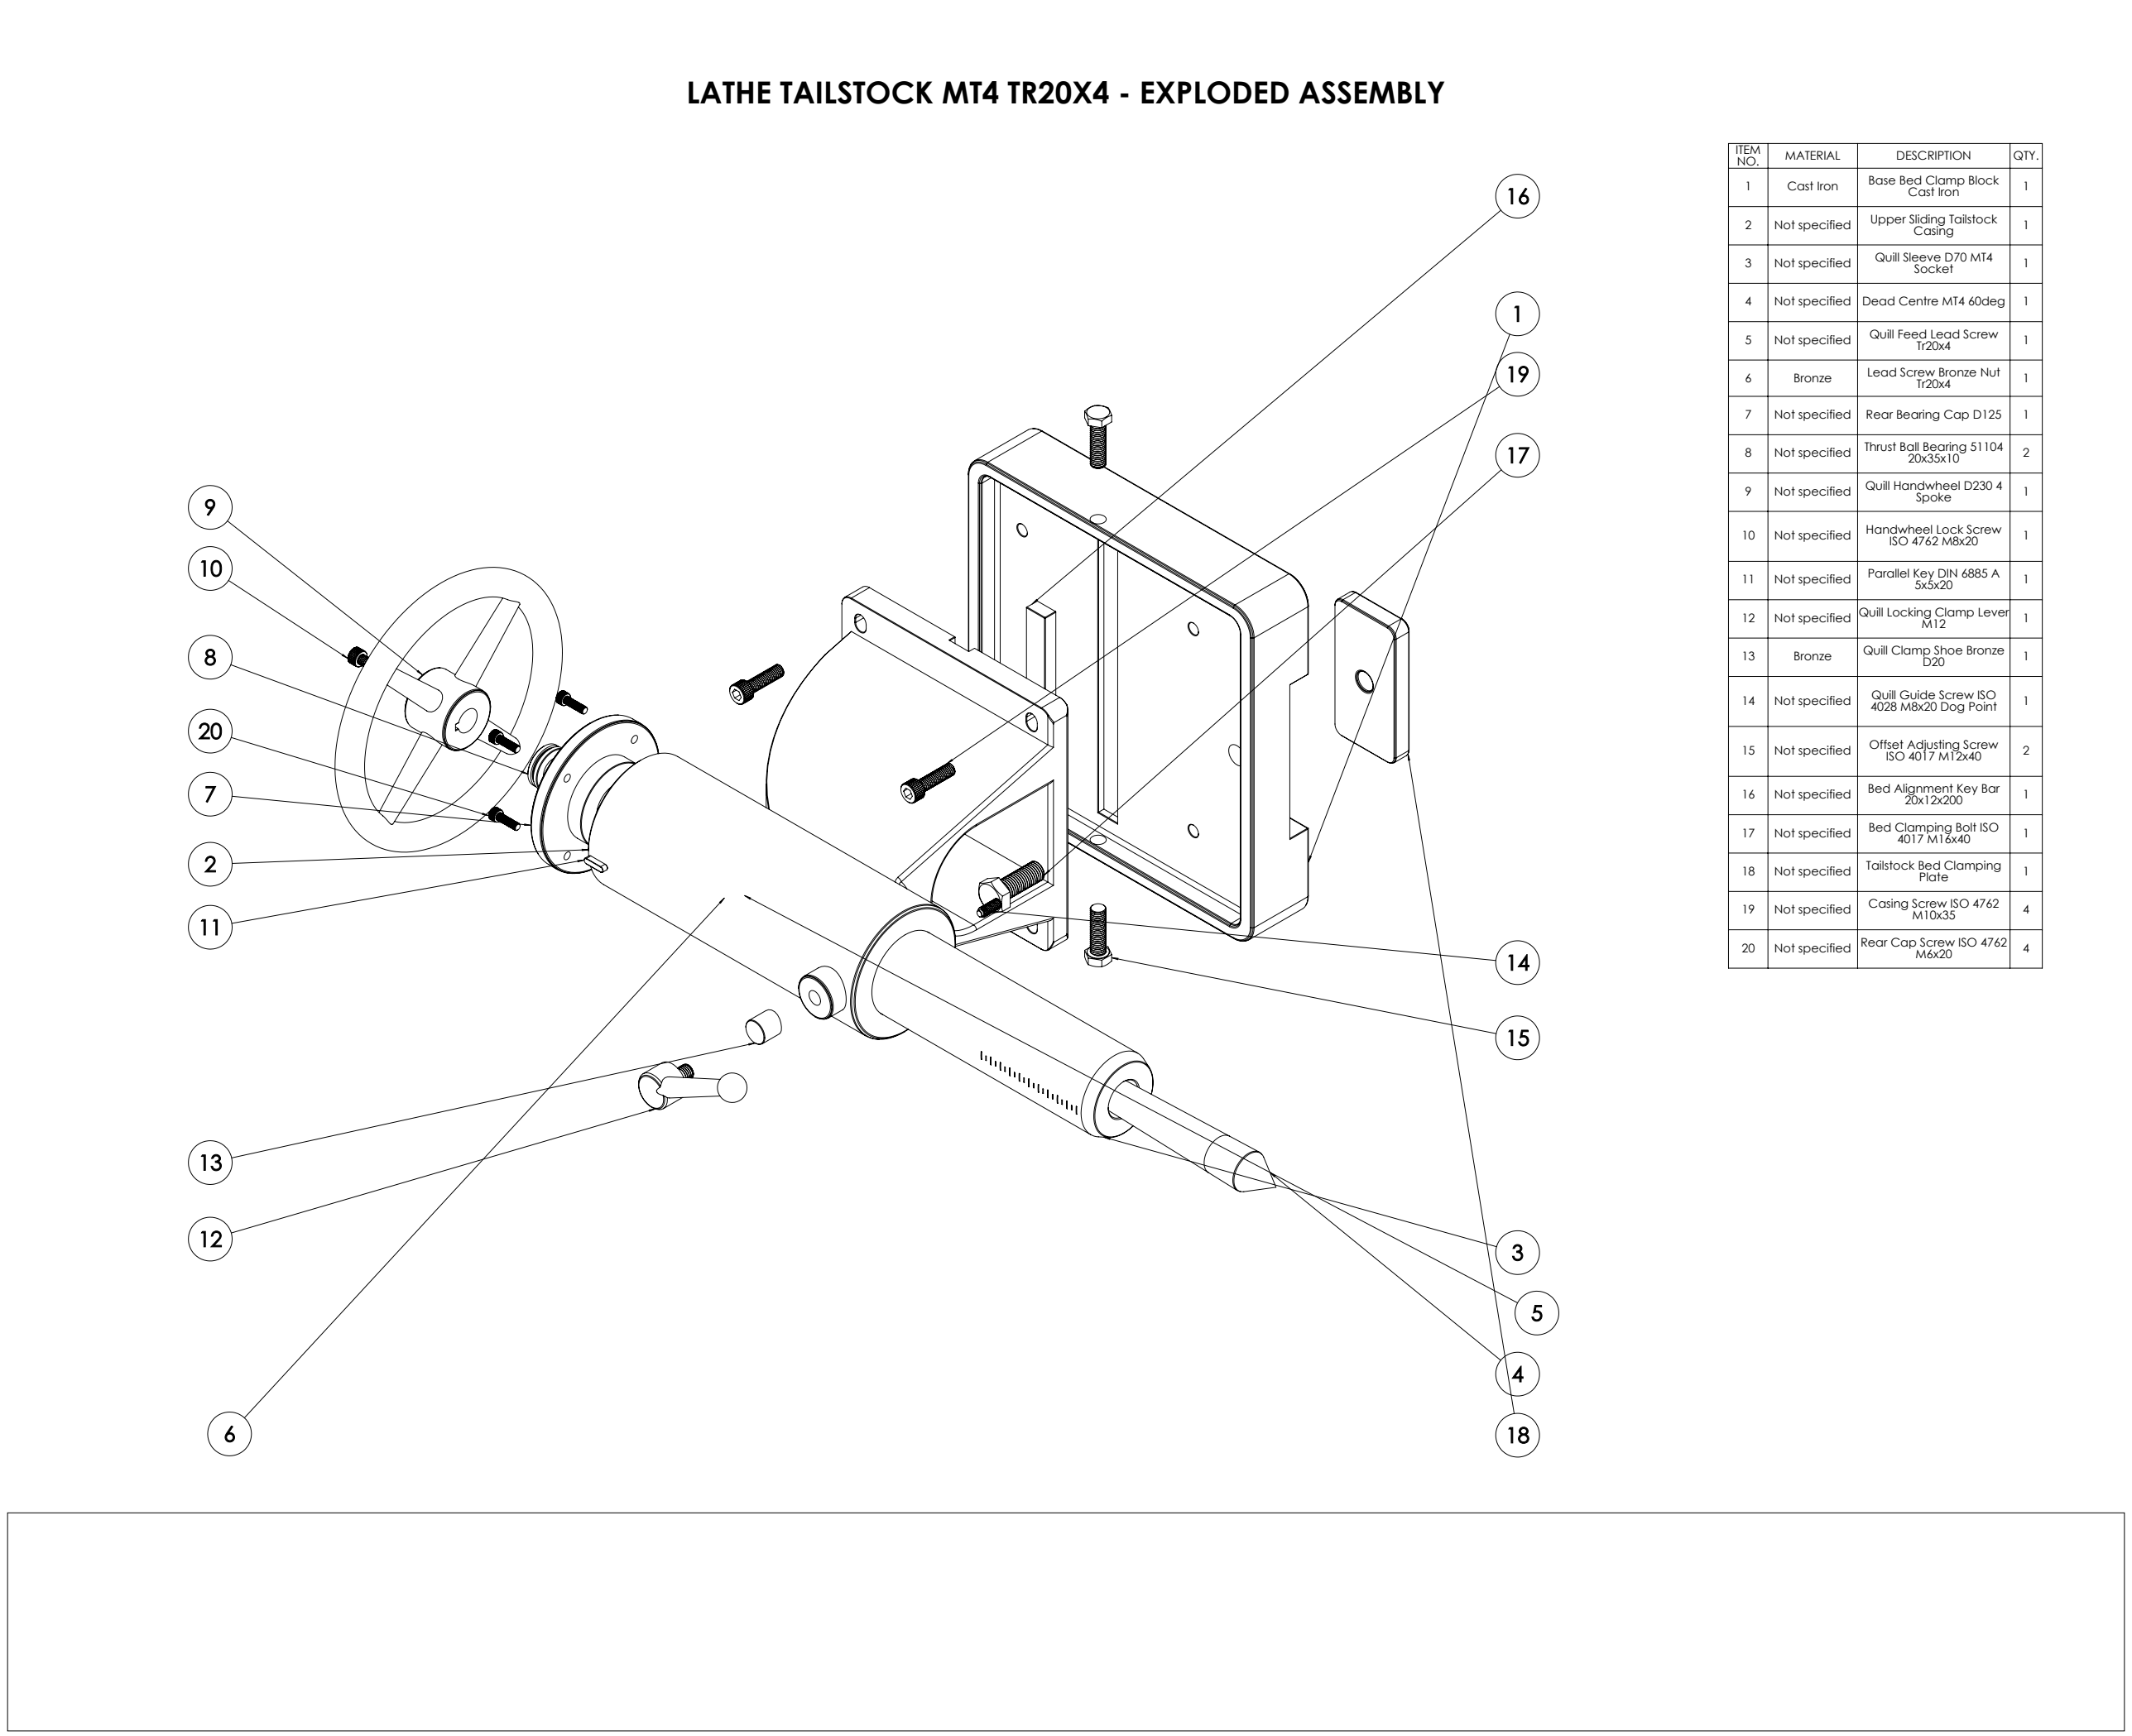
ISO-10303-21;
HEADER;
/* Generated by software containing ST-Developer
 * from STEP Tools, Inc. (www.steptools.com) 
 */

FILE_DESCRIPTION(
/* description */ (''),
/* implementation_level */ '2;1');

FILE_NAME(
/* name */ 'MAS-311',
/* time_stamp */ '2026-10-26T03:50:32-07:00',
/* author */ (''),
/* organization */ (''),
/* preprocessor_version */ 'ST-DEVELOPER v20.2',
/* originating_system */ 'Autodesk Translation Framework v15.15.0.0',
/* authorisation */ '');

FILE_SCHEMA (('AUTOMOTIVE_DESIGN { 1 0 10303 214 3 1 1 }'));
ENDSEC;

DATA;
#10=MECHANICAL_DESIGN_GEOMETRIC_PRESENTATION_REPRESENTATION('',(#1039,#1040,
#1041,#1042,#1043,#1044,#1045,#1046,#1047,#1048,#1049,#1050,#1051,#1052,
#1053,#1054,#1055,#1056,#1057,#1058),#76660);
#11=ITEM_DEFINED_TRANSFORMATION($,$,#26906,#29317);
#12=ITEM_DEFINED_TRANSFORMATION($,$,#27141,#29318);
#13=ITEM_DEFINED_TRANSFORMATION($,$,#27395,#29319);
#14=ITEM_DEFINED_TRANSFORMATION($,$,#27575,#29320);
#15=ITEM_DEFINED_TRANSFORMATION($,$,#27589,#29321);
#16=ITEM_DEFINED_TRANSFORMATION($,$,#27721,#29322);
#17=ITEM_DEFINED_TRANSFORMATION($,$,#27753,#29323);
#18=ITEM_DEFINED_TRANSFORMATION($,$,#28525,#29324);
#19=ITEM_DEFINED_TRANSFORMATION($,$,#27825,#29325);
#20=ITEM_DEFINED_TRANSFORMATION($,$,#27875,#29326);
#21=ITEM_DEFINED_TRANSFORMATION($,$,#28206,#29327);
#22=ITEM_DEFINED_TRANSFORMATION($,$,#28229,#29328);
#23=ITEM_DEFINED_TRANSFORMATION($,$,#28282,#29329);
#24=ITEM_DEFINED_TRANSFORMATION($,$,#28289,#29330);
#25=ITEM_DEFINED_TRANSFORMATION($,$,#28560,#29331);
#26=ITEM_DEFINED_TRANSFORMATION($,$,#28344,#29332);
#27=ITEM_DEFINED_TRANSFORMATION($,$,#28363,#29333);
#28=ITEM_DEFINED_TRANSFORMATION($,$,#28431,#29334);
#29=ITEM_DEFINED_TRANSFORMATION($,$,#28632,#29335);
#30=ITEM_DEFINED_TRANSFORMATION($,$,#28978,#29336);
#31=ITEM_DEFINED_TRANSFORMATION($,$,#28525,#29337);
#32=ITEM_DEFINED_TRANSFORMATION($,$,#28560,#29338);
#33=ITEM_DEFINED_TRANSFORMATION($,$,#28632,#29339);
#34=ITEM_DEFINED_TRANSFORMATION($,$,#28632,#29340);
#35=ITEM_DEFINED_TRANSFORMATION($,$,#28632,#29341);
#36=ITEM_DEFINED_TRANSFORMATION($,$,#28978,#29342);
#37=ITEM_DEFINED_TRANSFORMATION($,$,#28978,#29343);
#38=ITEM_DEFINED_TRANSFORMATION($,$,#28978,#29344);
#39=(
REPRESENTATION_RELATIONSHIP($,$,#76736,#76735)
REPRESENTATION_RELATIONSHIP_WITH_TRANSFORMATION(#11)
SHAPE_REPRESENTATION_RELATIONSHIP()
);
#40=(
REPRESENTATION_RELATIONSHIP($,$,#76737,#76735)
REPRESENTATION_RELATIONSHIP_WITH_TRANSFORMATION(#12)
SHAPE_REPRESENTATION_RELATIONSHIP()
);
#41=(
REPRESENTATION_RELATIONSHIP($,$,#76738,#76735)
REPRESENTATION_RELATIONSHIP_WITH_TRANSFORMATION(#13)
SHAPE_REPRESENTATION_RELATIONSHIP()
);
#42=(
REPRESENTATION_RELATIONSHIP($,$,#76739,#76735)
REPRESENTATION_RELATIONSHIP_WITH_TRANSFORMATION(#14)
SHAPE_REPRESENTATION_RELATIONSHIP()
);
#43=(
REPRESENTATION_RELATIONSHIP($,$,#76740,#76735)
REPRESENTATION_RELATIONSHIP_WITH_TRANSFORMATION(#15)
SHAPE_REPRESENTATION_RELATIONSHIP()
);
#44=(
REPRESENTATION_RELATIONSHIP($,$,#76741,#76735)
REPRESENTATION_RELATIONSHIP_WITH_TRANSFORMATION(#16)
SHAPE_REPRESENTATION_RELATIONSHIP()
);
#45=(
REPRESENTATION_RELATIONSHIP($,$,#76742,#76735)
REPRESENTATION_RELATIONSHIP_WITH_TRANSFORMATION(#17)
SHAPE_REPRESENTATION_RELATIONSHIP()
);
#46=(
REPRESENTATION_RELATIONSHIP($,$,#76752,#76735)
REPRESENTATION_RELATIONSHIP_WITH_TRANSFORMATION(#18)
SHAPE_REPRESENTATION_RELATIONSHIP()
);
#47=(
REPRESENTATION_RELATIONSHIP($,$,#76743,#76735)
REPRESENTATION_RELATIONSHIP_WITH_TRANSFORMATION(#19)
SHAPE_REPRESENTATION_RELATIONSHIP()
);
#48=(
REPRESENTATION_RELATIONSHIP($,$,#76744,#76735)
REPRESENTATION_RELATIONSHIP_WITH_TRANSFORMATION(#20)
SHAPE_REPRESENTATION_RELATIONSHIP()
);
#49=(
REPRESENTATION_RELATIONSHIP($,$,#76745,#76735)
REPRESENTATION_RELATIONSHIP_WITH_TRANSFORMATION(#21)
SHAPE_REPRESENTATION_RELATIONSHIP()
);
#50=(
REPRESENTATION_RELATIONSHIP($,$,#76746,#76735)
REPRESENTATION_RELATIONSHIP_WITH_TRANSFORMATION(#22)
SHAPE_REPRESENTATION_RELATIONSHIP()
);
#51=(
REPRESENTATION_RELATIONSHIP($,$,#76747,#76735)
REPRESENTATION_RELATIONSHIP_WITH_TRANSFORMATION(#23)
SHAPE_REPRESENTATION_RELATIONSHIP()
);
#52=(
REPRESENTATION_RELATIONSHIP($,$,#76748,#76735)
REPRESENTATION_RELATIONSHIP_WITH_TRANSFORMATION(#24)
SHAPE_REPRESENTATION_RELATIONSHIP()
);
#53=(
REPRESENTATION_RELATIONSHIP($,$,#76753,#76735)
REPRESENTATION_RELATIONSHIP_WITH_TRANSFORMATION(#25)
SHAPE_REPRESENTATION_RELATIONSHIP()
);
#54=(
REPRESENTATION_RELATIONSHIP($,$,#76749,#76735)
REPRESENTATION_RELATIONSHIP_WITH_TRANSFORMATION(#26)
SHAPE_REPRESENTATION_RELATIONSHIP()
);
#55=(
REPRESENTATION_RELATIONSHIP($,$,#76750,#76735)
REPRESENTATION_RELATIONSHIP_WITH_TRANSFORMATION(#27)
SHAPE_REPRESENTATION_RELATIONSHIP()
);
#56=(
REPRESENTATION_RELATIONSHIP($,$,#76751,#76735)
REPRESENTATION_RELATIONSHIP_WITH_TRANSFORMATION(#28)
SHAPE_REPRESENTATION_RELATIONSHIP()
);
#57=(
REPRESENTATION_RELATIONSHIP($,$,#76754,#76735)
REPRESENTATION_RELATIONSHIP_WITH_TRANSFORMATION(#29)
SHAPE_REPRESENTATION_RELATIONSHIP()
);
#58=(
REPRESENTATION_RELATIONSHIP($,$,#76755,#76735)
REPRESENTATION_RELATIONSHIP_WITH_TRANSFORMATION(#30)
SHAPE_REPRESENTATION_RELATIONSHIP()
);
#59=(
REPRESENTATION_RELATIONSHIP($,$,#76752,#76735)
REPRESENTATION_RELATIONSHIP_WITH_TRANSFORMATION(#31)
SHAPE_REPRESENTATION_RELATIONSHIP()
);
#60=(
REPRESENTATION_RELATIONSHIP($,$,#76753,#76735)
REPRESENTATION_RELATIONSHIP_WITH_TRANSFORMATION(#32)
SHAPE_REPRESENTATION_RELATIONSHIP()
);
#61=(
REPRESENTATION_RELATIONSHIP($,$,#76754,#76735)
REPRESENTATION_RELATIONSHIP_WITH_TRANSFORMATION(#33)
SHAPE_REPRESENTATION_RELATIONSHIP()
);
#62=(
REPRESENTATION_RELATIONSHIP($,$,#76754,#76735)
REPRESENTATION_RELATIONSHIP_WITH_TRANSFORMATION(#34)
SHAPE_REPRESENTATION_RELATIONSHIP()
);
#63=(
REPRESENTATION_RELATIONSHIP($,$,#76754,#76735)
REPRESENTATION_RELATIONSHIP_WITH_TRANSFORMATION(#35)
SHAPE_REPRESENTATION_RELATIONSHIP()
);
#64=(
REPRESENTATION_RELATIONSHIP($,$,#76755,#76735)
REPRESENTATION_RELATIONSHIP_WITH_TRANSFORMATION(#36)
SHAPE_REPRESENTATION_RELATIONSHIP()
);
#65=(
REPRESENTATION_RELATIONSHIP($,$,#76755,#76735)
REPRESENTATION_RELATIONSHIP_WITH_TRANSFORMATION(#37)
SHAPE_REPRESENTATION_RELATIONSHIP()
);
#66=(
REPRESENTATION_RELATIONSHIP($,$,#76755,#76735)
REPRESENTATION_RELATIONSHIP_WITH_TRANSFORMATION(#38)
SHAPE_REPRESENTATION_RELATIONSHIP()
);
#67=CONTEXT_DEPENDENT_SHAPE_REPRESENTATION(#39,#76707);
#68=CONTEXT_DEPENDENT_SHAPE_REPRESENTATION(#40,#76708);
#69=CONTEXT_DEPENDENT_SHAPE_REPRESENTATION(#41,#76709);
#70=CONTEXT_DEPENDENT_SHAPE_REPRESENTATION(#42,#76710);
#71=CONTEXT_DEPENDENT_SHAPE_REPRESENTATION(#43,#76711);
#72=CONTEXT_DEPENDENT_SHAPE_REPRESENTATION(#44,#76712);
#73=CONTEXT_DEPENDENT_SHAPE_REPRESENTATION(#45,#76713);
#74=CONTEXT_DEPENDENT_SHAPE_REPRESENTATION(#46,#76714);
#75=CONTEXT_DEPENDENT_SHAPE_REPRESENTATION(#47,#76715);
#76=CONTEXT_DEPENDENT_SHAPE_REPRESENTATION(#48,#76716);
#77=CONTEXT_DEPENDENT_SHAPE_REPRESENTATION(#49,#76717);
#78=CONTEXT_DEPENDENT_SHAPE_REPRESENTATION(#50,#76718);
#79=CONTEXT_DEPENDENT_SHAPE_REPRESENTATION(#51,#76719);
#80=CONTEXT_DEPENDENT_SHAPE_REPRESENTATION(#52,#76720);
#81=CONTEXT_DEPENDENT_SHAPE_REPRESENTATION(#53,#76721);
#82=CONTEXT_DEPENDENT_SHAPE_REPRESENTATION(#54,#76722);
#83=CONTEXT_DEPENDENT_SHAPE_REPRESENTATION(#55,#76723);
#84=CONTEXT_DEPENDENT_SHAPE_REPRESENTATION(#56,#76724);
#85=CONTEXT_DEPENDENT_SHAPE_REPRESENTATION(#57,#76725);
#86=CONTEXT_DEPENDENT_SHAPE_REPRESENTATION(#58,#76726);
#87=CONTEXT_DEPENDENT_SHAPE_REPRESENTATION(#59,#76727);
#88=CONTEXT_DEPENDENT_SHAPE_REPRESENTATION(#60,#76728);
#89=CONTEXT_DEPENDENT_SHAPE_REPRESENTATION(#61,#76729);
#90=CONTEXT_DEPENDENT_SHAPE_REPRESENTATION(#62,#76730);
#91=CONTEXT_DEPENDENT_SHAPE_REPRESENTATION(#63,#76731);
#92=CONTEXT_DEPENDENT_SHAPE_REPRESENTATION(#64,#76732);
#93=CONTEXT_DEPENDENT_SHAPE_REPRESENTATION(#65,#76733);
#94=CONTEXT_DEPENDENT_SHAPE_REPRESENTATION(#66,#76734);
#95=NEXT_ASSEMBLY_USAGE_OCCURRENCE(
'01_Base_Bed_Clamp_Block_Cast_Iron:1',
'01_Base_Bed_Clamp_Block_Cast_Iron:1',
'01_Base_Bed_Clamp_Block_Cast_Iron:1',#76757,#76758,
'01_Base_Bed_Clamp_Block_Cast_Iron:1');
#96=NEXT_ASSEMBLY_USAGE_OCCURRENCE(
'02_Upper_Sliding_Tailstock_Casing:1',
'02_Upper_Sliding_Tailstock_Casing:1',
'02_Upper_Sliding_Tailstock_Casing:1',#76757,#76759,
'02_Upper_Sliding_Tailstock_Casing:1');
#97=NEXT_ASSEMBLY_USAGE_OCCURRENCE('03_Quill_Sleeve_D70_MT4_Socket:1',
'03_Quill_Sleeve_D70_MT4_Socket:1','03_Quill_Sleeve_D70_MT4_Socket:1',#76757,
#76760,'03_Quill_Sleeve_D70_MT4_Socket:1');
#98=NEXT_ASSEMBLY_USAGE_OCCURRENCE('04_Dead_Centre_MT4_60deg:1',
'04_Dead_Centre_MT4_60deg:1','04_Dead_Centre_MT4_60deg:1',#76757,#76761,
'04_Dead_Centre_MT4_60deg:1');
#99=NEXT_ASSEMBLY_USAGE_OCCURRENCE('05_Quill_Feed_Lead_Screw_Tr20x4:1',
'05_Quill_Feed_Lead_Screw_Tr20x4:1','05_Quill_Feed_Lead_Screw_Tr20x4:1',
#76757,#76762,'05_Quill_Feed_Lead_Screw_Tr20x4:1');
#100=NEXT_ASSEMBLY_USAGE_OCCURRENCE('06_Lead_Screw_Bronze_Nut_Tr20x4:1',
'06_Lead_Screw_Bronze_Nut_Tr20x4:1','06_Lead_Screw_Bronze_Nut_Tr20x4:1',
#76757,#76763,'06_Lead_Screw_Bronze_Nut_Tr20x4:1');
#101=NEXT_ASSEMBLY_USAGE_OCCURRENCE('07_Rear_Bearing_Cap_D125:1',
'07_Rear_Bearing_Cap_D125:1','07_Rear_Bearing_Cap_D125:1',#76757,#76764,
'07_Rear_Bearing_Cap_D125:1');
#102=NEXT_ASSEMBLY_USAGE_OCCURRENCE(
'08_Thrust_Ball_Bearing_51104_20x35x10:1',
'08_Thrust_Ball_Bearing_51104_20x35x10:1',
'08_Thrust_Ball_Bearing_51104_20x35x10:1',#76757,#76774,
'08_Thrust_Ball_Bearing_51104_20x35x10:1');
#103=NEXT_ASSEMBLY_USAGE_OCCURRENCE('09_Quill_Handwheel_D230_4_Spoke:1',
'09_Quill_Handwheel_D230_4_Spoke:1','09_Quill_Handwheel_D230_4_Spoke:1',
#76757,#76765,'09_Quill_Handwheel_D230_4_Spoke:1');
#104=NEXT_ASSEMBLY_USAGE_OCCURRENCE(
'10_Handwheel_Lock_Screw_ISO_4762_M8x20:1',
'10_Handwheel_Lock_Screw_ISO_4762_M8x20:1',
'10_Handwheel_Lock_Screw_ISO_4762_M8x20:1',#76757,#76766,
'10_Handwheel_Lock_Screw_ISO_4762_M8x20:1');
#105=NEXT_ASSEMBLY_USAGE_OCCURRENCE(
'11_Parallel_Key_DIN_6885_A_5x5x20:1',
'11_Parallel_Key_DIN_6885_A_5x5x20:1',
'11_Parallel_Key_DIN_6885_A_5x5x20:1',#76757,#76767,
'11_Parallel_Key_DIN_6885_A_5x5x20:1');
#106=NEXT_ASSEMBLY_USAGE_OCCURRENCE(
'12_Quill_Locking_Clamp_Lever_M12:1',
'12_Quill_Locking_Clamp_Lever_M12:1',
'12_Quill_Locking_Clamp_Lever_M12:1',#76757,#76768,
'12_Quill_Locking_Clamp_Lever_M12:1');
#107=NEXT_ASSEMBLY_USAGE_OCCURRENCE('13_Quill_Clamp_Shoe_Bronze_D20:1',
'13_Quill_Clamp_Shoe_Bronze_D20:1','13_Quill_Clamp_Shoe_Bronze_D20:1',#76757,
#76769,'13_Quill_Clamp_Shoe_Bronze_D20:1');
#108=NEXT_ASSEMBLY_USAGE_OCCURRENCE(
'14_Quill_Guide_Screw_ISO_4028_M8x20_Dog_Point:1',
'14_Quill_Guide_Screw_ISO_4028_M8x20_Dog_Point:1',
'14_Quill_Guide_Screw_ISO_4028_M8x20_Dog_Point:1',#76757,#76770,
'14_Quill_Guide_Screw_ISO_4028_M8x20_Dog_Point:1');
#109=NEXT_ASSEMBLY_USAGE_OCCURRENCE(
'15_Offset_Adjusting_Screw_ISO_4017_M12x40:1',
'15_Offset_Adjusting_Screw_ISO_4017_M12x40:1',
'15_Offset_Adjusting_Screw_ISO_4017_M12x40:1',#76757,#76775,
'15_Offset_Adjusting_Screw_ISO_4017_M12x40:1');
#110=NEXT_ASSEMBLY_USAGE_OCCURRENCE(
'16_Bed_Alignment_Key_Bar_20x12x200:1',
'16_Bed_Alignment_Key_Bar_20x12x200:1',
'16_Bed_Alignment_Key_Bar_20x12x200:1',#76757,#76771,
'16_Bed_Alignment_Key_Bar_20x12x200:1');
#111=NEXT_ASSEMBLY_USAGE_OCCURRENCE(
'17_Bed_Clamping_Bolt_ISO_4017_M16x40:1',
'17_Bed_Clamping_Bolt_ISO_4017_M16x40:1',
'17_Bed_Clamping_Bolt_ISO_4017_M16x40:1',#76757,#76772,
'17_Bed_Clamping_Bolt_ISO_4017_M16x40:1');
#112=NEXT_ASSEMBLY_USAGE_OCCURRENCE('18_Tailstock_Bed_Clamping_Plate:1',
'18_Tailstock_Bed_Clamping_Plate:1','18_Tailstock_Bed_Clamping_Plate:1',
#76757,#76773,'18_Tailstock_Bed_Clamping_Plate:1');
#113=NEXT_ASSEMBLY_USAGE_OCCURRENCE('19_Casing_Screw_ISO_4762_M10x35:1',
'19_Casing_Screw_ISO_4762_M10x35:1','19_Casing_Screw_ISO_4762_M10x35:1',
#76757,#76776,'19_Casing_Screw_ISO_4762_M10x35:1');
#114=NEXT_ASSEMBLY_USAGE_OCCURRENCE(
'20_Rear_Cap_Screw_ISO_4762_M6x20:1',
'20_Rear_Cap_Screw_ISO_4762_M6x20:1',
'20_Rear_Cap_Screw_ISO_4762_M6x20:1',#76757,#76777,
'20_Rear_Cap_Screw_ISO_4762_M6x20:1');
#115=NEXT_ASSEMBLY_USAGE_OCCURRENCE(
'08_Thrust_Ball_Bearing_51104_20x35x10:2',
'08_Thrust_Ball_Bearing_51104_20x35x10:2',
'08_Thrust_Ball_Bearing_51104_20x35x10:2',#76757,#76774,
'08_Thrust_Ball_Bearing_51104_20x35x10:2');
#116=NEXT_ASSEMBLY_USAGE_OCCURRENCE(
'15_Offset_Adjusting_Screw_ISO_4017_M12x40:2',
'15_Offset_Adjusting_Screw_ISO_4017_M12x40:2',
'15_Offset_Adjusting_Screw_ISO_4017_M12x40:2',#76757,#76775,
'15_Offset_Adjusting_Screw_ISO_4017_M12x40:2');
#117=NEXT_ASSEMBLY_USAGE_OCCURRENCE('19_Casing_Screw_ISO_4762_M10x35:2',
'19_Casing_Screw_ISO_4762_M10x35:2','19_Casing_Screw_ISO_4762_M10x35:2',
#76757,#76776,'19_Casing_Screw_ISO_4762_M10x35:2');
#118=NEXT_ASSEMBLY_USAGE_OCCURRENCE('19_Casing_Screw_ISO_4762_M10x35:3',
'19_Casing_Screw_ISO_4762_M10x35:3','19_Casing_Screw_ISO_4762_M10x35:3',
#76757,#76776,'19_Casing_Screw_ISO_4762_M10x35:3');
#119=NEXT_ASSEMBLY_USAGE_OCCURRENCE('19_Casing_Screw_ISO_4762_M10x35:4',
'19_Casing_Screw_ISO_4762_M10x35:4','19_Casing_Screw_ISO_4762_M10x35:4',
#76757,#76776,'19_Casing_Screw_ISO_4762_M10x35:4');
#120=NEXT_ASSEMBLY_USAGE_OCCURRENCE(
'20_Rear_Cap_Screw_ISO_4762_M6x20:2',
'20_Rear_Cap_Screw_ISO_4762_M6x20:2',
'20_Rear_Cap_Screw_ISO_4762_M6x20:2',#76757,#76777,
'20_Rear_Cap_Screw_ISO_4762_M6x20:2');
#121=NEXT_ASSEMBLY_USAGE_OCCURRENCE(
'20_Rear_Cap_Screw_ISO_4762_M6x20:3',
'20_Rear_Cap_Screw_ISO_4762_M6x20:3',
'20_Rear_Cap_Screw_ISO_4762_M6x20:3',#76757,#76777,
'20_Rear_Cap_Screw_ISO_4762_M6x20:3');
#122=NEXT_ASSEMBLY_USAGE_OCCURRENCE(
'20_Rear_Cap_Screw_ISO_4762_M6x20:4',
'20_Rear_Cap_Screw_ISO_4762_M6x20:4',
'20_Rear_Cap_Screw_ISO_4762_M6x20:4',#76757,#76777,
'20_Rear_Cap_Screw_ISO_4762_M6x20:4');
#123=(
BOUNDED_CURVE()
B_SPLINE_CURVE(2,(#63169,#63170,#63171),.UNSPECIFIED.,.F.,.F.)
B_SPLINE_CURVE_WITH_KNOTS((3,3),(0.0830692064483411,1.5163968327409),
 .UNSPECIFIED.)
CURVE()
GEOMETRIC_REPRESENTATION_ITEM()
RATIONAL_B_SPLINE_CURVE((1.01933756729741,1.17702963774851,1.01933756729741))
REPRESENTATION_ITEM('')
);
#124=(
BOUNDED_CURVE()
B_SPLINE_CURVE(2,(#63173,#63174,#63175),.UNSPECIFIED.,.F.,.F.)
B_SPLINE_CURVE_WITH_KNOTS((3,3),(0.0830692064483407,1.5163968327409),
 .UNSPECIFIED.)
CURVE()
GEOMETRIC_REPRESENTATION_ITEM()
RATIONAL_B_SPLINE_CURVE((1.01933756729741,1.17702963774851,1.01933756729741))
REPRESENTATION_ITEM('')
);
#125=(
BOUNDED_CURVE()
B_SPLINE_CURVE(2,(#63177,#63178,#63179),.UNSPECIFIED.,.F.,.F.)
B_SPLINE_CURVE_WITH_KNOTS((3,3),(0.0830692064483414,1.5163968327409),
 .UNSPECIFIED.)
CURVE()
GEOMETRIC_REPRESENTATION_ITEM()
RATIONAL_B_SPLINE_CURVE((1.01933756729741,1.17702963774851,1.01933756729741))
REPRESENTATION_ITEM('')
);
#126=(
BOUNDED_CURVE()
B_SPLINE_CURVE(2,(#63181,#63182,#63183),.UNSPECIFIED.,.F.,.F.)
B_SPLINE_CURVE_WITH_KNOTS((3,3),(0.0830692064483412,1.5163968327409),
 .UNSPECIFIED.)
CURVE()
GEOMETRIC_REPRESENTATION_ITEM()
RATIONAL_B_SPLINE_CURVE((1.01933756729741,1.17702963774851,1.01933756729741))
REPRESENTATION_ITEM('')
);
#127=(
BOUNDED_CURVE()
B_SPLINE_CURVE(2,(#63185,#63186,#63187),.UNSPECIFIED.,.F.,.F.)
B_SPLINE_CURVE_WITH_KNOTS((3,3),(0.799733019594622,1.5163968327409),
 .UNSPECIFIED.)
CURVE()
GEOMETRIC_REPRESENTATION_ITEM()
RATIONAL_B_SPLINE_CURVE((1.09818360252296,1.09818360252296,1.01933756729741))
REPRESENTATION_ITEM('')
);
#128=(
BOUNDED_CURVE()
B_SPLINE_CURVE(2,(#63192,#63193,#63194),.UNSPECIFIED.,.F.,.F.)
B_SPLINE_CURVE_WITH_KNOTS((3,3),(0.083069206448341,0.799733019594622),
 .UNSPECIFIED.)
CURVE()
GEOMETRIC_REPRESENTATION_ITEM()
RATIONAL_B_SPLINE_CURVE((1.01933756729741,1.09818360252296,1.09818360252296))
REPRESENTATION_ITEM('')
);
#129=(
BOUNDED_CURVE()
B_SPLINE_CURVE(2,(#63195,#63196,#63197),.UNSPECIFIED.,.F.,.F.)
B_SPLINE_CURVE_WITH_KNOTS((3,3),(0.0830692064483408,1.5163968327409),
 .UNSPECIFIED.)
CURVE()
GEOMETRIC_REPRESENTATION_ITEM()
RATIONAL_B_SPLINE_CURVE((1.01933756729741,1.17702963774851,1.01933756729741))
REPRESENTATION_ITEM('')
);
#130=(
BOUNDED_CURVE()
B_SPLINE_CURVE(2,(#68996,#68997,#68998),.UNSPECIFIED.,.F.,.F.)
B_SPLINE_CURVE_WITH_KNOTS((3,3),(0.0817872044632405,1.1645820942826),
 .UNSPECIFIED.)
CURVE()
GEOMETRIC_REPRESENTATION_ITEM()
RATIONAL_B_SPLINE_CURVE((1.02578342306321,1.1844726708716,1.02578342306321))
REPRESENTATION_ITEM('')
);
#131=(
BOUNDED_CURVE()
B_SPLINE_CURVE(2,(#69000,#69001,#69002),.UNSPECIFIED.,.F.,.F.)
B_SPLINE_CURVE_WITH_KNOTS((3,3),(0.0817872044632409,1.1645820942826),
 .UNSPECIFIED.)
CURVE()
GEOMETRIC_REPRESENTATION_ITEM()
RATIONAL_B_SPLINE_CURVE((1.02578342306321,1.1844726708716,1.02578342306321))
REPRESENTATION_ITEM('')
);
#132=(
BOUNDED_CURVE()
B_SPLINE_CURVE(2,(#69004,#69005,#69006),.UNSPECIFIED.,.F.,.F.)
B_SPLINE_CURVE_WITH_KNOTS((3,3),(0.0817872044632405,1.1645820942826),
 .UNSPECIFIED.)
CURVE()
GEOMETRIC_REPRESENTATION_ITEM()
RATIONAL_B_SPLINE_CURVE((1.02578342306321,1.1844726708716,1.02578342306321))
REPRESENTATION_ITEM('')
);
#133=(
BOUNDED_CURVE()
B_SPLINE_CURVE(2,(#69008,#69009,#69010),.UNSPECIFIED.,.F.,.F.)
B_SPLINE_CURVE_WITH_KNOTS((3,3),(0.0817872044632409,1.1645820942826),
 .UNSPECIFIED.)
CURVE()
GEOMETRIC_REPRESENTATION_ITEM()
RATIONAL_B_SPLINE_CURVE((1.02578342306321,1.1844726708716,1.02578342306321))
REPRESENTATION_ITEM('')
);
#134=(
BOUNDED_CURVE()
B_SPLINE_CURVE(2,(#69012,#69013,#69014),.UNSPECIFIED.,.F.,.F.)
B_SPLINE_CURVE_WITH_KNOTS((3,3),(0.623184649372919,1.1645820942826),
 .UNSPECIFIED.)
CURVE()
GEOMETRIC_REPRESENTATION_ITEM()
RATIONAL_B_SPLINE_CURVE((1.1051280469674,1.1051280469674,1.02578342306321))
REPRESENTATION_ITEM('')
);
#135=(
BOUNDED_CURVE()
B_SPLINE_CURVE(2,(#69019,#69020,#69021),.UNSPECIFIED.,.F.,.F.)
B_SPLINE_CURVE_WITH_KNOTS((3,3),(0.081787204463241,0.623184649372919),
 .UNSPECIFIED.)
CURVE()
GEOMETRIC_REPRESENTATION_ITEM()
RATIONAL_B_SPLINE_CURVE((1.02578342306321,1.1051280469674,1.1051280469674))
REPRESENTATION_ITEM('')
);
#136=(
BOUNDED_CURVE()
B_SPLINE_CURVE(2,(#69022,#69023,#69024),.UNSPECIFIED.,.F.,.F.)
B_SPLINE_CURVE_WITH_KNOTS((3,3),(0.0817872044632407,1.1645820942826),
 .UNSPECIFIED.)
CURVE()
GEOMETRIC_REPRESENTATION_ITEM()
RATIONAL_B_SPLINE_CURVE((1.02578342306321,1.1844726708716,1.02578342306321))
REPRESENTATION_ITEM('')
);
#137=SPHERICAL_SURFACE('',#28269,1.1);
#138=B_SPLINE_SURFACE_WITH_KNOTS('',3,3,((#37277,#37278,#37279,#37280,#37281,
#37282,#37283,#37284,#37285,#37286,#37287,#37288,#37289,#37290,#37291,#37292,
#37293,#37294,#37295,#37296,#37297,#37298,#37299,#37300,#37301,#37302,#37303,
#37304,#37305,#37306,#37307,#37308,#37309,#37310,#37311,#37312,#37313,#37314,
#37315,#37316,#37317,#37318,#37319,#37320,#37321,#37322,#37323,#37324),
(#37325,#37326,#37327,#37328,#37329,#37330,#37331,#37332,#37333,#37334,
#37335,#37336,#37337,#37338,#37339,#37340,#37341,#37342,#37343,#37344,#37345,
#37346,#37347,#37348,#37349,#37350,#37351,#37352,#37353,#37354,#37355,#37356,
#37357,#37358,#37359,#37360,#37361,#37362,#37363,#37364,#37365,#37366,#37367,
#37368,#37369,#37370,#37371,#37372),(#37373,#37374,#37375,#37376,#37377,
#37378,#37379,#37380,#37381,#37382,#37383,#37384,#37385,#37386,#37387,#37388,
#37389,#37390,#37391,#37392,#37393,#37394,#37395,#37396,#37397,#37398,#37399,
#37400,#37401,#37402,#37403,#37404,#37405,#37406,#37407,#37408,#37409,#37410,
#37411,#37412,#37413,#37414,#37415,#37416,#37417,#37418,#37419,#37420),
(#37421,#37422,#37423,#37424,#37425,#37426,#37427,#37428,#37429,#37430,
#37431,#37432,#37433,#37434,#37435,#37436,#37437,#37438,#37439,#37440,#37441,
#37442,#37443,#37444,#37445,#37446,#37447,#37448,#37449,#37450,#37451,#37452,
#37453,#37454,#37455,#37456,#37457,#37458,#37459,#37460,#37461,#37462,#37463,
#37464,#37465,#37466,#37467,#37468)),.UNSPECIFIED.,.F.,.T.,.F.,(4,4),(4,
1,1,1,1,1,1,1,1,1,1,1,1,1,1,1,1,1,1,1,1,1,1,1,1,1,1,1,1,1,1,1,1,1,1,1,1,
1,1,1,1,1,1,1,1,4),(0.,1.),(0.,0.301700924572155,0.452551386858232,0.60340184914431,
0.62225815693007,0.641114464715829,0.678827080287349,0.716539695858868,
0.754252311430387,0.829677542573426,0.867390158144946,0.905102773716465,
1.20680369828862,1.23194544200297,1.25708718571731,1.307370673146,1.40793764800339,
1.81020554743293,1.83534729114728,1.86048903486162,1.91077252229031,2.0113394971477,
2.21247344686247,2.26275693429116,2.41360739657724,2.56445785886332,2.71530832114939,
2.86615878343547,2.94158401457851,2.96044032236427,2.97929663015003,2.99815293793579,
3.00758109182867,3.01229516877511,3.01700924572155,3.3187101702937,3.35642278586522,
3.39413540143674,3.46956063257978,3.54498586372282,3.58269847929434,3.6015547870801,
3.62041109486586,3.77126155715194,3.92211201943801,4.22381294401017),
 .UNSPECIFIED.);
#139=B_SPLINE_SURFACE_WITH_KNOTS('',3,3,((#37678,#37679,#37680,#37681,#37682,
#37683,#37684,#37685),(#37686,#37687,#37688,#37689,#37690,#37691,#37692,
#37693),(#37694,#37695,#37696,#37697,#37698,#37699,#37700,#37701),(#37702,
#37703,#37704,#37705,#37706,#37707,#37708,#37709)),.UNSPECIFIED.,.F.,.F.,
 .F.,(4,4),(4,1,1,1,1,4),(0.,1.),(0.,0.142857142857143,0.428571428571429,
0.571428571428571,0.857142857142857,1.),.UNSPECIFIED.);
#140=B_SPLINE_SURFACE_WITH_KNOTS('',3,3,((#37811,#37812,#37813,#37814,#37815,
#37816,#37817,#37818),(#37819,#37820,#37821,#37822,#37823,#37824,#37825,
#37826),(#37827,#37828,#37829,#37830,#37831,#37832,#37833,#37834),(#37835,
#37836,#37837,#37838,#37839,#37840,#37841,#37842)),.UNSPECIFIED.,.F.,.F.,
 .F.,(4,4),(4,1,1,1,1,4),(0.,1.),(0.,0.142857142857143,0.428571428571429,
0.571428571428571,0.857142857142857,1.),.UNSPECIFIED.);
#141=B_SPLINE_SURFACE_WITH_KNOTS('',3,3,((#37944,#37945,#37946,#37947,#37948),
(#37949,#37950,#37951,#37952,#37953),(#37954,#37955,#37956,#37957,#37958),
(#37959,#37960,#37961,#37962,#37963)),.UNSPECIFIED.,.F.,.F.,.F.,(4,4),(4,
1,4),(0.,1.),(1.87779361595245,2.32640602317479,2.66286532859155),
 .UNSPECIFIED.);
#142=B_SPLINE_SURFACE_WITH_KNOTS('',3,3,((#38058,#38059,#38060,#38061),
(#38062,#38063,#38064,#38065),(#38066,#38067,#38068,#38069),(#38070,#38071,
#38072,#38073)),.UNSPECIFIED.,.F.,.F.,.F.,(4,4),(4,4),(0.,1.),(-1.87779361595245,
-1.82480525135948),.UNSPECIFIED.);
#143=B_SPLINE_SURFACE_WITH_KNOTS('',3,3,((#38078,#38079,#38080,#38081,#38082),
(#38083,#38084,#38085,#38086,#38087),(#38088,#38089,#38090,#38091,#38092),
(#38093,#38094,#38095,#38096,#38097)),.UNSPECIFIED.,.F.,.F.,.F.,(4,4),(4,
1,4),(0.,1.),(0.000100035134689748,0.3365592783323,0.78517160259578),
 .UNSPECIFIED.);
#144=B_SPLINE_SURFACE_WITH_KNOTS('',3,3,((#38110,#38111,#38112,#38113),
(#38114,#38115,#38116,#38117),(#38118,#38119,#38120,#38121),(#38122,#38123,
#38124,#38125)),.UNSPECIFIED.,.F.,.F.,.F.,(4,4),(4,4),(0.,1.),(-0.838159967188763,
-0.78517160259578),.UNSPECIFIED.);
#145=B_SPLINE_SURFACE_WITH_KNOTS('',3,3,((#38503,#38504,#38505,#38506,#38507,
#38508,#38509,#38510),(#38511,#38512,#38513,#38514,#38515,#38516,#38517,
#38518),(#38519,#38520,#38521,#38522,#38523,#38524,#38525,#38526),(#38527,
#38528,#38529,#38530,#38531,#38532,#38533,#38534)),.UNSPECIFIED.,.F.,.F.,
 .F.,(4,4),(4,1,1,1,1,4),(0.,1.),(0.,0.142857142857143,0.428571428571429,
0.571428571428571,0.857142857142857,1.),.UNSPECIFIED.);
#146=B_SPLINE_SURFACE_WITH_KNOTS('',3,3,((#38592,#38593,#38594,#38595,#38596,
#38597,#38598,#38599),(#38600,#38601,#38602,#38603,#38604,#38605,#38606,
#38607),(#38608,#38609,#38610,#38611,#38612,#38613,#38614,#38615),(#38616,
#38617,#38618,#38619,#38620,#38621,#38622,#38623)),.UNSPECIFIED.,.F.,.F.,
 .F.,(4,4),(4,1,1,1,1,4),(0.,1.),(0.,0.142857142857143,0.428571428571429,
0.571428571428571,0.857142857142857,1.),.UNSPECIFIED.);
#147=B_SPLINE_SURFACE_WITH_KNOTS('',3,3,((#38722,#38723,#38724,#38725,#38726,
#38727,#38728),(#38729,#38730,#38731,#38732,#38733,#38734,#38735),(#38736,
#38737,#38738,#38739,#38740,#38741,#38742),(#38743,#38744,#38745,#38746,
#38747,#38748,#38749)),.UNSPECIFIED.,.F.,.F.,.F.,(4,4),(4,1,1,1,4),(0.,
1.),(9.97415695384386E-5,0.217192720402113,0.325739209818401,0.542832188650975,
0.75992516748355),.UNSPECIFIED.);
#148=B_SPLINE_SURFACE_WITH_KNOTS('',3,3,((#38791,#38792,#38793,#38794),
(#38795,#38796,#38797,#38798),(#38799,#38800,#38801,#38802),(#38803,#38804,
#38805,#38806)),.UNSPECIFIED.,.F.,.F.,.F.,(4,4),(4,4),(0.,1.),(0.759925167483548,
0.811761172549836),.UNSPECIFIED.);
#149=B_SPLINE_SURFACE_WITH_KNOTS('',3,3,((#38811,#38812,#38813,#38814,#38815,
#38816,#38817,#38818,#38819,#38820),(#38821,#38822,#38823,#38824,#38825,
#38826,#38827,#38828,#38829,#38830),(#38831,#38832,#38833,#38834,#38835,
#38836,#38837,#38838,#38839,#38840),(#38841,#38842,#38843,#38844,#38845,
#38846,#38847,#38848,#38849,#38850)),.UNSPECIFIED.,.F.,.F.,.F.,(4,4),(4,
2,1,1,2,4),(0.,1.),(1.90304005106469,2.0340806772701,2.19643291178007,2.27760902903505,
2.43996126354502,2.66286552223545),.UNSPECIFIED.);
#150=B_SPLINE_SURFACE_WITH_KNOTS('',3,3,((#38862,#38863,#38864,#38865),
(#38866,#38867,#38868,#38869),(#38870,#38871,#38872,#38873),(#38874,#38875,
#38876,#38877)),.UNSPECIFIED.,.F.,.F.,.F.,(4,4),(4,4),(0.,1.),(1.85120404599841,
1.90304005106469),.UNSPECIFIED.);
#151=B_SPLINE_SURFACE_WITH_KNOTS('',3,3,((#38903,#38904,#38905,#38906,#38907,
#38908,#38909,#38910,#38911,#38912,#38913,#38914,#38915,#38916,#38917,#38918,
#38919,#38920,#38921,#38922),(#38923,#38924,#38925,#38926,#38927,#38928,
#38929,#38930,#38931,#38932,#38933,#38934,#38935,#38936,#38937,#38938,#38939,
#38940,#38941,#38942),(#38943,#38944,#38945,#38946,#38947,#38948,#38949,
#38950,#38951,#38952,#38953,#38954,#38955,#38956,#38957,#38958,#38959,#38960,
#38961,#38962),(#38963,#38964,#38965,#38966,#38967,#38968,#38969,#38970,
#38971,#38972,#38973,#38974,#38975,#38976,#38977,#38978,#38979,#38980,#38981,
#38982)),.UNSPECIFIED.,.F.,.F.,.F.,(4,4),(4,1,1,1,1,1,1,1,1,1,1,1,1,1,1,
1,1,4),(0.,1.),(6.93617595249389,7.96866100733354,9.0011460621732,10.0336311170129,
10.5498736444327,11.0661161718525,12.0986012266922,13.1310862815318,13.8194096514249,
14.507733021318,15.1960563912111,16.5727031309973,17.2610265008905,17.7772690283103,
18.2935115557301,19.3259966105698,20.3584816654094,21.3909667202491),
 .UNSPECIFIED.);
#152=B_SPLINE_SURFACE_WITH_KNOTS('',3,3,((#39029,#39030,#39031,#39032),
(#39033,#39034,#39035,#39036),(#39037,#39038,#39039,#39040),(#39041,#39042,
#39043,#39044)),.UNSPECIFIED.,.F.,.F.,.F.,(4,4),(4,4),(0.,1.),(6.91671820418794,
6.93617595249389),.UNSPECIFIED.);
#153=B_SPLINE_SURFACE_WITH_KNOTS('',3,3,((#39053,#39054,#39055,#39056),
(#39057,#39058,#39059,#39060),(#39061,#39062,#39063,#39064),(#39065,#39066,
#39067,#39068)),.UNSPECIFIED.,.F.,.F.,.F.,(4,4),(4,4),(0.,1.),(21.3909667202491,
21.410424468555),.UNSPECIFIED.);
#154=B_SPLINE_SURFACE_WITH_KNOTS('',3,3,((#39101,#39102,#39103,#39104,#39105,
#39106,#39107),(#39108,#39109,#39110,#39111,#39112,#39113,#39114),(#39115,
#39116,#39117,#39118,#39119,#39120,#39121),(#39122,#39123,#39124,#39125,
#39126,#39127,#39128)),.UNSPECIFIED.,.F.,.F.,.F.,(4,4),(4,1,1,1,4),(0.,
1.),(0.645522939086389,0.821861702311259,0.998200465536129,1.23331881650262,
1.46843716746911),.UNSPECIFIED.);
#155=B_SPLINE_SURFACE_WITH_KNOTS('',3,3,((#39165,#39166,#39167,#39168,#39169,
#39170,#39171),(#39172,#39173,#39174,#39175,#39176,#39177,#39178),(#39179,
#39180,#39181,#39182,#39183,#39184,#39185),(#39186,#39187,#39188,#39189,
#39190,#39191,#39192)),.UNSPECIFIED.,.F.,.F.,.F.,(4,4),(4,1,1,1,4),(0.,
1.),(-1.46843716746912,-1.29209840424425,-1.11575964101938,-0.880641290052883,
-0.645522939086389),.UNSPECIFIED.);
#156=B_SPLINE_SURFACE_WITH_KNOTS('',3,3,((#39211,#39212,#39213,#39214,#39215,
#39216),(#39217,#39218,#39219,#39220,#39221,#39222),(#39223,#39224,#39225,
#39226,#39227,#39228),(#39229,#39230,#39231,#39232,#39233,#39234),(#39235,
#39236,#39237,#39238,#39239,#39240)),.UNSPECIFIED.,.F.,.F.,.F.,(4,1,4),
(4,1,1,4),(0.,0.571428571428571,1.),(3.93038111840777,4.35323723299001,
4.63514130937817,4.91704538576632),.UNSPECIFIED.);
#157=B_SPLINE_SURFACE_WITH_KNOTS('',3,3,((#39269,#39270,#39271,#39272,#39273,
#39274),(#39275,#39276,#39277,#39278,#39279,#39280),(#39281,#39282,#39283,
#39284,#39285,#39286),(#39287,#39288,#39289,#39290,#39291,#39292),(#39293,
#39294,#39295,#39296,#39297,#39298)),.UNSPECIFIED.,.F.,.F.,.F.,(4,1,4),
(4,1,1,4),(0.,0.571428571428571,1.),(0.317698823900363,0.599602900914624,
0.740554939421754,1.30436309345028),.UNSPECIFIED.);
#158=B_SPLINE_SURFACE_WITH_KNOTS('',3,3,((#45164,#45165,#45166,#45167,#45168,
#45169,#45170,#45171,#45172,#45173,#45174,#45175,#45176,#45177,#45178,#45179,
#45180,#45181,#45182,#45183,#45184,#45185,#45186,#45187,#45188,#45189,#45190,
#45191,#45192,#45193,#45194,#45195,#45196,#45197,#45198,#45199,#45200,#45201,
#45202,#45203,#45204,#45205,#45206,#45207,#45208,#45209,#45210,#45211,#45212,
#45213,#45214,#45215,#45216,#45217,#45218,#45219,#45220,#45221,#45222,#45223,
#45224,#45225,#45226,#45227,#45228,#45229,#45230,#45231,#45232,#45233,#45234,
#45235,#45236,#45237,#45238,#45239,#45240,#45241,#45242,#45243,#45244,#45245,
#45246,#45247,#45248,#45249,#45250,#45251,#45252,#45253,#45254,#45255,#45256,
#45257,#45258,#45259,#45260,#45261,#45262,#45263,#45264,#45265,#45266,#45267,
#45268,#45269,#45270,#45271,#45272,#45273,#45274,#45275,#45276,#45277,#45278,
#45279,#45280,#45281,#45282,#45283,#45284,#45285,#45286,#45287,#45288,#45289,
#45290,#45291,#45292,#45293,#45294,#45295,#45296,#45297,#45298,#45299,#45300,
#45301,#45302,#45303,#45304,#45305,#45306,#45307,#45308,#45309,#45310,#45311,
#45312,#45313,#45314,#45315,#45316,#45317,#45318,#45319,#45320,#45321,#45322,
#45323,#45324,#45325,#45326,#45327,#45328,#45329,#45330,#45331,#45332,#45333,
#45334,#45335,#45336,#45337,#45338,#45339,#45340,#45341,#45342,#45343,#45344,
#45345,#45346,#45347,#45348,#45349,#45350,#45351,#45352,#45353,#45354,#45355,
#45356,#45357,#45358,#45359,#45360,#45361,#45362,#45363,#45364,#45365,#45366,
#45367,#45368,#45369,#45370,#45371,#45372,#45373,#45374,#45375,#45376,#45377,
#45378,#45379,#45380,#45381,#45382,#45383,#45384,#45385,#45386,#45387,#45388,
#45389,#45390,#45391,#45392,#45393,#45394,#45395,#45396,#45397,#45398,#45399,
#45400,#45401,#45402,#45403,#45404,#45405,#45406,#45407,#45408,#45409,#45410,
#45411,#45412,#45413,#45414,#45415,#45416,#45417,#45418,#45419,#45420,#45421,
#45422,#45423,#45424,#45425,#45426,#45427,#45428,#45429,#45430,#45431,#45432,
#45433,#45434,#45435,#45436,#45437,#45438,#45439,#45440,#45441,#45442,#45443,
#45444,#45445,#45446,#45447,#45448,#45449,#45450,#45451,#45452,#45453,#45454,
#45455,#45456,#45457,#45458,#45459,#45460,#45461,#45462,#45463,#45464,#45465,
#45466,#45467,#45468,#45469,#45470,#45471,#45472,#45473,#45474,#45475,#45476,
#45477,#45478,#45479,#45480,#45481,#45482,#45483,#45484,#45485,#45486,#45487,
#45488,#45489,#45490,#45491,#45492,#45493,#45494,#45495,#45496,#45497,#45498,
#45499,#45500,#45501,#45502,#45503,#45504,#45505,#45506,#45507,#45508,#45509,
#45510,#45511,#45512,#45513,#45514,#45515,#45516,#45517,#45518,#45519,#45520,
#45521,#45522,#45523,#45524,#45525,#45526,#45527,#45528,#45529,#45530,#45531,
#45532,#45533,#45534,#45535,#45536,#45537,#45538,#45539,#45540,#45541,#45542,
#45543,#45544,#45545,#45546,#45547,#45548,#45549,#45550,#45551,#45552,#45553,
#45554,#45555,#45556,#45557,#45558,#45559,#45560,#45561,#45562,#45563,#45564,
#45565,#45566,#45567,#45568,#45569,#45570,#45571,#45572,#45573,#45574,#45575,
#45576,#45577,#45578,#45579,#45580,#45581,#45582,#45583,#45584,#45585,#45586,
#45587,#45588,#45589,#45590,#45591,#45592,#45593,#45594,#45595,#45596,#45597,
#45598,#45599,#45600,#45601,#45602,#45603,#45604,#45605,#45606,#45607,#45608,
#45609,#45610,#45611,#45612,#45613,#45614,#45615,#45616,#45617,#45618,#45619,
#45620,#45621,#45622,#45623,#45624,#45625,#45626,#45627,#45628,#45629,#45630,
#45631,#45632,#45633,#45634,#45635,#45636,#45637,#45638,#45639,#45640,#45641,
#45642,#45643,#45644,#45645,#45646,#45647,#45648,#45649,#45650,#45651,#45652,
#45653,#45654,#45655,#45656,#45657,#45658,#45659,#45660),(#45661,#45662,
#45663,#45664,#45665,#45666,#45667,#45668,#45669,#45670,#45671,#45672,#45673,
#45674,#45675,#45676,#45677,#45678,#45679,#45680,#45681,#45682,#45683,#45684,
#45685,#45686,#45687,#45688,#45689,#45690,#45691,#45692,#45693,#45694,#45695,
#45696,#45697,#45698,#45699,#45700,#45701,#45702,#45703,#45704,#45705,#45706,
#45707,#45708,#45709,#45710,#45711,#45712,#45713,#45714,#45715,#45716,#45717,
#45718,#45719,#45720,#45721,#45722,#45723,#45724,#45725,#45726,#45727,#45728,
#45729,#45730,#45731,#45732,#45733,#45734,#45735,#45736,#45737,#45738,#45739,
#45740,#45741,#45742,#45743,#45744,#45745,#45746,#45747,#45748,#45749,#45750,
#45751,#45752,#45753,#45754,#45755,#45756,#45757,#45758,#45759,#45760,#45761,
#45762,#45763,#45764,#45765,#45766,#45767,#45768,#45769,#45770,#45771,#45772,
#45773,#45774,#45775,#45776,#45777,#45778,#45779,#45780,#45781,#45782,#45783,
#45784,#45785,#45786,#45787,#45788,#45789,#45790,#45791,#45792,#45793,#45794,
#45795,#45796,#45797,#45798,#45799,#45800,#45801,#45802,#45803,#45804,#45805,
#45806,#45807,#45808,#45809,#45810,#45811,#45812,#45813,#45814,#45815,#45816,
#45817,#45818,#45819,#45820,#45821,#45822,#45823,#45824,#45825,#45826,#45827,
#45828,#45829,#45830,#45831,#45832,#45833,#45834,#45835,#45836,#45837,#45838,
#45839,#45840,#45841,#45842,#45843,#45844,#45845,#45846,#45847,#45848,#45849,
#45850,#45851,#45852,#45853,#45854,#45855,#45856,#45857,#45858,#45859,#45860,
#45861,#45862,#45863,#45864,#45865,#45866,#45867,#45868,#45869,#45870,#45871,
#45872,#45873,#45874,#45875,#45876,#45877,#45878,#45879,#45880,#45881,#45882,
#45883,#45884,#45885,#45886,#45887,#45888,#45889,#45890,#45891,#45892,#45893,
#45894,#45895,#45896,#45897,#45898,#45899,#45900,#45901,#45902,#45903,#45904,
#45905,#45906,#45907,#45908,#45909,#45910,#45911,#45912,#45913,#45914,#45915,
#45916,#45917,#45918,#45919,#45920,#45921,#45922,#45923,#45924,#45925,#45926,
#45927,#45928,#45929,#45930,#45931,#45932,#45933,#45934,#45935,#45936,#45937,
#45938,#45939,#45940,#45941,#45942,#45943,#45944,#45945,#45946,#45947,#45948,
#45949,#45950,#45951,#45952,#45953,#45954,#45955,#45956,#45957,#45958,#45959,
#45960,#45961,#45962,#45963,#45964,#45965,#45966,#45967,#45968,#45969,#45970,
#45971,#45972,#45973,#45974,#45975,#45976,#45977,#45978,#45979,#45980,#45981,
#45982,#45983,#45984,#45985,#45986,#45987,#45988,#45989,#45990,#45991,#45992,
#45993,#45994,#45995,#45996,#45997,#45998,#45999,#46000,#46001,#46002,#46003,
#46004,#46005,#46006,#46007,#46008,#46009,#46010,#46011,#46012,#46013,#46014,
#46015,#46016,#46017,#46018,#46019,#46020,#46021,#46022,#46023,#46024,#46025,
#46026,#46027,#46028,#46029,#46030,#46031,#46032,#46033,#46034,#46035,#46036,
#46037,#46038,#46039,#46040,#46041,#46042,#46043,#46044,#46045,#46046,#46047,
#46048,#46049,#46050,#46051,#46052,#46053,#46054,#46055,#46056,#46057,#46058,
#46059,#46060,#46061,#46062,#46063,#46064,#46065,#46066,#46067,#46068,#46069,
#46070,#46071,#46072,#46073,#46074,#46075,#46076,#46077,#46078,#46079,#46080,
#46081,#46082,#46083,#46084,#46085,#46086,#46087,#46088,#46089,#46090,#46091,
#46092,#46093,#46094,#46095,#46096,#46097,#46098,#46099,#46100,#46101,#46102,
#46103,#46104,#46105,#46106,#46107,#46108,#46109,#46110,#46111,#46112,#46113,
#46114,#46115,#46116,#46117,#46118,#46119,#46120,#46121,#46122,#46123,#46124,
#46125,#46126,#46127,#46128,#46129,#46130,#46131,#46132,#46133,#46134,#46135,
#46136,#46137,#46138,#46139,#46140,#46141,#46142,#46143,#46144,#46145,#46146,
#46147,#46148,#46149,#46150,#46151,#46152,#46153,#46154,#46155,#46156,#46157),
(#46158,#46159,#46160,#46161,#46162,#46163,#46164,#46165,#46166,#46167,
#46168,#46169,#46170,#46171,#46172,#46173,#46174,#46175,#46176,#46177,#46178,
#46179,#46180,#46181,#46182,#46183,#46184,#46185,#46186,#46187,#46188,#46189,
#46190,#46191,#46192,#46193,#46194,#46195,#46196,#46197,#46198,#46199,#46200,
#46201,#46202,#46203,#46204,#46205,#46206,#46207,#46208,#46209,#46210,#46211,
#46212,#46213,#46214,#46215,#46216,#46217,#46218,#46219,#46220,#46221,#46222,
#46223,#46224,#46225,#46226,#46227,#46228,#46229,#46230,#46231,#46232,#46233,
#46234,#46235,#46236,#46237,#46238,#46239,#46240,#46241,#46242,#46243,#46244,
#46245,#46246,#46247,#46248,#46249,#46250,#46251,#46252,#46253,#46254,#46255,
#46256,#46257,#46258,#46259,#46260,#46261,#46262,#46263,#46264,#46265,#46266,
#46267,#46268,#46269,#46270,#46271,#46272,#46273,#46274,#46275,#46276,#46277,
#46278,#46279,#46280,#46281,#46282,#46283,#46284,#46285,#46286,#46287,#46288,
#46289,#46290,#46291,#46292,#46293,#46294,#46295,#46296,#46297,#46298,#46299,
#46300,#46301,#46302,#46303,#46304,#46305,#46306,#46307,#46308,#46309,#46310,
#46311,#46312,#46313,#46314,#46315,#46316,#46317,#46318,#46319,#46320,#46321,
#46322,#46323,#46324,#46325,#46326,#46327,#46328,#46329,#46330,#46331,#46332,
#46333,#46334,#46335,#46336,#46337,#46338,#46339,#46340,#46341,#46342,#46343,
#46344,#46345,#46346,#46347,#46348,#46349,#46350,#46351,#46352,#46353,#46354,
#46355,#46356,#46357,#46358,#46359,#46360,#46361,#46362,#46363,#46364,#46365,
#46366,#46367,#46368,#46369,#46370,#46371,#46372,#46373,#46374,#46375,#46376,
#46377,#46378,#46379,#46380,#46381,#46382,#46383,#46384,#46385,#46386,#46387,
#46388,#46389,#46390,#46391,#46392,#46393,#46394,#46395,#46396,#46397,#46398,
#46399,#46400,#46401,#46402,#46403,#46404,#46405,#46406,#46407,#46408,#46409,
#46410,#46411,#46412,#46413,#46414,#46415,#46416,#46417,#46418,#46419,#46420,
#46421,#46422,#46423,#46424,#46425,#46426,#46427,#46428,#46429,#46430,#46431,
#46432,#46433,#46434,#46435,#46436,#46437,#46438,#46439,#46440,#46441,#46442,
#46443,#46444,#46445,#46446,#46447,#46448,#46449,#46450,#46451,#46452,#46453,
#46454,#46455,#46456,#46457,#46458,#46459,#46460,#46461,#46462,#46463,#46464,
#46465,#46466,#46467,#46468,#46469,#46470,#46471,#46472,#46473,#46474,#46475,
#46476,#46477,#46478,#46479,#46480,#46481,#46482,#46483,#46484,#46485,#46486,
#46487,#46488,#46489,#46490,#46491,#46492,#46493,#46494,#46495,#46496,#46497,
#46498,#46499,#46500,#46501,#46502,#46503,#46504,#46505,#46506,#46507,#46508,
#46509,#46510,#46511,#46512,#46513,#46514,#46515,#46516,#46517,#46518,#46519,
#46520,#46521,#46522,#46523,#46524,#46525,#46526,#46527,#46528,#46529,#46530,
#46531,#46532,#46533,#46534,#46535,#46536,#46537,#46538,#46539,#46540,#46541,
#46542,#46543,#46544,#46545,#46546,#46547,#46548,#46549,#46550,#46551,#46552,
#46553,#46554,#46555,#46556,#46557,#46558,#46559,#46560,#46561,#46562,#46563,
#46564,#46565,#46566,#46567,#46568,#46569,#46570,#46571,#46572,#46573,#46574,
#46575,#46576,#46577,#46578,#46579,#46580,#46581,#46582,#46583,#46584,#46585,
#46586,#46587,#46588,#46589,#46590,#46591,#46592,#46593,#46594,#46595,#46596,
#46597,#46598,#46599,#46600,#46601,#46602,#46603,#46604,#46605,#46606,#46607,
#46608,#46609,#46610,#46611,#46612,#46613,#46614,#46615,#46616,#46617,#46618,
#46619,#46620,#46621,#46622,#46623,#46624,#46625,#46626,#46627,#46628,#46629,
#46630,#46631,#46632,#46633,#46634,#46635,#46636,#46637,#46638,#46639,#46640,
#46641,#46642,#46643,#46644,#46645,#46646,#46647,#46648,#46649,#46650,#46651,
#46652,#46653,#46654),(#46655,#46656,#46657,#46658,#46659,#46660,#46661,
#46662,#46663,#46664,#46665,#46666,#46667,#46668,#46669,#46670,#46671,#46672,
#46673,#46674,#46675,#46676,#46677,#46678,#46679,#46680,#46681,#46682,#46683,
#46684,#46685,#46686,#46687,#46688,#46689,#46690,#46691,#46692,#46693,#46694,
#46695,#46696,#46697,#46698,#46699,#46700,#46701,#46702,#46703,#46704,#46705,
#46706,#46707,#46708,#46709,#46710,#46711,#46712,#46713,#46714,#46715,#46716,
#46717,#46718,#46719,#46720,#46721,#46722,#46723,#46724,#46725,#46726,#46727,
#46728,#46729,#46730,#46731,#46732,#46733,#46734,#46735,#46736,#46737,#46738,
#46739,#46740,#46741,#46742,#46743,#46744,#46745,#46746,#46747,#46748,#46749,
#46750,#46751,#46752,#46753,#46754,#46755,#46756,#46757,#46758,#46759,#46760,
#46761,#46762,#46763,#46764,#46765,#46766,#46767,#46768,#46769,#46770,#46771,
#46772,#46773,#46774,#46775,#46776,#46777,#46778,#46779,#46780,#46781,#46782,
#46783,#46784,#46785,#46786,#46787,#46788,#46789,#46790,#46791,#46792,#46793,
#46794,#46795,#46796,#46797,#46798,#46799,#46800,#46801,#46802,#46803,#46804,
#46805,#46806,#46807,#46808,#46809,#46810,#46811,#46812,#46813,#46814,#46815,
#46816,#46817,#46818,#46819,#46820,#46821,#46822,#46823,#46824,#46825,#46826,
#46827,#46828,#46829,#46830,#46831,#46832,#46833,#46834,#46835,#46836,#46837,
#46838,#46839,#46840,#46841,#46842,#46843,#46844,#46845,#46846,#46847,#46848,
#46849,#46850,#46851,#46852,#46853,#46854,#46855,#46856,#46857,#46858,#46859,
#46860,#46861,#46862,#46863,#46864,#46865,#46866,#46867,#46868,#46869,#46870,
#46871,#46872,#46873,#46874,#46875,#46876,#46877,#46878,#46879,#46880,#46881,
#46882,#46883,#46884,#46885,#46886,#46887,#46888,#46889,#46890,#46891,#46892,
#46893,#46894,#46895,#46896,#46897,#46898,#46899,#46900,#46901,#46902,#46903,
#46904,#46905,#46906,#46907,#46908,#46909,#46910,#46911,#46912,#46913,#46914,
#46915,#46916,#46917,#46918,#46919,#46920,#46921,#46922,#46923,#46924,#46925,
#46926,#46927,#46928,#46929,#46930,#46931,#46932,#46933,#46934,#46935,#46936,
#46937,#46938,#46939,#46940,#46941,#46942,#46943,#46944,#46945,#46946,#46947,
#46948,#46949,#46950,#46951,#46952,#46953,#46954,#46955,#46956,#46957,#46958,
#46959,#46960,#46961,#46962,#46963,#46964,#46965,#46966,#46967,#46968,#46969,
#46970,#46971,#46972,#46973,#46974,#46975,#46976,#46977,#46978,#46979,#46980,
#46981,#46982,#46983,#46984,#46985,#46986,#46987,#46988,#46989,#46990,#46991,
#46992,#46993,#46994,#46995,#46996,#46997,#46998,#46999,#47000,#47001,#47002,
#47003,#47004,#47005,#47006,#47007,#47008,#47009,#47010,#47011,#47012,#47013,
#47014,#47015,#47016,#47017,#47018,#47019,#47020,#47021,#47022,#47023,#47024,
#47025,#47026,#47027,#47028,#47029,#47030,#47031,#47032,#47033,#47034,#47035,
#47036,#47037,#47038,#47039,#47040,#47041,#47042,#47043,#47044,#47045,#47046,
#47047,#47048,#47049,#47050,#47051,#47052,#47053,#47054,#47055,#47056,#47057,
#47058,#47059,#47060,#47061,#47062,#47063,#47064,#47065,#47066,#47067,#47068,
#47069,#47070,#47071,#47072,#47073,#47074,#47075,#47076,#47077,#47078,#47079,
#47080,#47081,#47082,#47083,#47084,#47085,#47086,#47087,#47088,#47089,#47090,
#47091,#47092,#47093,#47094,#47095,#47096,#47097,#47098,#47099,#47100,#47101,
#47102,#47103,#47104,#47105,#47106,#47107,#47108,#47109,#47110,#47111,#47112,
#47113,#47114,#47115,#47116,#47117,#47118,#47119,#47120,#47121,#47122,#47123,
#47124,#47125,#47126,#47127,#47128,#47129,#47130,#47131,#47132,#47133,#47134,
#47135,#47136,#47137,#47138,#47139,#47140,#47141,#47142,#47143,#47144,#47145,
#47146,#47147,#47148,#47149,#47150,#47151)),.UNSPECIFIED.,.F.,.F.,.F.,(4,
4),(4,1,1,1,1,1,1,1,1,1,1,1,1,1,1,1,1,1,1,1,1,1,1,1,1,1,1,1,1,1,1,1,1,1,
1,1,1,1,1,1,1,1,1,1,1,1,1,1,1,1,1,1,1,1,1,1,1,1,1,1,1,1,1,1,1,1,1,1,1,1,
1,1,1,1,1,1,1,1,1,1,1,1,1,1,1,1,1,1,1,1,1,1,1,1,1,1,1,1,1,1,1,1,1,1,1,1,
1,1,1,1,1,1,1,1,1,1,1,1,1,1,1,1,1,1,1,1,1,1,1,1,1,1,1,1,1,1,1,1,1,1,1,1,
1,1,1,1,1,1,1,1,1,1,1,1,1,1,1,1,1,1,1,1,1,1,1,1,1,1,1,1,1,1,1,1,1,1,1,1,
1,1,1,1,1,1,1,1,1,1,1,1,1,1,1,1,1,1,1,1,1,1,1,1,1,1,1,1,1,1,1,1,1,1,1,1,
1,1,1,1,1,1,1,1,1,1,1,1,1,1,1,1,1,1,1,1,1,1,1,1,1,1,1,1,1,1,1,1,1,1,1,1,
1,1,1,1,1,1,1,1,1,1,1,1,1,1,1,1,1,1,1,1,1,1,1,1,1,1,1,1,1,1,1,1,1,1,1,1,
1,1,1,1,1,1,1,1,1,1,1,1,1,1,1,1,1,1,1,1,1,1,1,1,1,1,1,1,1,1,1,1,1,1,1,1,
1,1,1,1,1,1,1,1,1,1,1,1,1,1,1,1,1,1,1,1,1,1,1,1,1,1,1,1,1,1,1,1,1,1,1,1,
1,1,1,1,1,1,1,1,1,1,1,1,1,1,1,1,1,1,1,1,1,1,1,1,1,1,1,1,1,1,1,1,1,1,1,1,
1,1,1,1,1,1,1,1,1,1,1,1,1,1,1,1,1,1,1,1,1,1,1,1,1,1,1,1,1,1,1,1,1,1,1,1,
1,1,1,1,1,1,1,1,1,1,1,1,1,1,1,1,1,1,1,1,1,1,1,1,1,1,1,1,1,1,1,1,1,1,1,1,
1,1,1,1,1,1,1,1,1,1,1,1,1,1,1,1,1,1,1,1,1,1,1,1,1,1,1,1,4),(-1.54457385216123E-14,
0.236198260560645),(12.043305083964,12.5421366924057,13.0409683008475,13.5397999092893,
14.0386315177311,14.5374631261729,15.0362947346147,15.5351263430564,16.0339579514982,
17.0316211683818,17.5304527768236,18.0292843852654,18.5281159937072,19.0269476021489,
19.5257792105907,20.0246108190325,20.5234424274743,21.0222740359161,21.5211056443579,
22.0199372527997,22.5187688612414,23.0176004696832,24.0152636865668,24.5140952950086,
25.0129269034504,25.5117585118921,26.0105901203339,26.5094217287757,27.0082533372175,
27.5070849456593,28.0059165541011,28.5047481625429,29.0035797709846,29.5024113794264,
30.0012429878682,30.9989062047518,31.4977378131936,31.9965694216353,32.4954010300771,
32.9942326385189,33.4930642469607,33.9918958554025,34.4907274638443,34.9895590722861,
35.4883906807278,35.9872222891696,36.4860538976114,36.9848855060532,37.9825487229368,
38.4813803313785,38.9802119398203,39.4790435482621,39.9778751567039,40.4767067651457,
40.9755383735875,41.4743699820293,41.973201590471,42.4720331989128,42.9708648073546,
43.4696964157964,43.9685280242382,44.9661912411217,45.4650228495635,45.9638544580053,
46.4626860664471,46.9615176748889,47.4603492833307,47.9591808917725,48.4580125002142,
48.956844108656,49.4556757170978,49.9545073255396,50.4533389339814,50.9521705424232,
51.9498337593067,52.4486653677485,52.9474969761903,53.4463285846321,53.9451601930739,
54.4439918015157,54.9428234099574,55.4416550183992,55.940486626841,56.4393182352828,
56.9381498437246,57.4369814521664,57.9358130606082,58.9334762774917,59.4323078859335,
59.9311394943753,60.4299711028171,60.9288027112589,61.4276343197006,61.9264659281424,
62.4252975365842,62.924129145026,63.4229607534678,63.9217923619096,64.4206239703514,
64.9194555787931,65.9171187956767,66.4159504041185,66.9147820125603,67.4136136210021,
67.9124452294438,68.4112768378856,68.9101084463274,69.4089400547692,69.907771663211,
70.4066032716528,70.9054348800946,71.4042664885363,71.9030980969781,72.9007613138617,
73.3995929223035,73.8984245307453,74.397256139187,74.8960877476288,75.3949193560706,
75.8937509645124,76.3925825729542,76.891414181396,77.3902457898378,77.8890773982795,
78.3879090067213,78.8867406151631,79.8844038320467,80.3832354404885,80.8820670489303,
81.380898657372,81.8797302658138,82.3785618742556,82.8773934826974,83.3762250911392,
83.875056699581,84.3738883080227,84.8727199164645,85.3715515249063,85.8703831333481,
86.8680463502317,87.3668779586735,87.8657095671152,88.364541175557,88.8633727839988,
89.3622043924406,89.8610360008824,90.3598676093242,90.8586992177659,91.3575308262077,
91.8563624346495,92.3551940430913,92.8540256515331,93.8516888684167,94.3505204768584,
94.8493520853002,95.348183693742,95.8470153021838,96.3458469106256,96.8446785190674,
97.3435101275091,97.8423417359509,98.3411733443927,98.8400049528345,99.3388365612763,
99.8376681697181,100.835331386602,101.334162995043,101.832994603485,102.331826211927,
102.830657820369,103.329489428811,103.828321037252,104.327152645694,104.825984254136,
105.324815862578,105.823647471019,106.322479079461,106.821310687903,107.818973904787,
108.317805513228,108.81663712167,109.315468730112,109.814300338554,110.313131946996,
110.811963555437,111.310795163879,111.809626772321,112.308458380763,112.807289989204,
113.306121597646,113.804953206088,114.802616422972,115.301448031413,115.800279639855,
116.299111248297,116.797942856739,117.296774465181,117.795606073622,118.294437682064,
118.793269290506,119.292100898948,119.790932507389,120.289764115831,120.788595724273,
121.786258941157,122.285090549598,122.78392215804,123.282753766482,123.781585374924,
124.280416983366,124.779248591807,125.278080200249,125.776911808691,126.275743417133,
126.774575025574,127.273406634016,127.772238242458,128.769901459342,129.268733067783,
129.767564676225,130.266396284667,130.765227893109,131.26405950155,131.762891109992,
132.261722718434,132.760554326876,133.259385935318,133.758217543759,134.257049152201,
134.755880760643,135.753543977527,136.252375585968,136.75120719441,137.250038802852,
137.748870411294,138.247702019735,138.746533628177,139.245365236619,139.744196845061,
140.243028453503,140.741860061944,141.240691670386,141.739523278828,142.737186495712,
143.236018104153,143.734849712595,144.233681321037,144.732512929479,145.231344537921,
145.730176146362,146.229007754804,146.727839363246,147.725502580129,148.224334188571,
148.723165797013,149.221997405455,149.720829013897,150.219660622338,150.71849223078,
151.217323839222,151.716155447664,152.214987056105,152.713818664547,153.212650272989,
153.711481881431,154.709145098314,155.207976706756,155.706808315198,156.20563992364,
156.704471532082,157.203303140523,157.702134748965,158.200966357407,158.699797965849,
159.19862957429,159.697461182732,160.196292791174,160.695124399616,161.692787616499,
162.191619224941,162.690450833383,163.189282441825,163.688114050267,164.186945658708,
164.68577726715,165.184608875592,165.683440484034,166.182272092475,166.681103700917,
167.179935309359,167.678766917801,168.676430134684,169.175261743126,169.674093351568,
170.17292496001,170.671756568452,171.170588176893,171.669419785335,172.168251393777,
172.667083002219,173.16591461066,173.664746219102,174.163577827544,174.662409435986,
175.660072652869,176.158904261311,176.657735869753,177.156567478195,177.655399086636,
178.154230695078,178.65306230352,179.151893911962,179.650725520404,180.149557128845,
180.648388737287,181.147220345729,181.646051954171,182.643715171054,183.142546779496,
183.641378387938,184.14020999638,184.639041604821,185.137873213263,185.636704821705,
186.135536430147,186.634368038589,187.13319964703,187.632031255472,188.130862863914,
188.629694472356,189.627357689239,190.126189297681,190.625020906123,191.123852514565,
191.622684123006,192.121515731448,192.62034733989,193.119178948332,193.618010556774,
194.116842165215,194.615673773657,195.114505382099,195.613336990541,196.611000207424,
197.109831815866,197.608663424308,198.10749503275,198.606326641191,199.105158249633,
199.603989858075,200.102821466517,200.601653074959,201.1004846834,201.599316291842,
202.098147900284,202.596979508726,203.594642725609,204.093474334051,204.592305942493,
205.091137550935,205.589969159376,206.088800767818,206.58763237626,207.086463984702,
207.585295593144,208.084127201585,208.582958810027,209.081790418469,209.580622026911,
210.578285243794,211.077116852236,211.575948460678,212.07478006912,212.573611677561,
213.072443286003,213.571274894445,214.070106502887,214.568938111329,215.06776971977,
215.566601328212,216.065432936654,216.564264545096,217.561927761979,218.060759370421,
218.559590978863,219.058422587305,219.557254195746,220.056085804188,220.55491741263,
221.053749021072,221.552580629514,222.051412237955,222.550243846397,223.049075454839,
223.547907063281,224.545570280164,225.044401888606,225.543233497048,226.04206510549,
226.540896713931,227.039728322373,227.538559930815,228.037391539257,228.536223147699,
229.03505475614,229.533886364582,230.032717973024,230.531549581466,231.529212798349,
232.028044406791,232.526876015233,233.025707623675,233.524539232116,234.023370840558,
234.522202449,235.021034057442,235.519865665884,236.018697274325,236.517528882767,
237.016360491209,237.515192099651,238.512855316534,239.011686924976,239.510518533418,
240.00935014186,240.508181750301,241.007013358743,241.505844967185,242.004676575627,
242.503508184069,243.00233979251,243.501171400952,244.000003009394,244.498834617836,
245.496497834719,245.995329443161,246.494161051603,246.992992660045,247.491824268486,
247.990655876928,248.48948748537,248.988319093812,249.487150702254,249.985982310695,
250.484813919137,250.983645527579,251.482477136021,252.480140352904,252.978971961346,
253.477803569788,253.97663517823,254.475466786671,254.974298395113,255.473130003555,
255.971961611997,256.470793220438,256.96962482888,257.468456437322,257.967288045764,
258.466119654206,259.463782871089,259.962614479531,260.461446087973,260.960277696415,
261.459109304856,261.957940913298,262.45677252174,262.955604130182,263.454435738623,
263.953267347065,264.452098955507,264.950930563949,265.449762172391,266.447425389274,
266.946256997716,267.445088606158,267.9439202146,268.442751823041,268.941583431483,
269.440415039925,269.939246648367,270.438078256808,270.93690986525,271.435741473692,
271.934573082134,272.433404690576,273.431067907459,273.929899515901,274.428731124343,
274.927562732785,275.426394341226,275.925225949668,276.42405755811,276.922889166552,
277.421720774993),.UNSPECIFIED.);
#159=B_SPLINE_SURFACE_WITH_KNOTS('',3,3,((#47328,#47329,#47330,#47331,#47332,
#47333,#47334,#47335,#47336,#47337,#47338,#47339,#47340,#47341,#47342,#47343,
#47344,#47345,#47346,#47347,#47348,#47349,#47350,#47351,#47352,#47353,#47354,
#47355,#47356,#47357,#47358,#47359,#47360,#47361,#47362,#47363,#47364,#47365,
#47366,#47367,#47368,#47369,#47370,#47371,#47372,#47373,#47374,#47375,#47376,
#47377,#47378,#47379,#47380,#47381,#47382,#47383,#47384,#47385,#47386,#47387,
#47388,#47389,#47390,#47391,#47392,#47393,#47394,#47395,#47396,#47397,#47398,
#47399,#47400,#47401,#47402,#47403,#47404,#47405,#47406,#47407,#47408,#47409,
#47410,#47411,#47412,#47413,#47414,#47415,#47416,#47417,#47418,#47419,#47420,
#47421,#47422,#47423,#47424,#47425,#47426,#47427,#47428,#47429,#47430,#47431,
#47432,#47433,#47434,#47435,#47436,#47437,#47438,#47439,#47440,#47441,#47442,
#47443,#47444,#47445,#47446,#47447,#47448,#47449,#47450,#47451,#47452,#47453,
#47454,#47455,#47456,#47457,#47458,#47459,#47460,#47461,#47462,#47463,#47464,
#47465,#47466,#47467,#47468,#47469,#47470,#47471,#47472,#47473,#47474,#47475,
#47476,#47477,#47478,#47479,#47480,#47481,#47482,#47483,#47484,#47485,#47486,
#47487,#47488,#47489,#47490,#47491,#47492,#47493,#47494,#47495,#47496,#47497,
#47498,#47499,#47500,#47501,#47502,#47503,#47504,#47505,#47506,#47507,#47508,
#47509,#47510,#47511,#47512,#47513,#47514,#47515,#47516,#47517,#47518,#47519,
#47520,#47521,#47522,#47523,#47524,#47525,#47526,#47527,#47528,#47529,#47530,
#47531,#47532,#47533,#47534,#47535,#47536,#47537,#47538,#47539,#47540,#47541,
#47542,#47543,#47544,#47545,#47546,#47547,#47548,#47549,#47550,#47551,#47552,
#47553,#47554,#47555,#47556,#47557,#47558,#47559,#47560,#47561,#47562,#47563,
#47564,#47565,#47566,#47567,#47568,#47569,#47570,#47571,#47572,#47573,#47574,
#47575,#47576,#47577,#47578,#47579,#47580,#47581,#47582,#47583,#47584,#47585,
#47586,#47587,#47588,#47589,#47590,#47591,#47592,#47593,#47594,#47595,#47596,
#47597,#47598,#47599,#47600,#47601,#47602,#47603,#47604,#47605,#47606,#47607,
#47608,#47609,#47610,#47611,#47612,#47613,#47614,#47615,#47616,#47617,#47618,
#47619,#47620,#47621,#47622,#47623,#47624,#47625,#47626,#47627,#47628,#47629,
#47630,#47631,#47632,#47633,#47634,#47635,#47636,#47637,#47638,#47639,#47640,
#47641,#47642,#47643,#47644,#47645,#47646,#47647,#47648,#47649,#47650,#47651,
#47652,#47653,#47654,#47655,#47656,#47657,#47658,#47659,#47660,#47661,#47662,
#47663,#47664,#47665,#47666,#47667,#47668,#47669,#47670,#47671,#47672,#47673,
#47674,#47675,#47676,#47677,#47678,#47679,#47680,#47681,#47682,#47683,#47684,
#47685,#47686,#47687,#47688,#47689,#47690,#47691,#47692,#47693,#47694,#47695,
#47696,#47697,#47698,#47699,#47700,#47701,#47702,#47703,#47704,#47705,#47706,
#47707,#47708,#47709,#47710,#47711,#47712,#47713,#47714,#47715,#47716,#47717,
#47718,#47719,#47720,#47721,#47722,#47723,#47724,#47725,#47726,#47727,#47728,
#47729,#47730,#47731,#47732,#47733,#47734,#47735,#47736,#47737,#47738,#47739,
#47740,#47741,#47742,#47743,#47744,#47745,#47746,#47747,#47748,#47749,#47750,
#47751,#47752,#47753,#47754,#47755,#47756,#47757,#47758,#47759,#47760,#47761,
#47762,#47763,#47764,#47765,#47766,#47767,#47768,#47769,#47770,#47771,#47772,
#47773,#47774,#47775,#47776,#47777,#47778,#47779,#47780,#47781,#47782,#47783,
#47784,#47785,#47786,#47787,#47788,#47789,#47790,#47791,#47792,#47793,#47794,
#47795,#47796,#47797,#47798,#47799,#47800,#47801,#47802,#47803,#47804,#47805,
#47806,#47807,#47808,#47809,#47810,#47811,#47812,#47813,#47814,#47815,#47816,
#47817,#47818,#47819,#47820,#47821,#47822,#47823,#47824,#47825,#47826,#47827,
#47828,#47829,#47830,#47831,#47832,#47833,#47834,#47835,#47836,#47837,#47838,
#47839,#47840,#47841,#47842,#47843,#47844,#47845,#47846,#47847,#47848,#47849,
#47850,#47851,#47852,#47853,#47854,#47855,#47856,#47857,#47858),(#47859,
#47860,#47861,#47862,#47863,#47864,#47865,#47866,#47867,#47868,#47869,#47870,
#47871,#47872,#47873,#47874,#47875,#47876,#47877,#47878,#47879,#47880,#47881,
#47882,#47883,#47884,#47885,#47886,#47887,#47888,#47889,#47890,#47891,#47892,
#47893,#47894,#47895,#47896,#47897,#47898,#47899,#47900,#47901,#47902,#47903,
#47904,#47905,#47906,#47907,#47908,#47909,#47910,#47911,#47912,#47913,#47914,
#47915,#47916,#47917,#47918,#47919,#47920,#47921,#47922,#47923,#47924,#47925,
#47926,#47927,#47928,#47929,#47930,#47931,#47932,#47933,#47934,#47935,#47936,
#47937,#47938,#47939,#47940,#47941,#47942,#47943,#47944,#47945,#47946,#47947,
#47948,#47949,#47950,#47951,#47952,#47953,#47954,#47955,#47956,#47957,#47958,
#47959,#47960,#47961,#47962,#47963,#47964,#47965,#47966,#47967,#47968,#47969,
#47970,#47971,#47972,#47973,#47974,#47975,#47976,#47977,#47978,#47979,#47980,
#47981,#47982,#47983,#47984,#47985,#47986,#47987,#47988,#47989,#47990,#47991,
#47992,#47993,#47994,#47995,#47996,#47997,#47998,#47999,#48000,#48001,#48002,
#48003,#48004,#48005,#48006,#48007,#48008,#48009,#48010,#48011,#48012,#48013,
#48014,#48015,#48016,#48017,#48018,#48019,#48020,#48021,#48022,#48023,#48024,
#48025,#48026,#48027,#48028,#48029,#48030,#48031,#48032,#48033,#48034,#48035,
#48036,#48037,#48038,#48039,#48040,#48041,#48042,#48043,#48044,#48045,#48046,
#48047,#48048,#48049,#48050,#48051,#48052,#48053,#48054,#48055,#48056,#48057,
#48058,#48059,#48060,#48061,#48062,#48063,#48064,#48065,#48066,#48067,#48068,
#48069,#48070,#48071,#48072,#48073,#48074,#48075,#48076,#48077,#48078,#48079,
#48080,#48081,#48082,#48083,#48084,#48085,#48086,#48087,#48088,#48089,#48090,
#48091,#48092,#48093,#48094,#48095,#48096,#48097,#48098,#48099,#48100,#48101,
#48102,#48103,#48104,#48105,#48106,#48107,#48108,#48109,#48110,#48111,#48112,
#48113,#48114,#48115,#48116,#48117,#48118,#48119,#48120,#48121,#48122,#48123,
#48124,#48125,#48126,#48127,#48128,#48129,#48130,#48131,#48132,#48133,#48134,
#48135,#48136,#48137,#48138,#48139,#48140,#48141,#48142,#48143,#48144,#48145,
#48146,#48147,#48148,#48149,#48150,#48151,#48152,#48153,#48154,#48155,#48156,
#48157,#48158,#48159,#48160,#48161,#48162,#48163,#48164,#48165,#48166,#48167,
#48168,#48169,#48170,#48171,#48172,#48173,#48174,#48175,#48176,#48177,#48178,
#48179,#48180,#48181,#48182,#48183,#48184,#48185,#48186,#48187,#48188,#48189,
#48190,#48191,#48192,#48193,#48194,#48195,#48196,#48197,#48198,#48199,#48200,
#48201,#48202,#48203,#48204,#48205,#48206,#48207,#48208,#48209,#48210,#48211,
#48212,#48213,#48214,#48215,#48216,#48217,#48218,#48219,#48220,#48221,#48222,
#48223,#48224,#48225,#48226,#48227,#48228,#48229,#48230,#48231,#48232,#48233,
#48234,#48235,#48236,#48237,#48238,#48239,#48240,#48241,#48242,#48243,#48244,
#48245,#48246,#48247,#48248,#48249,#48250,#48251,#48252,#48253,#48254,#48255,
#48256,#48257,#48258,#48259,#48260,#48261,#48262,#48263,#48264,#48265,#48266,
#48267,#48268,#48269,#48270,#48271,#48272,#48273,#48274,#48275,#48276,#48277,
#48278,#48279,#48280,#48281,#48282,#48283,#48284,#48285,#48286,#48287,#48288,
#48289,#48290,#48291,#48292,#48293,#48294,#48295,#48296,#48297,#48298,#48299,
#48300,#48301,#48302,#48303,#48304,#48305,#48306,#48307,#48308,#48309,#48310,
#48311,#48312,#48313,#48314,#48315,#48316,#48317,#48318,#48319,#48320,#48321,
#48322,#48323,#48324,#48325,#48326,#48327,#48328,#48329,#48330,#48331,#48332,
#48333,#48334,#48335,#48336,#48337,#48338,#48339,#48340,#48341,#48342,#48343,
#48344,#48345,#48346,#48347,#48348,#48349,#48350,#48351,#48352,#48353,#48354,
#48355,#48356,#48357,#48358,#48359,#48360,#48361,#48362,#48363,#48364,#48365,
#48366,#48367,#48368,#48369,#48370,#48371,#48372,#48373,#48374,#48375,#48376,
#48377,#48378,#48379,#48380,#48381,#48382,#48383,#48384,#48385,#48386,#48387,
#48388,#48389),(#48390,#48391,#48392,#48393,#48394,#48395,#48396,#48397,
#48398,#48399,#48400,#48401,#48402,#48403,#48404,#48405,#48406,#48407,#48408,
#48409,#48410,#48411,#48412,#48413,#48414,#48415,#48416,#48417,#48418,#48419,
#48420,#48421,#48422,#48423,#48424,#48425,#48426,#48427,#48428,#48429,#48430,
#48431,#48432,#48433,#48434,#48435,#48436,#48437,#48438,#48439,#48440,#48441,
#48442,#48443,#48444,#48445,#48446,#48447,#48448,#48449,#48450,#48451,#48452,
#48453,#48454,#48455,#48456,#48457,#48458,#48459,#48460,#48461,#48462,#48463,
#48464,#48465,#48466,#48467,#48468,#48469,#48470,#48471,#48472,#48473,#48474,
#48475,#48476,#48477,#48478,#48479,#48480,#48481,#48482,#48483,#48484,#48485,
#48486,#48487,#48488,#48489,#48490,#48491,#48492,#48493,#48494,#48495,#48496,
#48497,#48498,#48499,#48500,#48501,#48502,#48503,#48504,#48505,#48506,#48507,
#48508,#48509,#48510,#48511,#48512,#48513,#48514,#48515,#48516,#48517,#48518,
#48519,#48520,#48521,#48522,#48523,#48524,#48525,#48526,#48527,#48528,#48529,
#48530,#48531,#48532,#48533,#48534,#48535,#48536,#48537,#48538,#48539,#48540,
#48541,#48542,#48543,#48544,#48545,#48546,#48547,#48548,#48549,#48550,#48551,
#48552,#48553,#48554,#48555,#48556,#48557,#48558,#48559,#48560,#48561,#48562,
#48563,#48564,#48565,#48566,#48567,#48568,#48569,#48570,#48571,#48572,#48573,
#48574,#48575,#48576,#48577,#48578,#48579,#48580,#48581,#48582,#48583,#48584,
#48585,#48586,#48587,#48588,#48589,#48590,#48591,#48592,#48593,#48594,#48595,
#48596,#48597,#48598,#48599,#48600,#48601,#48602,#48603,#48604,#48605,#48606,
#48607,#48608,#48609,#48610,#48611,#48612,#48613,#48614,#48615,#48616,#48617,
#48618,#48619,#48620,#48621,#48622,#48623,#48624,#48625,#48626,#48627,#48628,
#48629,#48630,#48631,#48632,#48633,#48634,#48635,#48636,#48637,#48638,#48639,
#48640,#48641,#48642,#48643,#48644,#48645,#48646,#48647,#48648,#48649,#48650,
#48651,#48652,#48653,#48654,#48655,#48656,#48657,#48658,#48659,#48660,#48661,
#48662,#48663,#48664,#48665,#48666,#48667,#48668,#48669,#48670,#48671,#48672,
#48673,#48674,#48675,#48676,#48677,#48678,#48679,#48680,#48681,#48682,#48683,
#48684,#48685,#48686,#48687,#48688,#48689,#48690,#48691,#48692,#48693,#48694,
#48695,#48696,#48697,#48698,#48699,#48700,#48701,#48702,#48703,#48704,#48705,
#48706,#48707,#48708,#48709,#48710,#48711,#48712,#48713,#48714,#48715,#48716,
#48717,#48718,#48719,#48720,#48721,#48722,#48723,#48724,#48725,#48726,#48727,
#48728,#48729,#48730,#48731,#48732,#48733,#48734,#48735,#48736,#48737,#48738,
#48739,#48740,#48741,#48742,#48743,#48744,#48745,#48746,#48747,#48748,#48749,
#48750,#48751,#48752,#48753,#48754,#48755,#48756,#48757,#48758,#48759,#48760,
#48761,#48762,#48763,#48764,#48765,#48766,#48767,#48768,#48769,#48770,#48771,
#48772,#48773,#48774,#48775,#48776,#48777,#48778,#48779,#48780,#48781,#48782,
#48783,#48784,#48785,#48786,#48787,#48788,#48789,#48790,#48791,#48792,#48793,
#48794,#48795,#48796,#48797,#48798,#48799,#48800,#48801,#48802,#48803,#48804,
#48805,#48806,#48807,#48808,#48809,#48810,#48811,#48812,#48813,#48814,#48815,
#48816,#48817,#48818,#48819,#48820,#48821,#48822,#48823,#48824,#48825,#48826,
#48827,#48828,#48829,#48830,#48831,#48832,#48833,#48834,#48835,#48836,#48837,
#48838,#48839,#48840,#48841,#48842,#48843,#48844,#48845,#48846,#48847,#48848,
#48849,#48850,#48851,#48852,#48853,#48854,#48855,#48856,#48857,#48858,#48859,
#48860,#48861,#48862,#48863,#48864,#48865,#48866,#48867,#48868,#48869,#48870,
#48871,#48872,#48873,#48874,#48875,#48876,#48877,#48878,#48879,#48880,#48881,
#48882,#48883,#48884,#48885,#48886,#48887,#48888,#48889,#48890,#48891,#48892,
#48893,#48894,#48895,#48896,#48897,#48898,#48899,#48900,#48901,#48902,#48903,
#48904,#48905,#48906,#48907,#48908,#48909,#48910,#48911,#48912,#48913,#48914,
#48915,#48916,#48917,#48918,#48919,#48920),(#48921,#48922,#48923,#48924,
#48925,#48926,#48927,#48928,#48929,#48930,#48931,#48932,#48933,#48934,#48935,
#48936,#48937,#48938,#48939,#48940,#48941,#48942,#48943,#48944,#48945,#48946,
#48947,#48948,#48949,#48950,#48951,#48952,#48953,#48954,#48955,#48956,#48957,
#48958,#48959,#48960,#48961,#48962,#48963,#48964,#48965,#48966,#48967,#48968,
#48969,#48970,#48971,#48972,#48973,#48974,#48975,#48976,#48977,#48978,#48979,
#48980,#48981,#48982,#48983,#48984,#48985,#48986,#48987,#48988,#48989,#48990,
#48991,#48992,#48993,#48994,#48995,#48996,#48997,#48998,#48999,#49000,#49001,
#49002,#49003,#49004,#49005,#49006,#49007,#49008,#49009,#49010,#49011,#49012,
#49013,#49014,#49015,#49016,#49017,#49018,#49019,#49020,#49021,#49022,#49023,
#49024,#49025,#49026,#49027,#49028,#49029,#49030,#49031,#49032,#49033,#49034,
#49035,#49036,#49037,#49038,#49039,#49040,#49041,#49042,#49043,#49044,#49045,
#49046,#49047,#49048,#49049,#49050,#49051,#49052,#49053,#49054,#49055,#49056,
#49057,#49058,#49059,#49060,#49061,#49062,#49063,#49064,#49065,#49066,#49067,
#49068,#49069,#49070,#49071,#49072,#49073,#49074,#49075,#49076,#49077,#49078,
#49079,#49080,#49081,#49082,#49083,#49084,#49085,#49086,#49087,#49088,#49089,
#49090,#49091,#49092,#49093,#49094,#49095,#49096,#49097,#49098,#49099,#49100,
#49101,#49102,#49103,#49104,#49105,#49106,#49107,#49108,#49109,#49110,#49111,
#49112,#49113,#49114,#49115,#49116,#49117,#49118,#49119,#49120,#49121,#49122,
#49123,#49124,#49125,#49126,#49127,#49128,#49129,#49130,#49131,#49132,#49133,
#49134,#49135,#49136,#49137,#49138,#49139,#49140,#49141,#49142,#49143,#49144,
#49145,#49146,#49147,#49148,#49149,#49150,#49151,#49152,#49153,#49154,#49155,
#49156,#49157,#49158,#49159,#49160,#49161,#49162,#49163,#49164,#49165,#49166,
#49167,#49168,#49169,#49170,#49171,#49172,#49173,#49174,#49175,#49176,#49177,
#49178,#49179,#49180,#49181,#49182,#49183,#49184,#49185,#49186,#49187,#49188,
#49189,#49190,#49191,#49192,#49193,#49194,#49195,#49196,#49197,#49198,#49199,
#49200,#49201,#49202,#49203,#49204,#49205,#49206,#49207,#49208,#49209,#49210,
#49211,#49212,#49213,#49214,#49215,#49216,#49217,#49218,#49219,#49220,#49221,
#49222,#49223,#49224,#49225,#49226,#49227,#49228,#49229,#49230,#49231,#49232,
#49233,#49234,#49235,#49236,#49237,#49238,#49239,#49240,#49241,#49242,#49243,
#49244,#49245,#49246,#49247,#49248,#49249,#49250,#49251,#49252,#49253,#49254,
#49255,#49256,#49257,#49258,#49259,#49260,#49261,#49262,#49263,#49264,#49265,
#49266,#49267,#49268,#49269,#49270,#49271,#49272,#49273,#49274,#49275,#49276,
#49277,#49278,#49279,#49280,#49281,#49282,#49283,#49284,#49285,#49286,#49287,
#49288,#49289,#49290,#49291,#49292,#49293,#49294,#49295,#49296,#49297,#49298,
#49299,#49300,#49301,#49302,#49303,#49304,#49305,#49306,#49307,#49308,#49309,
#49310,#49311,#49312,#49313,#49314,#49315,#49316,#49317,#49318,#49319,#49320,
#49321,#49322,#49323,#49324,#49325,#49326,#49327,#49328,#49329,#49330,#49331,
#49332,#49333,#49334,#49335,#49336,#49337,#49338,#49339,#49340,#49341,#49342,
#49343,#49344,#49345,#49346,#49347,#49348,#49349,#49350,#49351,#49352,#49353,
#49354,#49355,#49356,#49357,#49358,#49359,#49360,#49361,#49362,#49363,#49364,
#49365,#49366,#49367,#49368,#49369,#49370,#49371,#49372,#49373,#49374,#49375,
#49376,#49377,#49378,#49379,#49380,#49381,#49382,#49383,#49384,#49385,#49386,
#49387,#49388,#49389,#49390,#49391,#49392,#49393,#49394,#49395,#49396,#49397,
#49398,#49399,#49400,#49401,#49402,#49403,#49404,#49405,#49406,#49407,#49408,
#49409,#49410,#49411,#49412,#49413,#49414,#49415,#49416,#49417,#49418,#49419,
#49420,#49421,#49422,#49423,#49424,#49425,#49426,#49427,#49428,#49429,#49430,
#49431,#49432,#49433,#49434,#49435,#49436,#49437,#49438,#49439,#49440,#49441,
#49442,#49443,#49444,#49445,#49446,#49447,#49448,#49449,#49450,#49451)),
 .UNSPECIFIED.,.F.,.F.,.F.,(4,4),(4,1,1,1,1,1,1,1,1,1,1,1,1,1,1,1,1,1,1,
1,1,1,1,1,1,1,1,1,1,1,1,1,1,1,1,1,1,1,1,1,1,1,1,1,1,1,1,1,1,1,1,1,1,1,1,
1,1,1,1,1,1,1,1,1,1,1,1,1,1,1,1,1,1,1,1,1,1,1,1,1,1,1,1,1,1,1,1,1,1,1,1,
1,1,1,1,1,1,1,1,1,1,1,1,1,1,1,1,1,1,1,1,1,1,1,1,1,1,1,1,1,1,1,1,1,1,1,1,
1,1,1,1,1,1,1,1,1,1,1,1,1,1,1,1,1,1,1,1,1,1,1,1,1,1,1,1,1,1,1,1,1,1,1,1,
1,1,1,1,1,1,1,1,1,1,1,1,1,1,1,1,1,1,1,1,1,1,1,1,1,1,1,1,1,1,1,1,1,1,1,1,
1,1,1,1,1,1,1,1,1,1,1,1,1,1,1,1,1,1,1,1,1,1,1,1,1,1,1,1,1,1,1,1,1,1,1,1,
1,1,1,1,1,1,1,1,1,1,1,1,1,1,1,1,1,1,1,1,1,1,1,1,1,1,1,1,1,1,1,1,1,1,1,1,
1,1,1,1,1,1,1,1,1,1,1,1,1,1,1,1,1,1,1,1,1,1,1,1,1,1,1,1,1,1,1,1,1,1,1,1,
1,1,1,1,1,1,1,1,1,1,1,1,1,1,1,1,1,1,1,1,1,1,1,1,1,1,1,1,1,1,1,1,1,1,1,1,
1,1,1,1,1,1,1,1,1,1,1,1,1,1,1,1,1,1,1,1,1,1,1,1,1,1,1,1,1,1,1,1,1,1,1,1,
1,1,1,1,1,1,1,1,1,1,1,1,1,1,1,1,1,1,1,1,1,1,1,1,1,1,1,1,1,1,1,1,1,1,1,1,
1,1,1,1,1,1,1,1,1,1,1,1,1,1,1,1,1,1,1,1,1,1,1,1,1,1,1,1,1,1,1,1,1,1,1,1,
1,1,1,1,1,1,1,1,1,1,1,1,1,1,1,1,1,1,1,1,1,1,1,1,1,1,1,1,1,1,1,1,1,1,1,1,
1,1,1,1,1,1,1,1,1,1,1,1,1,1,1,1,1,1,1,1,1,1,1,1,1,1,1,1,1,1,1,1,1,1,1,1,
1,1,1,1,1,4),(-1.81545167298606E-13,0.23619887080812),(8.98757472625061,
9.48752163453545,9.98746854282029,10.4874154511051,10.98736235939,11.4873092676748,
11.9872561759597,12.4872030842445,12.9871499925294,13.4870969008142,13.987043809099,
14.4869907173839,14.9869376256687,15.4868845339536,15.9868314422384,16.4867783505233,
16.9867252588081,17.4866721670929,17.9866190753778,18.4865659836626,18.9865128919475,
19.4864598002323,19.9864067085172,20.486353616802,20.9863005250869,21.4862474333717,
21.9861943416565,22.4861412499414,22.9860881582262,23.4860350665111,23.9859819747959,
24.4859288830808,24.9858757913656,25.4858226996504,25.9857696079353,26.4857165162201,
26.985663424505,27.4856103327898,27.9855572410747,28.4855041493595,28.9854510576443,
29.4853979659292,29.985344874214,30.4852917824989,30.9852386907837,31.4851855990686,
31.9851325073534,32.4850794156383,32.9850263239231,33.4849732322079,33.9849201404928,
34.4848670487776,34.9848139570625,35.4847608653473,35.9847077736322,36.484654681917,
36.9846015902018,37.4845484984867,37.9844954067715,38.4844423150564,38.9843892233412,
39.4843361316261,39.9842830399109,40.4842299481957,40.9841768564806,41.4841237647654,
41.9840706730503,42.4840175813351,42.98396448962,43.4839113979048,43.9838583061896,
44.4838052144745,44.9837521227593,45.4836990310442,45.983645939329,46.4835928476139,
46.9835397558987,47.4834866641836,47.9834335724684,48.4833804807532,48.9833273890381,
49.4832742973229,49.9832212056078,50.4831681138926,50.9831150221775,51.4830619304623,
51.9830088387471,52.482955747032,52.9829026553168,53.4828495636017,53.9827964718865,
54.4827433801714,54.9826902884562,55.4826371967411,55.9825841050259,56.4825310133107,
56.9824779215956,57.4824248298804,57.9823717381653,58.4823186464501,58.982265554735,
59.4822124630198,59.9821593713046,60.4821062795895,60.9820531878743,61.4820000961592,
61.981947004444,62.4818939127289,62.9818408210137,63.4817877292985,63.9817346375834,
64.4816815458682,64.9816284541531,65.4815753624379,65.9815222707228,66.4814691790076,
66.9814160872924,67.4813629955773,67.9813099038621,68.481256812147,68.9812037204318,
69.4811506287167,69.9810975370015,70.4810444452864,70.9809913535712,71.480938261856,
71.9808851701409,72.4808320784257,72.9807789867106,73.4807258949954,73.9806728032802,
74.4806197115651,74.98056661985,75.4805135281348,75.9804604364196,76.4804073447045,
76.9803542529893,77.4803011612742,77.980248069559,78.4801949778438,78.9801418861287,
79.4800887944135,79.9800357026984,80.4799826109832,80.9799295192681,81.4798764275529,
81.9798233358378,82.4797702441226,82.9797171524074,83.4796640606923,83.9796109689771,
84.479557877262,84.9795047855468,85.4794516938317,85.9793986021165,86.4793455104013,
86.9792924186862,87.479239326971,87.9791862352559,88.4791331435407,88.9790800518255,
89.4790269601104,89.9789738683953,90.4789207766801,90.9788676849649,91.4788145932498,
91.9787615015346,92.4787084098195,92.9786553181043,93.4786022263891,93.978549134674,
94.4784960429588,94.9784429512437,95.4783898595285,95.9783367678134,96.4782836760982,
96.9782305843831,97.4781774926679,97.9781244009527,98.4780713092376,98.9780182175224,
99.4779651258073,99.9779120340921,100.477858942377,100.977805850662,101.477752758947,
101.977699667231,102.477646575516,102.977593483801,103.477540392086,103.977487300371,
104.477434208656,104.977381116941,105.477328025225,105.97727493351,106.477221841795,
106.97716875008,107.477115658365,107.97706256665,108.477009474934,108.976956383219,
109.476903291504,109.976850199789,110.476797108074,110.976744016359,111.476690924644,
111.976637832928,112.476584741213,112.976531649498,113.476478557783,113.976425466068,
114.476372374353,114.976319282637,115.476266190922,115.976213099207,116.476160007492,
116.976106915777,117.476053824062,117.976000732346,118.475947640631,118.975894548916,
119.475841457201,119.975788365486,120.475735273771,120.975682182056,121.47562909034,
121.975575998625,122.47552290691,122.975469815195,123.47541672348,123.975363631765,
124.475310540049,124.975257448334,125.475204356619,125.975151264904,126.475098173189,
126.975045081474,127.474991989759,127.974938898043,128.474885806328,128.974832714613,
129.474779622898,129.974726531183,130.474673439468,130.974620347752,131.474567256037,
131.974514164322,132.474461072607,132.974407980892,133.474354889177,133.974301797461,
134.474248705746,134.974195614031,135.474142522316,135.974089430601,136.474036338886,
136.973983247171,137.473930155455,137.97387706374,138.473823972025,138.97377088031,
139.97366469688,140.973558513449,141.473505421734,141.973452330019,142.473399238304,
142.973346146589,143.473293054873,143.973239963158,144.473186871443,144.973133779728,
145.473080688013,145.973027596298,146.472974504583,146.972921412867,147.472868321152,
147.972815229437,148.472762137722,148.972709046007,149.472655954292,149.972602862576,
150.472549770861,150.972496679146,151.472443587431,151.972390495716,152.472337404001,
152.972284312286,153.47223122057,153.972178128855,154.47212503714,154.972071945425,
155.47201885371,155.971965761995,156.471912670279,156.971859578564,157.471806486849,
157.971753395134,158.471700303419,158.971647211704,159.471594119988,159.971541028273,
160.471487936558,160.971434844843,161.471381753128,161.971328661413,162.471275569698,
162.971222477982,163.471169386267,163.971116294552,164.471063202837,164.971010111122,
165.470957019407,165.970903927691,166.470850835976,166.970797744261,167.470744652546,
167.970691560831,168.470638469116,168.970585377401,169.470532285685,169.97047919397,
170.470426102255,170.97037301054,171.470319918825,171.97026682711,172.470213735394,
172.970160643679,173.470107551964,173.970054460249,174.470001368534,174.969948276819,
175.469895185103,175.969842093388,176.469789001673,176.969735909958,177.469682818243,
177.969629726528,178.469576634813,178.969523543097,179.469470451382,179.969417359667,
180.469364267952,180.969311176237,181.469258084522,181.969204992806,182.469151901091,
182.969098809376,183.469045717661,183.968992625946,184.468939534231,184.968886442515,
185.4688333508,185.968780259085,186.46872716737,186.968674075655,187.46862098394,
187.968567892225,188.468514800509,188.968461708794,189.468408617079,189.968355525364,
190.468302433649,190.968249341934,191.468196250218,191.968143158503,192.468090066788,
192.968036975073,193.467983883358,193.967930791643,194.467877699928,194.967824608212,
195.467771516497,195.967718424782,196.467665333067,196.967612241352,197.467559149637,
197.967506057921,198.467452966206,198.967399874491,199.467346782776,199.967293691061,
200.467240599346,200.967187507631,201.467134415915,201.9670813242,202.467028232485,
202.96697514077,203.466922049055,203.96686895734,204.466815865624,204.966762773909,
205.466709682194,205.966656590479,206.466603498764,206.966550407049,207.466497315333,
207.966444223618,208.466391131903,208.966338040188,209.466284948473,209.966231856758,
210.466178765043,210.966125673327,211.466072581612,211.966019489897,212.465966398182,
212.965913306467,213.465860214752,213.965807123036,214.465754031321,214.965700939606,
215.465647847891,215.965594756176,216.465541664461,216.965488572745,217.46543548103,
217.965382389315,218.4653292976,218.965276205885,219.46522311417,219.965170022455,
220.465116930739,220.965063839024,221.465010747309,221.964957655594,222.464904563879,
222.964851472164,223.464798380448,223.964745288733,224.464692197018,224.964639105303,
225.464586013588,225.964532921873,226.464479830158,226.964426738442,227.464373646727,
227.964320555012,228.464267463297,228.964214371582,229.464161279867,229.964108188151,
230.464055096436,230.964002004721,231.463948913006,231.963895821291,232.463842729576,
232.96378963786,233.463736546145,233.96368345443,234.463630362715,234.963577271,
235.463524179285,235.96347108757,236.463417995854,236.963364904139,237.463311812424,
237.963258720709,238.463205628994,238.963152537279,239.463099445563,239.963046353848,
240.462993262133,240.962940170418,241.462887078703,241.962833986988,242.462780895273,
242.962727803557,243.462674711842,243.962621620127,244.462568528412,244.962515436697,
245.462462344982,245.962409253266,246.462356161551,246.962303069836,247.462249978121,
247.962196886406,248.462143794691,248.962090702975,249.46203761126,249.961984519545,
250.46193142783,250.961878336115,251.4618252444,251.961772152685,252.461719060969,
252.961665969254,253.461612877539,253.961559785824,254.461506694109,254.961453602394,
255.461400510678,255.961347418963,256.461294327248,256.961241235533,257.461188143818,
257.961135052103,258.461081960387,258.961028868672,259.460975776957,259.960922685242,
260.460869593527,260.960816501812,261.460763410097,261.960710318381,262.460657226666,
262.960604134951,263.460551043236,263.960497951521,264.460444859806,264.96039176809,
265.460338676375,265.96028558466,266.460232492945,266.96017940123,267.460126309515,
267.9600732178,268.460020126084,268.959967034369,269.459913942654,269.959860850939,
270.459807759224,270.959754667509,271.459701575793,271.959648484078,272.459595392363,
272.959542300648,273.459489208933,273.959436117218),.UNSPECIFIED.);
#160=B_SPLINE_SURFACE_WITH_KNOTS('',3,3,((#51582,#51583,#51584,#51585,#51586,
#51587,#51588,#51589,#51590,#51591,#51592,#51593,#51594,#51595,#51596,#51597,
#51598,#51599,#51600,#51601,#51602,#51603,#51604,#51605,#51606,#51607,#51608,
#51609,#51610,#51611,#51612,#51613,#51614,#51615,#51616,#51617,#51618,#51619,
#51620,#51621,#51622,#51623,#51624,#51625,#51626,#51627,#51628,#51629,#51630,
#51631,#51632,#51633,#51634,#51635,#51636,#51637,#51638,#51639,#51640,#51641,
#51642,#51643,#51644,#51645,#51646,#51647,#51648,#51649,#51650,#51651,#51652,
#51653,#51654,#51655,#51656,#51657,#51658,#51659,#51660,#51661,#51662,#51663,
#51664,#51665,#51666,#51667,#51668,#51669,#51670,#51671,#51672,#51673,#51674,
#51675,#51676,#51677,#51678,#51679,#51680,#51681,#51682,#51683,#51684),
(#51685,#51686,#51687,#51688,#51689,#51690,#51691,#51692,#51693,#51694,
#51695,#51696,#51697,#51698,#51699,#51700,#51701,#51702,#51703,#51704,#51705,
#51706,#51707,#51708,#51709,#51710,#51711,#51712,#51713,#51714,#51715,#51716,
#51717,#51718,#51719,#51720,#51721,#51722,#51723,#51724,#51725,#51726,#51727,
#51728,#51729,#51730,#51731,#51732,#51733,#51734,#51735,#51736,#51737,#51738,
#51739,#51740,#51741,#51742,#51743,#51744,#51745,#51746,#51747,#51748,#51749,
#51750,#51751,#51752,#51753,#51754,#51755,#51756,#51757,#51758,#51759,#51760,
#51761,#51762,#51763,#51764,#51765,#51766,#51767,#51768,#51769,#51770,#51771,
#51772,#51773,#51774,#51775,#51776,#51777,#51778,#51779,#51780,#51781,#51782,
#51783,#51784,#51785,#51786,#51787),(#51788,#51789,#51790,#51791,#51792,
#51793,#51794,#51795,#51796,#51797,#51798,#51799,#51800,#51801,#51802,#51803,
#51804,#51805,#51806,#51807,#51808,#51809,#51810,#51811,#51812,#51813,#51814,
#51815,#51816,#51817,#51818,#51819,#51820,#51821,#51822,#51823,#51824,#51825,
#51826,#51827,#51828,#51829,#51830,#51831,#51832,#51833,#51834,#51835,#51836,
#51837,#51838,#51839,#51840,#51841,#51842,#51843,#51844,#51845,#51846,#51847,
#51848,#51849,#51850,#51851,#51852,#51853,#51854,#51855,#51856,#51857,#51858,
#51859,#51860,#51861,#51862,#51863,#51864,#51865,#51866,#51867,#51868,#51869,
#51870,#51871,#51872,#51873,#51874,#51875,#51876,#51877,#51878,#51879,#51880,
#51881,#51882,#51883,#51884,#51885,#51886,#51887,#51888,#51889,#51890),
(#51891,#51892,#51893,#51894,#51895,#51896,#51897,#51898,#51899,#51900,
#51901,#51902,#51903,#51904,#51905,#51906,#51907,#51908,#51909,#51910,#51911,
#51912,#51913,#51914,#51915,#51916,#51917,#51918,#51919,#51920,#51921,#51922,
#51923,#51924,#51925,#51926,#51927,#51928,#51929,#51930,#51931,#51932,#51933,
#51934,#51935,#51936,#51937,#51938,#51939,#51940,#51941,#51942,#51943,#51944,
#51945,#51946,#51947,#51948,#51949,#51950,#51951,#51952,#51953,#51954,#51955,
#51956,#51957,#51958,#51959,#51960,#51961,#51962,#51963,#51964,#51965,#51966,
#51967,#51968,#51969,#51970,#51971,#51972,#51973,#51974,#51975,#51976,#51977,
#51978,#51979,#51980,#51981,#51982,#51983,#51984,#51985,#51986,#51987,#51988,
#51989,#51990,#51991,#51992,#51993)),.UNSPECIFIED.,.F.,.F.,.F.,(4,4),(4,
1,1,1,1,1,1,1,1,1,1,1,1,1,1,1,1,1,1,1,1,1,1,1,1,1,1,1,1,1,1,1,1,1,1,1,1,
1,1,1,1,1,1,1,1,1,1,1,1,1,1,1,1,1,1,1,1,1,1,1,1,1,1,1,1,1,1,1,1,1,1,1,1,
1,1,1,1,1,1,1,1,1,1,1,1,1,1,1,1,1,1,1,1,1,1,1,1,1,1,1,4),(0.,0.0820126057383863),
(8.31473274985795,9.30632309046341,10.2979134310689,11.2895037716743,12.2810941122798,
13.2726844528853,14.2642747934907,15.2558651340962,16.2474554747016,17.2390458153071,
18.2306361559126,19.222226496518,20.2138168371235,21.205407177729,22.1969975183344,
23.1885878589399,24.1801781995453,25.1717685401508,26.1633588807563,27.1549492213617,
28.1465395619672,29.1381299025727,30.1297202431781,31.1213105837836,32.112900924389,
33.1044912649945,34.0960816056,35.0876719462054,36.0792622868109,37.0708526274164,
38.0624429680218,39.0540333086273,40.0456236492327,41.0372139898382,42.0288043304437,
43.0203946710491,44.0119850116546,45.0035753522601,45.9951656928655,46.986756033471,
47.9783463740764,48.9699367146819,49.9615270552874,50.9531173958928,51.9447077364983,
52.9362980771037,53.9278884177092,54.9194787583147,55.9110690989201,56.9026594395256,
57.8942497801311,58.8858401207365,59.877430461342,60.8690208019474,61.8606111425529,
62.8522014831584,63.8437918237638,64.8353821643693,65.8269725049748,66.8185628455802,
67.8101531861857,68.8017435267912,69.7933338673966,70.7849242080021,71.7765145486075,
72.768104889213,73.7596952298185,74.7512855704239,75.7428759110294,76.7344662516349,
77.7260565922403,78.7176469328458,79.7092372734512,80.7008276140567,81.6924179546622,
82.6840082952676,83.6755986358731,84.6671889764786,85.658779317084,86.6503696576895,
87.6419599982949,88.6335503389004,89.6251406795059,90.6167310201113,91.6083213607168,
92.5999117013223,93.5915020419277,94.5830923825332,95.5746827231386,96.5662730637441,
97.5578634043496,98.549453744955,99.5410440855605,100.532634426166,101.524224766771,
102.515815107377,103.507405447982,104.498995788588,105.490586129193,106.482176469799,
107.473766810404),.UNSPECIFIED.);
#161=B_SPLINE_SURFACE_WITH_KNOTS('',3,3,((#52148,#52149,#52150,#52151,#52152,
#52153,#52154,#52155,#52156,#52157,#52158,#52159,#52160,#52161,#52162,#52163,
#52164,#52165,#52166,#52167,#52168,#52169,#52170,#52171,#52172,#52173,#52174,
#52175,#52176,#52177,#52178,#52179,#52180,#52181,#52182,#52183,#52184,#52185,
#52186,#52187,#52188,#52189,#52190,#52191,#52192,#52193,#52194,#52195,#52196,
#52197,#52198,#52199,#52200,#52201,#52202,#52203,#52204,#52205,#52206,#52207,
#52208,#52209,#52210,#52211,#52212,#52213,#52214,#52215,#52216,#52217,#52218,
#52219,#52220,#52221,#52222,#52223,#52224,#52225,#52226,#52227,#52228,#52229,
#52230,#52231,#52232,#52233,#52234,#52235,#52236,#52237,#52238,#52239,#52240,
#52241,#52242,#52243,#52244,#52245,#52246,#52247,#52248,#52249,#52250),
(#52251,#52252,#52253,#52254,#52255,#52256,#52257,#52258,#52259,#52260,
#52261,#52262,#52263,#52264,#52265,#52266,#52267,#52268,#52269,#52270,#52271,
#52272,#52273,#52274,#52275,#52276,#52277,#52278,#52279,#52280,#52281,#52282,
#52283,#52284,#52285,#52286,#52287,#52288,#52289,#52290,#52291,#52292,#52293,
#52294,#52295,#52296,#52297,#52298,#52299,#52300,#52301,#52302,#52303,#52304,
#52305,#52306,#52307,#52308,#52309,#52310,#52311,#52312,#52313,#52314,#52315,
#52316,#52317,#52318,#52319,#52320,#52321,#52322,#52323,#52324,#52325,#52326,
#52327,#52328,#52329,#52330,#52331,#52332,#52333,#52334,#52335,#52336,#52337,
#52338,#52339,#52340,#52341,#52342,#52343,#52344,#52345,#52346,#52347,#52348,
#52349,#52350,#52351,#52352,#52353),(#52354,#52355,#52356,#52357,#52358,
#52359,#52360,#52361,#52362,#52363,#52364,#52365,#52366,#52367,#52368,#52369,
#52370,#52371,#52372,#52373,#52374,#52375,#52376,#52377,#52378,#52379,#52380,
#52381,#52382,#52383,#52384,#52385,#52386,#52387,#52388,#52389,#52390,#52391,
#52392,#52393,#52394,#52395,#52396,#52397,#52398,#52399,#52400,#52401,#52402,
#52403,#52404,#52405,#52406,#52407,#52408,#52409,#52410,#52411,#52412,#52413,
#52414,#52415,#52416,#52417,#52418,#52419,#52420,#52421,#52422,#52423,#52424,
#52425,#52426,#52427,#52428,#52429,#52430,#52431,#52432,#52433,#52434,#52435,
#52436,#52437,#52438,#52439,#52440,#52441,#52442,#52443,#52444,#52445,#52446,
#52447,#52448,#52449,#52450,#52451,#52452,#52453,#52454,#52455,#52456),
(#52457,#52458,#52459,#52460,#52461,#52462,#52463,#52464,#52465,#52466,
#52467,#52468,#52469,#52470,#52471,#52472,#52473,#52474,#52475,#52476,#52477,
#52478,#52479,#52480,#52481,#52482,#52483,#52484,#52485,#52486,#52487,#52488,
#52489,#52490,#52491,#52492,#52493,#52494,#52495,#52496,#52497,#52498,#52499,
#52500,#52501,#52502,#52503,#52504,#52505,#52506,#52507,#52508,#52509,#52510,
#52511,#52512,#52513,#52514,#52515,#52516,#52517,#52518,#52519,#52520,#52521,
#52522,#52523,#52524,#52525,#52526,#52527,#52528,#52529,#52530,#52531,#52532,
#52533,#52534,#52535,#52536,#52537,#52538,#52539,#52540,#52541,#52542,#52543,
#52544,#52545,#52546,#52547,#52548,#52549,#52550,#52551,#52552,#52553,#52554,
#52555,#52556,#52557,#52558,#52559)),.UNSPECIFIED.,.F.,.F.,.F.,(4,4),(4,
1,1,1,1,1,1,1,1,1,1,1,1,1,1,1,1,1,1,1,1,1,1,1,1,1,1,1,1,1,1,1,1,1,1,1,1,
1,1,1,1,1,1,1,1,1,1,1,1,1,1,1,1,1,1,1,1,1,1,1,1,1,1,1,1,1,1,1,1,1,1,1,1,
1,1,1,1,1,1,1,1,1,1,1,1,1,1,1,1,1,1,1,1,1,1,1,1,1,1,1,4),(0.,0.0820126057383863),
(11.6152142277546,12.6068045683601,13.5983949089656,14.589985249571,15.5815755901765,
16.573165930782,17.5647562713874,18.5563466119929,19.5479369525983,20.5395272932038,
21.5311176338093,22.5227079744147,23.5142983150202,24.5058886556257,25.4974789962311,
26.4890693368366,27.480659677442,28.4722500180475,29.463840358653,30.4554306992584,
31.4470210398639,32.4386113804694,33.4302017210748,34.4217920616803,35.4133824022857,
36.4049727428912,37.3965630834967,38.3881534241021,39.3797437647076,40.3713341053131,
41.3629244459185,42.354514786524,43.3461051271294,44.3376954677349,45.3292858083404,
46.3208761489458,47.3124664895513,48.3040568301568,49.2956471707622,50.2872375113677,
51.2788278519731,52.2704181925786,53.2620085331841,54.2535988737895,55.245189214395,
56.2367795550005,57.2283698956059,58.2199602362114,59.2115505768168,60.2031409174223,
61.1947312580278,62.1863215986332,63.1779119392387,64.1695022798442,65.1610926204496,
66.1526829610551,67.1442733016605,68.135863642266,69.1274539828715,70.1190443234769,
71.1106346640824,72.1022250046879,73.0938153452933,74.0854056858988,75.0769960265042,
76.0685863671097,77.0601767077152,78.0517670483206,79.0433573889261,80.0349477295316,
81.026538070137,82.0181284107425,83.0097187513479,84.0013090919534,84.9928994325589,
85.9844897731643,86.9760801137698,87.9676704543753,88.9592607949807,89.9508511355862,
90.9424414761916,91.9340318167971,92.9256221574026,93.917212498008,94.9088028386135,
95.900393179219,96.8919835198244,97.8835738604299,98.8751642010353,99.8667545416408,
100.858344882246,101.849935222852,102.841525563457,103.833115904063,104.824706244668,
105.816296585274,106.807886925879,107.799477266485,108.79106760709,109.782657947695,
110.774248288301),.UNSPECIFIED.);
#162=B_SPLINE_SURFACE_WITH_KNOTS('',3,3,((#54617,#54618,#54619,#54620,#54621,
#54622,#54623,#54624,#54625,#54626,#54627,#54628,#54629,#54630,#54631,#54632,
#54633,#54634,#54635,#54636,#54637,#54638,#54639,#54640,#54641,#54642,#54643,
#54644,#54645,#54646,#54647,#54648,#54649,#54650,#54651,#54652,#54653,#54654,
#54655,#54656,#54657,#54658,#54659,#54660,#54661,#54662,#54663,#54664,#54665,
#54666,#54667,#54668,#54669,#54670,#54671,#54672,#54673,#54674,#54675,#54676,
#54677,#54678,#54679,#54680,#54681,#54682,#54683,#54684,#54685,#54686,#54687,
#54688,#54689,#54690,#54691,#54692,#54693,#54694,#54695,#54696,#54697,#54698,
#54699,#54700,#54701,#54702,#54703,#54704,#54705,#54706,#54707,#54708,#54709,
#54710,#54711,#54712,#54713,#54714,#54715,#54716,#54717,#54718,#54719,#54720,
#54721,#54722,#54723,#54724,#54725,#54726,#54727,#54728,#54729,#54730,#54731,
#54732,#54733,#54734,#54735,#54736,#54737,#54738,#54739,#54740,#54741,#54742,
#54743),(#54744,#54745,#54746,#54747,#54748,#54749,#54750,#54751,#54752,
#54753,#54754,#54755,#54756,#54757,#54758,#54759,#54760,#54761,#54762,#54763,
#54764,#54765,#54766,#54767,#54768,#54769,#54770,#54771,#54772,#54773,#54774,
#54775,#54776,#54777,#54778,#54779,#54780,#54781,#54782,#54783,#54784,#54785,
#54786,#54787,#54788,#54789,#54790,#54791,#54792,#54793,#54794,#54795,#54796,
#54797,#54798,#54799,#54800,#54801,#54802,#54803,#54804,#54805,#54806,#54807,
#54808,#54809,#54810,#54811,#54812,#54813,#54814,#54815,#54816,#54817,#54818,
#54819,#54820,#54821,#54822,#54823,#54824,#54825,#54826,#54827,#54828,#54829,
#54830,#54831,#54832,#54833,#54834,#54835,#54836,#54837,#54838,#54839,#54840,
#54841,#54842,#54843,#54844,#54845,#54846,#54847,#54848,#54849,#54850,#54851,
#54852,#54853,#54854,#54855,#54856,#54857,#54858,#54859,#54860,#54861,#54862,
#54863,#54864,#54865,#54866,#54867,#54868,#54869,#54870),(#54871,#54872,
#54873,#54874,#54875,#54876,#54877,#54878,#54879,#54880,#54881,#54882,#54883,
#54884,#54885,#54886,#54887,#54888,#54889,#54890,#54891,#54892,#54893,#54894,
#54895,#54896,#54897,#54898,#54899,#54900,#54901,#54902,#54903,#54904,#54905,
#54906,#54907,#54908,#54909,#54910,#54911,#54912,#54913,#54914,#54915,#54916,
#54917,#54918,#54919,#54920,#54921,#54922,#54923,#54924,#54925,#54926,#54927,
#54928,#54929,#54930,#54931,#54932,#54933,#54934,#54935,#54936,#54937,#54938,
#54939,#54940,#54941,#54942,#54943,#54944,#54945,#54946,#54947,#54948,#54949,
#54950,#54951,#54952,#54953,#54954,#54955,#54956,#54957,#54958,#54959,#54960,
#54961,#54962,#54963,#54964,#54965,#54966,#54967,#54968,#54969,#54970,#54971,
#54972,#54973,#54974,#54975,#54976,#54977,#54978,#54979,#54980,#54981,#54982,
#54983,#54984,#54985,#54986,#54987,#54988,#54989,#54990,#54991,#54992,#54993,
#54994,#54995,#54996,#54997),(#54998,#54999,#55000,#55001,#55002,#55003,
#55004,#55005,#55006,#55007,#55008,#55009,#55010,#55011,#55012,#55013,#55014,
#55015,#55016,#55017,#55018,#55019,#55020,#55021,#55022,#55023,#55024,#55025,
#55026,#55027,#55028,#55029,#55030,#55031,#55032,#55033,#55034,#55035,#55036,
#55037,#55038,#55039,#55040,#55041,#55042,#55043,#55044,#55045,#55046,#55047,
#55048,#55049,#55050,#55051,#55052,#55053,#55054,#55055,#55056,#55057,#55058,
#55059,#55060,#55061,#55062,#55063,#55064,#55065,#55066,#55067,#55068,#55069,
#55070,#55071,#55072,#55073,#55074,#55075,#55076,#55077,#55078,#55079,#55080,
#55081,#55082,#55083,#55084,#55085,#55086,#55087,#55088,#55089,#55090,#55091,
#55092,#55093,#55094,#55095,#55096,#55097,#55098,#55099,#55100,#55101,#55102,
#55103,#55104,#55105,#55106,#55107,#55108,#55109,#55110,#55111,#55112,#55113,
#55114,#55115,#55116,#55117,#55118,#55119,#55120,#55121,#55122,#55123,#55124)),
 .UNSPECIFIED.,.F.,.F.,.F.,(4,4),(4,1,1,1,1,1,1,1,1,1,1,1,1,1,1,1,1,1,1,
1,1,1,1,1,1,1,1,1,1,1,1,1,1,1,1,1,1,1,1,1,1,1,1,1,1,1,1,1,1,1,1,1,1,1,1,
1,1,1,1,1,1,1,1,1,1,1,1,1,1,1,1,1,1,1,1,1,1,1,1,1,1,1,1,1,1,1,1,1,1,1,1,
1,1,1,1,1,1,1,1,1,1,1,1,1,1,1,1,1,1,1,1,1,1,1,1,1,1,1,1,1,1,1,1,1,4),(0.,
0.115296848757171),(8.30592286723169,8.80277904269557,9.29963521815945,
9.79649139362333,10.2933475690872,10.7902037445511,11.287059920015,11.7839160954788,
12.2807722709427,12.7776284464066,13.2744846218705,13.7713407973344,14.2681969727983,
14.7650531482621,15.261909323726,15.7587654991899,16.2556216746538,16.7524778501176,
17.2493340255815,17.7461902010454,18.2430463765093,18.7399025519732,19.236758727437,
19.7336149029009,20.2304710783648,20.7273272538287,21.2241834292926,21.7210396047565,
22.2178957802203,22.7147519556842,23.2116081311481,23.708464306612,24.2053204820759,
24.7021766575397,25.1990328330036,25.6958890084675,26.1927451839314,26.6896013593953,
27.1864575348591,27.683313710323,28.1801698857869,28.6770260612508,29.1738822367147,
29.6707384121785,30.1675945876424,30.6644507631063,31.1613069385702,31.6581631140341,
32.1550192894979,32.6518754649618,33.1487316404257,33.6455878158896,34.1424439913535,
34.6393001668173,35.1361563422812,35.6330125177451,36.129868693209,36.6267248686729,
37.1235810441367,37.6204372196006,38.1172933950645,38.6141495705284,39.1110057459923,
39.6078619214561,40.10471809692,40.6015742723839,41.0984304478478,41.5952866233117,
42.0921427987755,42.5889989742394,43.0858551497033,43.5827113251672,44.0795675006311,
44.5764236760949,45.0732798515588,45.5701360270227,46.0669922024866,46.5638483779504,
47.0607045534143,47.5575607288782,48.0544169043421,48.551273079806,49.0481292552699,
49.5449854307337,50.0418416061976,50.5386977816615,51.0355539571254,51.5324101325893,
52.0292663080531,52.526122483517,53.0229786589809,53.5198348344448,54.0166910099087,
54.5135471853725,55.0104033608364,55.5072595363003,56.0041157117642,56.5009718872281,
56.9978280626919,57.4946842381558,57.9915404136197,58.4883965890836,58.9852527645475,
59.4821089400113,59.9789651154752,60.4758212909391,60.972677466403,61.4695336418669,
61.9663898173307,62.4632459927946,62.9601021682585,63.4569583437224,63.9538145191863,
64.4506706946501,64.947526870114,65.4443830455779,65.9412392210418,66.4380953965057,
66.9349515719695,67.4318077474334,67.9286639228973,68.4255200983612,68.9223762738251,
69.4192324492889,69.9160886247528),.UNSPECIFIED.);
#163=B_SPLINE_SURFACE_WITH_KNOTS('',3,3,((#55386,#55387,#55388,#55389,#55390,
#55391,#55392,#55393,#55394,#55395,#55396,#55397,#55398,#55399,#55400,#55401,
#55402,#55403,#55404,#55405,#55406,#55407,#55408,#55409,#55410,#55411,#55412,
#55413,#55414,#55415,#55416,#55417,#55418,#55419,#55420,#55421,#55422,#55423,
#55424,#55425,#55426,#55427,#55428,#55429,#55430,#55431,#55432,#55433,#55434,
#55435,#55436,#55437,#55438,#55439,#55440,#55441,#55442,#55443,#55444,#55445,
#55446,#55447,#55448,#55449,#55450,#55451,#55452,#55453,#55454,#55455,#55456,
#55457,#55458,#55459,#55460,#55461,#55462,#55463,#55464,#55465,#55466,#55467,
#55468,#55469,#55470,#55471,#55472,#55473,#55474,#55475,#55476,#55477,#55478,
#55479,#55480,#55481,#55482,#55483,#55484,#55485,#55486,#55487,#55488,#55489,
#55490,#55491,#55492,#55493,#55494,#55495,#55496,#55497,#55498,#55499,#55500,
#55501,#55502,#55503,#55504,#55505,#55506,#55507,#55508,#55509,#55510,#55511,
#55512),(#55513,#55514,#55515,#55516,#55517,#55518,#55519,#55520,#55521,
#55522,#55523,#55524,#55525,#55526,#55527,#55528,#55529,#55530,#55531,#55532,
#55533,#55534,#55535,#55536,#55537,#55538,#55539,#55540,#55541,#55542,#55543,
#55544,#55545,#55546,#55547,#55548,#55549,#55550,#55551,#55552,#55553,#55554,
#55555,#55556,#55557,#55558,#55559,#55560,#55561,#55562,#55563,#55564,#55565,
#55566,#55567,#55568,#55569,#55570,#55571,#55572,#55573,#55574,#55575,#55576,
#55577,#55578,#55579,#55580,#55581,#55582,#55583,#55584,#55585,#55586,#55587,
#55588,#55589,#55590,#55591,#55592,#55593,#55594,#55595,#55596,#55597,#55598,
#55599,#55600,#55601,#55602,#55603,#55604,#55605,#55606,#55607,#55608,#55609,
#55610,#55611,#55612,#55613,#55614,#55615,#55616,#55617,#55618,#55619,#55620,
#55621,#55622,#55623,#55624,#55625,#55626,#55627,#55628,#55629,#55630,#55631,
#55632,#55633,#55634,#55635,#55636,#55637,#55638,#55639),(#55640,#55641,
#55642,#55643,#55644,#55645,#55646,#55647,#55648,#55649,#55650,#55651,#55652,
#55653,#55654,#55655,#55656,#55657,#55658,#55659,#55660,#55661,#55662,#55663,
#55664,#55665,#55666,#55667,#55668,#55669,#55670,#55671,#55672,#55673,#55674,
#55675,#55676,#55677,#55678,#55679,#55680,#55681,#55682,#55683,#55684,#55685,
#55686,#55687,#55688,#55689,#55690,#55691,#55692,#55693,#55694,#55695,#55696,
#55697,#55698,#55699,#55700,#55701,#55702,#55703,#55704,#55705,#55706,#55707,
#55708,#55709,#55710,#55711,#55712,#55713,#55714,#55715,#55716,#55717,#55718,
#55719,#55720,#55721,#55722,#55723,#55724,#55725,#55726,#55727,#55728,#55729,
#55730,#55731,#55732,#55733,#55734,#55735,#55736,#55737,#55738,#55739,#55740,
#55741,#55742,#55743,#55744,#55745,#55746,#55747,#55748,#55749,#55750,#55751,
#55752,#55753,#55754,#55755,#55756,#55757,#55758,#55759,#55760,#55761,#55762,
#55763,#55764,#55765,#55766),(#55767,#55768,#55769,#55770,#55771,#55772,
#55773,#55774,#55775,#55776,#55777,#55778,#55779,#55780,#55781,#55782,#55783,
#55784,#55785,#55786,#55787,#55788,#55789,#55790,#55791,#55792,#55793,#55794,
#55795,#55796,#55797,#55798,#55799,#55800,#55801,#55802,#55803,#55804,#55805,
#55806,#55807,#55808,#55809,#55810,#55811,#55812,#55813,#55814,#55815,#55816,
#55817,#55818,#55819,#55820,#55821,#55822,#55823,#55824,#55825,#55826,#55827,
#55828,#55829,#55830,#55831,#55832,#55833,#55834,#55835,#55836,#55837,#55838,
#55839,#55840,#55841,#55842,#55843,#55844,#55845,#55846,#55847,#55848,#55849,
#55850,#55851,#55852,#55853,#55854,#55855,#55856,#55857,#55858,#55859,#55860,
#55861,#55862,#55863,#55864,#55865,#55866,#55867,#55868,#55869,#55870,#55871,
#55872,#55873,#55874,#55875,#55876,#55877,#55878,#55879,#55880,#55881,#55882,
#55883,#55884,#55885,#55886,#55887,#55888,#55889,#55890,#55891,#55892,#55893)),
 .UNSPECIFIED.,.F.,.F.,.F.,(4,4),(4,1,1,1,1,1,1,1,1,1,1,1,1,1,1,1,1,1,1,
1,1,1,1,1,1,1,1,1,1,1,1,1,1,1,1,1,1,1,1,1,1,1,1,1,1,1,1,1,1,1,1,1,1,1,1,
1,1,1,1,1,1,1,1,1,1,1,1,1,1,1,1,1,1,1,1,1,1,1,1,1,1,1,1,1,1,1,1,1,1,1,1,
1,1,1,1,1,1,1,1,1,1,1,1,1,1,1,1,1,1,1,1,1,1,1,1,1,1,1,1,1,1,1,1,1,4),(0.,
0.115296848757171),(11.6154215191106,12.1122776945745,12.6091338700384,
13.1059900455022,13.6028462209661,14.09970239643,14.5965585718939,15.0934147473578,
15.5902709228216,16.0871270982855,16.5839832737494,17.0808394492133,17.5776956246772,
18.074551800141,18.5714079756049,19.0682641510688,19.5651203265327,20.0619765019966,
20.5588326774604,21.0556888529243,21.5525450283882,22.0494012038521,22.546257379316,
23.0431135547798,23.5399697302437,24.0368259057076,24.5336820811715,25.0305382566354,
25.5273944320992,26.0242506075631,26.521106783027,27.0179629584909,27.5148191339548,
28.0116753094186,28.5085314848825,29.0053876603464,29.5022438358103,29.9991000112742,
30.495956186738,30.9928123622019,31.4896685376658,31.9865247131297,32.4833808885936,
32.9802370640574,33.4770932395213,33.9739494149852,34.4708055904491,34.967661765913,
35.4645179413769,35.9613741168407,36.4582302923046,36.9550864677685,37.4519426432324,
37.9487988186963,38.4456549941601,38.942511169624,39.4393673450879,39.9362235205518,
40.4330796960157,40.9299358714795,41.4267920469434,41.9236482224073,42.4205043978712,
42.9173605733351,43.4142167487989,43.9110729242628,44.4079290997267,44.9047852751906,
45.4016414506545,45.8984976261183,46.3953538015822,46.8922099770461,47.38906615251,
47.8859223279739,48.3827785034377,48.8796346789016,49.3764908543655,49.8733470298294,
50.3702032052933,50.8670593807571,51.363915556221,51.8607717316849,52.3576279071488,
52.8544840826127,53.3513402580765,53.8481964335404,54.3450526090043,54.8419087844682,
55.3387649599321,55.8356211353959,56.3324773108598,56.8293334863237,57.3261896617876,
57.8230458372515,58.3199020127153,58.8167581881792,59.3136143636431,59.810470539107,
60.3073267145709,60.8041828900348,61.3010390654986,61.7978952409625,62.2947514164264,
62.7916075918903,63.2884637673542,63.785319942818,64.2821761182819,64.7790322937458,
65.2758884692097,65.7727446446736,66.2696008201374,66.7664569956013,67.2633131710652,
67.7601693465291,68.257025521993,68.7538816974568,69.2507378729207,69.7475940483846,
70.2444502238485,70.7413063993124,71.2381625747762,71.7350187502401,72.231874925704,
72.7287311011679,73.2255872766318),.UNSPECIFIED.);
#164=B_SPLINE_SURFACE_WITH_KNOTS('',3,3,((#57090,#57091,#57092,#57093,#57094,
#57095,#57096,#57097,#57098,#57099,#57100,#57101,#57102,#57103,#57104,#57105,
#57106,#57107,#57108,#57109,#57110,#57111,#57112,#57113,#57114,#57115,#57116,
#57117,#57118,#57119,#57120,#57121,#57122,#57123,#57124,#57125,#57126,#57127,
#57128,#57129,#57130,#57131,#57132,#57133,#57134,#57135,#57136,#57137,#57138,
#57139,#57140,#57141,#57142,#57143,#57144,#57145,#57146,#57147,#57148,#57149,
#57150,#57151,#57152,#57153,#57154,#57155,#57156,#57157,#57158,#57159,#57160,
#57161,#57162,#57163,#57164,#57165,#57166,#57167,#57168,#57169,#57170,#57171,
#57172,#57173,#57174,#57175,#57176,#57177,#57178,#57179,#57180,#57181,#57182),
(#57183,#57184,#57185,#57186,#57187,#57188,#57189,#57190,#57191,#57192,
#57193,#57194,#57195,#57196,#57197,#57198,#57199,#57200,#57201,#57202,#57203,
#57204,#57205,#57206,#57207,#57208,#57209,#57210,#57211,#57212,#57213,#57214,
#57215,#57216,#57217,#57218,#57219,#57220,#57221,#57222,#57223,#57224,#57225,
#57226,#57227,#57228,#57229,#57230,#57231,#57232,#57233,#57234,#57235,#57236,
#57237,#57238,#57239,#57240,#57241,#57242,#57243,#57244,#57245,#57246,#57247,
#57248,#57249,#57250,#57251,#57252,#57253,#57254,#57255,#57256,#57257,#57258,
#57259,#57260,#57261,#57262,#57263,#57264,#57265,#57266,#57267,#57268,#57269,
#57270,#57271,#57272,#57273,#57274,#57275),(#57276,#57277,#57278,#57279,
#57280,#57281,#57282,#57283,#57284,#57285,#57286,#57287,#57288,#57289,#57290,
#57291,#57292,#57293,#57294,#57295,#57296,#57297,#57298,#57299,#57300,#57301,
#57302,#57303,#57304,#57305,#57306,#57307,#57308,#57309,#57310,#57311,#57312,
#57313,#57314,#57315,#57316,#57317,#57318,#57319,#57320,#57321,#57322,#57323,
#57324,#57325,#57326,#57327,#57328,#57329,#57330,#57331,#57332,#57333,#57334,
#57335,#57336,#57337,#57338,#57339,#57340,#57341,#57342,#57343,#57344,#57345,
#57346,#57347,#57348,#57349,#57350,#57351,#57352,#57353,#57354,#57355,#57356,
#57357,#57358,#57359,#57360,#57361,#57362,#57363,#57364,#57365,#57366,#57367,
#57368),(#57369,#57370,#57371,#57372,#57373,#57374,#57375,#57376,#57377,
#57378,#57379,#57380,#57381,#57382,#57383,#57384,#57385,#57386,#57387,#57388,
#57389,#57390,#57391,#57392,#57393,#57394,#57395,#57396,#57397,#57398,#57399,
#57400,#57401,#57402,#57403,#57404,#57405,#57406,#57407,#57408,#57409,#57410,
#57411,#57412,#57413,#57414,#57415,#57416,#57417,#57418,#57419,#57420,#57421,
#57422,#57423,#57424,#57425,#57426,#57427,#57428,#57429,#57430,#57431,#57432,
#57433,#57434,#57435,#57436,#57437,#57438,#57439,#57440,#57441,#57442,#57443,
#57444,#57445,#57446,#57447,#57448,#57449,#57450,#57451,#57452,#57453,#57454,
#57455,#57456,#57457,#57458,#57459,#57460,#57461)),.UNSPECIFIED.,.F.,.F.,
 .F.,(4,4),(4,1,1,1,1,1,1,1,1,1,1,1,1,1,1,1,1,1,1,1,1,1,1,1,1,1,1,1,1,1,
1,1,1,1,1,1,1,1,1,1,1,1,1,1,1,1,1,1,1,1,1,1,1,1,1,1,1,1,1,1,1,1,1,1,1,1,
1,1,1,1,1,1,1,1,1,1,1,1,1,1,1,1,1,1,1,1,1,1,1,1,4),(0.,0.0820126057383863),
(8.31473274985796,9.31317630325708,10.3116198566562,11.3100634100553,12.3085069634544,
13.3069505168535,14.3053940702527,15.3038376236518,16.3022811770509,17.30072473045,
18.2991682838491,19.2976118372482,20.2960553906474,21.2944989440465,22.2929424974456,
23.2913860508447,24.2898296042438,25.2882731576429,26.2867167110421,27.2851602644412,
28.2836038178403,29.2820473712394,30.2804909246385,31.2789344780376,32.2773780314368,
33.2758215848359,34.274265138235,35.2727086916341,36.2711522450332,37.2695957984323,
38.2680393518314,39.2664829052306,40.2649264586297,41.2633700120288,42.2618135654279,
43.260257118827,44.2587006722261,45.2571442256253,46.2555877790244,47.2540313324235,
48.2524748858226,49.2509184392217,50.2493619926208,51.2478055460199,52.2462490994191,
53.2446926528182,54.2431362062173,55.2415797596164,56.2400233130155,57.2384668664147,
58.2369104198138,59.2353539732129,60.233797526612,61.2322410800111,62.2306846334102,
63.2291281868093,64.2275717402085,65.2260152936076,66.2244588470067,67.2229024004058,
68.2213459538049,69.219789507204,70.2182330606032,71.2166766140023,72.2151201674014,
73.2135637208005,74.2120072741996,75.2104508275987,76.2088943809979,77.207337934397,
78.2057814877961,79.2042250411952,80.2026685945943,81.2011121479934,82.1995557013926,
83.1979992547917,84.1964428081908,85.1948863615899,86.193329914989,87.1917734683881,
88.1902170217872,89.1886605751864,90.1871041285855,91.1855476819846,92.1839912353837,
93.1824347887828,94.1808783421819,95.1793218955811,96.1777654489802,97.1762090023793,
98.1746525557784),.UNSPECIFIED.);
#165=B_SPLINE_SURFACE_WITH_KNOTS('',3,3,((#57702,#57703,#57704,#57705,#57706,
#57707,#57708,#57709,#57710,#57711,#57712,#57713,#57714,#57715,#57716,#57717,
#57718,#57719,#57720,#57721,#57722,#57723,#57724,#57725,#57726,#57727,#57728,
#57729,#57730,#57731,#57732,#57733,#57734,#57735,#57736,#57737,#57738,#57739,
#57740,#57741,#57742,#57743,#57744,#57745,#57746,#57747,#57748,#57749,#57750,
#57751,#57752,#57753,#57754,#57755,#57756,#57757,#57758,#57759,#57760,#57761,
#57762,#57763,#57764,#57765,#57766,#57767,#57768,#57769,#57770,#57771,#57772,
#57773,#57774,#57775,#57776,#57777,#57778,#57779,#57780,#57781,#57782,#57783,
#57784,#57785,#57786,#57787,#57788,#57789,#57790,#57791,#57792,#57793,#57794),
(#57795,#57796,#57797,#57798,#57799,#57800,#57801,#57802,#57803,#57804,
#57805,#57806,#57807,#57808,#57809,#57810,#57811,#57812,#57813,#57814,#57815,
#57816,#57817,#57818,#57819,#57820,#57821,#57822,#57823,#57824,#57825,#57826,
#57827,#57828,#57829,#57830,#57831,#57832,#57833,#57834,#57835,#57836,#57837,
#57838,#57839,#57840,#57841,#57842,#57843,#57844,#57845,#57846,#57847,#57848,
#57849,#57850,#57851,#57852,#57853,#57854,#57855,#57856,#57857,#57858,#57859,
#57860,#57861,#57862,#57863,#57864,#57865,#57866,#57867,#57868,#57869,#57870,
#57871,#57872,#57873,#57874,#57875,#57876,#57877,#57878,#57879,#57880,#57881,
#57882,#57883,#57884,#57885,#57886,#57887),(#57888,#57889,#57890,#57891,
#57892,#57893,#57894,#57895,#57896,#57897,#57898,#57899,#57900,#57901,#57902,
#57903,#57904,#57905,#57906,#57907,#57908,#57909,#57910,#57911,#57912,#57913,
#57914,#57915,#57916,#57917,#57918,#57919,#57920,#57921,#57922,#57923,#57924,
#57925,#57926,#57927,#57928,#57929,#57930,#57931,#57932,#57933,#57934,#57935,
#57936,#57937,#57938,#57939,#57940,#57941,#57942,#57943,#57944,#57945,#57946,
#57947,#57948,#57949,#57950,#57951,#57952,#57953,#57954,#57955,#57956,#57957,
#57958,#57959,#57960,#57961,#57962,#57963,#57964,#57965,#57966,#57967,#57968,
#57969,#57970,#57971,#57972,#57973,#57974,#57975,#57976,#57977,#57978,#57979,
#57980),(#57981,#57982,#57983,#57984,#57985,#57986,#57987,#57988,#57989,
#57990,#57991,#57992,#57993,#57994,#57995,#57996,#57997,#57998,#57999,#58000,
#58001,#58002,#58003,#58004,#58005,#58006,#58007,#58008,#58009,#58010,#58011,
#58012,#58013,#58014,#58015,#58016,#58017,#58018,#58019,#58020,#58021,#58022,
#58023,#58024,#58025,#58026,#58027,#58028,#58029,#58030,#58031,#58032,#58033,
#58034,#58035,#58036,#58037,#58038,#58039,#58040,#58041,#58042,#58043,#58044,
#58045,#58046,#58047,#58048,#58049,#58050,#58051,#58052,#58053,#58054,#58055,
#58056,#58057,#58058,#58059,#58060,#58061,#58062,#58063,#58064,#58065,#58066,
#58067,#58068,#58069,#58070,#58071,#58072,#58073)),.UNSPECIFIED.,.F.,.F.,
 .F.,(4,4),(4,1,1,1,1,1,1,1,1,1,1,1,1,1,1,1,1,1,1,1,1,1,1,1,1,1,1,1,1,1,
1,1,1,1,1,1,1,1,1,1,1,1,1,1,1,1,1,1,1,1,1,1,1,1,1,1,1,1,1,1,1,1,1,1,1,1,
1,1,1,1,1,1,1,1,1,1,1,1,1,1,1,1,1,1,1,1,1,1,1,1,4),(0.,0.0820126057383863),
(11.6152142277547,12.6136577811538,13.6121013345529,14.610544887952,15.6089884413511,
16.6074319947502,17.6058755481493,18.6043191015485,19.6027626549476,20.6012062083467,
21.5996497617458,22.5980933151449,23.596536868544,24.5949804219432,25.5934239753423,
26.5918675287414,27.5903110821405,28.5887546355396,29.5871981889387,30.5856417423379,
31.584085295737,32.5825288491361,33.5809724025352,34.5794159559343,35.5778595093334,
36.5763030627326,37.5747466161317,38.5731901695308,39.5716337229299,40.570077276329,
41.5685208297281,42.5669643831273,43.5654079365264,44.5638514899255,45.5622950433246,
46.5607385967237,47.5591821501228,48.557625703522,49.5560692569211,50.5545128103202,
51.5529563637193,52.5513999171184,53.5498434705175,54.5482870239167,55.5467305773158,
56.5451741307149,57.543617684114,58.5420612375131,59.5405047909122,60.5389483443114,
61.5373918977105,62.5358354511096,63.5342790045087,64.5327225579078,65.5311661113069,
66.529609664706,67.5280532181052,68.5264967715043,69.5249403249034,70.5233838783025,
71.5218274317016,72.5202709851007,73.5187145384999,74.517158091899,75.5156016452981,
76.5140451986972,77.5124887520963,78.5109323054954,79.5093758588945,80.5078194122937,
81.5062629656928,82.5047065190919,83.503150072491,84.5015936258901,85.5000371792893,
86.4984807326884,87.4969242860875,88.4953678394866,89.4938113928857,90.4922549462848,
91.4906984996839,92.4891420530831,93.4875856064822,94.4860291598813,95.4844727132804,
96.4829162666795,97.4813598200786,98.4798033734778,99.4782469268769,100.476690480276,
101.475134033675),.UNSPECIFIED.);
#166=B_SPLINE_SURFACE_WITH_KNOTS('',3,3,((#60732,#60733,#60734,#60735,#60736,
#60737,#60738,#60739,#60740,#60741,#60742,#60743,#60744,#60745,#60746,#60747,
#60748,#60749,#60750,#60751,#60752,#60753,#60754,#60755,#60756,#60757,#60758,
#60759,#60760,#60761,#60762,#60763,#60764,#60765,#60766,#60767,#60768,#60769,
#60770,#60771,#60772,#60773,#60774,#60775,#60776,#60777,#60778,#60779,#60780,
#60781,#60782,#60783,#60784,#60785,#60786,#60787,#60788,#60789,#60790,#60791,
#60792,#60793,#60794,#60795,#60796,#60797,#60798,#60799,#60800,#60801,#60802,
#60803,#60804,#60805,#60806,#60807,#60808,#60809,#60810,#60811,#60812,#60813,
#60814,#60815,#60816,#60817,#60818,#60819,#60820,#60821,#60822,#60823,#60824,
#60825,#60826,#60827,#60828,#60829,#60830,#60831,#60832,#60833,#60834,#60835,
#60836,#60837,#60838,#60839,#60840,#60841,#60842,#60843,#60844,#60845,#60846,
#60847,#60848,#60849,#60850,#60851,#60852,#60853,#60854,#60855,#60856,#60857,
#60858,#60859,#60860,#60861,#60862,#60863,#60864,#60865,#60866,#60867,#60868,
#60869,#60870,#60871,#60872,#60873,#60874,#60875,#60876,#60877,#60878,#60879,
#60880,#60881,#60882,#60883,#60884,#60885,#60886,#60887,#60888,#60889,#60890,
#60891,#60892,#60893,#60894,#60895,#60896,#60897,#60898,#60899,#60900,#60901,
#60902,#60903,#60904,#60905,#60906,#60907,#60908,#60909,#60910,#60911,#60912,
#60913,#60914,#60915,#60916,#60917,#60918,#60919,#60920,#60921,#60922,#60923,
#60924,#60925,#60926,#60927,#60928,#60929,#60930,#60931,#60932,#60933,#60934,
#60935,#60936,#60937,#60938,#60939,#60940,#60941,#60942,#60943,#60944,#60945,
#60946,#60947,#60948,#60949,#60950,#60951,#60952,#60953,#60954,#60955,#60956,
#60957,#60958,#60959,#60960,#60961,#60962,#60963,#60964,#60965,#60966,#60967,
#60968,#60969,#60970,#60971,#60972,#60973,#60974,#60975,#60976,#60977,#60978,
#60979,#60980,#60981,#60982,#60983,#60984,#60985,#60986,#60987,#60988),
(#60989,#60990,#60991,#60992,#60993,#60994,#60995,#60996,#60997,#60998,
#60999,#61000,#61001,#61002,#61003,#61004,#61005,#61006,#61007,#61008,#61009,
#61010,#61011,#61012,#61013,#61014,#61015,#61016,#61017,#61018,#61019,#61020,
#61021,#61022,#61023,#61024,#61025,#61026,#61027,#61028,#61029,#61030,#61031,
#61032,#61033,#61034,#61035,#61036,#61037,#61038,#61039,#61040,#61041,#61042,
#61043,#61044,#61045,#61046,#61047,#61048,#61049,#61050,#61051,#61052,#61053,
#61054,#61055,#61056,#61057,#61058,#61059,#61060,#61061,#61062,#61063,#61064,
#61065,#61066,#61067,#61068,#61069,#61070,#61071,#61072,#61073,#61074,#61075,
#61076,#61077,#61078,#61079,#61080,#61081,#61082,#61083,#61084,#61085,#61086,
#61087,#61088,#61089,#61090,#61091,#61092,#61093,#61094,#61095,#61096,#61097,
#61098,#61099,#61100,#61101,#61102,#61103,#61104,#61105,#61106,#61107,#61108,
#61109,#61110,#61111,#61112,#61113,#61114,#61115,#61116,#61117,#61118,#61119,
#61120,#61121,#61122,#61123,#61124,#61125,#61126,#61127,#61128,#61129,#61130,
#61131,#61132,#61133,#61134,#61135,#61136,#61137,#61138,#61139,#61140,#61141,
#61142,#61143,#61144,#61145,#61146,#61147,#61148,#61149,#61150,#61151,#61152,
#61153,#61154,#61155,#61156,#61157,#61158,#61159,#61160,#61161,#61162,#61163,
#61164,#61165,#61166,#61167,#61168,#61169,#61170,#61171,#61172,#61173,#61174,
#61175,#61176,#61177,#61178,#61179,#61180,#61181,#61182,#61183,#61184,#61185,
#61186,#61187,#61188,#61189,#61190,#61191,#61192,#61193,#61194,#61195,#61196,
#61197,#61198,#61199,#61200,#61201,#61202,#61203,#61204,#61205,#61206,#61207,
#61208,#61209,#61210,#61211,#61212,#61213,#61214,#61215,#61216,#61217,#61218,
#61219,#61220,#61221,#61222,#61223,#61224,#61225,#61226,#61227,#61228,#61229,
#61230,#61231,#61232,#61233,#61234,#61235,#61236,#61237,#61238,#61239,#61240,
#61241,#61242,#61243,#61244,#61245),(#61246,#61247,#61248,#61249,#61250,
#61251,#61252,#61253,#61254,#61255,#61256,#61257,#61258,#61259,#61260,#61261,
#61262,#61263,#61264,#61265,#61266,#61267,#61268,#61269,#61270,#61271,#61272,
#61273,#61274,#61275,#61276,#61277,#61278,#61279,#61280,#61281,#61282,#61283,
#61284,#61285,#61286,#61287,#61288,#61289,#61290,#61291,#61292,#61293,#61294,
#61295,#61296,#61297,#61298,#61299,#61300,#61301,#61302,#61303,#61304,#61305,
#61306,#61307,#61308,#61309,#61310,#61311,#61312,#61313,#61314,#61315,#61316,
#61317,#61318,#61319,#61320,#61321,#61322,#61323,#61324,#61325,#61326,#61327,
#61328,#61329,#61330,#61331,#61332,#61333,#61334,#61335,#61336,#61337,#61338,
#61339,#61340,#61341,#61342,#61343,#61344,#61345,#61346,#61347,#61348,#61349,
#61350,#61351,#61352,#61353,#61354,#61355,#61356,#61357,#61358,#61359,#61360,
#61361,#61362,#61363,#61364,#61365,#61366,#61367,#61368,#61369,#61370,#61371,
#61372,#61373,#61374,#61375,#61376,#61377,#61378,#61379,#61380,#61381,#61382,
#61383,#61384,#61385,#61386,#61387,#61388,#61389,#61390,#61391,#61392,#61393,
#61394,#61395,#61396,#61397,#61398,#61399,#61400,#61401,#61402,#61403,#61404,
#61405,#61406,#61407,#61408,#61409,#61410,#61411,#61412,#61413,#61414,#61415,
#61416,#61417,#61418,#61419,#61420,#61421,#61422,#61423,#61424,#61425,#61426,
#61427,#61428,#61429,#61430,#61431,#61432,#61433,#61434,#61435,#61436,#61437,
#61438,#61439,#61440,#61441,#61442,#61443,#61444,#61445,#61446,#61447,#61448,
#61449,#61450,#61451,#61452,#61453,#61454,#61455,#61456,#61457,#61458,#61459,
#61460,#61461,#61462,#61463,#61464,#61465,#61466,#61467,#61468,#61469,#61470,
#61471,#61472,#61473,#61474,#61475,#61476,#61477,#61478,#61479,#61480,#61481,
#61482,#61483,#61484,#61485,#61486,#61487,#61488,#61489,#61490,#61491,#61492,
#61493,#61494,#61495,#61496,#61497,#61498,#61499,#61500,#61501,#61502),
(#61503,#61504,#61505,#61506,#61507,#61508,#61509,#61510,#61511,#61512,
#61513,#61514,#61515,#61516,#61517,#61518,#61519,#61520,#61521,#61522,#61523,
#61524,#61525,#61526,#61527,#61528,#61529,#61530,#61531,#61532,#61533,#61534,
#61535,#61536,#61537,#61538,#61539,#61540,#61541,#61542,#61543,#61544,#61545,
#61546,#61547,#61548,#61549,#61550,#61551,#61552,#61553,#61554,#61555,#61556,
#61557,#61558,#61559,#61560,#61561,#61562,#61563,#61564,#61565,#61566,#61567,
#61568,#61569,#61570,#61571,#61572,#61573,#61574,#61575,#61576,#61577,#61578,
#61579,#61580,#61581,#61582,#61583,#61584,#61585,#61586,#61587,#61588,#61589,
#61590,#61591,#61592,#61593,#61594,#61595,#61596,#61597,#61598,#61599,#61600,
#61601,#61602,#61603,#61604,#61605,#61606,#61607,#61608,#61609,#61610,#61611,
#61612,#61613,#61614,#61615,#61616,#61617,#61618,#61619,#61620,#61621,#61622,
#61623,#61624,#61625,#61626,#61627,#61628,#61629,#61630,#61631,#61632,#61633,
#61634,#61635,#61636,#61637,#61638,#61639,#61640,#61641,#61642,#61643,#61644,
#61645,#61646,#61647,#61648,#61649,#61650,#61651,#61652,#61653,#61654,#61655,
#61656,#61657,#61658,#61659,#61660,#61661,#61662,#61663,#61664,#61665,#61666,
#61667,#61668,#61669,#61670,#61671,#61672,#61673,#61674,#61675,#61676,#61677,
#61678,#61679,#61680,#61681,#61682,#61683,#61684,#61685,#61686,#61687,#61688,
#61689,#61690,#61691,#61692,#61693,#61694,#61695,#61696,#61697,#61698,#61699,
#61700,#61701,#61702,#61703,#61704,#61705,#61706,#61707,#61708,#61709,#61710,
#61711,#61712,#61713,#61714,#61715,#61716,#61717,#61718,#61719,#61720,#61721,
#61722,#61723,#61724,#61725,#61726,#61727,#61728,#61729,#61730,#61731,#61732,
#61733,#61734,#61735,#61736,#61737,#61738,#61739,#61740,#61741,#61742,#61743,
#61744,#61745,#61746,#61747,#61748,#61749,#61750,#61751,#61752,#61753,#61754,
#61755,#61756,#61757,#61758,#61759)),.UNSPECIFIED.,.F.,.F.,.F.,(4,4),(4,
1,1,1,1,1,1,1,1,1,1,1,1,1,1,1,1,1,1,1,1,1,1,1,1,1,1,1,1,1,1,1,1,1,1,1,1,
1,1,1,1,1,1,1,1,1,1,1,1,1,1,1,1,1,1,1,1,1,1,1,1,1,1,1,1,1,1,1,1,1,1,1,1,
1,1,1,1,1,1,1,1,1,1,1,1,1,1,1,1,1,1,1,1,1,1,1,1,1,1,1,1,1,1,1,1,1,1,1,1,
1,1,1,1,1,1,1,1,1,1,1,1,1,1,1,1,1,1,1,1,1,1,1,1,1,1,1,1,1,1,1,1,1,1,1,1,
1,1,1,1,1,1,1,1,1,1,1,1,1,1,1,1,1,1,1,1,1,1,1,1,1,1,1,1,1,1,1,1,1,1,1,1,
1,1,1,1,1,1,1,1,1,1,1,1,1,1,1,1,1,1,1,1,1,1,1,1,1,1,1,1,1,1,1,1,1,1,1,1,
1,1,1,1,1,1,1,1,1,1,1,1,1,1,1,1,1,1,1,1,1,1,1,1,1,1,1,1,1,1,1,1,1,1,1,1,
1,4),(0.,0.132097741590587),(8.30112925462614,8.79771720254068,9.29430515045521,
9.79089309836974,10.2874810462843,10.7840689941988,11.2806569421133,11.7772448900279,
12.2738328379424,12.7704207858569,13.2670087337715,13.763596681686,14.2601846296005,
14.7567725775151,15.2533605254296,15.7499484733441,16.2465364212587,16.7431243691732,
17.2397123170877,17.7363002650023,18.2328882129168,18.7294761608313,19.2260641087459,
19.7226520566604,20.2192400045749,20.7158279524895,21.212415900404,21.7090038483185,
22.2055917962331,22.7021797441476,23.1987676920621,23.6953556399767,24.1919435878912,
24.6885315358057,25.1851194837203,25.6817074316348,26.1782953795493,26.6748833274639,
27.1714712753784,27.6680592232929,28.1646471712075,28.661235119122,29.1578230670365,
29.6544110149511,30.1509989628656,30.6475869107801,31.1441748586947,31.6407628066092,
32.1373507545237,32.6339387024382,33.1305266503528,33.6271145982673,34.1237025461818,
34.6202904940964,35.1168784420109,35.6134663899254,36.11005433784,36.6066422857545,
37.103230233669,37.5998181815836,38.0964061294981,38.5929940774126,39.0895820253272,
39.5861699732417,40.0827579211562,40.5793458690708,41.0759338169853,41.5725217648998,
42.0691097128144,42.5656976607289,43.0622856086434,43.558873556558,44.0554615044725,
44.552049452387,45.0486374003016,45.5452253482161,46.0418132961306,46.5384012440452,
47.0349891919597,47.5315771398742,48.0281650877888,48.5247530357033,49.0213409836178,
49.5179289315324,50.0145168794469,50.5111048273614,51.007692775276,51.5042807231905,
52.000868671105,52.4974566190196,52.9940445669341,53.4906325148486,53.9872204627632,
54.4838084106777,54.9803963585922,55.4769843065068,55.9735722544213,56.4701602023358,
56.9667481502504,57.4633360981649,57.9599240460794,58.456511993994,58.9530999419085,
59.449687889823,59.9462758377375,60.4428637856521,60.9394517335666,61.4360396814811,
61.9326276293957,62.4292155773102,62.9258035252248,63.4223914731393,63.9189794210538,
64.4155673689683,64.9121553168829,65.4087432647974,65.9053312127119,66.4019191606265,
66.898507108541,67.3950950564555,67.8916830043701,68.3882709522846,68.8848589001991,
69.3814468481137,69.8780347960282,70.3746227439427,70.8712106918573,71.3677986397718,
71.8643865876863,72.3609745356009,72.8575624835154,73.3541504314299,73.8507383793445,
74.347326327259,74.8439142751735,75.3405022230881,75.8370901710026,76.3336781189171,
76.8302660668317,77.3268540147462,77.8234419626607,78.3200299105753,78.8166178584898,
79.3132058064043,79.8097937543189,80.3063817022334,80.8029696501479,81.2995575980625,
81.796145545977,82.2927334938915,82.7893214418061,83.2859093897206,83.7824973376351,
84.2790852855497,84.7756732334642,85.2722611813787,85.7688491292933,86.2654370772078,
86.7620250251223,87.2586129730369,87.7552009209514,88.2517888688659,88.7483768167804,
89.244964764695,89.7415527126095,90.2381406605241,90.7347286084386,91.2313165563531,
91.7279045042677,92.2244924521822,92.7210804000967,93.2176683480112,93.7142562959258,
94.2108442438403,94.7074321917548,95.2040201396694,95.7006080875839,96.1971960354985,
96.693783983413,97.1903719313275,97.686959879242,98.1835478271566,98.6801357750711,
99.1767237229856,99.6733116709002,100.169899618815,100.666487566729,101.163075514644,
101.659663462558,102.156251410473,102.652839358387,103.149427306302,103.646015254216,
104.142603202131,104.639191150046,105.13577909796,105.632367045875,106.128954993789,
106.625542941704,107.122130889618,107.618718837533,108.115306785447,108.611894733362,
109.108482681276,109.605070629191,110.101658577105,110.59824652502,111.094834472934,
111.591422420849,112.088010368763,112.584598316678,113.081186264593,113.577774212507,
114.074362160422,114.570950108336,115.067538056251,115.564126004165,116.06071395208,
116.557301899994,117.053889847909,117.550477795823,118.047065743738,118.543653691652,
119.040241639567,119.536829587481,120.033417535396,120.530005483311,121.026593431225,
121.52318137914,122.019769327054,122.516357274969,123.012945222883,123.509533170798,
124.006121118712,124.502709066627,124.999297014541,125.495884962456,125.99247291037,
126.489060858285,126.985648806199,127.482236754114,127.978824702029,128.475412649943,
128.972000597858,129.468588545772,129.965176493687,130.461764441601,130.958352389516,
131.45494033743,131.951528285345,132.448116233259,132.944704181174,133.441292129088,
133.937880077003,134.434468024917),.UNSPECIFIED.);
#167=B_SPLINE_SURFACE_WITH_KNOTS('',3,3,((#62045,#62046,#62047,#62048,#62049,
#62050,#62051,#62052,#62053,#62054,#62055,#62056,#62057,#62058,#62059,#62060,
#62061,#62062,#62063,#62064,#62065,#62066,#62067,#62068,#62069,#62070,#62071,
#62072,#62073,#62074,#62075,#62076,#62077,#62078,#62079,#62080,#62081,#62082,
#62083,#62084,#62085,#62086,#62087,#62088,#62089,#62090,#62091,#62092,#62093,
#62094,#62095,#62096,#62097,#62098,#62099,#62100,#62101,#62102,#62103,#62104,
#62105,#62106,#62107,#62108,#62109,#62110,#62111,#62112,#62113,#62114,#62115,
#62116,#62117,#62118,#62119,#62120,#62121,#62122,#62123,#62124,#62125,#62126,
#62127,#62128,#62129,#62130,#62131,#62132,#62133,#62134,#62135,#62136,#62137,
#62138,#62139,#62140,#62141,#62142,#62143,#62144,#62145,#62146,#62147,#62148,
#62149,#62150,#62151,#62152,#62153,#62154,#62155,#62156,#62157,#62158,#62159,
#62160,#62161,#62162,#62163,#62164,#62165,#62166,#62167,#62168,#62169,#62170,
#62171,#62172,#62173,#62174,#62175,#62176,#62177,#62178,#62179,#62180,#62181,
#62182,#62183,#62184,#62185,#62186,#62187,#62188,#62189,#62190,#62191,#62192,
#62193,#62194,#62195,#62196,#62197,#62198,#62199,#62200,#62201,#62202,#62203,
#62204,#62205,#62206,#62207,#62208,#62209,#62210,#62211,#62212,#62213,#62214,
#62215,#62216,#62217,#62218,#62219,#62220,#62221,#62222,#62223,#62224,#62225,
#62226,#62227,#62228,#62229,#62230,#62231,#62232,#62233,#62234,#62235,#62236,
#62237,#62238,#62239,#62240,#62241,#62242,#62243,#62244,#62245,#62246,#62247,
#62248,#62249,#62250,#62251,#62252,#62253,#62254,#62255,#62256,#62257,#62258,
#62259,#62260,#62261,#62262,#62263,#62264,#62265,#62266,#62267,#62268,#62269,
#62270,#62271,#62272,#62273,#62274,#62275,#62276,#62277,#62278,#62279,#62280,
#62281,#62282,#62283,#62284,#62285,#62286,#62287,#62288,#62289,#62290,#62291,
#62292,#62293,#62294,#62295,#62296,#62297,#62298,#62299,#62300,#62301),
(#62302,#62303,#62304,#62305,#62306,#62307,#62308,#62309,#62310,#62311,
#62312,#62313,#62314,#62315,#62316,#62317,#62318,#62319,#62320,#62321,#62322,
#62323,#62324,#62325,#62326,#62327,#62328,#62329,#62330,#62331,#62332,#62333,
#62334,#62335,#62336,#62337,#62338,#62339,#62340,#62341,#62342,#62343,#62344,
#62345,#62346,#62347,#62348,#62349,#62350,#62351,#62352,#62353,#62354,#62355,
#62356,#62357,#62358,#62359,#62360,#62361,#62362,#62363,#62364,#62365,#62366,
#62367,#62368,#62369,#62370,#62371,#62372,#62373,#62374,#62375,#62376,#62377,
#62378,#62379,#62380,#62381,#62382,#62383,#62384,#62385,#62386,#62387,#62388,
#62389,#62390,#62391,#62392,#62393,#62394,#62395,#62396,#62397,#62398,#62399,
#62400,#62401,#62402,#62403,#62404,#62405,#62406,#62407,#62408,#62409,#62410,
#62411,#62412,#62413,#62414,#62415,#62416,#62417,#62418,#62419,#62420,#62421,
#62422,#62423,#62424,#62425,#62426,#62427,#62428,#62429,#62430,#62431,#62432,
#62433,#62434,#62435,#62436,#62437,#62438,#62439,#62440,#62441,#62442,#62443,
#62444,#62445,#62446,#62447,#62448,#62449,#62450,#62451,#62452,#62453,#62454,
#62455,#62456,#62457,#62458,#62459,#62460,#62461,#62462,#62463,#62464,#62465,
#62466,#62467,#62468,#62469,#62470,#62471,#62472,#62473,#62474,#62475,#62476,
#62477,#62478,#62479,#62480,#62481,#62482,#62483,#62484,#62485,#62486,#62487,
#62488,#62489,#62490,#62491,#62492,#62493,#62494,#62495,#62496,#62497,#62498,
#62499,#62500,#62501,#62502,#62503,#62504,#62505,#62506,#62507,#62508,#62509,
#62510,#62511,#62512,#62513,#62514,#62515,#62516,#62517,#62518,#62519,#62520,
#62521,#62522,#62523,#62524,#62525,#62526,#62527,#62528,#62529,#62530,#62531,
#62532,#62533,#62534,#62535,#62536,#62537,#62538,#62539,#62540,#62541,#62542,
#62543,#62544,#62545,#62546,#62547,#62548,#62549,#62550,#62551,#62552,#62553,
#62554,#62555,#62556,#62557,#62558),(#62559,#62560,#62561,#62562,#62563,
#62564,#62565,#62566,#62567,#62568,#62569,#62570,#62571,#62572,#62573,#62574,
#62575,#62576,#62577,#62578,#62579,#62580,#62581,#62582,#62583,#62584,#62585,
#62586,#62587,#62588,#62589,#62590,#62591,#62592,#62593,#62594,#62595,#62596,
#62597,#62598,#62599,#62600,#62601,#62602,#62603,#62604,#62605,#62606,#62607,
#62608,#62609,#62610,#62611,#62612,#62613,#62614,#62615,#62616,#62617,#62618,
#62619,#62620,#62621,#62622,#62623,#62624,#62625,#62626,#62627,#62628,#62629,
#62630,#62631,#62632,#62633,#62634,#62635,#62636,#62637,#62638,#62639,#62640,
#62641,#62642,#62643,#62644,#62645,#62646,#62647,#62648,#62649,#62650,#62651,
#62652,#62653,#62654,#62655,#62656,#62657,#62658,#62659,#62660,#62661,#62662,
#62663,#62664,#62665,#62666,#62667,#62668,#62669,#62670,#62671,#62672,#62673,
#62674,#62675,#62676,#62677,#62678,#62679,#62680,#62681,#62682,#62683,#62684,
#62685,#62686,#62687,#62688,#62689,#62690,#62691,#62692,#62693,#62694,#62695,
#62696,#62697,#62698,#62699,#62700,#62701,#62702,#62703,#62704,#62705,#62706,
#62707,#62708,#62709,#62710,#62711,#62712,#62713,#62714,#62715,#62716,#62717,
#62718,#62719,#62720,#62721,#62722,#62723,#62724,#62725,#62726,#62727,#62728,
#62729,#62730,#62731,#62732,#62733,#62734,#62735,#62736,#62737,#62738,#62739,
#62740,#62741,#62742,#62743,#62744,#62745,#62746,#62747,#62748,#62749,#62750,
#62751,#62752,#62753,#62754,#62755,#62756,#62757,#62758,#62759,#62760,#62761,
#62762,#62763,#62764,#62765,#62766,#62767,#62768,#62769,#62770,#62771,#62772,
#62773,#62774,#62775,#62776,#62777,#62778,#62779,#62780,#62781,#62782,#62783,
#62784,#62785,#62786,#62787,#62788,#62789,#62790,#62791,#62792,#62793,#62794,
#62795,#62796,#62797,#62798,#62799,#62800,#62801,#62802,#62803,#62804,#62805,
#62806,#62807,#62808,#62809,#62810,#62811,#62812,#62813,#62814,#62815),
(#62816,#62817,#62818,#62819,#62820,#62821,#62822,#62823,#62824,#62825,
#62826,#62827,#62828,#62829,#62830,#62831,#62832,#62833,#62834,#62835,#62836,
#62837,#62838,#62839,#62840,#62841,#62842,#62843,#62844,#62845,#62846,#62847,
#62848,#62849,#62850,#62851,#62852,#62853,#62854,#62855,#62856,#62857,#62858,
#62859,#62860,#62861,#62862,#62863,#62864,#62865,#62866,#62867,#62868,#62869,
#62870,#62871,#62872,#62873,#62874,#62875,#62876,#62877,#62878,#62879,#62880,
#62881,#62882,#62883,#62884,#62885,#62886,#62887,#62888,#62889,#62890,#62891,
#62892,#62893,#62894,#62895,#62896,#62897,#62898,#62899,#62900,#62901,#62902,
#62903,#62904,#62905,#62906,#62907,#62908,#62909,#62910,#62911,#62912,#62913,
#62914,#62915,#62916,#62917,#62918,#62919,#62920,#62921,#62922,#62923,#62924,
#62925,#62926,#62927,#62928,#62929,#62930,#62931,#62932,#62933,#62934,#62935,
#62936,#62937,#62938,#62939,#62940,#62941,#62942,#62943,#62944,#62945,#62946,
#62947,#62948,#62949,#62950,#62951,#62952,#62953,#62954,#62955,#62956,#62957,
#62958,#62959,#62960,#62961,#62962,#62963,#62964,#62965,#62966,#62967,#62968,
#62969,#62970,#62971,#62972,#62973,#62974,#62975,#62976,#62977,#62978,#62979,
#62980,#62981,#62982,#62983,#62984,#62985,#62986,#62987,#62988,#62989,#62990,
#62991,#62992,#62993,#62994,#62995,#62996,#62997,#62998,#62999,#63000,#63001,
#63002,#63003,#63004,#63005,#63006,#63007,#63008,#63009,#63010,#63011,#63012,
#63013,#63014,#63015,#63016,#63017,#63018,#63019,#63020,#63021,#63022,#63023,
#63024,#63025,#63026,#63027,#63028,#63029,#63030,#63031,#63032,#63033,#63034,
#63035,#63036,#63037,#63038,#63039,#63040,#63041,#63042,#63043,#63044,#63045,
#63046,#63047,#63048,#63049,#63050,#63051,#63052,#63053,#63054,#63055,#63056,
#63057,#63058,#63059,#63060,#63061,#63062,#63063,#63064,#63065,#63066,#63067,
#63068,#63069,#63070,#63071,#63072)),.UNSPECIFIED.,.F.,.F.,.F.,(4,4),(4,
1,1,1,1,1,1,1,1,1,1,1,1,1,1,1,1,1,1,1,1,1,1,1,1,1,1,1,1,1,1,1,1,1,1,1,1,
1,1,1,1,1,1,1,1,1,1,1,1,1,1,1,1,1,1,1,1,1,1,1,1,1,1,1,1,1,1,1,1,1,1,1,1,
1,1,1,1,1,1,1,1,1,1,1,1,1,1,1,1,1,1,1,1,1,1,1,1,1,1,1,1,1,1,1,1,1,1,1,1,
1,1,1,1,1,1,1,1,1,1,1,1,1,1,1,1,1,1,1,1,1,1,1,1,1,1,1,1,1,1,1,1,1,1,1,1,
1,1,1,1,1,1,1,1,1,1,1,1,1,1,1,1,1,1,1,1,1,1,1,1,1,1,1,1,1,1,1,1,1,1,1,1,
1,1,1,1,1,1,1,1,1,1,1,1,1,1,1,1,1,1,1,1,1,1,1,1,1,1,1,1,1,1,1,1,1,1,1,1,
1,1,1,1,1,1,1,1,1,1,1,1,1,1,1,1,1,1,1,1,1,1,1,1,1,1,1,1,1,1,1,1,1,1,1,1,
1,4),(0.,0.132097741590587),(11.6150328478182,12.1116207957327,12.6082087436472,
13.1047966915618,13.6013846394763,14.0979725873908,14.5945605353054,15.0911484832199,
15.5877364311344,16.084324379049,16.5809123269635,17.077500274878,17.5740882227926,
18.0706761707071,18.5672641186216,19.0638520665362,19.5604400144507,20.0570279623652,
20.5536159102798,21.0502038581943,21.5467918061088,22.0433797540234,22.5399677019379,
23.0365556498524,23.533143597767,24.0297315456815,24.526319493596,25.0229074415106,
25.5194953894251,26.0160833373396,26.5126712852542,27.0092592331687,27.5058471810832,
28.0024351289978,28.4990230769123,28.9956110248268,29.4921989727414,29.9887869206559,
30.4853748685704,30.981962816485,31.4785507643995,31.975138712314,32.4717266602286,
32.9683146081431,33.4649025560576,33.9614905039722,34.4580784518867,34.9546663998012,
35.4512543477158,35.9478422956303,36.4444302435448,36.9410181914593,37.4376061393739,
37.9341940872884,38.430782035203,38.9273699831175,39.423957931032,39.9205458789466,
40.4171338268611,40.9137217747756,41.4103097226902,41.9068976706047,42.4034856185192,
42.9000735664337,43.3966615143483,43.8932494622628,44.3898374101773,44.8864253580919,
45.3830133060064,45.8796012539209,46.3761892018355,46.87277714975,47.3693650976645,
47.8659530455791,48.3625409934936,48.8591289414081,49.3557168893227,49.8523048372372,
50.3488927851517,50.8454807330663,51.3420686809808,51.8386566288953,52.3352445768099,
52.8318325247244,53.3284204726389,53.8250084205535,54.321596368468,54.8181843163825,
55.3147722642971,55.8113602122116,56.3079481601261,56.8045361080407,57.3011240559552,
57.7977120038697,58.2942999517843,58.7908878996988,59.2874758476133,59.7840637955279,
60.2806517434424,60.7772396913569,61.2738276392715,61.770415587186,62.2670035351005,
62.7635914830151,63.2601794309296,63.7567673788441,64.2533553267587,64.7499432746732,
65.2465312225877,65.7431191705023,66.2397071184168,66.7362950663313,67.2328830142459,
67.7294709621604,68.2260589100749,68.7226468579895,69.219234805904,69.7158227538185,
70.2124107017331,70.7089986496476,71.2055865975621,71.7021745454767,72.1987624933912,
72.6953504413057,73.1919383892203,73.6885263371348,74.1851142850493,74.6817022329639,
75.1782901808784,75.6748781287929,76.1714660767074,76.668054024622,77.1646419725365,
77.661229920451,78.1578178683656,78.6544058162801,79.1509937641947,79.6475817121092,
80.1441696600237,80.6407576079382,81.1373455558528,81.6339335037673,82.1305214516818,
82.6271093995964,83.1236973475109,83.6202852954254,84.11687324334,84.6134611912545,
85.110049139169,85.6066370870836,86.1032250349981,86.5998129829126,87.0964009308272,
87.5929888787417,88.0895768266562,88.5861647745708,89.0827527224853,89.5793406703998,
90.0759286183144,90.5725165662289,91.0691045141434,91.565692462058,92.0622804099725,
92.558868357887,93.0554563058016,93.5520442537161,94.0486322016306,94.5452201495452,
95.0418080974597,95.5383960453742,96.0349839932888,96.5315719412033,97.0281598891178,
97.5247478370324,98.0213357849469,98.5179237328614,99.014511680776,99.5110996286905,
100.007687576605,100.50427552452,101.000863472434,101.497451420349,101.994039368263,
102.490627316178,102.987215264092,103.483803212007,103.980391159921,104.476979107836,
104.97356705575,105.470155003665,105.966742951579,106.463330899494,106.959918847408,
107.456506795323,107.953094743238,108.449682691152,108.946270639067,109.442858586981,
109.939446534896,110.43603448281,110.932622430725,111.429210378639,111.925798326554,
112.422386274468,112.918974222383,113.415562170297,113.912150118212,114.408738066126,
114.905326014041,115.401913961956,115.89850190987,116.395089857785,116.891677805699,
117.388265753614,117.884853701528,118.381441649443,118.878029597357,119.374617545272,
119.871205493186,120.367793441101,120.864381389015,121.36096933693,121.857557284844,
122.354145232759,122.850733180674,123.347321128588,123.843909076503,124.340497024417,
124.837084972332,125.333672920246,125.830260868161,126.326848816075,126.82343676399,
127.320024711904,127.816612659819,128.313200607733,128.809788555648,129.306376503562,
129.802964451477,130.299552399392,130.796140347306,131.292728295221,131.789316243135,
132.28590419105,132.782492138964,133.279080086879,133.775668034793,134.272255982708,
134.768843930622,135.265431878537,135.762019826451,136.258607774366,136.75519572228,
137.251783670195,137.74837161811),.UNSPECIFIED.);
#168=B_SPLINE_SURFACE_WITH_KNOTS('',3,3,((#66314,#66315,#66316,#66317,#66318,
#66319,#66320,#66321,#66322,#66323,#66324,#66325,#66326,#66327,#66328,#66329,
#66330,#66331,#66332,#66333,#66334,#66335,#66336,#66337,#66338,#66339,#66340,
#66341,#66342,#66343,#66344,#66345,#66346,#66347,#66348,#66349,#66350,#66351,
#66352,#66353,#66354,#66355,#66356,#66357,#66358,#66359,#66360,#66361,#66362,
#66363,#66364,#66365,#66366,#66367,#66368,#66369,#66370,#66371,#66372,#66373,
#66374,#66375,#66376,#66377,#66378,#66379,#66380,#66381,#66382,#66383,#66384,
#66385,#66386,#66387,#66388,#66389,#66390,#66391,#66392,#66393,#66394,#66395,
#66396,#66397,#66398,#66399,#66400,#66401,#66402,#66403,#66404,#66405,#66406,
#66407,#66408,#66409,#66410,#66411,#66412,#66413,#66414,#66415,#66416,#66417,
#66418,#66419,#66420,#66421,#66422,#66423,#66424,#66425,#66426,#66427,#66428,
#66429,#66430,#66431,#66432,#66433,#66434,#66435,#66436,#66437,#66438,#66439,
#66440,#66441,#66442,#66443,#66444,#66445,#66446,#66447,#66448,#66449,#66450,
#66451,#66452,#66453,#66454,#66455,#66456,#66457,#66458,#66459,#66460,#66461,
#66462,#66463,#66464,#66465,#66466,#66467,#66468,#66469,#66470,#66471,#66472,
#66473,#66474,#66475,#66476,#66477,#66478,#66479,#66480,#66481,#66482,#66483,
#66484,#66485,#66486,#66487,#66488,#66489,#66490,#66491,#66492,#66493,#66494,
#66495,#66496,#66497,#66498,#66499,#66500,#66501,#66502,#66503,#66504,#66505,
#66506,#66507,#66508,#66509,#66510,#66511,#66512,#66513,#66514,#66515,#66516,
#66517,#66518,#66519,#66520,#66521,#66522,#66523,#66524,#66525,#66526,#66527,
#66528,#66529,#66530,#66531,#66532,#66533,#66534,#66535,#66536,#66537,#66538,
#66539,#66540,#66541,#66542,#66543,#66544,#66545,#66546,#66547,#66548,#66549,
#66550,#66551,#66552,#66553,#66554,#66555,#66556,#66557,#66558,#66559,#66560,
#66561,#66562,#66563,#66564,#66565,#66566,#66567,#66568,#66569,#66570,#66571,
#66572,#66573,#66574,#66575,#66576,#66577,#66578,#66579,#66580,#66581,#66582,
#66583,#66584,#66585,#66586,#66587,#66588,#66589,#66590,#66591,#66592,#66593,
#66594,#66595,#66596,#66597,#66598,#66599,#66600,#66601,#66602,#66603,#66604),
(#66605,#66606,#66607,#66608,#66609,#66610,#66611,#66612,#66613,#66614,
#66615,#66616,#66617,#66618,#66619,#66620,#66621,#66622,#66623,#66624,#66625,
#66626,#66627,#66628,#66629,#66630,#66631,#66632,#66633,#66634,#66635,#66636,
#66637,#66638,#66639,#66640,#66641,#66642,#66643,#66644,#66645,#66646,#66647,
#66648,#66649,#66650,#66651,#66652,#66653,#66654,#66655,#66656,#66657,#66658,
#66659,#66660,#66661,#66662,#66663,#66664,#66665,#66666,#66667,#66668,#66669,
#66670,#66671,#66672,#66673,#66674,#66675,#66676,#66677,#66678,#66679,#66680,
#66681,#66682,#66683,#66684,#66685,#66686,#66687,#66688,#66689,#66690,#66691,
#66692,#66693,#66694,#66695,#66696,#66697,#66698,#66699,#66700,#66701,#66702,
#66703,#66704,#66705,#66706,#66707,#66708,#66709,#66710,#66711,#66712,#66713,
#66714,#66715,#66716,#66717,#66718,#66719,#66720,#66721,#66722,#66723,#66724,
#66725,#66726,#66727,#66728,#66729,#66730,#66731,#66732,#66733,#66734,#66735,
#66736,#66737,#66738,#66739,#66740,#66741,#66742,#66743,#66744,#66745,#66746,
#66747,#66748,#66749,#66750,#66751,#66752,#66753,#66754,#66755,#66756,#66757,
#66758,#66759,#66760,#66761,#66762,#66763,#66764,#66765,#66766,#66767,#66768,
#66769,#66770,#66771,#66772,#66773,#66774,#66775,#66776,#66777,#66778,#66779,
#66780,#66781,#66782,#66783,#66784,#66785,#66786,#66787,#66788,#66789,#66790,
#66791,#66792,#66793,#66794,#66795,#66796,#66797,#66798,#66799,#66800,#66801,
#66802,#66803,#66804,#66805,#66806,#66807,#66808,#66809,#66810,#66811,#66812,
#66813,#66814,#66815,#66816,#66817,#66818,#66819,#66820,#66821,#66822,#66823,
#66824,#66825,#66826,#66827,#66828,#66829,#66830,#66831,#66832,#66833,#66834,
#66835,#66836,#66837,#66838,#66839,#66840,#66841,#66842,#66843,#66844,#66845,
#66846,#66847,#66848,#66849,#66850,#66851,#66852,#66853,#66854,#66855,#66856,
#66857,#66858,#66859,#66860,#66861,#66862,#66863,#66864,#66865,#66866,#66867,
#66868,#66869,#66870,#66871,#66872,#66873,#66874,#66875,#66876,#66877,#66878,
#66879,#66880,#66881,#66882,#66883,#66884,#66885,#66886,#66887,#66888,#66889,
#66890,#66891,#66892,#66893,#66894,#66895),(#66896,#66897,#66898,#66899,
#66900,#66901,#66902,#66903,#66904,#66905,#66906,#66907,#66908,#66909,#66910,
#66911,#66912,#66913,#66914,#66915,#66916,#66917,#66918,#66919,#66920,#66921,
#66922,#66923,#66924,#66925,#66926,#66927,#66928,#66929,#66930,#66931,#66932,
#66933,#66934,#66935,#66936,#66937,#66938,#66939,#66940,#66941,#66942,#66943,
#66944,#66945,#66946,#66947,#66948,#66949,#66950,#66951,#66952,#66953,#66954,
#66955,#66956,#66957,#66958,#66959,#66960,#66961,#66962,#66963,#66964,#66965,
#66966,#66967,#66968,#66969,#66970,#66971,#66972,#66973,#66974,#66975,#66976,
#66977,#66978,#66979,#66980,#66981,#66982,#66983,#66984,#66985,#66986,#66987,
#66988,#66989,#66990,#66991,#66992,#66993,#66994,#66995,#66996,#66997,#66998,
#66999,#67000,#67001,#67002,#67003,#67004,#67005,#67006,#67007,#67008,#67009,
#67010,#67011,#67012,#67013,#67014,#67015,#67016,#67017,#67018,#67019,#67020,
#67021,#67022,#67023,#67024,#67025,#67026,#67027,#67028,#67029,#67030,#67031,
#67032,#67033,#67034,#67035,#67036,#67037,#67038,#67039,#67040,#67041,#67042,
#67043,#67044,#67045,#67046,#67047,#67048,#67049,#67050,#67051,#67052,#67053,
#67054,#67055,#67056,#67057,#67058,#67059,#67060,#67061,#67062,#67063,#67064,
#67065,#67066,#67067,#67068,#67069,#67070,#67071,#67072,#67073,#67074,#67075,
#67076,#67077,#67078,#67079,#67080,#67081,#67082,#67083,#67084,#67085,#67086,
#67087,#67088,#67089,#67090,#67091,#67092,#67093,#67094,#67095,#67096,#67097,
#67098,#67099,#67100,#67101,#67102,#67103,#67104,#67105,#67106,#67107,#67108,
#67109,#67110,#67111,#67112,#67113,#67114,#67115,#67116,#67117,#67118,#67119,
#67120,#67121,#67122,#67123,#67124,#67125,#67126,#67127,#67128,#67129,#67130,
#67131,#67132,#67133,#67134,#67135,#67136,#67137,#67138,#67139,#67140,#67141,
#67142,#67143,#67144,#67145,#67146,#67147,#67148,#67149,#67150,#67151,#67152,
#67153,#67154,#67155,#67156,#67157,#67158,#67159,#67160,#67161,#67162,#67163,
#67164,#67165,#67166,#67167,#67168,#67169,#67170,#67171,#67172,#67173,#67174,
#67175,#67176,#67177,#67178,#67179,#67180,#67181,#67182,#67183,#67184,#67185,
#67186),(#67187,#67188,#67189,#67190,#67191,#67192,#67193,#67194,#67195,
#67196,#67197,#67198,#67199,#67200,#67201,#67202,#67203,#67204,#67205,#67206,
#67207,#67208,#67209,#67210,#67211,#67212,#67213,#67214,#67215,#67216,#67217,
#67218,#67219,#67220,#67221,#67222,#67223,#67224,#67225,#67226,#67227,#67228,
#67229,#67230,#67231,#67232,#67233,#67234,#67235,#67236,#67237,#67238,#67239,
#67240,#67241,#67242,#67243,#67244,#67245,#67246,#67247,#67248,#67249,#67250,
#67251,#67252,#67253,#67254,#67255,#67256,#67257,#67258,#67259,#67260,#67261,
#67262,#67263,#67264,#67265,#67266,#67267,#67268,#67269,#67270,#67271,#67272,
#67273,#67274,#67275,#67276,#67277,#67278,#67279,#67280,#67281,#67282,#67283,
#67284,#67285,#67286,#67287,#67288,#67289,#67290,#67291,#67292,#67293,#67294,
#67295,#67296,#67297,#67298,#67299,#67300,#67301,#67302,#67303,#67304,#67305,
#67306,#67307,#67308,#67309,#67310,#67311,#67312,#67313,#67314,#67315,#67316,
#67317,#67318,#67319,#67320,#67321,#67322,#67323,#67324,#67325,#67326,#67327,
#67328,#67329,#67330,#67331,#67332,#67333,#67334,#67335,#67336,#67337,#67338,
#67339,#67340,#67341,#67342,#67343,#67344,#67345,#67346,#67347,#67348,#67349,
#67350,#67351,#67352,#67353,#67354,#67355,#67356,#67357,#67358,#67359,#67360,
#67361,#67362,#67363,#67364,#67365,#67366,#67367,#67368,#67369,#67370,#67371,
#67372,#67373,#67374,#67375,#67376,#67377,#67378,#67379,#67380,#67381,#67382,
#67383,#67384,#67385,#67386,#67387,#67388,#67389,#67390,#67391,#67392,#67393,
#67394,#67395,#67396,#67397,#67398,#67399,#67400,#67401,#67402,#67403,#67404,
#67405,#67406,#67407,#67408,#67409,#67410,#67411,#67412,#67413,#67414,#67415,
#67416,#67417,#67418,#67419,#67420,#67421,#67422,#67423,#67424,#67425,#67426,
#67427,#67428,#67429,#67430,#67431,#67432,#67433,#67434,#67435,#67436,#67437,
#67438,#67439,#67440,#67441,#67442,#67443,#67444,#67445,#67446,#67447,#67448,
#67449,#67450,#67451,#67452,#67453,#67454,#67455,#67456,#67457,#67458,#67459,
#67460,#67461,#67462,#67463,#67464,#67465,#67466,#67467,#67468,#67469,#67470,
#67471,#67472,#67473,#67474,#67475,#67476,#67477)),.UNSPECIFIED.,.F.,.F.,
 .F.,(4,4),(4,1,1,1,1,1,1,1,1,1,1,1,1,1,1,1,1,1,1,1,1,1,1,1,1,1,1,1,1,1,
1,1,1,1,1,1,1,1,1,1,1,1,1,1,1,1,1,1,1,1,1,1,1,1,1,1,1,1,1,1,1,1,1,1,1,1,
1,1,1,1,1,1,1,1,1,1,1,1,1,1,1,1,1,1,1,1,1,1,1,1,1,1,1,1,1,1,1,1,1,1,1,1,
1,1,1,1,1,1,1,1,1,1,1,1,1,1,1,1,1,1,1,1,1,1,1,1,1,1,1,1,1,1,1,1,1,1,1,1,
1,1,1,1,1,1,1,1,1,1,1,1,1,1,1,1,1,1,1,1,1,1,1,1,1,1,1,1,1,1,1,1,1,1,1,1,
1,1,1,1,1,1,1,1,1,1,1,1,1,1,1,1,1,1,1,1,1,1,1,1,1,1,1,1,1,1,1,1,1,1,1,1,
1,1,1,1,1,1,1,1,1,1,1,1,1,1,1,1,1,1,1,1,1,1,1,1,1,1,1,1,1,1,1,1,1,1,1,1,
1,1,1,1,1,1,1,1,1,1,1,1,1,1,1,1,1,1,1,1,1,1,1,1,1,1,1,1,1,1,1,1,1,1,1,1,
1,1,1,1,1,1,4),(0.,0.115296848757168),(8.30592286723176,8.80533305296603,
9.30474323870031,9.80415342443458,10.3035636101689,10.8029737959031,11.3023839816374,
11.8017941673717,12.301204353106,12.8006145388402,13.3000247245745,13.7994349103088,
14.298845096043,14.7982552817773,15.2976654675116,15.7970756532459,16.2964858389801,
16.7958960247144,17.2953062104487,17.794716396183,18.2941265819172,18.7935367676515,
19.2929469533858,19.7923571391201,20.2917673248543,20.7911775105886,21.2905876963229,
21.7899978820572,22.2894080677914,22.7888182535257,23.28822843926,23.7876386249943,
24.2870488107285,24.7864589964628,25.2858691821971,25.7852793679313,26.2846895536656,
26.7840997393999,27.2835099251342,27.7829201108684,28.2823302966027,28.781740482337,
29.2811506680713,29.7805608538055,30.2799710395398,30.7793812252741,31.2787914110084,
31.7782015967426,32.2776117824769,32.7770219682112,33.2764321539455,33.7758423396797,
34.275252525414,34.7746627111483,35.2740728968826,35.7734830826168,36.2728932683511,
36.7723034540854,37.2717136398197,37.7711238255539,38.2705340112882,38.7699441970225,
39.2693543827567,39.768764568491,40.2681747542253,40.7675849399596,41.2669951256938,
41.7664053114281,42.2658154971624,42.7652256828967,43.2646358686309,43.7640460543652,
44.2634562400995,44.7628664258338,45.262276611568,45.7616867973023,46.2610969830366,
46.7605071687709,47.2599173545051,47.7593275402394,48.2587377259737,48.758147911708,
49.2575580974422,49.7569682831765,50.2563784689108,50.755788654645,51.2551988403793,
51.7546090261136,52.2540192118479,52.7534293975821,53.2528395833164,53.7522497690507,
54.251659954785,54.7510701405192,55.2504803262535,55.7498905119878,56.2493006977221,
56.7487108834563,57.2481210691906,57.7475312549249,58.2469414406592,58.7463516263934,
59.2457618121277,59.745171997862,60.2445821835963,60.7439923693305,61.2434025550648,
61.7428127407991,62.2422229265333,62.7416331122676,63.2410432980019,63.7404534837362,
64.2398636694704,64.7392738552047,65.238684040939,65.7380942266733,66.2375044124075,
66.7369145981418,67.2363247838761,67.7357349696103,68.2351451553446,68.7345553410789,
69.2339655268132,69.7333757125475,70.2327858982817,70.732196084016,71.2316062697503,
71.7310164554845,72.2304266412188,72.7298368269531,73.2292470126874,73.7286571984216,
74.2280673841559,74.7274775698902,75.2268877556245,75.7262979413587,76.225708127093,
76.7251183128273,77.2245284985616,77.7239386842958,78.2233488700301,78.7227590557644,
79.2221692414986,79.7215794272329,80.2209896129672,80.7203997987015,81.2198099844358,
81.71922017017,82.2186303559043,82.7180405416386,83.2174507273728,83.7168609131071,
84.2162710988414,84.7156812845757,85.2150914703099,85.7145016560442,86.2139118417785,
86.7133220275128,87.212732213247,87.7121423989813,88.2115525847156,88.7109627704499,
89.2103729561841,89.7097831419184,90.2091933276527,90.7086035133869,91.2080136991212,
91.7074238848555,92.2068340705898,92.7062442563241,93.2056544420583,93.7050646277926,
94.2044748135269,94.7038849992611,95.2032951849954,95.7027053707297,96.202115556464,
96.7015257421982,97.2009359279325,97.7003461136668,98.1997562994011,98.6991664851353,
99.1985766708696,99.6979868566039,100.197397042338,100.696807228072,101.196217413807,
101.695627599541,102.195037785275,102.69444797101,103.193858156744,103.693268342478,
104.192678528212,104.692088713947,105.191498899681,105.690909085415,106.190319271149,
106.689729456884,107.189139642618,107.688549828352,108.187960014087,108.687370199821,
109.186780385555,109.686190571289,110.185600757024,110.685010942758,111.184421128492,
111.683831314226,112.183241499961,112.682651685695,113.182061871429,113.681472057164,
114.180882242898,114.680292428632,115.179702614366,115.679112800101,116.178522985835,
116.677933171569,117.177343357303,117.676753543038,118.176163728772,118.675573914506,
119.174984100241,119.674394285975,120.173804471709,120.673214657443,121.172624843178,
121.672035028912,122.171445214646,122.67085540038,123.170265586115,123.669675771849,
124.169085957583,124.668496143318,125.167906329052,125.667316514786,126.16672670052,
126.666136886255,127.165547071989,127.664957257723,128.164367443458,128.663777629192,
129.163187814926,129.66259800066,130.162008186395,130.661418372129,131.160828557863,
131.660238743597,132.159648929332,132.659059115066,133.1584693008,133.657879486535,
134.157289672269,134.656699858003,135.156110043737,135.655520229472,136.154930415206,
136.65434060094,137.153750786674,137.653160972409,138.152571158143,138.651981343877,
139.151391529612,139.650801715346,140.15021190108,140.649622086814,141.149032272549,
141.648442458283,142.147852644017,142.647262829751,143.146673015486,143.64608320122,
144.145493386954,144.644903572689,145.144313758423,145.643723944157,146.143134129891,
146.642544315626,147.14195450136,147.641364687094,148.140774872828,148.640185058563,
149.139595244297,149.639005430031,150.138415615766,150.6378258015,151.137235987234,
151.636646172968,152.136056358703),.UNSPECIFIED.);
#169=B_SPLINE_SURFACE_WITH_KNOTS('',3,3,((#67742,#67743,#67744,#67745,#67746,
#67747,#67748,#67749,#67750,#67751,#67752,#67753,#67754,#67755,#67756,#67757,
#67758,#67759,#67760,#67761,#67762,#67763,#67764,#67765,#67766,#67767,#67768,
#67769,#67770,#67771,#67772,#67773,#67774,#67775,#67776,#67777,#67778,#67779,
#67780,#67781,#67782,#67783,#67784,#67785,#67786,#67787,#67788,#67789,#67790,
#67791,#67792,#67793,#67794,#67795,#67796,#67797,#67798,#67799,#67800,#67801,
#67802,#67803,#67804,#67805,#67806,#67807,#67808,#67809,#67810,#67811,#67812,
#67813,#67814,#67815,#67816,#67817,#67818,#67819,#67820,#67821,#67822,#67823,
#67824,#67825,#67826,#67827,#67828,#67829,#67830,#67831,#67832,#67833,#67834,
#67835,#67836,#67837,#67838,#67839,#67840,#67841,#67842,#67843,#67844,#67845,
#67846,#67847,#67848,#67849,#67850,#67851,#67852,#67853,#67854,#67855,#67856,
#67857,#67858,#67859,#67860,#67861,#67862,#67863,#67864,#67865,#67866,#67867,
#67868,#67869,#67870,#67871,#67872,#67873,#67874,#67875,#67876,#67877,#67878,
#67879,#67880,#67881,#67882,#67883,#67884,#67885,#67886,#67887,#67888,#67889,
#67890,#67891,#67892,#67893,#67894,#67895,#67896,#67897,#67898,#67899,#67900,
#67901,#67902,#67903,#67904,#67905,#67906,#67907,#67908,#67909,#67910,#67911,
#67912,#67913,#67914,#67915,#67916,#67917,#67918,#67919,#67920,#67921,#67922,
#67923,#67924,#67925,#67926,#67927,#67928,#67929,#67930,#67931,#67932,#67933,
#67934,#67935,#67936,#67937,#67938,#67939,#67940,#67941,#67942,#67943,#67944,
#67945,#67946,#67947,#67948,#67949,#67950,#67951,#67952,#67953,#67954,#67955,
#67956,#67957,#67958,#67959,#67960,#67961,#67962,#67963,#67964,#67965,#67966,
#67967,#67968,#67969,#67970,#67971,#67972,#67973,#67974,#67975,#67976,#67977,
#67978,#67979,#67980,#67981,#67982,#67983,#67984,#67985,#67986,#67987,#67988,
#67989,#67990,#67991,#67992,#67993,#67994,#67995,#67996,#67997,#67998,#67999,
#68000,#68001,#68002,#68003,#68004,#68005,#68006,#68007,#68008,#68009,#68010,
#68011,#68012,#68013,#68014,#68015,#68016,#68017,#68018,#68019,#68020,#68021,
#68022,#68023,#68024,#68025,#68026,#68027,#68028,#68029,#68030,#68031,#68032),
(#68033,#68034,#68035,#68036,#68037,#68038,#68039,#68040,#68041,#68042,
#68043,#68044,#68045,#68046,#68047,#68048,#68049,#68050,#68051,#68052,#68053,
#68054,#68055,#68056,#68057,#68058,#68059,#68060,#68061,#68062,#68063,#68064,
#68065,#68066,#68067,#68068,#68069,#68070,#68071,#68072,#68073,#68074,#68075,
#68076,#68077,#68078,#68079,#68080,#68081,#68082,#68083,#68084,#68085,#68086,
#68087,#68088,#68089,#68090,#68091,#68092,#68093,#68094,#68095,#68096,#68097,
#68098,#68099,#68100,#68101,#68102,#68103,#68104,#68105,#68106,#68107,#68108,
#68109,#68110,#68111,#68112,#68113,#68114,#68115,#68116,#68117,#68118,#68119,
#68120,#68121,#68122,#68123,#68124,#68125,#68126,#68127,#68128,#68129,#68130,
#68131,#68132,#68133,#68134,#68135,#68136,#68137,#68138,#68139,#68140,#68141,
#68142,#68143,#68144,#68145,#68146,#68147,#68148,#68149,#68150,#68151,#68152,
#68153,#68154,#68155,#68156,#68157,#68158,#68159,#68160,#68161,#68162,#68163,
#68164,#68165,#68166,#68167,#68168,#68169,#68170,#68171,#68172,#68173,#68174,
#68175,#68176,#68177,#68178,#68179,#68180,#68181,#68182,#68183,#68184,#68185,
#68186,#68187,#68188,#68189,#68190,#68191,#68192,#68193,#68194,#68195,#68196,
#68197,#68198,#68199,#68200,#68201,#68202,#68203,#68204,#68205,#68206,#68207,
#68208,#68209,#68210,#68211,#68212,#68213,#68214,#68215,#68216,#68217,#68218,
#68219,#68220,#68221,#68222,#68223,#68224,#68225,#68226,#68227,#68228,#68229,
#68230,#68231,#68232,#68233,#68234,#68235,#68236,#68237,#68238,#68239,#68240,
#68241,#68242,#68243,#68244,#68245,#68246,#68247,#68248,#68249,#68250,#68251,
#68252,#68253,#68254,#68255,#68256,#68257,#68258,#68259,#68260,#68261,#68262,
#68263,#68264,#68265,#68266,#68267,#68268,#68269,#68270,#68271,#68272,#68273,
#68274,#68275,#68276,#68277,#68278,#68279,#68280,#68281,#68282,#68283,#68284,
#68285,#68286,#68287,#68288,#68289,#68290,#68291,#68292,#68293,#68294,#68295,
#68296,#68297,#68298,#68299,#68300,#68301,#68302,#68303,#68304,#68305,#68306,
#68307,#68308,#68309,#68310,#68311,#68312,#68313,#68314,#68315,#68316,#68317,
#68318,#68319,#68320,#68321,#68322,#68323),(#68324,#68325,#68326,#68327,
#68328,#68329,#68330,#68331,#68332,#68333,#68334,#68335,#68336,#68337,#68338,
#68339,#68340,#68341,#68342,#68343,#68344,#68345,#68346,#68347,#68348,#68349,
#68350,#68351,#68352,#68353,#68354,#68355,#68356,#68357,#68358,#68359,#68360,
#68361,#68362,#68363,#68364,#68365,#68366,#68367,#68368,#68369,#68370,#68371,
#68372,#68373,#68374,#68375,#68376,#68377,#68378,#68379,#68380,#68381,#68382,
#68383,#68384,#68385,#68386,#68387,#68388,#68389,#68390,#68391,#68392,#68393,
#68394,#68395,#68396,#68397,#68398,#68399,#68400,#68401,#68402,#68403,#68404,
#68405,#68406,#68407,#68408,#68409,#68410,#68411,#68412,#68413,#68414,#68415,
#68416,#68417,#68418,#68419,#68420,#68421,#68422,#68423,#68424,#68425,#68426,
#68427,#68428,#68429,#68430,#68431,#68432,#68433,#68434,#68435,#68436,#68437,
#68438,#68439,#68440,#68441,#68442,#68443,#68444,#68445,#68446,#68447,#68448,
#68449,#68450,#68451,#68452,#68453,#68454,#68455,#68456,#68457,#68458,#68459,
#68460,#68461,#68462,#68463,#68464,#68465,#68466,#68467,#68468,#68469,#68470,
#68471,#68472,#68473,#68474,#68475,#68476,#68477,#68478,#68479,#68480,#68481,
#68482,#68483,#68484,#68485,#68486,#68487,#68488,#68489,#68490,#68491,#68492,
#68493,#68494,#68495,#68496,#68497,#68498,#68499,#68500,#68501,#68502,#68503,
#68504,#68505,#68506,#68507,#68508,#68509,#68510,#68511,#68512,#68513,#68514,
#68515,#68516,#68517,#68518,#68519,#68520,#68521,#68522,#68523,#68524,#68525,
#68526,#68527,#68528,#68529,#68530,#68531,#68532,#68533,#68534,#68535,#68536,
#68537,#68538,#68539,#68540,#68541,#68542,#68543,#68544,#68545,#68546,#68547,
#68548,#68549,#68550,#68551,#68552,#68553,#68554,#68555,#68556,#68557,#68558,
#68559,#68560,#68561,#68562,#68563,#68564,#68565,#68566,#68567,#68568,#68569,
#68570,#68571,#68572,#68573,#68574,#68575,#68576,#68577,#68578,#68579,#68580,
#68581,#68582,#68583,#68584,#68585,#68586,#68587,#68588,#68589,#68590,#68591,
#68592,#68593,#68594,#68595,#68596,#68597,#68598,#68599,#68600,#68601,#68602,
#68603,#68604,#68605,#68606,#68607,#68608,#68609,#68610,#68611,#68612,#68613,
#68614),(#68615,#68616,#68617,#68618,#68619,#68620,#68621,#68622,#68623,
#68624,#68625,#68626,#68627,#68628,#68629,#68630,#68631,#68632,#68633,#68634,
#68635,#68636,#68637,#68638,#68639,#68640,#68641,#68642,#68643,#68644,#68645,
#68646,#68647,#68648,#68649,#68650,#68651,#68652,#68653,#68654,#68655,#68656,
#68657,#68658,#68659,#68660,#68661,#68662,#68663,#68664,#68665,#68666,#68667,
#68668,#68669,#68670,#68671,#68672,#68673,#68674,#68675,#68676,#68677,#68678,
#68679,#68680,#68681,#68682,#68683,#68684,#68685,#68686,#68687,#68688,#68689,
#68690,#68691,#68692,#68693,#68694,#68695,#68696,#68697,#68698,#68699,#68700,
#68701,#68702,#68703,#68704,#68705,#68706,#68707,#68708,#68709,#68710,#68711,
#68712,#68713,#68714,#68715,#68716,#68717,#68718,#68719,#68720,#68721,#68722,
#68723,#68724,#68725,#68726,#68727,#68728,#68729,#68730,#68731,#68732,#68733,
#68734,#68735,#68736,#68737,#68738,#68739,#68740,#68741,#68742,#68743,#68744,
#68745,#68746,#68747,#68748,#68749,#68750,#68751,#68752,#68753,#68754,#68755,
#68756,#68757,#68758,#68759,#68760,#68761,#68762,#68763,#68764,#68765,#68766,
#68767,#68768,#68769,#68770,#68771,#68772,#68773,#68774,#68775,#68776,#68777,
#68778,#68779,#68780,#68781,#68782,#68783,#68784,#68785,#68786,#68787,#68788,
#68789,#68790,#68791,#68792,#68793,#68794,#68795,#68796,#68797,#68798,#68799,
#68800,#68801,#68802,#68803,#68804,#68805,#68806,#68807,#68808,#68809,#68810,
#68811,#68812,#68813,#68814,#68815,#68816,#68817,#68818,#68819,#68820,#68821,
#68822,#68823,#68824,#68825,#68826,#68827,#68828,#68829,#68830,#68831,#68832,
#68833,#68834,#68835,#68836,#68837,#68838,#68839,#68840,#68841,#68842,#68843,
#68844,#68845,#68846,#68847,#68848,#68849,#68850,#68851,#68852,#68853,#68854,
#68855,#68856,#68857,#68858,#68859,#68860,#68861,#68862,#68863,#68864,#68865,
#68866,#68867,#68868,#68869,#68870,#68871,#68872,#68873,#68874,#68875,#68876,
#68877,#68878,#68879,#68880,#68881,#68882,#68883,#68884,#68885,#68886,#68887,
#68888,#68889,#68890,#68891,#68892,#68893,#68894,#68895,#68896,#68897,#68898,
#68899,#68900,#68901,#68902,#68903,#68904,#68905)),.UNSPECIFIED.,.F.,.F.,
 .F.,(4,4),(4,1,1,1,1,1,1,1,1,1,1,1,1,1,1,1,1,1,1,1,1,1,1,1,1,1,1,1,1,1,
1,1,1,1,1,1,1,1,1,1,1,1,1,1,1,1,1,1,1,1,1,1,1,1,1,1,1,1,1,1,1,1,1,1,1,1,
1,1,1,1,1,1,1,1,1,1,1,1,1,1,1,1,1,1,1,1,1,1,1,1,1,1,1,1,1,1,1,1,1,1,1,1,
1,1,1,1,1,1,1,1,1,1,1,1,1,1,1,1,1,1,1,1,1,1,1,1,1,1,1,1,1,1,1,1,1,1,1,1,
1,1,1,1,1,1,1,1,1,1,1,1,1,1,1,1,1,1,1,1,1,1,1,1,1,1,1,1,1,1,1,1,1,1,1,1,
1,1,1,1,1,1,1,1,1,1,1,1,1,1,1,1,1,1,1,1,1,1,1,1,1,1,1,1,1,1,1,1,1,1,1,1,
1,1,1,1,1,1,1,1,1,1,1,1,1,1,1,1,1,1,1,1,1,1,1,1,1,1,1,1,1,1,1,1,1,1,1,1,
1,1,1,1,1,1,1,1,1,1,1,1,1,1,1,1,1,1,1,1,1,1,1,1,1,1,1,1,1,1,1,1,1,1,1,1,
1,1,1,1,1,1,4),(0.,0.115296848757168),(11.6154215191107,12.1148317048449,
12.6142418905792,13.1136520763135,13.6130622620478,14.112472447782,14.6118826335163,
15.1112928192506,15.6107030049849,16.1101131907191,16.6095233764534,17.1089335621877,
17.608343747922,18.1077539336562,18.6071641193905,19.1065743051248,19.6059844908591,
20.1053946765933,20.6048048623276,21.1042150480619,21.6036252337962,22.1030354195304,
22.6024456052647,23.101855790999,23.6012659767333,24.1006761624675,24.6000863482018,
25.0994965339361,25.5989067196703,26.0983169054046,26.5977270911389,27.0971372768732,
27.5965474626074,28.0959576483417,28.595367834076,29.0947780198103,29.5941882055445,
30.0935983912788,30.5930085770131,31.0924187627474,31.5918289484816,32.0912391342159,
32.5906493199502,33.0900595056845,33.5894696914187,34.088879877153,34.5882900628873,
35.0877002486216,35.5871104343558,36.0865206200901,36.5859308058244,37.0853409915587,
37.5847511772929,38.0841613630272,38.5835715487615,39.0829817344957,39.58239192023,
40.0818021059643,40.5812122916986,41.0806224774328,41.5800326631671,42.0794428489014,
42.5788530346357,43.0782632203699,43.5776734061042,44.0770835918385,44.5764937775728,
45.075903963307,45.5753141490413,46.0747243347756,46.5741345205099,47.0735447062441,
47.5729548919784,48.0723650777127,48.571775263447,49.0711854491812,49.5705956349155,
50.0700058206498,50.5694160063841,51.0688261921183,51.5682363778526,52.0676465635869,
52.5670567493211,53.0664669350554,53.5658771207897,54.065287306524,54.5646974922582,
55.0641076779925,55.5635178637268,56.0629280494611,56.5623382351953,57.0617484209296,
57.5611586066639,58.0605687923982,58.5599789781324,59.0593891638667,59.558799349601,
60.0582095353353,60.5576197210695,61.0570299068038,61.5564400925381,62.0558502782724,
62.5552604640066,63.0546706497409,63.5540808354752,64.0534910212095,64.5529012069437,
65.052311392678,65.5517215784123,66.0511317641465,66.5505419498808,67.0499521356151,
67.5493623213494,68.0487725070836,68.5481826928179,69.0475928785522,69.5470030642865,
70.0464132500207,70.545823435755,71.0452336214893,71.5446438072236,72.0440539929578,
72.5434641786921,73.0428743644264,73.5422845501607,74.0416947358949,74.5411049216292,
75.0405151073635,75.5399252930978,76.039335478832,76.5387456645663,77.0381558503006,
77.5375660360349,78.0369762217691,78.5363864075034,79.0357965932377,79.5352067789719,
80.0346169647062,80.5340271504405,81.0334373361748,81.532847521909,82.0322577076433,
82.5316678933776,83.0310780791119,83.5304882648461,84.0298984505804,84.5293086363147,
85.028718822049,85.5281290077832,86.0275391935175,86.5269493792518,87.0263595649861,
87.5257697507203,88.0251799364546,88.5245901221889,89.0240003079231,89.5234104936574,
90.0228206793917,90.522230865126,91.0216410508603,91.5210512365945,92.0204614223288,
92.5198716080631,93.0192817937973,93.5186919795316,94.0181021652659,94.5175123510002,
95.0169225367344,95.5163327224687,96.015742908203,96.5151530939373,97.0145632796715,
97.5139734654058,98.0133836511401,98.5127938368744,99.0122040226086,99.5116142083429,
100.011024394077,100.510434579811,101.009844765546,101.50925495128,102.008665137014,
102.508075322749,103.007485508483,103.506895694217,104.006305879951,104.505716065686,
105.00512625142,105.504536437154,106.003946622888,106.503356808623,107.002766994357,
107.502177180091,108.001587365826,108.50099755156,109.000407737294,109.499817923028,
109.999228108763,110.498638294497,110.998048480231,111.497458665965,111.9968688517,
112.496279037434,112.995689223168,113.495099408903,113.994509594637,114.493919780371,
114.993329966105,115.49274015184,115.992150337574,116.491560523308,116.990970709043,
117.490380894777,117.989791080511,118.489201266245,118.98861145198,119.488021637714,
119.987431823448,120.486842009182,120.986252194917,121.485662380651,121.985072566385,
122.48448275212,122.983892937854,123.483303123588,123.982713309322,124.482123495057,
124.981533680791,125.480943866525,125.980354052259,126.479764237994,126.979174423728,
127.478584609462,127.977994795197,128.477404980931,128.976815166665,129.476225352399,
129.975635538134,130.475045723868,130.974455909602,131.473866095336,131.973276281071,
132.472686466805,132.972096652539,133.471506838274,133.970917024008,134.470327209742,
134.969737395476,135.469147581211,135.968557766945,136.467967952679,136.967378138413,
137.466788324148,137.966198509882,138.465608695616,138.965018881351,139.464429067085,
139.963839252819,140.463249438553,140.962659624288,141.462069810022,141.961479995756,
142.46089018149,142.960300367225,143.459710552959,143.959120738693,144.458530924428,
144.957941110162,145.457351295896,145.95676148163,146.456171667365,146.955581853099,
147.454992038833,147.954402224568,148.453812410302,148.953222596036,149.45263278177,
149.952042967505,150.451453153239,150.950863338973,151.450273524707,151.949683710442,
152.449093896176,152.94850408191,153.447914267645,153.947324453379,154.446734639113,
154.946144824847,155.445555010582),.UNSPECIFIED.);
#170=B_SPLINE_SURFACE_WITH_KNOTS('',3,3,((#70882,#70883,#70884,#70885,#70886,
#70887,#70888,#70889,#70890,#70891,#70892,#70893,#70894,#70895,#70896,#70897,
#70898,#70899,#70900,#70901,#70902,#70903,#70904,#70905,#70906,#70907,#70908,
#70909,#70910,#70911,#70912,#70913,#70914,#70915,#70916,#70917,#70918,#70919,
#70920,#70921,#70922,#70923,#70924,#70925,#70926,#70927,#70928,#70929,#70930,
#70931,#70932,#70933,#70934,#70935,#70936,#70937,#70938,#70939,#70940,#70941,
#70942,#70943,#70944,#70945,#70946,#70947,#70948,#70949,#70950,#70951,#70952,
#70953,#70954,#70955,#70956,#70957,#70958,#70959,#70960,#70961,#70962,#70963,
#70964,#70965,#70966,#70967,#70968,#70969,#70970,#70971,#70972,#70973,#70974,
#70975,#70976,#70977,#70978,#70979,#70980,#70981,#70982,#70983,#70984,#70985,
#70986,#70987,#70988,#70989,#70990,#70991,#70992,#70993,#70994,#70995,#70996,
#70997,#70998,#70999,#71000,#71001,#71002,#71003,#71004,#71005,#71006,#71007,
#71008,#71009,#71010,#71011,#71012,#71013,#71014,#71015,#71016,#71017,#71018,
#71019,#71020,#71021,#71022,#71023,#71024,#71025,#71026,#71027,#71028,#71029,
#71030,#71031,#71032),(#71033,#71034,#71035,#71036,#71037,#71038,#71039,
#71040,#71041,#71042,#71043,#71044,#71045,#71046,#71047,#71048,#71049,#71050,
#71051,#71052,#71053,#71054,#71055,#71056,#71057,#71058,#71059,#71060,#71061,
#71062,#71063,#71064,#71065,#71066,#71067,#71068,#71069,#71070,#71071,#71072,
#71073,#71074,#71075,#71076,#71077,#71078,#71079,#71080,#71081,#71082,#71083,
#71084,#71085,#71086,#71087,#71088,#71089,#71090,#71091,#71092,#71093,#71094,
#71095,#71096,#71097,#71098,#71099,#71100,#71101,#71102,#71103,#71104,#71105,
#71106,#71107,#71108,#71109,#71110,#71111,#71112,#71113,#71114,#71115,#71116,
#71117,#71118,#71119,#71120,#71121,#71122,#71123,#71124,#71125,#71126,#71127,
#71128,#71129,#71130,#71131,#71132,#71133,#71134,#71135,#71136,#71137,#71138,
#71139,#71140,#71141,#71142,#71143,#71144,#71145,#71146,#71147,#71148,#71149,
#71150,#71151,#71152,#71153,#71154,#71155,#71156,#71157,#71158,#71159,#71160,
#71161,#71162,#71163,#71164,#71165,#71166,#71167,#71168,#71169,#71170,#71171,
#71172,#71173,#71174,#71175,#71176,#71177,#71178,#71179,#71180,#71181,#71182,
#71183),(#71184,#71185,#71186,#71187,#71188,#71189,#71190,#71191,#71192,
#71193,#71194,#71195,#71196,#71197,#71198,#71199,#71200,#71201,#71202,#71203,
#71204,#71205,#71206,#71207,#71208,#71209,#71210,#71211,#71212,#71213,#71214,
#71215,#71216,#71217,#71218,#71219,#71220,#71221,#71222,#71223,#71224,#71225,
#71226,#71227,#71228,#71229,#71230,#71231,#71232,#71233,#71234,#71235,#71236,
#71237,#71238,#71239,#71240,#71241,#71242,#71243,#71244,#71245,#71246,#71247,
#71248,#71249,#71250,#71251,#71252,#71253,#71254,#71255,#71256,#71257,#71258,
#71259,#71260,#71261,#71262,#71263,#71264,#71265,#71266,#71267,#71268,#71269,
#71270,#71271,#71272,#71273,#71274,#71275,#71276,#71277,#71278,#71279,#71280,
#71281,#71282,#71283,#71284,#71285,#71286,#71287,#71288,#71289,#71290,#71291,
#71292,#71293,#71294,#71295,#71296,#71297,#71298,#71299,#71300,#71301,#71302,
#71303,#71304,#71305,#71306,#71307,#71308,#71309,#71310,#71311,#71312,#71313,
#71314,#71315,#71316,#71317,#71318,#71319,#71320,#71321,#71322,#71323,#71324,
#71325,#71326,#71327,#71328,#71329,#71330,#71331,#71332,#71333,#71334),
(#71335,#71336,#71337,#71338,#71339,#71340,#71341,#71342,#71343,#71344,
#71345,#71346,#71347,#71348,#71349,#71350,#71351,#71352,#71353,#71354,#71355,
#71356,#71357,#71358,#71359,#71360,#71361,#71362,#71363,#71364,#71365,#71366,
#71367,#71368,#71369,#71370,#71371,#71372,#71373,#71374,#71375,#71376,#71377,
#71378,#71379,#71380,#71381,#71382,#71383,#71384,#71385,#71386,#71387,#71388,
#71389,#71390,#71391,#71392,#71393,#71394,#71395,#71396,#71397,#71398,#71399,
#71400,#71401,#71402,#71403,#71404,#71405,#71406,#71407,#71408,#71409,#71410,
#71411,#71412,#71413,#71414,#71415,#71416,#71417,#71418,#71419,#71420,#71421,
#71422,#71423,#71424,#71425,#71426,#71427,#71428,#71429,#71430,#71431,#71432,
#71433,#71434,#71435,#71436,#71437,#71438,#71439,#71440,#71441,#71442,#71443,
#71444,#71445,#71446,#71447,#71448,#71449,#71450,#71451,#71452,#71453,#71454,
#71455,#71456,#71457,#71458,#71459,#71460,#71461,#71462,#71463,#71464,#71465,
#71466,#71467,#71468,#71469,#71470,#71471,#71472,#71473,#71474,#71475,#71476,
#71477,#71478,#71479,#71480,#71481,#71482,#71483,#71484,#71485)),
 .UNSPECIFIED.,.F.,.F.,.F.,(4,4),(4,1,1,1,1,1,1,1,1,1,1,1,1,1,1,1,1,1,1,
1,1,1,1,1,1,1,1,1,1,1,1,1,1,1,1,1,1,1,1,1,1,1,1,1,1,1,1,1,1,1,1,1,1,1,1,
1,1,1,1,1,1,1,1,1,1,1,1,1,1,1,1,1,1,1,1,1,1,1,1,1,1,1,1,1,1,1,1,1,1,1,1,
1,1,1,1,1,1,1,1,1,1,1,1,1,1,1,1,1,1,1,1,1,1,1,1,1,1,1,1,1,1,1,1,1,1,1,1,
1,1,1,1,1,1,1,1,1,1,1,1,1,1,1,1,1,1,1,1,1,4),(0.,0.0986691610045069),(8.3098959515534,
8.80937110859088,9.30884626562835,10.3077965797033,11.3067468937783,12.3056972078532,
13.3046475219282,14.3035978360031,15.3025481500781,16.3014984641531,17.300448778228,
18.299399092303,19.2983494063779,20.2972997204529,21.2962500345278,22.2952003486028,
23.2941506626778,24.2931009767527,25.2920512908277,26.2910016049026,27.2899519189776,
28.2889022330525,29.2878525471275,30.2868028612024,31.2857531752774,32.2847034893524,
33.2836538034273,34.2826041175023,35.2815544315772,36.2805047456522,37.2794550597271,
38.2784053738021,39.2773556878771,40.276306001952,41.275256316027,42.2742066301019,
43.2731569441769,44.2721072582518,45.2710575723268,46.2700078864018,47.2689582004767,
48.2679085145517,49.2668588286266,50.2658091427016,51.2647594567765,52.2637097708515,
53.2626600849265,54.2616103990014,55.2605607130764,56.2595110271513,57.2584613412263,
58.2574116553012,59.2563619693762,60.2553122834511,61.2542625975261,62.2532129116011,
63.252163225676,64.251113539751,65.2500638538259,66.2490141679009,67.2479644819759,
68.2469147960508,69.2458651101258,70.2448154242007,71.2437657382757,72.2427160523506,
73.2416663664256,74.2406166805006,75.2395669945755,76.2385173086505,77.2374676227254,
78.2364179368004,79.2353682508753,80.2343185649503,81.2332688790252,82.2322191931002,
83.2311695071752,84.2301198212501,85.2290701353251,86.2280204494,87.226970763475,
88.2259210775499,89.2248713916249,90.2238217056999,91.2227720197748,92.2217223338498,
93.2206726479247,94.2196229619997,95.2185732760747,96.2175235901496,97.2164739042246,
98.2154242182995,99.2143745323745,100.213324846449,101.212275160524,102.211225474599,
103.210175788674,104.209126102749,105.208076416824,106.207026730899,107.205977044974,
108.204927359049,109.203877673124,110.202827987199,111.201778301274,112.200728615349,
113.199678929424,114.198629243499,115.197579557574,116.196529871649,117.195480185724,
118.194430499799,119.193380813874,120.192331127949,121.191281442024,122.190231756098,
123.189182070173,124.188132384248,125.187082698323,126.186033012398,127.184983326473,
128.183933640548,129.182883954623,130.181834268698,131.180784582773,132.179734896848,
133.178685210923,134.177635524998,135.176585839073,136.175536153148,137.174486467223,
138.173436781298,139.172387095373,140.171337409448,141.170287723523,142.169238037598,
143.168188351673,144.167138665748,145.166088979822,146.165039293897,147.163989607972,
148.162939922047,149.161890236122,150.160840550197,151.159790864272,152.158741178347,
153.157691492422,153.65716664946,154.156641806497),.UNSPECIFIED.);
#171=B_SPLINE_SURFACE_WITH_KNOTS('',3,3,((#71662,#71663,#71664,#71665,#71666,
#71667,#71668,#71669,#71670,#71671,#71672,#71673,#71674,#71675,#71676,#71677,
#71678,#71679,#71680,#71681,#71682,#71683,#71684,#71685,#71686,#71687,#71688,
#71689,#71690,#71691,#71692,#71693,#71694,#71695,#71696,#71697,#71698,#71699,
#71700,#71701,#71702,#71703,#71704,#71705,#71706,#71707,#71708,#71709,#71710,
#71711,#71712,#71713,#71714,#71715,#71716,#71717,#71718,#71719,#71720,#71721,
#71722,#71723,#71724,#71725,#71726,#71727,#71728,#71729,#71730,#71731,#71732,
#71733,#71734,#71735,#71736,#71737,#71738,#71739,#71740,#71741,#71742,#71743,
#71744,#71745,#71746,#71747,#71748,#71749,#71750,#71751,#71752,#71753,#71754,
#71755,#71756,#71757,#71758,#71759,#71760,#71761,#71762,#71763,#71764,#71765,
#71766,#71767,#71768,#71769,#71770,#71771,#71772,#71773,#71774,#71775,#71776,
#71777,#71778,#71779,#71780,#71781,#71782,#71783,#71784,#71785,#71786,#71787,
#71788,#71789,#71790,#71791,#71792,#71793,#71794,#71795,#71796,#71797,#71798,
#71799,#71800,#71801,#71802,#71803,#71804,#71805,#71806,#71807,#71808,#71809,
#71810,#71811,#71812),(#71813,#71814,#71815,#71816,#71817,#71818,#71819,
#71820,#71821,#71822,#71823,#71824,#71825,#71826,#71827,#71828,#71829,#71830,
#71831,#71832,#71833,#71834,#71835,#71836,#71837,#71838,#71839,#71840,#71841,
#71842,#71843,#71844,#71845,#71846,#71847,#71848,#71849,#71850,#71851,#71852,
#71853,#71854,#71855,#71856,#71857,#71858,#71859,#71860,#71861,#71862,#71863,
#71864,#71865,#71866,#71867,#71868,#71869,#71870,#71871,#71872,#71873,#71874,
#71875,#71876,#71877,#71878,#71879,#71880,#71881,#71882,#71883,#71884,#71885,
#71886,#71887,#71888,#71889,#71890,#71891,#71892,#71893,#71894,#71895,#71896,
#71897,#71898,#71899,#71900,#71901,#71902,#71903,#71904,#71905,#71906,#71907,
#71908,#71909,#71910,#71911,#71912,#71913,#71914,#71915,#71916,#71917,#71918,
#71919,#71920,#71921,#71922,#71923,#71924,#71925,#71926,#71927,#71928,#71929,
#71930,#71931,#71932,#71933,#71934,#71935,#71936,#71937,#71938,#71939,#71940,
#71941,#71942,#71943,#71944,#71945,#71946,#71947,#71948,#71949,#71950,#71951,
#71952,#71953,#71954,#71955,#71956,#71957,#71958,#71959,#71960,#71961,#71962,
#71963),(#71964,#71965,#71966,#71967,#71968,#71969,#71970,#71971,#71972,
#71973,#71974,#71975,#71976,#71977,#71978,#71979,#71980,#71981,#71982,#71983,
#71984,#71985,#71986,#71987,#71988,#71989,#71990,#71991,#71992,#71993,#71994,
#71995,#71996,#71997,#71998,#71999,#72000,#72001,#72002,#72003,#72004,#72005,
#72006,#72007,#72008,#72009,#72010,#72011,#72012,#72013,#72014,#72015,#72016,
#72017,#72018,#72019,#72020,#72021,#72022,#72023,#72024,#72025,#72026,#72027,
#72028,#72029,#72030,#72031,#72032,#72033,#72034,#72035,#72036,#72037,#72038,
#72039,#72040,#72041,#72042,#72043,#72044,#72045,#72046,#72047,#72048,#72049,
#72050,#72051,#72052,#72053,#72054,#72055,#72056,#72057,#72058,#72059,#72060,
#72061,#72062,#72063,#72064,#72065,#72066,#72067,#72068,#72069,#72070,#72071,
#72072,#72073,#72074,#72075,#72076,#72077,#72078,#72079,#72080,#72081,#72082,
#72083,#72084,#72085,#72086,#72087,#72088,#72089,#72090,#72091,#72092,#72093,
#72094,#72095,#72096,#72097,#72098,#72099,#72100,#72101,#72102,#72103,#72104,
#72105,#72106,#72107,#72108,#72109,#72110,#72111,#72112,#72113,#72114),
(#72115,#72116,#72117,#72118,#72119,#72120,#72121,#72122,#72123,#72124,
#72125,#72126,#72127,#72128,#72129,#72130,#72131,#72132,#72133,#72134,#72135,
#72136,#72137,#72138,#72139,#72140,#72141,#72142,#72143,#72144,#72145,#72146,
#72147,#72148,#72149,#72150,#72151,#72152,#72153,#72154,#72155,#72156,#72157,
#72158,#72159,#72160,#72161,#72162,#72163,#72164,#72165,#72166,#72167,#72168,
#72169,#72170,#72171,#72172,#72173,#72174,#72175,#72176,#72177,#72178,#72179,
#72180,#72181,#72182,#72183,#72184,#72185,#72186,#72187,#72188,#72189,#72190,
#72191,#72192,#72193,#72194,#72195,#72196,#72197,#72198,#72199,#72200,#72201,
#72202,#72203,#72204,#72205,#72206,#72207,#72208,#72209,#72210,#72211,#72212,
#72213,#72214,#72215,#72216,#72217,#72218,#72219,#72220,#72221,#72222,#72223,
#72224,#72225,#72226,#72227,#72228,#72229,#72230,#72231,#72232,#72233,#72234,
#72235,#72236,#72237,#72238,#72239,#72240,#72241,#72242,#72243,#72244,#72245,
#72246,#72247,#72248,#72249,#72250,#72251,#72252,#72253,#72254,#72255,#72256,
#72257,#72258,#72259,#72260,#72261,#72262,#72263,#72264,#72265)),
 .UNSPECIFIED.,.F.,.F.,.F.,(4,4),(4,1,1,1,1,1,1,1,1,1,1,1,1,1,1,1,1,1,1,
1,1,1,1,1,1,1,1,1,1,1,1,1,1,1,1,1,1,1,1,1,1,1,1,1,1,1,1,1,1,1,1,1,1,1,1,
1,1,1,1,1,1,1,1,1,1,1,1,1,1,1,1,1,1,1,1,1,1,1,1,1,1,1,1,1,1,1,1,1,1,1,1,
1,1,1,1,1,1,1,1,1,1,1,1,1,1,1,1,1,1,1,1,1,1,1,1,1,1,1,1,1,1,1,1,1,1,1,1,
1,1,1,1,1,1,1,1,1,1,1,1,1,1,1,1,1,1,1,1,1,4),(0.,0.0986691610045069),(11.6147305479243,
12.1142057049618,12.6136808619992,13.6126311760742,14.6115814901491,15.6105318042241,
16.6094821182991,17.608432432374,18.607382746449,19.6063330605239,20.6052833745989,
21.6042336886738,22.6031840027488,23.6021343168238,24.6010846308987,25.6000349449737,
26.5989852590486,27.5979355731236,28.5968858871985,29.5958362012735,30.5947865153485,
31.5937368294234,32.5926871434984,33.5916374575733,34.5905877716483,35.5895380857232,
36.5884883997982,37.5874387138731,38.5863890279481,39.5853393420231,40.584289656098,
41.583239970173,42.5821902842479,43.5811405983229,44.5800909123978,45.5790412264728,
46.5779915405478,47.5769418546227,48.5758921686977,49.5748424827726,50.5737927968476,
51.5727431109225,52.5716934249975,53.5706437390725,54.5695940531474,55.5685443672224,
56.5674946812973,57.5664449953723,58.5653953094472,59.5643456235222,60.5632959375972,
61.5622462516721,62.5611965657471,63.560146879822,64.559097193897,65.5580475079719,
66.5569978220469,67.5559481361219,68.5548984501968,69.5538487642718,70.5527990783467,
71.5517493924217,72.5506997064966,73.5496500205716,74.5486003346466,75.5475506487215,
76.5465009627965,77.5454512768714,78.5444015909464,79.5433519050213,80.5423022190963,
81.5412525331712,82.5402028472462,83.5391531613212,84.5381034753961,85.5370537894711,
86.536004103546,87.534954417621,88.5339047316959,89.5328550457709,90.5318053598459,
91.5307556739208,92.5297059879958,93.5286563020707,94.5276066161457,95.5265569302206,
96.5255072442956,97.5244575583706,98.5234078724455,99.5223581865205,100.521308500595,
101.52025881467,102.519209128745,103.51815944282,104.517109756895,105.51606007097,
106.515010385045,107.51396069912,108.512911013195,109.51186132727,110.510811641345,
111.50976195542,112.508712269495,113.50766258357,114.506612897645,115.50556321172,
116.504513525795,117.50346383987,118.502414153945,119.50136446802,120.500314782095,
121.49926509617,122.498215410244,123.497165724319,124.496116038394,125.495066352469,
126.494016666544,127.492966980619,128.491917294694,129.490867608769,130.489817922844,
131.488768236919,132.487718550994,133.486668865069,134.485619179144,135.484569493219,
136.483519807294,137.482470121369,138.481420435444,139.480370749519,140.479321063594,
141.478271377669,142.477221691744,143.476172005819,144.475122319894,145.474072633968,
146.473022948043,147.471973262118,148.470923576193,149.469873890268,150.468824204343,
151.467774518418,152.466724832493,153.465675146568,154.464625460643,155.463575774718,
156.462526088793,156.96200124583,157.461476402868),.UNSPECIFIED.);
#172=B_SPLINE_SURFACE_WITH_KNOTS('',3,3,((#74631,#74632,#74633,#74634,#74635,
#74636,#74637,#74638,#74639,#74640,#74641,#74642,#74643,#74644,#74645,#74646,
#74647,#74648,#74649,#74650,#74651,#74652,#74653,#74654,#74655,#74656,#74657,
#74658,#74659,#74660,#74661,#74662,#74663,#74664,#74665,#74666,#74667,#74668,
#74669,#74670,#74671,#74672,#74673,#74674,#74675,#74676,#74677,#74678,#74679,
#74680,#74681,#74682,#74683,#74684,#74685,#74686,#74687,#74688,#74689,#74690,
#74691,#74692,#74693,#74694,#74695,#74696,#74697,#74698,#74699,#74700,#74701,
#74702,#74703,#74704,#74705,#74706,#74707,#74708,#74709,#74710,#74711,#74712,
#74713,#74714,#74715,#74716,#74717,#74718,#74719,#74720,#74721,#74722,#74723,
#74724,#74725,#74726,#74727,#74728,#74729,#74730,#74731,#74732,#74733,#74734,
#74735,#74736,#74737,#74738,#74739,#74740,#74741,#74742,#74743,#74744,#74745,
#74746,#74747,#74748,#74749,#74750,#74751,#74752,#74753,#74754,#74755,#74756,
#74757),(#74758,#74759,#74760,#74761,#74762,#74763,#74764,#74765,#74766,
#74767,#74768,#74769,#74770,#74771,#74772,#74773,#74774,#74775,#74776,#74777,
#74778,#74779,#74780,#74781,#74782,#74783,#74784,#74785,#74786,#74787,#74788,
#74789,#74790,#74791,#74792,#74793,#74794,#74795,#74796,#74797,#74798,#74799,
#74800,#74801,#74802,#74803,#74804,#74805,#74806,#74807,#74808,#74809,#74810,
#74811,#74812,#74813,#74814,#74815,#74816,#74817,#74818,#74819,#74820,#74821,
#74822,#74823,#74824,#74825,#74826,#74827,#74828,#74829,#74830,#74831,#74832,
#74833,#74834,#74835,#74836,#74837,#74838,#74839,#74840,#74841,#74842,#74843,
#74844,#74845,#74846,#74847,#74848,#74849,#74850,#74851,#74852,#74853,#74854,
#74855,#74856,#74857,#74858,#74859,#74860,#74861,#74862,#74863,#74864,#74865,
#74866,#74867,#74868,#74869,#74870,#74871,#74872,#74873,#74874,#74875,#74876,
#74877,#74878,#74879,#74880,#74881,#74882,#74883,#74884),(#74885,#74886,
#74887,#74888,#74889,#74890,#74891,#74892,#74893,#74894,#74895,#74896,#74897,
#74898,#74899,#74900,#74901,#74902,#74903,#74904,#74905,#74906,#74907,#74908,
#74909,#74910,#74911,#74912,#74913,#74914,#74915,#74916,#74917,#74918,#74919,
#74920,#74921,#74922,#74923,#74924,#74925,#74926,#74927,#74928,#74929,#74930,
#74931,#74932,#74933,#74934,#74935,#74936,#74937,#74938,#74939,#74940,#74941,
#74942,#74943,#74944,#74945,#74946,#74947,#74948,#74949,#74950,#74951,#74952,
#74953,#74954,#74955,#74956,#74957,#74958,#74959,#74960,#74961,#74962,#74963,
#74964,#74965,#74966,#74967,#74968,#74969,#74970,#74971,#74972,#74973,#74974,
#74975,#74976,#74977,#74978,#74979,#74980,#74981,#74982,#74983,#74984,#74985,
#74986,#74987,#74988,#74989,#74990,#74991,#74992,#74993,#74994,#74995,#74996,
#74997,#74998,#74999,#75000,#75001,#75002,#75003,#75004,#75005,#75006,#75007,
#75008,#75009,#75010,#75011),(#75012,#75013,#75014,#75015,#75016,#75017,
#75018,#75019,#75020,#75021,#75022,#75023,#75024,#75025,#75026,#75027,#75028,
#75029,#75030,#75031,#75032,#75033,#75034,#75035,#75036,#75037,#75038,#75039,
#75040,#75041,#75042,#75043,#75044,#75045,#75046,#75047,#75048,#75049,#75050,
#75051,#75052,#75053,#75054,#75055,#75056,#75057,#75058,#75059,#75060,#75061,
#75062,#75063,#75064,#75065,#75066,#75067,#75068,#75069,#75070,#75071,#75072,
#75073,#75074,#75075,#75076,#75077,#75078,#75079,#75080,#75081,#75082,#75083,
#75084,#75085,#75086,#75087,#75088,#75089,#75090,#75091,#75092,#75093,#75094,
#75095,#75096,#75097,#75098,#75099,#75100,#75101,#75102,#75103,#75104,#75105,
#75106,#75107,#75108,#75109,#75110,#75111,#75112,#75113,#75114,#75115,#75116,
#75117,#75118,#75119,#75120,#75121,#75122,#75123,#75124,#75125,#75126,#75127,
#75128,#75129,#75130,#75131,#75132,#75133,#75134,#75135,#75136,#75137,#75138)),
 .UNSPECIFIED.,.F.,.F.,.F.,(4,4),(4,1,1,1,1,1,1,1,1,1,1,1,1,1,1,1,1,1,1,
1,1,1,1,1,1,1,1,1,1,1,1,1,1,1,1,1,1,1,1,1,1,1,1,1,1,1,1,1,1,1,1,1,1,1,1,
1,1,1,1,1,1,1,1,1,1,1,1,1,1,1,1,1,1,1,1,1,1,1,1,1,1,1,1,1,1,1,1,1,1,1,1,
1,1,1,1,1,1,1,1,1,1,1,1,1,1,1,1,1,1,1,1,1,1,1,1,1,1,1,1,1,1,1,1,1,4),(0.,
0.0658467982010767),(8.30747755240103,9.30251287567468,10.2975481989483,
11.292583522222,12.2876188454956,13.2826541687693,14.2776894920429,15.2727248153166,
16.2677601385902,17.2627954618639,18.2578307851375,19.2528661084112,20.2479014316848,
21.2429367549585,22.2379720782321,23.2330074015058,24.2280427247794,25.2230780480531,
26.2181133713267,27.2131486946004,28.208184017874,29.2032193411477,30.1982546644213,
31.193289987695,32.1883253109686,33.1833606342423,34.1783959575159,35.1734312807896,
36.1684666040632,37.1635019273369,38.1585372506105,39.1535725738842,40.1486078971578,
41.1436432204315,42.1386785437051,43.1337138669788,44.1287491902524,45.1237845135261,
46.1188198367997,47.1138551600734,48.108890483347,49.1039258066207,50.0989611298943,
51.093996453168,52.0890317764416,53.0840670997153,54.0791024229889,55.0741377462626,
56.0691730695362,57.0642083928099,58.0592437160835,59.0542790393572,60.0493143626308,
61.0443496859045,62.0393850091781,63.0344203324518,64.0294556557254,65.0244909789991,
66.0195263022727,67.0145616255464,68.00959694882,69.0046322720937,69.9996675953673,
70.994702918641,71.9897382419146,72.9847735651883,73.9798088884619,74.9748442117356,
75.9698795350092,76.9649148582829,77.9599501815565,78.9549855048302,79.9500208281038,
80.9450561513775,81.9400914746511,82.9351267979248,83.9301621211984,84.9251974444721,
85.9202327677457,86.9152680910194,87.910303414293,88.9053387375667,89.9003740608403,
90.895409384114,91.8904447073876,92.8854800306613,93.8805153539349,94.8755506772086,
95.8705860004822,96.8656213237559,97.8606566470295,98.8556919703032,99.8507272935768,
100.84576261685,101.840797940124,102.835833263398,103.830868586671,104.825903909945,
105.820939233219,106.815974556492,107.811009879766,108.80604520304,109.801080526313,
110.796115849587,111.791151172861,112.786186496134,113.781221819408,114.776257142682,
115.771292465955,116.766327789229,117.761363112503,118.756398435776,119.75143375905,
120.746469082323,121.741504405597,122.736539728871,123.731575052144,124.726610375418,
125.721645698692,126.716681021965,127.711716345239,128.706751668513,129.701786991786,
130.69682231506,131.691857638334),.UNSPECIFIED.);
#173=B_SPLINE_SURFACE_WITH_KNOTS('',3,3,((#75281,#75282,#75283,#75284,#75285,
#75286,#75287,#75288,#75289,#75290,#75291,#75292,#75293,#75294,#75295,#75296,
#75297,#75298,#75299,#75300,#75301,#75302,#75303,#75304,#75305,#75306,#75307,
#75308,#75309,#75310,#75311,#75312,#75313,#75314,#75315,#75316,#75317,#75318,
#75319,#75320,#75321,#75322,#75323,#75324,#75325,#75326,#75327,#75328,#75329,
#75330,#75331,#75332,#75333,#75334,#75335,#75336,#75337,#75338,#75339,#75340,
#75341,#75342,#75343,#75344,#75345,#75346,#75347,#75348,#75349,#75350,#75351,
#75352,#75353,#75354,#75355,#75356,#75357,#75358,#75359,#75360,#75361,#75362,
#75363,#75364,#75365,#75366,#75367,#75368,#75369,#75370,#75371,#75372,#75373,
#75374,#75375,#75376,#75377,#75378,#75379,#75380,#75381,#75382,#75383,#75384,
#75385,#75386,#75387,#75388,#75389,#75390,#75391,#75392,#75393,#75394,#75395,
#75396,#75397,#75398,#75399,#75400,#75401,#75402,#75403,#75404,#75405,#75406,
#75407),(#75408,#75409,#75410,#75411,#75412,#75413,#75414,#75415,#75416,
#75417,#75418,#75419,#75420,#75421,#75422,#75423,#75424,#75425,#75426,#75427,
#75428,#75429,#75430,#75431,#75432,#75433,#75434,#75435,#75436,#75437,#75438,
#75439,#75440,#75441,#75442,#75443,#75444,#75445,#75446,#75447,#75448,#75449,
#75450,#75451,#75452,#75453,#75454,#75455,#75456,#75457,#75458,#75459,#75460,
#75461,#75462,#75463,#75464,#75465,#75466,#75467,#75468,#75469,#75470,#75471,
#75472,#75473,#75474,#75475,#75476,#75477,#75478,#75479,#75480,#75481,#75482,
#75483,#75484,#75485,#75486,#75487,#75488,#75489,#75490,#75491,#75492,#75493,
#75494,#75495,#75496,#75497,#75498,#75499,#75500,#75501,#75502,#75503,#75504,
#75505,#75506,#75507,#75508,#75509,#75510,#75511,#75512,#75513,#75514,#75515,
#75516,#75517,#75518,#75519,#75520,#75521,#75522,#75523,#75524,#75525,#75526,
#75527,#75528,#75529,#75530,#75531,#75532,#75533,#75534),(#75535,#75536,
#75537,#75538,#75539,#75540,#75541,#75542,#75543,#75544,#75545,#75546,#75547,
#75548,#75549,#75550,#75551,#75552,#75553,#75554,#75555,#75556,#75557,#75558,
#75559,#75560,#75561,#75562,#75563,#75564,#75565,#75566,#75567,#75568,#75569,
#75570,#75571,#75572,#75573,#75574,#75575,#75576,#75577,#75578,#75579,#75580,
#75581,#75582,#75583,#75584,#75585,#75586,#75587,#75588,#75589,#75590,#75591,
#75592,#75593,#75594,#75595,#75596,#75597,#75598,#75599,#75600,#75601,#75602,
#75603,#75604,#75605,#75606,#75607,#75608,#75609,#75610,#75611,#75612,#75613,
#75614,#75615,#75616,#75617,#75618,#75619,#75620,#75621,#75622,#75623,#75624,
#75625,#75626,#75627,#75628,#75629,#75630,#75631,#75632,#75633,#75634,#75635,
#75636,#75637,#75638,#75639,#75640,#75641,#75642,#75643,#75644,#75645,#75646,
#75647,#75648,#75649,#75650,#75651,#75652,#75653,#75654,#75655,#75656,#75657,
#75658,#75659,#75660,#75661),(#75662,#75663,#75664,#75665,#75666,#75667,
#75668,#75669,#75670,#75671,#75672,#75673,#75674,#75675,#75676,#75677,#75678,
#75679,#75680,#75681,#75682,#75683,#75684,#75685,#75686,#75687,#75688,#75689,
#75690,#75691,#75692,#75693,#75694,#75695,#75696,#75697,#75698,#75699,#75700,
#75701,#75702,#75703,#75704,#75705,#75706,#75707,#75708,#75709,#75710,#75711,
#75712,#75713,#75714,#75715,#75716,#75717,#75718,#75719,#75720,#75721,#75722,
#75723,#75724,#75725,#75726,#75727,#75728,#75729,#75730,#75731,#75732,#75733,
#75734,#75735,#75736,#75737,#75738,#75739,#75740,#75741,#75742,#75743,#75744,
#75745,#75746,#75747,#75748,#75749,#75750,#75751,#75752,#75753,#75754,#75755,
#75756,#75757,#75758,#75759,#75760,#75761,#75762,#75763,#75764,#75765,#75766,
#75767,#75768,#75769,#75770,#75771,#75772,#75773,#75774,#75775,#75776,#75777,
#75778,#75779,#75780,#75781,#75782,#75783,#75784,#75785,#75786,#75787,#75788)),
 .UNSPECIFIED.,.F.,.F.,.F.,(4,4),(4,1,1,1,1,1,1,1,1,1,1,1,1,1,1,1,1,1,1,
1,1,1,1,1,1,1,1,1,1,1,1,1,1,1,1,1,1,1,1,1,1,1,1,1,1,1,1,1,1,1,1,1,1,1,1,
1,1,1,1,1,1,1,1,1,1,1,1,1,1,1,1,1,1,1,1,1,1,1,1,1,1,1,1,1,1,1,1,1,1,1,1,
1,1,1,1,1,1,1,1,1,1,1,1,1,1,1,1,1,1,1,1,1,1,1,1,1,1,1,1,1,1,1,1,1,4),(0.,
0.0658467982010767),(11.6150328478182,12.6100681710919,13.6051034943655,
14.6001388176392,15.5951741409128,16.5902094641865,17.5852447874601,18.5802801107338,
19.5753154340074,20.5703507572811,21.5653860805547,22.5604214038284,23.555456727102,
24.5504920503757,25.5455273736493,26.540562696923,27.5355980201966,28.5306333434703,
29.5256686667439,30.5207039900176,31.5157393132912,32.5107746365649,33.5058099598385,
34.5008452831122,35.4958806063858,36.4909159296595,37.4859512529331,38.4809865762068,
39.4760218994804,40.4710572227541,41.4660925460277,42.4611278693014,43.456163192575,
44.4511985158487,45.4462338391223,46.441269162396,47.4363044856696,48.4313398089433,
49.4263751322169,50.4214104554906,51.4164457787642,52.4114811020379,53.4065164253115,
54.4015517485852,55.3965870718588,56.3916223951325,57.3866577184061,58.3816930416798,
59.3767283649534,60.3717636882271,61.3667990115007,62.3618343347744,63.356869658048,
64.3519049813217,65.3469403045953,66.341975627869,67.3370109511426,68.3320462744163,
69.3270815976899,70.3221169209636,71.3171522442372,72.3121875675109,73.3072228907845,
74.3022582140582,75.2972935373318,76.2923288606055,77.2873641838791,78.2823995071528,
79.2774348304264,80.2724701537001,81.2675054769737,82.2625408002474,83.257576123521,
84.2526114467947,85.2476467700683,86.242682093342,87.2377174166156,88.2327527398893,
89.2277880631629,90.2228233864366,91.2178587097102,92.2128940329839,93.2079293562575,
94.2029646795312,95.1980000028048,96.1930353260785,97.1880706493521,98.1831059726258,
99.1781412958994,100.173176619173,101.168211942447,102.16324726572,103.158282588994,
104.153317912268,105.148353235541,106.143388558815,107.138423882089,108.133459205362,
109.128494528636,110.12352985191,111.118565175183,112.113600498457,113.108635821731,
114.103671145004,115.098706468278,116.093741791551,117.088777114825,118.083812438099,
119.078847761372,120.073883084646,121.06891840792,122.063953731193,123.058989054467,
124.054024377741,125.049059701014,126.044095024288,127.039130347562,128.034165670835,
129.029200994109,130.024236317383,131.019271640656,132.01430696393,133.009342287204,
134.004377610477,134.999412933751),.UNSPECIFIED.);
#174=B_SPLINE_CURVE_WITH_KNOTS('',3,(#37067,#37068,#37069,#37070,#37071,
#37072,#37073,#37074,#37075,#37076,#37077,#37078,#37079,#37080,#37081,#37082,
#37083,#37084),.UNSPECIFIED.,.F.,.F.,(4,2,2,2,2,2,2,2,4),(0.,0.341830025609023,
0.683660051218047,1.02549007682707,1.36732010243609,1.7090034027405,2.05068670304491,
2.39237000334931,2.73405330365372),.UNSPECIFIED.);
#175=B_SPLINE_CURVE_WITH_KNOTS('',3,(#37085,#37086,#37087,#37088,#37089,
#37090,#37091,#37092,#37093,#37094,#37095,#37096,#37097,#37098,#37099,#37100,
#37101,#37102,#37103,#37104,#37105,#37106,#37107,#37108,#37109,#37110,#37111,
#37112,#37113,#37114,#37115,#37116,#37117,#37118,#37119,#37120,#37121,#37122,
#37123,#37124,#37125,#37126,#37127,#37128,#37129,#37130,#37131,#37132,#37133,
#37134),.UNSPECIFIED.,.F.,.F.,(4,2,2,2,2,2,2,2,2,2,2,2,2,2,2,2,2,2,2,2,
2,2,2,2,4),(2.73405330365372,3.07573660395812,3.41741990426253,3.75910320456694,
4.10078650487134,4.44261653048037,4.78444655608939,5.12627658169841,5.46810660730744,
5.80993663291646,6.15176665852548,6.49359668413451,6.83542670974353,7.17711001004794,
7.51879331035234,7.86047661065675,8.20215991096115,8.54384321126556,8.88552651156997,
9.22720981187437,9.56889311217878,9.9107231377878,10.2525531633968,10.5943831890058,
10.9362132146149),.UNSPECIFIED.);
#176=B_SPLINE_CURVE_WITH_KNOTS('',3,(#37138,#37139,#37140,#37141,#37142,
#37143),.UNSPECIFIED.,.F.,.F.,(4,2,4),(1.71566353344894,1.90989804259815,
2.10413255174736),.UNSPECIFIED.);
#177=B_SPLINE_CURVE_WITH_KNOTS('',3,(#37163,#37164,#37165,#37166,#37167,
#37168),.UNSPECIFIED.,.F.,.F.,(4,2,4),(1.71566348905116,1.90989799807537,
2.10413250709959),.UNSPECIFIED.);
#178=B_SPLINE_CURVE_WITH_KNOTS('',3,(#37172,#37173,#37174,#37175,#37176,
#37177),.UNSPECIFIED.,.F.,.F.,(4,2,4),(1.71529227392093,1.90952573777923,
2.10375920163752),.UNSPECIFIED.);
#179=B_SPLINE_CURVE_WITH_KNOTS('',3,(#37181,#37182,#37183,#37184,#37185,
#37186),.UNSPECIFIED.,.F.,.F.,(4,2,4),(1.7156635334436,1.90989804259278,
2.10413255174196),.UNSPECIFIED.);
#180=B_SPLINE_CURVE_WITH_KNOTS('',3,(#37222,#37223,#37224,#37225),
 .UNSPECIFIED.,.F.,.F.,(4,4),(-1.87779361595245,-1.82480525135948),
 .UNSPECIFIED.);
#181=B_SPLINE_CURVE_WITH_KNOTS('',3,(#37229,#37230,#37231,#37232),
 .UNSPECIFIED.,.F.,.F.,(4,4),(-0.838159967188763,-0.78517160259578),
 .UNSPECIFIED.);
#182=B_SPLINE_CURVE_WITH_KNOTS('',3,(#37473,#37474,#37475,#37476,#37477,
#37478,#37479,#37480,#37481,#37482,#37483,#37484,#37485,#37486,#37487,#37488,
#37489,#37490,#37491,#37492,#37493,#37494,#37495,#37496,#37497,#37498,#37499,
#37500,#37501,#37502,#37503,#37504,#37505,#37506,#37507,#37508,#37509,#37510),
 .UNSPECIFIED.,.F.,.F.,(4,1,1,1,1,1,1,1,1,1,1,1,1,1,1,1,1,1,1,1,1,1,1,1,
1,1,1,1,1,1,1,1,1,1,1,4),(0.,0.301700924572155,0.452551386858232,0.60340184914431,
0.62225815693007,0.641114464715829,0.678827080287349,0.716539695858868,
0.754252311430387,0.829677542573426,0.867390158144946,0.905102773716465,
1.20680369828862,1.23194544200297,1.25708718571731,1.307370673146,1.40793764800339,
1.81020554743293,1.83534729114728,1.86048903486162,1.91077252229031,2.0113394971477,
2.21247344686247,2.26275693429116,2.41360739657724,2.56445785886332,2.71530832114939,
2.86615878343547,2.94158401457851,2.96044032236427,2.97929663015003,2.99815293793579,
3.00758109182867,3.01229516877511,3.01700924572155,3.16785970800763),
 .UNSPECIFIED.);
#183=B_SPLINE_CURVE_WITH_KNOTS('',3,(#37511,#37512,#37513,#37514,#37515,
#37516,#37517,#37518,#37519,#37520,#37521,#37522,#37523,#37524),
 .UNSPECIFIED.,.F.,.F.,(4,1,1,1,1,1,1,1,1,1,1,4),(3.16785970800763,3.3187101702937,
3.35642278586522,3.39413540143674,3.46956063257978,3.54498586372282,3.58269847929434,
3.6015547870801,3.62041109486586,3.77126155715194,3.92211201943801,4.22381294401017),
 .UNSPECIFIED.);
#184=B_SPLINE_CURVE_WITH_KNOTS('',3,(#37525,#37526,#37527,#37528,#37529,
#37530,#37531,#37532,#37533,#37534,#37535,#37536,#37537,#37538,#37539,#37540,
#37541,#37542,#37543,#37544,#37545,#37546,#37547,#37548,#37549,#37550,#37551,
#37552,#37553,#37554,#37555,#37556,#37557,#37558,#37559,#37560,#37561,#37562,
#37563,#37564,#37565,#37566,#37567,#37568,#37569,#37570,#37571,#37572),
 .UNSPECIFIED.,.T.,.F.,(4,1,1,1,1,1,1,1,1,1,1,1,1,1,1,1,1,1,1,1,1,1,1,1,
1,1,1,1,1,1,1,1,1,1,1,1,1,1,1,1,1,1,1,1,1,4),(-4.22381294401017,-3.92211201943801,
-3.77126155715194,-3.62041109486586,-3.6015547870801,-3.58269847929434,
-3.54498586372282,-3.46956063257978,-3.39413540143674,-3.35642278586522,
-3.3187101702937,-3.01700924572155,-3.01229516877511,-3.00758109182867,
-2.99815293793579,-2.97929663015003,-2.96044032236427,-2.94158401457851,
-2.86615878343547,-2.71530832114939,-2.56445785886332,-2.41360739657724,
-2.26275693429116,-2.21247344686247,-2.0113394971477,-1.91077252229031,
-1.86048903486162,-1.83534729114728,-1.81020554743293,-1.40793764800339,
-1.307370673146,-1.25708718571731,-1.23194544200297,-1.20680369828862,-0.905102773716465,
-0.867390158144946,-0.829677542573426,-0.754252311430387,-0.716539695858868,
-0.678827080287349,-0.641114464715829,-0.62225815693007,-0.60340184914431,
-0.452551386858232,-0.301700924572155,0.),.UNSPECIFIED.);
#185=B_SPLINE_CURVE_WITH_KNOTS('',3,(#37583,#37584,#37585,#37586,#37587,
#37588,#37589),.UNSPECIFIED.,.F.,.F.,(4,3,4),(0.,0.0706076080518625,0.140717785645037),
 .UNSPECIFIED.);
#186=B_SPLINE_CURVE_WITH_KNOTS('',3,(#37591,#37592,#37593,#37594,#37595,
#37596,#37597,#37598,#37599,#37600,#37601,#37602,#37603,#37604,#37605,#37606,
#37607,#37608,#37609,#37610,#37611,#37612,#37613,#37614,#37615,#37616,#37617),
 .UNSPECIFIED.,.F.,.F.,(4,2,2,2,2,2,3,2,2,2,2,2,4),(-4.20812861828807,-3.99425066999856,
-3.16073871853832,-2.37055403890373,-1.58036935926916,-0.790184679634578,
0.,0.79018467963458,1.58036935926916,2.37055403890374,3.16073871853832,
3.99425066999856,4.20812861828807),.UNSPECIFIED.);
#187=B_SPLINE_CURVE_WITH_KNOTS('',3,(#37619,#37620,#37621,#37622,#37623,
#37624,#37625),.UNSPECIFIED.,.F.,.F.,(4,3,4),(0.,0.0701050024887815,0.140717775218191),
 .UNSPECIFIED.);
#188=B_SPLINE_CURVE_WITH_KNOTS('',3,(#37629,#37630,#37631,#37632,#37633,
#37634,#37635,#37636,#37637,#37638),.UNSPECIFIED.,.F.,.F.,(4,2,2,2,4),(0.,
0.120853732558559,0.299961593709033,0.490853831409324,0.492261507196457),
 .UNSPECIFIED.);
#189=B_SPLINE_CURVE_WITH_KNOTS('',3,(#37641,#37642,#37643,#37644,#37645,
#37646,#37647,#37648,#37649,#37650),.UNSPECIFIED.,.F.,.F.,(4,2,2,2,4),(-0.00109523829507863,
0.,0.141893095426123,0.28665904951154,0.476004129030812),.UNSPECIFIED.);
#190=B_SPLINE_CURVE_WITH_KNOTS('',3,(#37712,#37713,#37714,#37715,#37716,
#37717,#37718,#37719,#37720,#37721,#37722,#37723,#37724,#37725,#37726,#37727,
#37728,#37729,#37730,#37731,#37732,#37733,#37734,#37735,#37736,#37737,#37738,
#37739,#37740,#37741,#37742,#37743,#37744,#37745,#37746,#37747,#37748,#37749,
#37750,#37751),.UNSPECIFIED.,.F.,.F.,(4,3,3,3,3,3,3,3,3,3,3,3,3,4),(0.,
0.0642058267314402,0.135298039610793,0.216720613163576,0.322214526794598,
0.406937710945273,0.476869411739625,0.550300205763178,0.627974002306146,
0.731399879303705,0.815726896068677,0.88866362574166,0.953773893187292,
1.),.UNSPECIFIED.);
#191=B_SPLINE_CURVE_WITH_KNOTS('',3,(#37753,#37754,#37755,#37756),
 .UNSPECIFIED.,.F.,.F.,(4,4),(0.,1.),.UNSPECIFIED.);
#192=B_SPLINE_CURVE_WITH_KNOTS('',3,(#37758,#37759,#37760,#37761,#37762,
#37763,#37764,#37765,#37766,#37767,#37768,#37769,#37770,#37771,#37772,#37773,
#37774,#37775,#37776,#37777,#37778,#37779,#37780,#37781,#37782,#37783,#37784,
#37785,#37786,#37787,#37788,#37789,#37790,#37791,#37792,#37793,#37794,#37795,
#37796,#37797,#37798,#37799,#37800,#37801,#37802,#37803,#37804,#37805,#37806,
#37807,#37808,#37809),.UNSPECIFIED.,.F.,.F.,(4,3,3,3,3,3,3,3,3,3,3,3,3,
3,3,3,3,4),(0.,0.0470013637169586,0.0964181016740628,0.149229530335118,
0.208169836206556,0.286934368114381,0.357340819180099,0.414362060111408,
0.466217667030896,0.532940458652034,0.585846875133388,0.644811876239638,
0.72711087277581,0.795333154581857,0.850882587463839,0.902663377962928,
0.951331688981464,1.),.UNSPECIFIED.);
#193=B_SPLINE_CURVE_WITH_KNOTS('',3,(#37845,#37846,#37847,#37848,#37849,
#37850,#37851,#37852,#37853,#37854,#37855,#37856,#37857,#37858,#37859,#37860,
#37861,#37862,#37863,#37864,#37865,#37866,#37867,#37868,#37869,#37870,#37871,
#37872,#37873,#37874,#37875,#37876,#37877,#37878,#37879,#37880,#37881,#37882,
#37883,#37884,#37885,#37886,#37887,#37888,#37889,#37890,#37891,#37892,#37893,
#37894,#37895,#37896),.UNSPECIFIED.,.F.,.F.,(4,3,3,3,3,3,3,3,3,3,3,3,3,
3,3,3,3,4),(0.,0.0469954003122149,0.0964054107400102,0.149208793967372,
0.208136804390094,0.286850662832856,0.357279255948468,0.414301991680454,
0.466156507957792,0.532886944463068,0.585793820692173,0.644755325044784,
0.727049300721868,0.795286975541401,0.85084796357777,0.9026376409811,0.95131882049055,
1.),.UNSPECIFIED.);
#194=B_SPLINE_CURVE_WITH_KNOTS('',3,(#37898,#37899,#37900,#37901),
 .UNSPECIFIED.,.F.,.F.,(4,4),(-1.,0.),.UNSPECIFIED.);
#195=B_SPLINE_CURVE_WITH_KNOTS('',3,(#37903,#37904,#37905,#37906,#37907,
#37908,#37909,#37910,#37911,#37912,#37913,#37914,#37915,#37916,#37917,#37918,
#37919,#37920,#37921,#37922,#37923,#37924,#37925,#37926,#37927,#37928,#37929,
#37930,#37931,#37932,#37933,#37934,#37935,#37936,#37937,#37938,#37939,#37940,
#37941,#37942),.UNSPECIFIED.,.F.,.F.,(4,3,3,3,3,3,3,3,3,3,3,3,3,4),(0.,
0.0642045803508197,0.135295214744166,0.216715461741643,0.322211745001425,
0.406935276876247,0.476866299954066,0.550298370624421,0.62797200200528,
0.73139484549015,0.815724459936111,0.888662483366991,0.953773603714735,
1.),.UNSPECIFIED.);
#196=B_SPLINE_CURVE_WITH_KNOTS('',3,(#37964,#37965,#37966,#37967,#37968),
 .UNSPECIFIED.,.F.,.F.,(4,1,4),(-2.66286532859155,-2.32640602317479,-1.87779361595245),
 .UNSPECIFIED.);
#197=B_SPLINE_CURVE_WITH_KNOTS('',3,(#37971,#37972,#37973,#37974,#37975),
 .UNSPECIFIED.,.F.,.F.,(4,1,4),(1.87779361595245,2.32640602317479,2.66286532859155),
 .UNSPECIFIED.);
#198=B_SPLINE_CURVE_WITH_KNOTS('',3,(#38074,#38075,#38076,#38077),
 .UNSPECIFIED.,.F.,.F.,(4,4),(1.82480525135948,1.87779361595245),
 .UNSPECIFIED.);
#199=B_SPLINE_CURVE_WITH_KNOTS('',3,(#38099,#38100,#38101,#38102,#38103),
 .UNSPECIFIED.,.F.,.F.,(4,1,4),(0.000100035134689748,0.3365592783323,0.78517160259578),
 .UNSPECIFIED.);
#200=B_SPLINE_CURVE_WITH_KNOTS('',3,(#38105,#38106,#38107,#38108,#38109),
 .UNSPECIFIED.,.F.,.F.,(4,1,4),(-0.78517160259578,-0.3365592783323,-0.000100035134689748),
 .UNSPECIFIED.);
#201=B_SPLINE_CURVE_WITH_KNOTS('',3,(#38126,#38127,#38128,#38129),
 .UNSPECIFIED.,.F.,.F.,(4,4),(0.78517160259578,0.838159967188763),
 .UNSPECIFIED.);
#202=B_SPLINE_CURVE_WITH_KNOTS('',3,(#38140,#38141,#38142,#38143,#38144,
#38145,#38146,#38147,#38148,#38149,#38150,#38151,#38152,#38153,#38154,#38155,
#38156,#38157,#38158,#38159,#38160,#38161,#38162,#38163,#38164,#38165,#38166,
#38167,#38168,#38169,#38170,#38171,#38172,#38173,#38174,#38175,#38176,#38177,
#38178,#38179),.UNSPECIFIED.,.F.,.F.,(4,3,3,3,3,3,3,3,3,3,3,3,3,4),(0.,
0.0642049615968745,0.13529611806662,0.216717311062181,0.322210830481009,
0.406934476670883,0.476865564838168,0.550296903893395,0.627969426873969,
0.73138741425766,0.815717741324156,0.888655709551853,0.95376643384809,1.),
 .UNSPECIFIED.);
#203=B_SPLINE_CURVE_WITH_KNOTS('',3,(#38181,#38182,#38183,#38184,#38185,
#38186,#38187,#38188,#38189,#38190),.UNSPECIFIED.,.F.,.F.,(4,2,1,1,2,4),
(1.90304005106469,2.0340806772701,2.19643291178007,2.27760902903505,2.43996126354502,
2.66286552223545),.UNSPECIFIED.);
#204=B_SPLINE_CURVE_WITH_KNOTS('',3,(#38192,#38193,#38194,#38195),
 .UNSPECIFIED.,.F.,.F.,(4,4),(1.85120404599841,1.90304005106469),
 .UNSPECIFIED.);
#205=B_SPLINE_CURVE_WITH_KNOTS('',3,(#38397,#38398,#38399,#38400),
 .UNSPECIFIED.,.F.,.F.,(4,4),(-1.90304005106469,-1.85120404599841),
 .UNSPECIFIED.);
#206=B_SPLINE_CURVE_WITH_KNOTS('',3,(#38423,#38424,#38425,#38426),
 .UNSPECIFIED.,.F.,.F.,(4,4),(-0.811761172549836,-0.759925167483548),
 .UNSPECIFIED.);
#207=B_SPLINE_CURVE_WITH_KNOTS('',3,(#38536,#38537,#38538,#38539,#38540,
#38541,#38542,#38543,#38544,#38545,#38546,#38547,#38548,#38549,#38550,#38551,
#38552,#38553,#38554,#38555,#38556,#38557,#38558,#38559,#38560,#38561,#38562,
#38563,#38564,#38565,#38566,#38567,#38568,#38569,#38570,#38571,#38572,#38573,
#38574,#38575,#38576,#38577,#38578,#38579,#38580,#38581,#38582,#38583,#38584,
#38585,#38586,#38587),.UNSPECIFIED.,.F.,.F.,(4,3,3,3,3,3,3,3,3,3,3,3,3,
3,3,3,3,4),(0.,0.0469948696945841,0.0964043092295198,0.149207058425544,
0.208134234796173,0.28684591375033,0.357274586919083,0.414296923289968,
0.466151007737128,0.532882131769987,0.585788839820251,0.644749528487852,
0.727041946185393,0.795281459639045,0.850844102970669,0.902635002958616,
0.951317501479308,1.),.UNSPECIFIED.);
#208=B_SPLINE_CURVE_WITH_KNOTS('',3,(#38588,#38589,#38590,#38591),
 .UNSPECIFIED.,.F.,.F.,(4,4),(-1.,0.),.UNSPECIFIED.);
#209=B_SPLINE_CURVE_WITH_KNOTS('',3,(#38625,#38626,#38627,#38628,#38629,
#38630,#38631,#38632,#38633,#38634,#38635,#38636,#38637,#38638,#38639,#38640,
#38641,#38642,#38643,#38644,#38645,#38646,#38647,#38648,#38649,#38650,#38651,
#38652,#38653,#38654,#38655,#38656,#38657,#38658,#38659,#38660,#38661,#38662,
#38663,#38664),.UNSPECIFIED.,.F.,.F.,(4,3,3,3,3,3,3,3,3,3,3,3,3,4),(0.,
0.0642044939750475,0.135295066626768,0.216715381562263,0.322209970902435,
0.406933724539631,0.476864590196812,0.550296651109942,0.627969500567193,
0.731388236611723,0.815719035368179,0.888657375631424,0.953768460302656,
1.),.UNSPECIFIED.);
#210=B_SPLINE_CURVE_WITH_KNOTS('',3,(#38666,#38667,#38668,#38669),
 .UNSPECIFIED.,.F.,.F.,(4,4),(0.,1.),.UNSPECIFIED.);
#211=B_SPLINE_CURVE_WITH_KNOTS('',3,(#38670,#38671,#38672,#38673,#38674,
#38675,#38676,#38677,#38678,#38679,#38680,#38681,#38682,#38683,#38684,#38685,
#38686,#38687,#38688,#38689,#38690,#38691,#38692,#38693,#38694,#38695,#38696,
#38697,#38698,#38699,#38700,#38701,#38702,#38703,#38704,#38705,#38706,#38707,
#38708,#38709,#38710,#38711,#38712,#38713,#38714,#38715,#38716,#38717,#38718,
#38719,#38720,#38721),.UNSPECIFIED.,.F.,.F.,(4,3,3,3,3,3,3,3,3,3,3,3,3,
3,3,3,3,4),(0.,0.0470027094723439,0.0964210394547843,0.149234501608351,
0.208178283267004,0.286960064846777,0.357356255023185,0.414375729071717,
0.466230636148304,0.532951806629766,0.585857475727138,0.644822009403465,
0.727120616369207,0.795340462276906,0.850888128017495,0.90266743730169,
0.951333718650845,1.),.UNSPECIFIED.);
#212=B_SPLINE_CURVE_WITH_KNOTS('',3,(#38751,#38752,#38753,#38754,#38755,
#38756,#38757),.UNSPECIFIED.,.F.,.F.,(4,1,1,1,4),(9.97415695384386E-5,0.217192720402113,
0.325739209818401,0.542832188650975,0.75992516748355),.UNSPECIFIED.);
#213=B_SPLINE_CURVE_WITH_KNOTS('',3,(#38759,#38760,#38761,#38762,#38763,
#38764,#38765),.UNSPECIFIED.,.F.,.F.,(4,1,1,1,4),(-0.75992516748355,-0.542832188650975,
-0.325739209818401,-0.217192720402113,-9.97415695384386E-5),
 .UNSPECIFIED.);
#214=B_SPLINE_CURVE_WITH_KNOTS('',3,(#38807,#38808,#38809,#38810),
 .UNSPECIFIED.,.F.,.F.,(4,4),(0.759925167483548,0.811761172549836),
 .UNSPECIFIED.);
#215=B_SPLINE_CURVE_WITH_KNOTS('',3,(#38851,#38852,#38853,#38854,#38855,
#38856,#38857,#38858,#38859,#38860),.UNSPECIFIED.,.F.,.F.,(4,2,1,1,2,4),
(-2.66286552223545,-2.43996126354502,-2.27760902903505,-2.19643291178007,
-2.0340806772701,-1.90304005106469),.UNSPECIFIED.);
#216=B_SPLINE_CURVE_WITH_KNOTS('',3,(#38893,#38894,#38895,#38896),
 .UNSPECIFIED.,.F.,.F.,(4,4),(0.,0.0707569587600326),.UNSPECIFIED.);
#217=B_SPLINE_CURVE_WITH_KNOTS('',3,(#38987,#38988,#38989,#38990,#38991,
#38992,#38993,#38994,#38995,#38996,#38997,#38998,#38999,#39000,#39001,#39002,
#39003,#39004,#39005,#39006),.UNSPECIFIED.,.F.,.F.,(4,1,1,1,1,1,1,1,1,1,
1,1,1,1,1,1,1,4),(6.93617595249389,7.96866100733354,9.0011460621732,10.0336311170129,
10.5498736444327,11.0661161718525,12.0986012266922,13.1310862815318,13.8194096514249,
14.507733021318,15.1960563912111,16.5727031309973,17.2610265008905,17.7772690283103,
18.2935115557301,19.3259966105698,20.3584816654094,21.3909667202491),
 .UNSPECIFIED.);
#218=B_SPLINE_CURVE_WITH_KNOTS('',3,(#39009,#39010,#39011,#39012,#39013,
#39014,#39015,#39016,#39017,#39018,#39019,#39020,#39021,#39022,#39023,#39024,
#39025,#39026,#39027,#39028),.UNSPECIFIED.,.F.,.F.,(4,1,1,1,1,1,1,1,1,1,
1,1,1,1,1,1,1,4),(-21.3909667202491,-20.3584816654094,-19.3259966105698,
-18.2935115557301,-17.7772690283103,-17.2610265008905,-16.5727031309973,
-15.1960563912111,-14.507733021318,-13.8194096514249,-13.1310862815318,
-12.0986012266922,-11.0661161718525,-10.5498736444327,-10.0336311170129,
-9.0011460621732,-7.96866100733354,-6.93617595249389),.UNSPECIFIED.);
#219=B_SPLINE_CURVE_WITH_KNOTS('',3,(#39045,#39046,#39047,#39048),
 .UNSPECIFIED.,.F.,.F.,(4,4),(-6.93617595249389,-6.91671820418794),
 .UNSPECIFIED.);
#220=B_SPLINE_CURVE_WITH_KNOTS('',3,(#39049,#39050,#39051,#39052),
 .UNSPECIFIED.,.F.,.F.,(4,4),(6.91671820418794,6.93617595249389),
 .UNSPECIFIED.);
#221=B_SPLINE_CURVE_WITH_KNOTS('',3,(#39069,#39070,#39071,#39072),
 .UNSPECIFIED.,.F.,.F.,(4,4),(-21.410424468555,-21.3909667202491),
 .UNSPECIFIED.);
#222=B_SPLINE_CURVE_WITH_KNOTS('',3,(#39073,#39074,#39075,#39076),
 .UNSPECIFIED.,.F.,.F.,(4,4),(21.3909667202491,21.410424468555),
 .UNSPECIFIED.);
#223=B_SPLINE_CURVE_WITH_KNOTS('',3,(#39093,#39094,#39095,#39096,#39097,
#39098,#39099),.UNSPECIFIED.,.F.,.F.,(4,3,4),(-0.0722630748993823,-0.0361526280409953,
0.),.UNSPECIFIED.);
#224=B_SPLINE_CURVE_WITH_KNOTS('',3,(#39129,#39130,#39131,#39132,#39133,
#39134,#39135),.UNSPECIFIED.,.F.,.F.,(4,1,1,1,4),(-1.46843716746911,-1.23331881650262,
-0.998200465536129,-0.821861702311259,-0.645522939086389),.UNSPECIFIED.);
#225=B_SPLINE_CURVE_WITH_KNOTS('',3,(#39136,#39137,#39138,#39139,#39140,
#39141,#39142),.UNSPECIFIED.,.F.,.F.,(4,1,1,1,4),(0.651509071335782,0.821861702311259,
0.998200465536129,1.23331881650262,1.46789448307402),.UNSPECIFIED.);
#226=B_SPLINE_CURVE_WITH_KNOTS('',3,(#39147,#39148,#39149,#39150,#39151,
#39152,#39153),.UNSPECIFIED.,.F.,.F.,(4,1,1,1,4),(-1.46789448307312,-1.29209840424425,
-1.11575964101938,-0.880641290052883,-0.651509067467386),.UNSPECIFIED.);
#227=B_SPLINE_CURVE_WITH_KNOTS('',3,(#39158,#39159,#39160,#39161,#39162,
#39163,#39164),.UNSPECIFIED.,.F.,.F.,(4,3,4),(-0.0724895287827058,-0.0362236180763736,
0.),.UNSPECIFIED.);
#228=B_SPLINE_CURVE_WITH_KNOTS('',3,(#39193,#39194,#39195,#39196,#39197,
#39198,#39199),.UNSPECIFIED.,.F.,.F.,(4,1,1,1,4),(0.645522939086389,0.880641290052883,
1.11575964101938,1.29209840424425,1.46843716746912),.UNSPECIFIED.);
#229=B_SPLINE_CURVE_WITH_KNOTS('',3,(#39202,#39203,#39204,#39205,#39206),
 .UNSPECIFIED.,.F.,.F.,(4,1,4),(3.93038111840777,4.35323723299001,4.44759047801891),
 .UNSPECIFIED.);
#230=B_SPLINE_CURVE_WITH_KNOTS('',3,(#39241,#39242,#39243,#39244,#39245,
#39246,#39247,#39248,#39249,#39250,#39251,#39252,#39253,#39254,#39255,#39256,
#39257,#39258,#39259,#39260,#39261,#39262,#39263,#39264,#39265,#39266,#39267,
#39268),.UNSPECIFIED.,.F.,.F.,(4,3,3,3,3,3,3,3,3,4),(-4.91704538576632,
-4.77089990935868,-4.70272379532275,-4.63510958231822,-4.4904291378749,
-4.46686475597115,-4.35321853983198,-4.20436404417231,-4.01903755304543,
-3.93038111840777),.UNSPECIFIED.);
#231=B_SPLINE_CURVE_WITH_KNOTS('',3,(#39301,#39302,#39303,#39304,#39305,
#39306),.UNSPECIFIED.,.F.,.F.,(4,1,1,4),(-1.30436309345028,-0.740554939421754,
-0.599602900914624,-0.317698823900363),.UNSPECIFIED.);
#232=B_SPLINE_CURVE_WITH_KNOTS('',3,(#39307,#39308,#39309,#39310),
 .UNSPECIFIED.,.F.,.F.,(4,4),(0.787258846493104,1.30436309345028),
 .UNSPECIFIED.);
#233=B_SPLINE_CURVE_WITH_KNOTS('',3,(#39348,#39349,#39350,#39351,#39352,
#39353,#39354,#39355,#39356,#39357),.UNSPECIFIED.,.F.,.F.,(4,2,2,2,4),(0.,
0.1527055005571,0.3054110011142,0.458115566811898,0.610820132509595),
 .UNSPECIFIED.);
#234=B_SPLINE_CURVE_WITH_KNOTS('',3,(#39358,#39359,#39360,#39361,#39362,
#39363,#39364,#39365,#39366,#39367,#39368,#39369,#39370,#39371,#39372,#39373,
#39374,#39375,#39376,#39377,#39378,#39379,#39380,#39381,#39382,#39383),
 .UNSPECIFIED.,.F.,.F.,(4,2,2,2,2,2,2,2,2,2,2,2,4),(0.610820132509595,0.763524698207293,
0.916229263904991,1.06893476446209,1.22164026501919,1.37434576557629,1.52705126613339,
1.67975583183109,1.83246039752879,1.98516496322648,2.13786952892418,2.29057502948128,
2.44328053003838),.UNSPECIFIED.);
#235=B_SPLINE_CURVE_WITH_KNOTS('',3,(#39387,#39388,#39389,#39390,#39391,
#39392,#39393,#39394,#39395,#39396,#39397,#39398,#39399,#39400,#39401,#39402,
#39403,#39404,#39405,#39406,#39407,#39408,#39409,#39410,#39411,#39412),
 .UNSPECIFIED.,.F.,.F.,(4,2,2,2,2,2,2,2,2,2,2,2,4),(0.,0.380941401599584,
0.761882803199167,1.14272967212036,1.52357654104155,1.90442340996273,2.28527027888392,
2.66621168048351,3.04715308208309,3.42809448368267,3.80903588528226,4.18988275420345,
4.57072962312464),.UNSPECIFIED.);
#236=B_SPLINE_CURVE_WITH_KNOTS('',3,(#39413,#39414,#39415,#39416,#39417,
#39418,#39419,#39420,#39421,#39422),.UNSPECIFIED.,.F.,.F.,(4,2,2,2,4),(4.57072962312464,
4.95157649204583,5.33242336096701,5.7133647625666,6.09430616416618),
 .UNSPECIFIED.);
#237=B_SPLINE_CURVE_WITH_KNOTS('',3,(#39988,#39989,#39990,#39991,#39992,
#39993,#39994,#39995,#39996,#39997,#39998,#39999,#40000,#40001,#40002,#40003,
#40004,#40005),.UNSPECIFIED.,.F.,.F.,(4,2,2,2,2,2,2,2,4),(0.,0.113065755992561,
0.226131511985123,0.3391970600484,0.452262608111676,0.565328156174953,0.67839370423823,
0.791459460230791,0.904525216223353),.UNSPECIFIED.);
#238=B_SPLINE_CURVE_WITH_KNOTS('',3,(#40016,#40017,#40018,#40019,#40020,
#40021,#40022,#40023,#40024,#40025,#40026,#40027,#40028,#40029,#40030,#40031,
#40032,#40033),.UNSPECIFIED.,.F.,.F.,(4,2,2,2,2,2,2,2,4),(-0.904525216223347,
-0.791459460230787,-0.678393704238228,-0.565328156174951,-0.452262608111673,
-0.339197060048396,-0.226131511985119,-0.11306575599256,0.),
 .UNSPECIFIED.);
#239=B_SPLINE_CURVE_WITH_KNOTS('',3,(#40100,#40101,#40102,#40103,#40104,
#40105,#40106,#40107,#40108,#40109,#40110,#40111,#40112,#40113,#40114,#40115,
#40116,#40117,#40118,#40119,#40120,#40121),.UNSPECIFIED.,.F.,.F.,(4,3,3,
3,3,3,3,4),(-3.6646581839854,-3.4918212590925,-2.99298965065071,-2.49415804220892,
-1.99532643376714,-1.49649482532536,-0.99766321688357,-0.960268764914586),
 .UNSPECIFIED.);
#240=B_SPLINE_CURVE_WITH_KNOTS('',3,(#40124,#40125,#40126,#40127),
 .UNSPECIFIED.,.F.,.F.,(4,4),(0.,0.437203234519499),.UNSPECIFIED.);
#241=B_SPLINE_CURVE_WITH_KNOTS('',3,(#40132,#40133,#40134,#40135,#40136,
#40137,#40138,#40139,#40140,#40141,#40142,#40143,#40144,#40145,#40146,#40147,
#40148,#40149,#40150,#40151,#40152,#40153,#40154,#40155,#40156,#40157,#40158,
#40159,#40160,#40161,#40162,#40163,#40164,#40165,#40166,#40167,#40168),
 .UNSPECIFIED.,.F.,.F.,(4,3,3,3,3,3,3,3,3,3,3,3,4),(-9.94784349116496,-9.47780056039391,
-8.97896895195213,-8.48013734351034,-7.98130573506856,-7.48247412662677,
-6.98364251818499,-6.48481090974321,-5.98597930130142,-5.48714769285963,
-4.98831608441785,-3.99065286753428,-3.6646581839854),.UNSPECIFIED.);
#242=B_SPLINE_CURVE_WITH_KNOTS('',3,(#40169,#40170,#40171,#40172,#40173,
#40174,#40175,#40176,#40177,#40178,#40179,#40180,#40181,#40182,#40183,#40184,
#40185,#40186,#40187,#40188,#40189,#40190,#40191,#40192,#40193,#40194,#40195,
#40196,#40197,#40198,#40199,#40200,#40201,#40202,#40203,#40204,#40205,#40206,
#40207,#40208,#40209,#40210,#40211),.UNSPECIFIED.,.F.,.F.,(4,3,3,3,3,3,
3,3,3,3,3,3,3,3,4),(0.437203234519499,0.499946908284749,0.999893816569588,
1.49984072485443,1.99978763313927,2.49973454142411,2.99968144970895,3.49962835799379,
3.99957526627863,4.49952217456346,4.99946908284831,5.49941599113315,5.99936289941799,
6.49930980770282,6.72038854169909),.UNSPECIFIED.);
#243=B_SPLINE_CURVE_WITH_KNOTS('',3,(#40216,#40217,#40218,#40219,#40220,
#40221,#40222,#40223,#40224,#40225,#40226,#40227,#40228,#40229,#40230,#40231,
#40232,#40233,#40234,#40235,#40236,#40237,#40238,#40239,#40240,#40241,#40242,
#40243,#40244,#40245,#40246,#40247,#40248,#40249,#40250,#40251,#40252,#40253,
#40254,#40255),.UNSPECIFIED.,.F.,.F.,(4,3,3,3,3,3,3,3,3,3,3,3,3,4),(-16.2310287983446,
-15.9626114701371,-15.4637798616953,-14.9649482532535,-14.4661166448118,
-13.96728503637,-13.4684534279282,-12.9696218194864,-12.4707902110446,-11.9719586026028,
-10.9742953857193,-10.4754637772775,-9.9766321688357,-9.94784349116496),
 .UNSPECIFIED.);
#244=B_SPLINE_CURVE_WITH_KNOTS('',3,(#40256,#40257,#40258,#40259,#40260,
#40261,#40262,#40263,#40264,#40265,#40266,#40267,#40268,#40269,#40270,#40271,
#40272,#40273,#40274,#40275,#40276,#40277,#40278,#40279,#40280,#40281,#40282,
#40283,#40284,#40285,#40286,#40287,#40288,#40289,#40290,#40291,#40292,#40293,
#40294,#40295,#40296,#40297,#40298),.UNSPECIFIED.,.F.,.F.,(4,3,3,3,3,3,
3,3,3,3,3,3,3,3,4),(6.72038854169909,6.99925671598767,7.49920362427252,
7.99915053255736,8.49909744084221,8.99904434912705,9.4989912574119,9.99893816569675,
10.4988850739816,10.9988319822664,11.4987788905513,11.9987257988361,12.498672707121,
12.9986196154058,13.0035738488787),.UNSPECIFIED.);
#245=B_SPLINE_CURVE_WITH_KNOTS('',3,(#40303,#40304,#40305,#40306,#40307,
#40308,#40309,#40310,#40311,#40312,#40313,#40314,#40315,#40316,#40317,#40318,
#40319,#40320,#40321,#40322,#40323,#40324,#40325,#40326,#40327,#40328,#40329,
#40330,#40331,#40332,#40333,#40334,#40335,#40336,#40337,#40338,#40339,#40340,
#40341,#40342),.UNSPECIFIED.,.F.,.F.,(4,3,3,3,3,3,3,3,3,3,3,3,3,4),(-22.5142141055241,
-22.4474223798803,-21.9485907714385,-21.4497591629967,-20.950927554555,
-20.4520959461132,-19.9532643376714,-19.4544327292296,-18.9556011207878,
-17.9579379039043,-17.4591062954625,-16.9602746870207,-16.4614430785789,
-16.2310287983446),.UNSPECIFIED.);
#246=B_SPLINE_CURVE_WITH_KNOTS('',3,(#40343,#40344,#40345,#40346,#40347,
#40348,#40349,#40350,#40351,#40352,#40353,#40354,#40355,#40356,#40357,#40358,
#40359,#40360,#40361,#40362,#40363,#40364,#40365,#40366,#40367,#40368,#40369,
#40370,#40371,#40372,#40373,#40374,#40375,#40376,#40377,#40378,#40379,#40380,
#40381,#40382),.UNSPECIFIED.,.F.,.F.,(4,3,3,3,3,3,3,3,3,3,3,3,3,4),(13.0035738488787,
13.4985665236907,13.9985134319755,14.4984603402604,14.9984072485452,15.49835415683,
15.9983010651149,16.4982479733997,16.9981948816846,17.4981417899694,17.9980886982543,
18.4980356065391,18.9979825148239,19.2867591560582),.UNSPECIFIED.);
#247=B_SPLINE_CURVE_WITH_KNOTS('',3,(#40387,#40388,#40389,#40390,#40391,
#40392,#40393,#40394,#40395,#40396,#40397,#40398,#40399,#40400,#40401,#40402,
#40403,#40404,#40405,#40406,#40407,#40408,#40409,#40410,#40411),
 .UNSPECIFIED.,.F.,.F.,(4,3,3,3,3,3,3,3,4),(-28.7973994127037,-28.008505735355,
-27.2196120580062,-26.4307183806574,-25.6418247033086,-24.8529310259599,
-24.0640373486111,-23.2751436712623,-22.5142141055241),.UNSPECIFIED.);
#248=B_SPLINE_CURVE_WITH_KNOTS('',3,(#40412,#40413,#40414,#40415,#40416,
#40417,#40418,#40419,#40420,#40421,#40422,#40423,#40424,#40425,#40426,#40427,
#40428,#40429,#40430,#40431,#40432,#40433,#40434,#40435,#40436,#40437,#40438,
#40439,#40440,#40441,#40442,#40443,#40444,#40445,#40446,#40447,#40448,#40449,
#40450,#40451,#40452,#40453,#40454),.UNSPECIFIED.,.F.,.F.,(4,3,3,3,3,3,
3,3,3,3,3,3,3,3,4),(19.2867591560582,19.4979294231088,19.9978763313936,
20.4978232396785,20.9977701479633,21.4977170562482,21.997663964533,22.4976108728179,
22.9975577811027,23.4975046893875,23.9974515976724,24.4973985059572,24.9973454142421,
25.4972923225269,25.5699444632378),.UNSPECIFIED.);
#249=B_SPLINE_CURVE_WITH_KNOTS('',3,(#40459,#40460,#40461,#40462,#40463,
#40464,#40465,#40466,#40467,#40468,#40469,#40470,#40471,#40472,#40473,#40474,
#40475,#40476,#40477,#40478,#40479,#40480,#40481,#40482,#40483),
 .UNSPECIFIED.,.F.,.F.,(4,3,3,3,3,3,3,3,4),(-35.0805847198833,-34.2916910425345,
-33.5027973651858,-32.713903687837,-31.9250100104882,-31.1361163331394,
-30.3472226557907,-29.5583289784419,-28.7973994127037),.UNSPECIFIED.);
#250=B_SPLINE_CURVE_WITH_KNOTS('',3,(#40484,#40485,#40486,#40487,#40488,
#40489,#40490,#40491,#40492,#40493,#40494,#40495,#40496,#40497,#40498,#40499,
#40500,#40501,#40502,#40503,#40504,#40505,#40506,#40507,#40508,#40509,#40510,
#40511,#40512,#40513,#40514,#40515,#40516,#40517,#40518,#40519,#40520,#40521,
#40522,#40523),.UNSPECIFIED.,.F.,.F.,(4,3,3,3,3,3,3,3,3,3,3,3,3,4),(25.5699444632378,
25.9972392308118,26.4971861390966,26.9971330473814,27.4970799556663,27.9970268639511,
28.496973772236,28.9969206805208,29.4968675888057,29.9968144970905,30.4967614053753,
30.9967083136602,31.496655221945,31.8531297704174),.UNSPECIFIED.);
#251=B_SPLINE_CURVE_WITH_KNOTS('',3,(#40528,#40529,#40530,#40531,#40532,
#40533,#40534,#40535,#40536,#40537,#40538,#40539,#40540,#40541,#40542,#40543,
#40544,#40545,#40546,#40547,#40548,#40549,#40550,#40551,#40552,#40553,#40554,
#40555,#40556,#40557,#40558,#40559,#40560,#40561,#40562,#40563,#40564),
 .UNSPECIFIED.,.F.,.F.,(4,3,3,3,3,3,3,3,3,3,3,3,4),(-41.3637700270629,-40.9041918922264,
-40.4053602837846,-39.9065286753428,-38.9088654584592,-38.4100338500174,
-37.9112022415756,-37.4123706331339,-36.9135390246921,-36.4147074162503,
-35.9158758078085,-35.4170441993667,-35.0805847198833),.UNSPECIFIED.);
#252=B_SPLINE_CURVE_WITH_KNOTS('',3,(#40565,#40566,#40567,#40568,#40569,
#40570,#40571,#40572,#40573,#40574,#40575,#40576,#40577,#40578,#40579,#40580,
#40581,#40582,#40583,#40584,#40585,#40586,#40587,#40588,#40589,#40590,#40591,
#40592,#40593,#40594,#40595,#40596,#40597,#40598,#40599,#40600,#40601,#40602,
#40603,#40604,#40605,#40606,#40607),.UNSPECIFIED.,.F.,.F.,(4,3,3,3,3,3,
3,3,3,3,3,3,3,3,4),(31.8531297704174,31.9966021302299,32.4965490385147,
32.9964959467996,33.4964428550844,33.9963897633693,34.4963366716541,34.9962835799389,
35.4962304882238,35.9961773965086,36.4961243047935,36.9960712130783,37.4960181213632,
37.995965029648,38.136315077597),.UNSPECIFIED.);
#253=B_SPLINE_CURVE_WITH_KNOTS('',3,(#40612,#40613,#40614,#40615,#40616,
#40617,#40618,#40619,#40620,#40621,#40622,#40623,#40624,#40625,#40626,#40627,
#40628,#40629,#40630,#40631,#40632,#40633,#40634,#40635,#40636,#40637,#40638,
#40639,#40640,#40641,#40642,#40643,#40644,#40645,#40646,#40647,#40648,#40649,
#40650,#40651),.UNSPECIFIED.,.F.,.F.,(4,3,3,3,3,3,3,3,3,3,3,3,3,4),(-47.6469553342425,
-47.3890028019696,-46.8901711935278,-45.8925079766442,-45.3936763682024,
-44.8948447597606,-44.3960131513188,-43.8971815428771,-43.3983499344353,
-42.8995183259935,-42.4006867175517,-41.9018551091099,-41.4030235006681,
-41.3637700270629),.UNSPECIFIED.);
#254=B_SPLINE_CURVE_WITH_KNOTS('',3,(#40652,#40653,#40654,#40655,#40656,
#40657,#40658,#40659,#40660,#40661,#40662,#40663,#40664,#40665,#40666,#40667,
#40668,#40669,#40670,#40671,#40672,#40673,#40674,#40675,#40676,#40677,#40678,
#40679,#40680,#40681,#40682,#40683,#40684,#40685,#40686,#40687,#40688,#40689,
#40690,#40691),.UNSPECIFIED.,.F.,.F.,(4,3,3,3,3,3,3,3,3,3,3,3,3,4),(38.136315077597,
38.4959119379328,38.9958588462177,39.4958057545025,39.9957526627874,40.4956995710722,
40.9956464793571,41.4955933876419,41.9955402959268,42.4954872042116,42.9954341124965,
43.4953810207813,43.9953279290661,44.4195003847766),.UNSPECIFIED.);
#255=B_SPLINE_CURVE_WITH_KNOTS('',3,(#40696,#40697,#40698,#40699,#40700,
#40701,#40702,#40703,#40704,#40705,#40706,#40707,#40708,#40709,#40710,#40711,
#40712,#40713,#40714,#40715,#40716,#40717,#40718,#40719,#40720,#40721,#40722,
#40723,#40724,#40725,#40726,#40727,#40728,#40729,#40730,#40731,#40732,#40733,
#40734,#40735),.UNSPECIFIED.,.F.,.F.,(4,3,3,3,3,3,3,3,3,3,3,3,3,4),(-53.9301406414221,
-53.8738137117128,-52.8761504948292,-52.3773188863874,-51.8784872779456,
-51.3796556695038,-50.8808240610621,-50.3819924526203,-49.8831608441785,
-49.3843292357367,-48.8854976272949,-48.3866660188531,-47.8878344104113,
-47.6469553342425),.UNSPECIFIED.);
#256=B_SPLINE_CURVE_WITH_KNOTS('',3,(#40736,#40737,#40738,#40739,#40740,
#40741,#40742,#40743,#40744,#40745,#40746,#40747,#40748,#40749,#40750,#40751,
#40752,#40753,#40754,#40755,#40756,#40757,#40758,#40759,#40760,#40761,#40762,
#40763,#40764,#40765,#40766,#40767,#40768,#40769,#40770,#40771,#40772,#40773,
#40774,#40775,#40776,#40777,#40778),.UNSPECIFIED.,.F.,.F.,(4,3,3,3,3,3,
3,3,3,3,3,3,3,3,4),(44.4195003847766,44.495274837351,44.9952217456358,45.4951686539207,
45.9951155622055,46.4950624704904,46.9950093787752,47.49495628706,47.9949031953449,
48.4948501036297,48.9947970119145,49.4947439201994,49.9946908284842,50.4946377367691,
50.7026856919562),.UNSPECIFIED.);
#257=B_SPLINE_CURVE_WITH_KNOTS('',3,(#40783,#40784,#40785,#40786,#40787,
#40788,#40789,#40790,#40791,#40792,#40793,#40794,#40795,#40796,#40797,#40798,
#40799,#40800,#40801,#40802,#40803,#40804,#40805,#40806,#40807,#40808,#40809,
#40810,#40811,#40812,#40813,#40814,#40815,#40816,#40817,#40818,#40819,#40820,
#40821,#40822),.UNSPECIFIED.,.F.,.F.,(4,3,3,3,3,3,3,3,3,3,3,3,3,4),(-60.2133259486017,
-59.8597930130142,-59.3609614045724,-58.8621297961306,-58.3632981876888,
-57.864466579247,-57.3656349708053,-56.8668033623635,-56.3679717539217,
-55.8691401454799,-55.3703085370381,-54.8714769285963,-54.3726453201545,
-53.9301406414221),.UNSPECIFIED.);
#258=B_SPLINE_CURVE_WITH_KNOTS('',3,(#40823,#40824,#40825,#40826,#40827,
#40828,#40829,#40830,#40831,#40832,#40833,#40834,#40835,#40836,#40837,#40838,
#40839,#40840,#40841,#40842,#40843,#40844,#40845,#40846,#40847,#40848,#40849,
#40850,#40851,#40852,#40853,#40854,#40855,#40856,#40857,#40858,#40859,#40860,
#40861,#40862),.UNSPECIFIED.,.F.,.F.,(4,3,3,3,3,3,3,3,3,3,3,3,3,4),(50.7026856919562,
50.9945846450539,51.4945315533388,51.9944784616236,52.4944253699085,52.9943722781933,
53.4943191864781,53.994266094763,54.4942130030478,54.9941599113327,55.4941068196175,
55.9940537279024,56.4940006361872,56.9858709991358),.UNSPECIFIED.);
#259=B_SPLINE_CURVE_WITH_KNOTS('',3,(#40867,#40868,#40869,#40870,#40871,
#40872,#40873,#40874,#40875,#40876,#40877,#40878,#40879,#40880,#40881,#40882,
#40883,#40884,#40885,#40886,#40887,#40888,#40889,#40890,#40891,#40892,#40893,
#40894,#40895,#40896,#40897,#40898,#40899,#40900,#40901,#40902,#40903,#40904,
#40905,#40906),.UNSPECIFIED.,.F.,.F.,(4,3,3,3,3,3,3,3,3,3,3,3,3,4),(-66.4965112557813,
-66.3446039227574,-65.8457723143156,-65.3469407058738,-64.848109097432,
-64.3492774889902,-63.8504458805484,-63.3516142721067,-62.8527826636649,
-62.3539510552231,-61.8551194467813,-61.3562878383395,-60.8574562298977,
-60.2133259486017),.UNSPECIFIED.);
#260=B_SPLINE_CURVE_WITH_KNOTS('',3,(#40907,#40908,#40909,#40910,#40911,
#40912,#40913,#40914,#40915,#40916,#40917,#40918,#40919,#40920,#40921,#40922,
#40923,#40924,#40925,#40926,#40927,#40928,#40929,#40930,#40931,#40932,#40933,
#40934,#40935,#40936,#40937,#40938,#40939,#40940,#40941,#40942,#40943,#40944,
#40945,#40946,#40947,#40948,#40949),.UNSPECIFIED.,.F.,.F.,(4,3,3,3,3,3,
3,3,3,3,3,3,3,3,4),(56.9858709991358,56.9939475444721,57.4938944527569,
57.9938413610417,58.4937882693266,58.9937351776114,59.4936820858963,59.9936289941811,
60.493575902466,60.9935228107508,61.4934697190356,61.9934166273205,62.4933635356053,
62.9933104438902,63.2690563063154),.UNSPECIFIED.);
#261=B_SPLINE_CURVE_WITH_KNOTS('',3,(#40954,#40955,#40956,#40957,#40958,
#40959,#40960,#40961,#40962,#40963,#40964,#40965,#40966,#40967,#40968,#40969,
#40970,#40971,#40972,#40973,#40974,#40975,#40976,#40977,#40978,#40979,#40980,
#40981,#40982,#40983,#40984,#40985,#40986,#40987,#40988,#40989,#40990),
 .UNSPECIFIED.,.F.,.F.,(4,3,3,3,3,3,3,3,3,3,3,3,4),(-72.7796965629609,-72.3305832240588,
-71.831751615617,-71.3329200071752,-70.8340883987335,-70.3352567902917,
-69.8364251818499,-69.3375935734081,-68.8387619649663,-68.3399303565245,
-67.8410987480827,-66.8434355311992,-66.4965112557813),.UNSPECIFIED.);
#262=B_SPLINE_CURVE_WITH_KNOTS('',3,(#40991,#40992,#40993,#40994,#40995,
#40996,#40997,#40998,#40999,#41000,#41001,#41002,#41003,#41004,#41005,#41006,
#41007,#41008,#41009,#41010,#41011,#41012,#41013,#41014,#41015,#41016,#41017,
#41018,#41019,#41020,#41021,#41022,#41023,#41024,#41025,#41026,#41027,#41028,
#41029,#41030,#41031,#41032,#41033),.UNSPECIFIED.,.F.,.F.,(4,3,3,3,3,3,
3,3,3,3,3,3,3,3,4),(63.2690563063154,63.493257352175,63.9932042604598,64.4931511687447,
64.9930980770295,65.4930449853144,65.9929918935992,66.4929388018841,66.9928857101689,
67.4928326184538,67.9927795267386,68.4927264350235,68.9926733433083,69.4926202515931,
69.552241613495),.UNSPECIFIED.);
#263=B_SPLINE_CURVE_WITH_KNOTS('',3,(#41038,#41039,#41040,#41041,#41042,
#41043,#41044,#41045,#41046,#41047,#41048,#41049,#41050,#41051,#41052,#41053,
#41054,#41055,#41056,#41057,#41058,#41059,#41060,#41061,#41062,#41063,#41064,
#41065,#41066,#41067,#41068,#41069,#41070,#41071,#41072,#41073,#41074,#41075,
#41076,#41077),.UNSPECIFIED.,.F.,.F.,(4,3,3,3,3,3,3,3,3,3,3,3,3,4),(-79.0628818701405,
-78.815394133802,-78.3165625253602,-77.8177309169184,-77.3188993084766,
-76.8200677000349,-76.3212360915931,-75.8224044831513,-75.3235728747095,
-74.8247412662677,-73.8270780493842,-73.3282464409424,-72.8294148325006,
-72.7796965629609),.UNSPECIFIED.);
#264=B_SPLINE_CURVE_WITH_KNOTS('',3,(#41078,#41079,#41080,#41081,#41082,
#41083,#41084,#41085,#41086,#41087,#41088,#41089,#41090,#41091,#41092,#41093,
#41094,#41095,#41096,#41097,#41098,#41099,#41100,#41101,#41102,#41103,#41104,
#41105,#41106,#41107,#41108,#41109,#41110,#41111,#41112,#41113,#41114,#41115,
#41116,#41117),.UNSPECIFIED.,.F.,.F.,(4,3,3,3,3,3,3,3,3,3,3,3,3,4),(69.552241613495,
69.992567159878,70.4925140681628,70.9924609764477,71.4924078847325,71.9923547930174,
72.4923017013022,72.9922486095871,73.4921955178719,73.9921424261567,74.4920893344416,
74.9920362427264,75.4919831510113,75.8354269206746),.UNSPECIFIED.);
#265=B_SPLINE_CURVE_WITH_KNOTS('',3,(#41122,#41123,#41124,#41125,#41126,
#41127,#41128,#41129,#41130,#41131,#41132,#41133,#41134,#41135,#41136,#41137,
#41138,#41139,#41140,#41141,#41142,#41143,#41144,#41145,#41146,#41147,#41148,
#41149,#41150,#41151,#41152,#41153,#41154,#41155,#41156,#41157,#41158,#41159,
#41160,#41161),.UNSPECIFIED.,.F.,.F.,(4,3,3,3,3,3,3,3,3,3,3,3,3,4),(-85.3460671773201,
-85.3002050435452,-84.8013734351034,-84.3025418266616,-83.8037102182198,
-83.3048786097781,-82.8060470013363,-82.3072153928945,-81.8083837844527,
-80.8107205675691,-80.3118889591274,-79.8130573506856,-79.3142257422438,
-79.0628818701405),.UNSPECIFIED.);
#266=B_SPLINE_CURVE_WITH_KNOTS('',3,(#41162,#41163,#41164,#41165,#41166,
#41167,#41168,#41169,#41170,#41171,#41172,#41173,#41174,#41175,#41176,#41177,
#41178,#41179,#41180,#41181,#41182,#41183,#41184,#41185,#41186,#41187,#41188,
#41189,#41190,#41191,#41192,#41193,#41194,#41195,#41196,#41197,#41198,#41199,
#41200,#41201,#41202,#41203,#41204),.UNSPECIFIED.,.F.,.F.,(4,3,3,3,3,3,
3,3,3,3,3,3,3,3,4),(75.8354269206746,75.9919300592961,76.491876967581,76.9918238758658,
77.4917707841506,77.9917176924355,78.4916646007203,78.9916115090052,79.49155841729,
79.9915053255748,80.4914522338597,80.9913991421445,81.4913460504294,81.9912929587142,
82.1186122278542),.UNSPECIFIED.);
#267=B_SPLINE_CURVE_WITH_KNOTS('',3,(#41209,#41210,#41211,#41212,#41213,
#41214,#41215,#41216,#41217,#41218,#41219,#41220,#41221,#41222,#41223,#41224,
#41225,#41226,#41227,#41228,#41229,#41230,#41231,#41232,#41233),
 .UNSPECIFIED.,.F.,.F.,(4,3,3,3,3,3,3,3,4),(-91.6292524844997,-90.8403588071509,
-90.0514651298022,-89.2625714524534,-88.4736777751046,-87.6847840977559,
-86.8958904204071,-86.1069967430584,-85.3460671773201),.UNSPECIFIED.);
#268=B_SPLINE_CURVE_WITH_KNOTS('',3,(#41234,#41235,#41236,#41237,#41238,
#41239,#41240,#41241,#41242,#41243,#41244,#41245,#41246,#41247,#41248,#41249,
#41250,#41251,#41252,#41253,#41254,#41255,#41256,#41257,#41258,#41259,#41260,
#41261,#41262,#41263,#41264,#41265,#41266,#41267,#41268,#41269,#41270,#41271,
#41272,#41273),.UNSPECIFIED.,.F.,.F.,(4,3,3,3,3,3,3,3,3,3,3,3,3,4),(82.1186122278542,
82.4912398669991,82.9911867752839,83.4911336835687,83.9910805918536,84.4910275001384,
84.9909744084233,85.4909213167081,85.990868224993,86.4908151332778,86.9907620415627,
87.4907089498475,87.9906558581323,88.4017975350338),.UNSPECIFIED.);
#269=B_SPLINE_CURVE_WITH_KNOTS('',3,(#41278,#41279,#41280,#41281,#41282,
#41283,#41284,#41285,#41286,#41287,#41288,#41289,#41290,#41291,#41292,#41293,
#41294,#41295,#41296,#41297,#41298,#41299,#41300,#41301,#41302),
 .UNSPECIFIED.,.F.,.F.,(4,3,3,3,3,3,3,3,4),(-97.9124377916793,-97.1235441143305,
-96.3346504369817,-95.545756759633,-94.7568630822842,-93.9679694049355,
-93.1790757275867,-92.390182050238,-91.6292524844997),.UNSPECIFIED.);
#270=B_SPLINE_CURVE_WITH_KNOTS('',3,(#41303,#41304,#41305,#41306,#41307,
#41308,#41309,#41310,#41311,#41312,#41313,#41314,#41315,#41316,#41317,#41318,
#41319,#41320,#41321,#41322,#41323,#41324,#41325,#41326,#41327,#41328,#41329,
#41330,#41331,#41332,#41333,#41334,#41335,#41336,#41337,#41338,#41339,#41340,
#41341,#41342,#41343,#41344,#41345),.UNSPECIFIED.,.F.,.F.,(4,3,3,3,3,3,
3,3,3,3,3,3,3,3,4),(88.4017975350338,88.4906027664172,88.990549674702,89.4904965829869,
89.9904434912717,90.4903903995565,90.9903373078414,91.4902842161263,91.9902311244111,
92.4901780326959,92.9901249409808,93.4900718492656,93.9900187575504,94.4899656658353,
94.6849828422133),.UNSPECIFIED.);
#271=B_SPLINE_CURVE_WITH_KNOTS('',3,(#41350,#41351,#41352,#41353,#41354,
#41355,#41356,#41357,#41358,#41359,#41360,#41361,#41362,#41363,#41364,#41365,
#41366,#41367,#41368,#41369,#41370,#41371,#41372,#41373,#41374,#41375,#41376,
#41377,#41378,#41379,#41380,#41381,#41382,#41383,#41384,#41385,#41386),
 .UNSPECIFIED.,.F.,.F.,(4,3,3,3,3,3,3,3,3,3,3,3,4),(-104.195623098859,-103.756974555891,
-103.258142947449,-102.759311339008,-101.761648122124,-101.262816513682,
-100.763984905241,-100.265153296799,-99.766321688357,-99.2674900799152,
-98.7686584714734,-98.2698268630316,-97.9124377916793),.UNSPECIFIED.);
#272=B_SPLINE_CURVE_WITH_KNOTS('',3,(#41387,#41388,#41389,#41390,#41391,
#41392,#41393,#41394,#41395,#41396,#41397,#41398,#41399,#41400,#41401,#41402,
#41403,#41404,#41405,#41406,#41407,#41408,#41409,#41410,#41411,#41412,#41413,
#41414,#41415,#41416,#41417,#41418,#41419,#41420,#41421,#41422,#41423,#41424,
#41425,#41426),.UNSPECIFIED.,.F.,.F.,(4,3,3,3,3,3,3,3,3,3,3,3,3,4),(94.6849828422133,
94.9899125741201,95.489859482405,95.9898063906898,96.4897532989747,96.9897002072595,
97.4896471155444,97.9895940238292,98.4895409321141,98.9894878403989,99.4894347486837,
99.9893816569686,100.489328565253,100.968168149393),.UNSPECIFIED.);
#273=B_SPLINE_CURVE_WITH_KNOTS('',3,(#41431,#41432,#41433,#41434,#41435,
#41436,#41437,#41438,#41439,#41440,#41441,#41442,#41443,#41444,#41445,#41446,
#41447,#41448,#41449,#41450,#41451,#41452,#41453,#41454,#41455,#41456,#41457,
#41458,#41459,#41460,#41461,#41462,#41463,#41464,#41465,#41466,#41467,#41468,
#41469,#41470),.UNSPECIFIED.,.F.,.F.,(4,3,3,3,3,3,3,3,3,3,3,3,3,4),(-110.478808406038,
-110.241785465634,-109.742953857193,-108.745290640309,-108.246459031867,
-107.747627423426,-107.248795814984,-106.749964206542,-106.2511325981,-105.752300989658,
-105.253469381217,-104.754637772775,-104.255806164333,-104.195623098859),
 .UNSPECIFIED.);
#274=B_SPLINE_CURVE_WITH_KNOTS('',3,(#41471,#41472,#41473,#41474,#41475,
#41476,#41477,#41478,#41479,#41480,#41481,#41482,#41483,#41484,#41485,#41486,
#41487,#41488,#41489,#41490,#41491,#41492,#41493,#41494,#41495,#41496,#41497,
#41498,#41499,#41500,#41501,#41502,#41503,#41504,#41505,#41506,#41507,#41508,
#41509,#41510,#41511,#41512,#41513),.UNSPECIFIED.,.F.,.F.,(4,3,3,3,3,3,
3,3,3,3,3,3,3,3,4),(100.968168149393,100.989275473538,101.489222381823,
101.989169290108,102.489116198393,102.989063106678,103.489010014963,103.988956923247,
104.488903831532,104.988850739817,105.488797648102,105.988744556387,106.488691464672,
106.988638372956,107.251353456573),.UNSPECIFIED.);
#275=B_SPLINE_CURVE_WITH_KNOTS('',3,(#41518,#41519,#41520,#41521,#41522,
#41523,#41524,#41525,#41526,#41527,#41528,#41529,#41530,#41531,#41532,#41533,
#41534,#41535,#41536,#41537,#41538,#41539,#41540,#41541,#41542,#41543,#41544,
#41545,#41546,#41547,#41548,#41549,#41550,#41551,#41552,#41553,#41554,#41555,
#41556,#41557),.UNSPECIFIED.,.F.,.F.,(4,3,3,3,3,3,3,3,3,3,3,3,3,4),(-116.761993713218,
-116.726596375378,-115.728933158494,-115.230101550052,-114.731269941611,
-114.232438333169,-113.733606724727,-113.234775116285,-112.735943507843,
-112.237111899402,-111.73828029096,-111.239448682518,-110.740617074076,
-110.478808406038),.UNSPECIFIED.);
#276=B_SPLINE_CURVE_WITH_KNOTS('',3,(#41558,#41559,#41560,#41561,#41562,
#41563,#41564,#41565,#41566,#41567,#41568,#41569,#41570,#41571,#41572,#41573,
#41574,#41575,#41576,#41577,#41578,#41579,#41580,#41581,#41582,#41583,#41584,
#41585,#41586,#41587,#41588,#41589,#41590,#41591,#41592,#41593,#41594,#41595,
#41596,#41597,#41598,#41599,#41600),.UNSPECIFIED.,.F.,.F.,(4,3,3,3,3,3,
3,3,3,3,3,3,3,3,4),(107.251353456573,107.488585281241,107.988532189526,
108.488479097811,108.988426006096,109.488372914381,109.988319822665,110.48826673095,
110.988213639235,111.48816054752,111.988107455805,112.48805436409,112.988001272375,
113.487948180659,113.534538763752),.UNSPECIFIED.);
#277=B_SPLINE_CURVE_WITH_KNOTS('',3,(#41605,#41606,#41607,#41608,#41609,
#41610,#41611,#41612,#41613,#41614,#41615,#41616,#41617,#41618,#41619,#41620,
#41621,#41622,#41623,#41624,#41625,#41626,#41627,#41628,#41629,#41630,#41631,
#41632,#41633,#41634,#41635,#41636,#41637,#41638,#41639,#41640,#41641,#41642,
#41643,#41644),.UNSPECIFIED.,.F.,.F.,(4,3,3,3,3,3,3,3,3,3,3,3,3,4),(-123.045179020398,
-122.712575676679,-122.213744068237,-121.714912459795,-121.216080851354,
-120.717249242912,-120.21841763447,-119.719586026028,-119.220754417587,
-118.721922809145,-118.223091200703,-117.724259592261,-117.225427983819,
-116.761993713218),.UNSPECIFIED.);
#278=B_SPLINE_CURVE_WITH_KNOTS('',3,(#41645,#41646,#41647,#41648,#41649,
#41650,#41651,#41652,#41653,#41654,#41655,#41656,#41657,#41658,#41659,#41660,
#41661,#41662,#41663,#41664,#41665,#41666,#41667,#41668,#41669,#41670,#41671,
#41672,#41673,#41674,#41675,#41676,#41677,#41678,#41679,#41680,#41681,#41682,
#41683,#41684),.UNSPECIFIED.,.F.,.F.,(4,3,3,3,3,3,3,3,3,3,3,3,3,4),(113.534538763752,
113.987895088944,114.487841997229,114.987788905514,115.487735813799,115.987682722084,
116.487629630368,116.987576538653,117.487523446938,117.987470355223,118.487417263508,
118.987364171793,119.487311080077,119.817724070932),.UNSPECIFIED.);
#279=B_SPLINE_CURVE_WITH_KNOTS('',3,(#41689,#41690,#41691,#41692,#41693,
#41694,#41695,#41696,#41697,#41698,#41699,#41700,#41701,#41702,#41703,#41704,
#41705,#41706,#41707,#41708,#41709,#41710,#41711,#41712,#41713,#41714,#41715,
#41716,#41717,#41718,#41719,#41720,#41721,#41722,#41723,#41724,#41725,#41726,
#41727,#41728),.UNSPECIFIED.,.F.,.F.,(4,3,3,3,3,3,3,3,3,3,3,3,3,4),(-129.328364327577,
-129.197386586422,-128.698554977981,-128.199723369539,-127.700891761097,
-127.202060152655,-126.703228544213,-126.204396935772,-125.70556532733,
-125.206733718888,-124.707902110446,-124.209070502004,-123.710238893563,
-123.045179020398),.UNSPECIFIED.);
#280=B_SPLINE_CURVE_WITH_KNOTS('',3,(#41729,#41730,#41731,#41732,#41733,
#41734,#41735,#41736,#41737,#41738,#41739,#41740,#41741,#41742,#41743,#41744,
#41745,#41746,#41747,#41748,#41749,#41750,#41751,#41752,#41753,#41754,#41755,
#41756,#41757,#41758,#41759,#41760,#41761,#41762,#41763,#41764,#41765,#41766,
#41767,#41768,#41769,#41770,#41771),.UNSPECIFIED.,.F.,.F.,(4,3,3,3,3,3,
3,3,3,3,3,3,3,3,4),(119.817724070932,119.987257988362,120.487204896647,
120.987151804932,121.487098713217,121.987045621502,122.486992529787,122.986939438071,
123.486886346356,123.986833254641,124.486780162926,124.986727071211,125.486673979496,
125.98662088778,126.100909378111),.UNSPECIFIED.);
#281=B_SPLINE_CURVE_WITH_KNOTS('',3,(#41776,#41777,#41778,#41779,#41780,
#41781,#41782,#41783,#41784,#41785,#41786,#41787,#41788,#41789,#41790,#41791,
#41792,#41793,#41794,#41795,#41796,#41797,#41798,#41799,#41800,#41801,#41802,
#41803,#41804,#41805,#41806,#41807,#41808,#41809),.UNSPECIFIED.,.F.,.F.,
(4,3,3,3,3,3,3,3,3,3,3,4),(-135.611549634757,-134.684534279282,-134.18570267084,
-133.686871062398,-133.188039453957,-132.689207845515,-132.190376237073,
-131.691544628631,-131.192713020189,-130.693881411748,-129.696218194864,
-129.328364327577),.UNSPECIFIED.);
#282=B_SPLINE_CURVE_WITH_KNOTS('',3,(#41810,#41811,#41812,#41813,#41814,
#41815,#41816,#41817,#41818,#41819,#41820,#41821,#41822,#41823,#41824,#41825,
#41826,#41827,#41828,#41829,#41830,#41831,#41832,#41833,#41834,#41835,#41836,
#41837,#41838,#41839,#41840,#41841,#41842,#41843),.UNSPECIFIED.,.F.,.F.,
(4,3,3,3,3,3,3,3,3,3,3,4),(126.100909378111,126.486567796065,126.98651470435,
127.486461612635,127.98640852092,128.486355429205,128.98630233749,129.486249245774,
129.986196154059,130.986089970629,131.985983787199,132.384094685291),
 .UNSPECIFIED.);
#283=B_SPLINE_CURVE_WITH_KNOTS('',3,(#41848,#41849,#41850,#41851,#41852,
#41853,#41854,#41855,#41856,#41857,#41858,#41859,#41860,#41861,#41862,#41863,
#41864,#41865,#41866,#41867,#41868,#41869,#41870,#41871,#41872,#41873,#41874,
#41875,#41876,#41877,#41878,#41879,#41880,#41881,#41882,#41883,#41884,#41885,
#41886,#41887,#41888,#41889,#41890),.UNSPECIFIED.,.F.,.F.,(4,3,3,3,3,3,
3,3,3,3,3,3,3,3,4),(-141.894734941936,-141.668176797467,-141.169345189025,
-140.670513580583,-140.171681972142,-139.6728503637,-139.174018755258,-138.675187146816,
-138.176355538374,-137.677523929933,-137.178692321491,-136.679860713049,
-136.181029104607,-135.682197496165,-135.611549634757),.UNSPECIFIED.);
#284=B_SPLINE_CURVE_WITH_KNOTS('',3,(#41891,#41892,#41893,#41894,#41895,
#41896,#41897,#41898,#41899,#41900,#41901,#41902,#41903,#41904,#41905,#41906,
#41907,#41908,#41909,#41910,#41911,#41912,#41913,#41914,#41915,#41916,#41917,
#41918,#41919,#41920,#41921,#41922,#41923,#41924,#41925,#41926,#41927,#41928,
#41929,#41930,#41931,#41932,#41933),.UNSPECIFIED.,.F.,.F.,(4,3,3,3,3,3,
3,3,3,3,3,3,3,3,4),(132.384094685291,132.485930695483,132.985877603768,
133.485824512053,133.985771420338,134.485718328623,134.985665236908,135.485612145193,
135.985559053477,136.485505961762,136.985452870047,137.485399778332,137.985346686617,
138.485293594902,138.66727999247),.UNSPECIFIED.);
#285=B_SPLINE_CURVE_WITH_KNOTS('',3,(#41938,#41939,#41940,#41941,#41942,
#41943,#41944,#41945,#41946,#41947,#41948,#41949,#41950,#41951,#41952,#41953,
#41954,#41955,#41956,#41957,#41958,#41959,#41960,#41961,#41962,#41963,#41964,
#41965,#41966,#41967,#41968,#41969,#41970,#41971,#41972,#41973,#41974,#41975,
#41976,#41977),.UNSPECIFIED.,.F.,.F.,(4,3,3,3,3,3,3,3,3,3,3,3,3,4),(-148.177920249116,
-148.15298770721,-147.654156098768,-147.155324490327,-146.656492881885,
-146.157661273443,-145.658829665001,-145.159998056559,-144.661166448118,
-144.162334839676,-143.663503231234,-143.164671622792,-142.66584001435,
-141.894734941936),.UNSPECIFIED.);
#286=B_SPLINE_CURVE_WITH_KNOTS('',3,(#41978,#41979,#41980,#41981,#41982,
#41983,#41984,#41985,#41986,#41987,#41988,#41989,#41990,#41991,#41992,#41993,
#41994,#41995,#41996,#41997,#41998,#41999,#42000,#42001,#42002,#42003,#42004,
#42005,#42006,#42007,#42008,#42009,#42010,#42011,#42012,#42013,#42014,#42015,
#42016,#42017),.UNSPECIFIED.,.F.,.F.,(4,3,3,3,3,3,3,3,3,3,3,3,3,4),(138.66727999247,
138.985240503186,139.485187411471,139.985134319756,140.485081228041,140.985028136326,
141.484975044611,141.984921952895,142.48486886118,142.984815769465,143.48476267775,
143.984709586035,144.48465649432,144.95046529965),.UNSPECIFIED.);
#287=B_SPLINE_CURVE_WITH_KNOTS('',3,(#42022,#42023,#42024,#42025,#42026,
#42027,#42028,#42029,#42030,#42031,#42032,#42033,#42034,#42035,#42036,#42037,
#42038,#42039,#42040,#42041,#42042,#42043,#42044,#42045,#42046,#42047,#42048,
#42049,#42050,#42051,#42052,#42053,#42054,#42055,#42056,#42057,#42058),
 .UNSPECIFIED.,.F.,.F.,(4,3,3,3,3,3,3,3,3,3,3,3,4),(-154.461105556295,-154.138967008512,
-153.64013540007,-153.141303791628,-152.642472183186,-152.143640574744,
-151.644808966303,-151.145977357861,-150.647145749419,-150.148314140977,
-149.649482532535,-148.651819315652,-148.177920249116),.UNSPECIFIED.);
#288=B_SPLINE_CURVE_WITH_KNOTS('',3,(#42059,#42060,#42061,#42062,#42063,
#42064,#42065,#42066,#42067,#42068,#42069,#42070,#42071,#42072,#42073,#42074,
#42075,#42076,#42077,#42078,#42079,#42080,#42081,#42082,#42083,#42084,#42085,
#42086,#42087,#42088,#42089,#42090,#42091,#42092,#42093,#42094,#42095,#42096,
#42097,#42098,#42099,#42100,#42101),.UNSPECIFIED.,.F.,.F.,(4,3,3,3,3,3,
3,3,3,3,3,3,3,3,4),(144.95046529965,144.984603402604,145.484550310889,145.984497219174,
146.484444127459,146.984391035744,147.484337944029,147.984284852314,148.484231760598,
148.984178668883,149.484125577168,149.984072485453,150.484019393738,150.983966302023,
151.23365060683),.UNSPECIFIED.);
#289=B_SPLINE_CURVE_WITH_KNOTS('',3,(#42106,#42107,#42108,#42109,#42110,
#42111,#42112,#42113,#42114,#42115,#42116,#42117,#42118,#42119,#42120,#42121,
#42122,#42123,#42124,#42125,#42126,#42127,#42128,#42129,#42130,#42131,#42132,
#42133,#42134,#42135,#42136,#42137,#42138,#42139,#42140,#42141,#42142,#42143,
#42144,#42145),.UNSPECIFIED.,.F.,.F.,(4,3,3,3,3,3,3,3,3,3,3,3,3,4),(-160.744290863475,
-160.623777918255,-160.124946309813,-159.626114701371,-159.127283092929,
-158.628451484488,-158.129619876046,-157.630788267604,-157.131956659162,
-156.63312505072,-155.635461833837,-155.136630225395,-154.637798616953,
-154.461105556295),.UNSPECIFIED.);
#290=B_SPLINE_CURVE_WITH_KNOTS('',3,(#42146,#42147,#42148,#42149,#42150,
#42151,#42152,#42153,#42154,#42155,#42156,#42157,#42158,#42159,#42160,#42161,
#42162,#42163,#42164,#42165,#42166,#42167,#42168,#42169,#42170,#42171,#42172,
#42173,#42174,#42175,#42176,#42177,#42178,#42179,#42180,#42181,#42182,#42183,
#42184,#42185,#42186,#42187,#42188),.UNSPECIFIED.,.F.,.F.,(4,3,3,3,3,3,
3,3,3,3,3,3,3,3,4),(151.23365060683,151.483913210307,151.983860118592,152.483807026877,
152.983753935162,153.483700843447,153.983647751732,154.483594660017,154.983541568301,
155.483488476586,155.983435384871,156.483382293156,156.983329201441,157.483276109726,
157.516835914009),.UNSPECIFIED.);
#291=B_SPLINE_CURVE_WITH_KNOTS('',3,(#42193,#42194,#42195,#42196,#42197,
#42198,#42199,#42200,#42201,#42202,#42203,#42204,#42205,#42206,#42207,#42208,
#42209,#42210,#42211,#42212,#42213,#42214,#42215,#42216,#42217,#42218,#42219,
#42220,#42221,#42222,#42223,#42224,#42225,#42226,#42227,#42228,#42229),
 .UNSPECIFIED.,.F.,.F.,(4,3,3,3,3,3,3,3,3,3,3,3,4),(-167.027476170655,-166.609757219556,
-166.110925611114,-165.612094002673,-165.113262394231,-164.614430785789,
-164.115599177347,-163.616767568905,-162.619104352022,-162.12027274358,
-161.621441135138,-161.122609526696,-160.744290863475),.UNSPECIFIED.);
#292=B_SPLINE_CURVE_WITH_KNOTS('',3,(#42230,#42231,#42232,#42233,#42234,
#42235,#42236,#42237,#42238,#42239,#42240,#42241,#42242,#42243,#42244,#42245,
#42246,#42247,#42248,#42249,#42250,#42251,#42252,#42253,#42254,#42255,#42256,
#42257,#42258,#42259,#42260,#42261,#42262,#42263,#42264,#42265,#42266,#42267,
#42268,#42269),.UNSPECIFIED.,.F.,.F.,(4,3,3,3,3,3,3,3,3,3,3,3,3,4),(157.516835914009,
157.98322301801,158.483169926295,158.98311683458,159.483063742865,159.98301065115,
160.482957559435,160.98290446772,161.482851376004,161.982798284289,162.482745192574,
162.982692100859,163.482639009144,163.800021221189),.UNSPECIFIED.);
#293=B_SPLINE_CURVE_WITH_KNOTS('',3,(#42274,#42275,#42276,#42277,#42278,
#42279,#42280,#42281,#42282,#42283,#42284,#42285,#42286,#42287,#42288,#42289,
#42290,#42291,#42292,#42293,#42294,#42295,#42296,#42297,#42298),
 .UNSPECIFIED.,.F.,.F.,(4,3,3,3,3,3,3,3,4),(-173.310661477834,-172.521767800485,
-171.732874123137,-170.943980445788,-170.155086768439,-169.36619309109,
-168.577299413742,-167.788405736393,-167.027476170655),.UNSPECIFIED.);
#294=B_SPLINE_CURVE_WITH_KNOTS('',3,(#42299,#42300,#42301,#42302,#42303,
#42304,#42305,#42306,#42307,#42308,#42309,#42310,#42311,#42312,#42313,#42314,
#42315,#42316,#42317,#42318,#42319,#42320,#42321,#42322,#42323,#42324,#42325,
#42326,#42327,#42328,#42329,#42330,#42331,#42332,#42333,#42334,#42335,#42336,
#42337,#42338,#42339,#42340,#42341),.UNSPECIFIED.,.F.,.F.,(4,3,3,3,3,3,
3,3,3,3,3,3,3,3,4),(163.800021221189,163.982585917429,164.482532825713,
164.982479733998,165.482426642283,165.982373550568,166.482320458853,166.982267367138,
167.482214275422,167.982161183707,168.482108091992,168.982055000277,169.482001908562,
169.981948816847,170.083206528368),.UNSPECIFIED.);
#295=B_SPLINE_CURVE_WITH_KNOTS('',3,(#42346,#42347,#42348,#42349,#42350,
#42351,#42352,#42353,#42354,#42355,#42356,#42357,#42358,#42359,#42360,#42361,
#42362,#42363,#42364,#42365,#42366,#42367,#42368,#42369,#42370),
 .UNSPECIFIED.,.F.,.F.,(4,3,3,3,3,3,3,3,4),(-179.593846785014,-178.804953107665,
-178.016059430316,-177.227165752967,-176.438272075619,-175.64937839827,
-174.860484720921,-174.071591043572,-173.310661477834),.UNSPECIFIED.);
#296=B_SPLINE_CURVE_WITH_KNOTS('',3,(#42371,#42372,#42373,#42374,#42375,
#42376,#42377,#42378,#42379,#42380,#42381,#42382,#42383,#42384,#42385,#42386,
#42387,#42388,#42389,#42390,#42391,#42392,#42393,#42394,#42395,#42396,#42397,
#42398,#42399,#42400,#42401,#42402,#42403,#42404,#42405,#42406,#42407,#42408,
#42409,#42410),.UNSPECIFIED.,.F.,.F.,(4,3,3,3,3,3,3,3,3,3,3,3,3,4),(170.083206528368,
170.481895725131,170.981842633416,171.481789541701,171.981736449986,172.481683358271,
172.981630266556,173.481577174841,173.981524083125,174.48147099141,174.981417899695,
175.48136480798,175.981311716265,176.366391835548),.UNSPECIFIED.);
#297=B_SPLINE_CURVE_WITH_KNOTS('',3,(#42415,#42416,#42417,#42418,#42419,
#42420,#42421,#42422,#42423,#42424,#42425,#42426,#42427,#42428,#42429,#42430,
#42431,#42432,#42433,#42434,#42435,#42436,#42437,#42438,#42439,#42440,#42441,
#42442,#42443,#42444,#42445,#42446,#42447,#42448,#42449,#42450,#42451),
 .UNSPECIFIED.,.F.,.F.,(4,3,3,3,3,3,3,3,3,3,3,3,4),(-185.877032092193,-185.565358340344,
-185.066526731902,-184.56769512346,-183.570031906577,-183.071200298135,
-182.572368689693,-182.073537081251,-181.57470547281,-181.075873864368,
-180.577042255926,-180.078210647484,-179.593846785014),.UNSPECIFIED.);
#298=B_SPLINE_CURVE_WITH_KNOTS('',3,(#42452,#42453,#42454,#42455,#42456,
#42457,#42458,#42459,#42460,#42461,#42462,#42463,#42464,#42465,#42466,#42467,
#42468,#42469,#42470,#42471,#42472,#42473,#42474,#42475,#42476,#42477,#42478,
#42479,#42480,#42481,#42482,#42483,#42484,#42485,#42486,#42487,#42488,#42489,
#42490,#42491,#42492,#42493,#42494),.UNSPECIFIED.,.F.,.F.,(4,3,3,3,3,3,
3,3,3,3,3,3,3,3,4),(176.366391835548,176.48125862455,176.981205532834,177.481152441119,
177.981099349404,178.481046257689,178.980993165974,179.480940074259,179.980886982544,
180.480833890828,180.980780799113,181.480727707398,181.980674615683,182.480621523968,
182.649577142727),.UNSPECIFIED.);
#299=B_SPLINE_CURVE_WITH_KNOTS('',3,(#42499,#42500,#42501,#42502,#42503,
#42504,#42505,#42506,#42507,#42508,#42509,#42510,#42511,#42512,#42513,#42514,
#42515,#42516,#42517,#42518,#42519,#42520,#42521,#42522,#42523,#42524,#42525,
#42526,#42527,#42528,#42529,#42530,#42531,#42532,#42533,#42534,#42535,#42536,
#42537,#42538),.UNSPECIFIED.,.F.,.F.,(4,3,3,3,3,3,3,3,3,3,3,3,3,4),(-192.160217399373,
-192.050169250087,-191.551337641645,-190.553674424762,-190.05484281632,
-189.556011207878,-189.057179599436,-188.558347990995,-188.059516382553,
-187.560684774111,-187.061853165669,-186.563021557228,-186.064189948786,
-185.877032092193),.UNSPECIFIED.);
#300=B_SPLINE_CURVE_WITH_KNOTS('',3,(#42539,#42540,#42541,#42542,#42543,
#42544,#42545,#42546,#42547,#42548,#42549,#42550,#42551,#42552,#42553,#42554,
#42555,#42556,#42557,#42558,#42559,#42560,#42561,#42562,#42563,#42564,#42565,
#42566,#42567,#42568,#42569,#42570,#42571,#42572,#42573,#42574,#42575,#42576,
#42577,#42578),.UNSPECIFIED.,.F.,.F.,(4,3,3,3,3,3,3,3,3,3,3,3,3,4),(182.649577142727,
182.980568432253,183.480515340537,183.980462248822,184.480409157107,184.980356065392,
185.480302973677,185.980249881962,186.480196790247,186.980143698531,187.480090606816,
187.980037515101,188.479984423386,188.932762449907),.UNSPECIFIED.);
#301=B_SPLINE_CURVE_WITH_KNOTS('',3,(#42583,#42584,#42585,#42586,#42587,
#42588,#42589,#42590,#42591,#42592,#42593,#42594,#42595,#42596,#42597,#42598,
#42599,#42600,#42601,#42602,#42603,#42604,#42605,#42606,#42607,#42608,#42609,
#42610,#42611,#42612,#42613,#42614,#42615,#42616,#42617,#42618,#42619),
 .UNSPECIFIED.,.F.,.F.,(4,3,3,3,3,3,3,3,3,3,3,3,4),(-198.443402706552,-197.537316942947,
-197.038485334505,-196.539653726063,-196.040822117621,-195.54199050918,
-195.043158900738,-194.544327292296,-194.045495683854,-193.546664075412,
-193.047832466971,-192.549000858529,-192.160217399373),.UNSPECIFIED.);
#302=B_SPLINE_CURVE_WITH_KNOTS('',3,(#42620,#42621,#42622,#42623,#42624,
#42625,#42626,#42627,#42628,#42629,#42630,#42631,#42632,#42633,#42634,#42635,
#42636,#42637,#42638,#42639,#42640,#42641,#42642,#42643,#42644,#42645,#42646,
#42647,#42648,#42649,#42650,#42651,#42652,#42653,#42654,#42655,#42656,#42657,
#42658,#42659,#42660,#42661,#42662),.UNSPECIFIED.,.F.,.F.,(4,3,3,3,3,3,
3,3,3,3,3,3,3,3,4),(188.932762449907,188.979931331671,189.479878239956,
189.97982514824,190.479772056525,190.97971896481,191.479665873095,191.97961278138,
192.479559689665,192.979506597949,193.479453506234,193.979400414519,194.479347322804,
194.979294231089,195.215947757087),.UNSPECIFIED.);
#303=B_SPLINE_CURVE_WITH_KNOTS('',3,(#42667,#42668,#42669,#42670,#42671,
#42672,#42673,#42674,#42675,#42676,#42677,#42678,#42679,#42680,#42681,#42682,
#42683,#42684,#42685,#42686,#42687,#42688,#42689,#42690,#42691,#42692,#42693,
#42694,#42695,#42696,#42697,#42698,#42699,#42700,#42701,#42702,#42703,#42704,
#42705,#42706,#42707,#42708,#42709),.UNSPECIFIED.,.F.,.F.,(4,3,3,3,3,3,
3,3,3,3,3,3,3,3,4),(-204.726588013732,-204.520959461132,-204.02212785269,
-203.523296244248,-203.024464635806,-202.525633027365,-202.026801418923,
-201.527969810481,-201.029138202039,-200.530306593597,-200.031474985156,
-199.532643376714,-199.033811768272,-198.53498015983,-198.443402706552),
 .UNSPECIFIED.);
#304=B_SPLINE_CURVE_WITH_KNOTS('',3,(#42710,#42711,#42712,#42713,#42714,
#42715,#42716,#42717,#42718,#42719,#42720,#42721,#42722,#42723,#42724,#42725,
#42726,#42727,#42728,#42729,#42730,#42731,#42732,#42733,#42734,#42735,#42736,
#42737,#42738,#42739,#42740,#42741,#42742,#42743,#42744,#42745,#42746,#42747,
#42748,#42749,#42750,#42751,#42752),.UNSPECIFIED.,.F.,.F.,(4,3,3,3,3,3,
3,3,3,3,3,3,3,3,4),(195.215947757087,195.479241139374,195.979188047659,
196.479134955943,196.979081864228,197.479028772513,197.978975680798,198.478922589083,
198.978869497368,199.478816405652,199.978763313937,200.478710222222,200.978657130507,
201.478604038792,201.499133064266),.UNSPECIFIED.);
#305=B_SPLINE_CURVE_WITH_KNOTS('',3,(#42757,#42758,#42759,#42760,#42761,
#42762,#42763,#42764,#42765,#42766,#42767,#42768,#42769,#42770,#42771,#42772,
#42773,#42774,#42775,#42776,#42777,#42778,#42779,#42780,#42781,#42782,#42783,
#42784,#42785,#42786,#42787,#42788,#42789,#42790,#42791,#42792,#42793,#42794,
#42795,#42796),.UNSPECIFIED.,.F.,.F.,(4,3,3,3,3,3,3,3,3,3,3,3,3,4),(-211.009773320912,
-211.005770370875,-210.506938762433,-210.008107153991,-209.50927554555,
-209.010443937108,-208.511612328666,-208.012780720224,-207.513949111782,
-207.015117503341,-206.516285894899,-206.017454286457,-205.518622678015,
-204.726588013732),.UNSPECIFIED.);
#306=B_SPLINE_CURVE_WITH_KNOTS('',3,(#42797,#42798,#42799,#42800,#42801,
#42802,#42803,#42804,#42805,#42806,#42807,#42808,#42809,#42810,#42811,#42812,
#42813,#42814,#42815,#42816,#42817,#42818,#42819,#42820,#42821,#42822,#42823,
#42824,#42825,#42826,#42827,#42828,#42829,#42830,#42831,#42832,#42833,#42834,
#42835,#42836),.UNSPECIFIED.,.F.,.F.,(4,3,3,3,3,3,3,3,3,3,3,3,3,4),(201.499133064266,
201.978550947077,202.478497855361,202.978444763646,203.478391671931,203.978338580216,
204.478285488501,204.978232396786,205.478179305071,205.978126213355,206.47807312164,
206.978020029925,207.47796693821,207.782318371446),.UNSPECIFIED.);
#307=B_SPLINE_CURVE_WITH_KNOTS('',3,(#42841,#42842,#42843,#42844,#42845,
#42846,#42847,#42848,#42849,#42850,#42851,#42852,#42853,#42854,#42855,#42856,
#42857,#42858,#42859,#42860,#42861,#42862,#42863,#42864,#42865,#42866,#42867,
#42868,#42869,#42870,#42871,#42872,#42873,#42874,#42875,#42876,#42877),
 .UNSPECIFIED.,.F.,.F.,(4,3,3,3,3,3,3,3,3,3,3,3,4),(-217.292958628091,-216.991749672176,
-216.492918063735,-215.994086455293,-215.495254846851,-214.996423238409,
-214.497591629967,-213.998760021526,-213.499928413084,-213.001096804642,
-212.5022651962,-211.504601979317,-211.009773320912),.UNSPECIFIED.);
#308=B_SPLINE_CURVE_WITH_KNOTS('',3,(#42878,#42879,#42880,#42881,#42882,
#42883,#42884,#42885,#42886,#42887,#42888,#42889,#42890,#42891,#42892,#42893,
#42894,#42895,#42896,#42897,#42898,#42899,#42900,#42901,#42902,#42903,#42904,
#42905,#42906,#42907,#42908,#42909,#42910,#42911,#42912,#42913,#42914,#42915,
#42916,#42917,#42918,#42919,#42920),.UNSPECIFIED.,.F.,.F.,(4,3,3,3,3,3,
3,3,3,3,3,3,3,3,4),(207.782318371446,207.977913846495,208.47786075478,208.977807663065,
209.477754571349,209.977701479634,210.477648387919,210.977595296204,211.477542204489,
211.977489112774,212.477436021058,212.977382929343,213.477329837628,213.977276745913,
214.065503678625),.UNSPECIFIED.);
#309=B_SPLINE_CURVE_WITH_KNOTS('',3,(#42925,#42926,#42927,#42928,#42929,
#42930,#42931,#42932,#42933,#42934,#42935,#42936,#42937,#42938,#42939,#42940,
#42941,#42942,#42943,#42944,#42945,#42946,#42947,#42948,#42949,#42950,#42951,
#42952,#42953,#42954,#42955,#42956,#42957,#42958,#42959,#42960,#42961,#42962,
#42963,#42964),.UNSPECIFIED.,.F.,.F.,(4,3,3,3,3,3,3,3,3,3,3,3,3,4),(-223.576143935271,
-223.47656058192,-222.977728973478,-222.478897365036,-221.980065756594,
-221.481234148152,-220.982402539711,-220.483570931269,-219.984739322827,
-219.485907714385,-218.488244497502,-217.98941288906,-217.490581280618,
-217.292958628091),.UNSPECIFIED.);
#310=B_SPLINE_CURVE_WITH_KNOTS('',3,(#42965,#42966,#42967,#42968,#42969,
#42970,#42971,#42972,#42973,#42974,#42975,#42976,#42977,#42978,#42979,#42980,
#42981,#42982,#42983,#42984,#42985,#42986,#42987,#42988,#42989,#42990,#42991,
#42992,#42993,#42994,#42995,#42996,#42997,#42998,#42999,#43000,#43001,#43002,
#43003,#43004),.UNSPECIFIED.,.F.,.F.,(4,3,3,3,3,3,3,3,3,3,3,3,3,4),(214.065503678625,
214.477223654198,214.977170562483,215.477117470767,215.977064379052,216.477011287337,
216.976958195622,217.476905103907,217.976852012192,218.476798920477,218.976745828761,
219.476692737046,219.976639645331,220.348688985805),.UNSPECIFIED.);
#311=B_SPLINE_CURVE_WITH_KNOTS('',3,(#43009,#43010,#43011,#43012,#43013,
#43014,#43015,#43016,#43017,#43018,#43019,#43020,#43021,#43022,#43023,#43024,
#43025,#43026,#43027,#43028,#43029,#43030,#43031,#43032,#43033,#43034,#43035,
#43036,#43037,#43038,#43039,#43040,#43041,#43042,#43043,#43044,#43045),
 .UNSPECIFIED.,.F.,.F.,(4,3,3,3,3,3,3,3,3,3,3,3,4),(-229.85932924245,-229.462539883221,
-228.963708274779,-228.464876666337,-227.966045057896,-227.467213449454,
-226.968381841012,-226.46955023257,-225.471887015687,-224.973055407245,
-224.474223798803,-223.975392190361,-223.576143935271),.UNSPECIFIED.);
#312=B_SPLINE_CURVE_WITH_KNOTS('',3,(#43046,#43047,#43048,#43049,#43050,
#43051,#43052,#43053,#43054,#43055,#43056,#43057,#43058,#43059,#43060,#43061,
#43062,#43063,#43064,#43065,#43066,#43067,#43068,#43069,#43070,#43071,#43072,
#43073,#43074,#43075,#43076,#43077,#43078,#43079,#43080,#43081,#43082,#43083,
#43084,#43085,#43086,#43087,#43088),.UNSPECIFIED.,.F.,.F.,(4,3,3,3,3,3,
3,3,3,3,3,3,3,3,4),(220.348688985805,220.476586553616,220.976533461901,
221.476480370186,221.97642727847,222.476374186755,222.97632109504,223.476268003325,
223.97621491161,224.476161819895,224.976108728179,225.476055636464,225.976002544749,
226.475949453034,226.631874292984),.UNSPECIFIED.);
#313=B_SPLINE_CURVE_WITH_KNOTS('',3,(#43093,#43094,#43095,#43096,#43097,
#43098,#43099,#43100,#43101,#43102,#43103,#43104,#43105,#43106,#43107,#43108,
#43109,#43110,#43111,#43112,#43113,#43114,#43115,#43116,#43117),
 .UNSPECIFIED.,.F.,.F.,(4,3,3,3,3,3,3,3,4),(-236.14251454963,-235.353620872281,
-234.564727194932,-233.775833517583,-232.986939840235,-232.198046162886,
-231.409152485537,-230.620258808188,-229.85932924245),.UNSPECIFIED.);
#314=B_SPLINE_CURVE_WITH_KNOTS('',3,(#43118,#43119,#43120,#43121,#43122,
#43123,#43124,#43125,#43126,#43127,#43128,#43129,#43130,#43131,#43132,#43133,
#43134,#43135,#43136,#43137,#43138,#43139,#43140,#43141,#43142,#43143,#43144,
#43145,#43146,#43147,#43148,#43149,#43150,#43151,#43152,#43153,#43154,#43155,
#43156,#43157),.UNSPECIFIED.,.F.,.F.,(4,3,3,3,3,3,3,3,3,3,3,3,3,4),(226.631874292984,
226.975896361319,227.475843269604,227.975790177889,228.475737086173,228.975683994458,
229.475630902743,229.975577811028,230.475524719313,230.975471627598,231.475418535882,
231.975365444167,232.475312352452,232.915059600164),.UNSPECIFIED.);
#315=B_SPLINE_CURVE_WITH_KNOTS('',3,(#43162,#43163,#43164,#43165,#43166,
#43167,#43168,#43169,#43170,#43171,#43172,#43173,#43174,#43175,#43176,#43177,
#43178,#43179,#43180,#43181,#43182,#43183,#43184,#43185,#43186,#43187,#43188,
#43189,#43190,#43191,#43192,#43193,#43194,#43195,#43196,#43197,#43198),
 .UNSPECIFIED.,.F.,.F.,(4,3,3,3,3,3,3,3,3,3,3,3,4),(-242.425699856809,-241.933330094266,
-241.434498485824,-240.935666877382,-240.43683526894,-239.439172052057,
-238.940340443615,-238.441508835173,-237.942677226731,-237.44384561829,
-236.945014009848,-236.446182401406,-236.14251454963),.UNSPECIFIED.);
#316=B_SPLINE_CURVE_WITH_KNOTS('',3,(#43199,#43200,#43201,#43202,#43203,
#43204,#43205,#43206,#43207,#43208,#43209,#43210,#43211,#43212,#43213,#43214,
#43215,#43216,#43217,#43218,#43219,#43220,#43221,#43222,#43223,#43224,#43225,
#43226,#43227,#43228,#43229,#43230,#43231,#43232,#43233,#43234,#43235,#43236,
#43237,#43238,#43239,#43240,#43241),.UNSPECIFIED.,.F.,.F.,(4,3,3,3,3,3,
3,3,3,3,3,3,3,3,4),(232.915059600164,232.975259260737,233.475206169022,
233.975153077307,234.475099985591,234.975046893876,235.474993802161,235.974940710446,
236.474887618731,236.974834527016,237.474781435301,237.974728343585,238.47467525187,
238.974622160155,239.198244907343),.UNSPECIFIED.);
#317=B_SPLINE_CURVE_WITH_KNOTS('',3,(#43246,#43247,#43248,#43249,#43250,
#43251,#43252,#43253,#43254,#43255,#43256,#43257,#43258,#43259,#43260,#43261,
#43262,#43263,#43264,#43265,#43266,#43267,#43268,#43269,#43270,#43271,#43272,
#43273,#43274,#43275,#43276,#43277,#43278,#43279,#43280,#43281,#43282,#43283,
#43284,#43285),.UNSPECIFIED.,.F.,.F.,(4,3,3,3,3,3,3,3,3,3,3,3,3,4),(-248.708885163989,
-248.418141004009,-247.919309395567,-247.420477787125,-246.422814570242,
-245.9239829618,-245.425151353358,-244.926319744916,-244.427488136475,-243.928656528033,
-243.429824919591,-242.930993311149,-242.432161702707,-242.425699856809),
 .UNSPECIFIED.);
#318=B_SPLINE_CURVE_WITH_KNOTS('',3,(#43286,#43287,#43288,#43289,#43290,
#43291,#43292,#43293,#43294,#43295,#43296,#43297,#43298,#43299,#43300,#43301,
#43302,#43303,#43304,#43305,#43306,#43307,#43308,#43309,#43310,#43311,#43312,
#43313,#43314,#43315,#43316,#43317,#43318,#43319,#43320,#43321,#43322,#43323,
#43324,#43325,#43326,#43327,#43328),.UNSPECIFIED.,.F.,.F.,(4,3,3,3,3,3,
3,3,3,3,3,3,3,3,4),(239.198244907343,239.47456906844,239.974515976725,240.47446288501,
240.974409793294,241.474356701579,241.974303609864,242.474250518149,242.974197426434,
243.474144334719,243.974091243004,244.474038151288,244.973985059573,245.473931967858,
245.481430214523),.UNSPECIFIED.);
#319=B_SPLINE_CURVE_WITH_KNOTS('',3,(#43333,#43334,#43335,#43336,#43337,
#43338,#43339,#43340,#43341,#43342,#43343,#43344,#43345,#43346,#43347,#43348,
#43349,#43350,#43351,#43352,#43353,#43354,#43355,#43356,#43357,#43358,#43359,
#43360,#43361,#43362,#43363,#43364,#43365,#43366,#43367,#43368,#43369,#43370,
#43371,#43372),.UNSPECIFIED.,.F.,.F.,(4,3,3,3,3,3,3,3,3,3,3,3,3,4),(-254.992070471168,
-254.902951913752,-254.40412030531,-253.406457088427,-252.907625479985,
-252.408793871543,-251.909962263101,-251.41113065466,-250.912299046218,
-250.413467437776,-249.914635829334,-249.415804220892,-248.916972612451,
-248.708885163989),.UNSPECIFIED.);
#320=B_SPLINE_CURVE_WITH_KNOTS('',3,(#43373,#43374,#43375,#43376,#43377,
#43378,#43379,#43380,#43381,#43382,#43383,#43384,#43385,#43386,#43387,#43388,
#43389,#43390,#43391,#43392,#43393,#43394,#43395,#43396,#43397,#43398,#43399,
#43400,#43401,#43402,#43403,#43404,#43405,#43406,#43407,#43408,#43409,#43410,
#43411,#43412),.UNSPECIFIED.,.F.,.F.,(4,3,3,3,3,3,3,3,3,3,3,3,3,4),(245.481430214523,
245.973878876143,246.473825784428,246.973772692713,247.473719600997,247.973666509282,
248.473613417567,248.973560325852,249.473507234137,249.973454142422,250.473401050706,
250.973347958991,251.473294867276,251.764615521703),.UNSPECIFIED.);
#321=B_SPLINE_CURVE_WITH_KNOTS('',3,(#43417,#43418,#43419,#43420,#43421,
#43422,#43423,#43424,#43425,#43426,#43427,#43428,#43429,#43430,#43431,#43432,
#43433,#43434,#43435,#43436,#43437,#43438,#43439,#43440,#43441,#43442,#43443,
#43444,#43445,#43446,#43447,#43448,#43449,#43450,#43451,#43452,#43453),
 .UNSPECIFIED.,.F.,.F.,(4,3,3,3,3,3,3,3,3,3,3,3,4),(-261.275255778348,-260.390099606612,
-259.89126799817,-259.392436389728,-258.893604781286,-258.394773172845,
-257.895941564403,-257.397109955961,-256.898278347519,-256.399446739077,
-255.900615130636,-255.401783522194,-254.992070471168),.UNSPECIFIED.);
#322=B_SPLINE_CURVE_WITH_KNOTS('',3,(#43454,#43455,#43456,#43457,#43458,
#43459,#43460,#43461,#43462,#43463,#43464,#43465,#43466,#43467,#43468,#43469,
#43470,#43471,#43472,#43473,#43474,#43475,#43476,#43477,#43478,#43479,#43480,
#43481,#43482,#43483,#43484,#43485,#43486,#43487,#43488,#43489,#43490,#43491,
#43492,#43493,#43494,#43495,#43496),.UNSPECIFIED.,.F.,.F.,(4,3,3,3,3,3,
3,3,3,3,3,3,3,3,4),(251.764615521703,251.973241775561,252.473188683846,
252.973135592131,253.473082500416,253.9730294087,254.472976316985,254.97292322527,
255.472870133555,255.97281704184,256.472763950125,256.972710858409,257.472657766694,
257.972604674979,258.047800828882),.UNSPECIFIED.);
#323=B_SPLINE_CURVE_WITH_KNOTS('',3,(#43502,#43503,#43504,#43505,#43506,
#43507,#43508,#43509,#43510,#43511),.UNSPECIFIED.,.F.,.F.,(4,1,1,1,1,1,
1,4),(273.318560862312,273.431067907459,273.929899515901,274.428731124343,
274.927562732785,275.426394341226,275.925225949668,276.054897710016),
 .UNSPECIFIED.);
#324=B_SPLINE_CURVE_WITH_KNOTS('',3,(#43514,#43515,#43516,#43517,#43518),
 .UNSPECIFIED.,.F.,.F.,(4,1,4),(273.318560862312,273.459489208933,273.959436117218),
 .UNSPECIFIED.);
#325=B_SPLINE_CURVE_WITH_KNOTS('',3,(#43523,#43524,#43525,#43526,#43527,
#43528,#43529,#43530,#43531,#43532,#43533,#43534,#43535,#43536,#43537),
 .UNSPECIFIED.,.F.,.F.,(4,1,1,1,1,1,1,1,1,1,1,1,4),(267.035375555132,267.445088606158,
267.9439202146,268.442751823041,268.941583431483,269.440415039925,269.939246648367,
270.438078256808,270.93690986525,271.435741473692,271.934573082134,272.433404690576,
273.318560862312),.UNSPECIFIED.);
#326=B_SPLINE_CURVE_WITH_KNOTS('',3,(#43538,#43539,#43540,#43541,#43542,
#43543,#43544,#43545,#43546,#43547,#43548,#43549,#43550,#43551,#43552,#43553),
 .UNSPECIFIED.,.F.,.F.,(4,1,1,1,1,1,1,1,1,1,1,1,1,4),(267.035375555132,
267.460126309515,267.9600732178,268.460020126084,268.959967034369,269.459913942654,
269.959860850939,270.459807759224,270.959754667509,271.459701575793,271.959648484078,
272.459595392363,272.959542300648,273.318560862312),.UNSPECIFIED.);
#327=B_SPLINE_CURVE_WITH_KNOTS('',3,(#43558,#43559,#43560,#43561,#43562,
#43563,#43564,#43565,#43566,#43567,#43568,#43569,#43570,#43571,#43572,#43573),
 .UNSPECIFIED.,.F.,.F.,(4,1,1,1,1,1,1,1,1,1,1,1,1,4),(260.752190247953,
260.960277696415,261.459109304856,261.957940913298,262.45677252174,262.955604130182,
263.454435738623,263.953267347065,264.452098955507,264.950930563949,265.449762172391,
266.447425389274,266.946256997716,267.035375555132),.UNSPECIFIED.);
#328=B_SPLINE_CURVE_WITH_KNOTS('',3,(#43574,#43575,#43576,#43577,#43578,
#43579,#43580,#43581,#43582,#43583,#43584,#43585,#43586,#43587,#43588,#43589,
#43590),.UNSPECIFIED.,.F.,.F.,(4,1,1,1,1,1,1,1,1,1,1,1,1,1,4),(260.752190247953,
260.960816501812,261.460763410097,261.960710318381,262.460657226666,262.960604134951,
263.460551043236,263.960497951521,264.460444859806,264.96039176809,265.460338676375,
265.96028558466,266.460232492945,266.96017940123,267.035375555132),
 .UNSPECIFIED.);
#329=B_SPLINE_CURVE_WITH_KNOTS('',3,(#43595,#43596,#43597,#43598,#43599,
#43600,#43601,#43602,#43603,#43604,#43605,#43606,#43607,#43608,#43609,#43610),
 .UNSPECIFIED.,.F.,.F.,(4,1,1,1,1,1,1,1,1,1,1,1,1,4),(254.469004940773,
254.475466786671,254.974298395113,255.473130003555,255.971961611997,256.470793220438,
256.96962482888,257.468456437322,257.967288045764,258.466119654206,259.463782871089,
259.962614479531,260.461446087973,260.752190247953),.UNSPECIFIED.);
#330=B_SPLINE_CURVE_WITH_KNOTS('',3,(#43611,#43612,#43613,#43614,#43615,
#43616,#43617,#43618,#43619,#43620,#43621,#43622,#43623,#43624,#43625,#43626),
 .UNSPECIFIED.,.F.,.F.,(4,1,1,1,1,1,1,1,1,1,1,1,1,4),(254.469004940773,
254.961453602394,255.461400510678,255.961347418963,256.461294327248,256.961241235533,
257.461188143818,257.961135052103,258.461081960387,258.961028868672,259.460975776957,
259.960922685242,260.460869593527,260.752190247953),.UNSPECIFIED.);
#331=B_SPLINE_CURVE_WITH_KNOTS('',3,(#43631,#43632,#43633,#43634,#43635,
#43636,#43637,#43638,#43639,#43640,#43641,#43642,#43643,#43644,#43645),
 .UNSPECIFIED.,.F.,.F.,(4,1,1,1,1,1,1,1,1,1,1,1,4),(248.185819633594,248.48948748537,
248.988319093812,249.487150702254,249.985982310695,250.484813919137,250.983645527579,
251.482477136021,252.480140352904,252.978971961346,253.477803569788,253.97663517823,
254.469004940773),.UNSPECIFIED.);
#332=B_SPLINE_CURVE_WITH_KNOTS('',3,(#43646,#43647,#43648,#43649,#43650,
#43651,#43652,#43653,#43654,#43655,#43656,#43657,#43658,#43659,#43660,#43661,
#43662),.UNSPECIFIED.,.F.,.F.,(4,1,1,1,1,1,1,1,1,1,1,1,1,1,4),(248.185819633594,
248.462143794691,248.962090702975,249.46203761126,249.961984519545,250.46193142783,
250.961878336115,251.4618252444,251.961772152685,252.461719060969,252.961665969254,
253.461612877539,253.961559785824,254.461506694109,254.469004940773),
 .UNSPECIFIED.);
#333=B_SPLINE_CURVE_WITH_KNOTS('',3,(#43667,#43668,#43669,#43670,#43671,
#43672,#43673,#43674,#43675,#43676,#43677,#43678,#43679,#43680,#43681,#43682,
#43683,#43684,#43685,#43686,#43687,#43688,#43689,#43690,#43691),
 .UNSPECIFIED.,.F.,.F.,(4,3,3,3,3,3,3,3,4),(241.902634326414,242.744762189266,
243.586890052118,244.42901791497,245.271145777822,246.113273640674,246.955401503526,
247.797529366378,248.185819633594),.UNSPECIFIED.);
#334=B_SPLINE_CURVE_WITH_KNOTS('',3,(#43692,#43693,#43694,#43695,#43696,
#43697,#43698,#43699,#43700,#43701,#43702,#43703,#43704,#43705,#43706,#43707,
#43708),.UNSPECIFIED.,.F.,.F.,(4,1,1,1,1,1,1,1,1,1,1,1,1,1,4),(241.902634326414,
241.962833986988,242.462780895273,242.962727803557,243.462674711842,243.962621620127,
244.462568528412,244.962515436697,245.462462344982,245.962409253266,246.462356161551,
246.962303069836,247.462249978121,247.962196886406,248.185819633594),
 .UNSPECIFIED.);
#335=B_SPLINE_CURVE_WITH_KNOTS('',3,(#43713,#43714,#43715,#43716,#43717,
#43718,#43719,#43720,#43721,#43722,#43723,#43724,#43725,#43726,#43727),
 .UNSPECIFIED.,.F.,.F.,(4,1,1,1,1,1,1,1,1,1,1,1,4),(235.619449019234,236.018697274325,
236.517528882767,237.016360491209,237.515192099651,238.512855316534,239.011686924976,
239.510518533418,240.00935014186,240.508181750301,241.007013358743,241.505844967185,
241.902634326414),.UNSPECIFIED.);
#336=B_SPLINE_CURVE_WITH_KNOTS('',3,(#43728,#43729,#43730,#43731,#43732,
#43733,#43734,#43735,#43736,#43737,#43738,#43739,#43740,#43741,#43742,#43743),
 .UNSPECIFIED.,.F.,.F.,(4,1,1,1,1,1,1,1,1,1,1,1,1,4),(235.619449019235,
235.96347108757,236.463417995854,236.963364904139,237.463311812424,237.963258720709,
238.463205628994,238.963152537279,239.463099445563,239.963046353848,240.462993262133,
240.962940170418,241.462887078703,241.902634326414),.UNSPECIFIED.);
#337=B_SPLINE_CURVE_WITH_KNOTS('',3,(#43748,#43749,#43750,#43751,#43752,
#43753,#43754,#43755,#43756,#43757,#43758,#43759,#43760,#43761,#43762,#43763),
 .UNSPECIFIED.,.F.,.F.,(4,1,1,1,1,1,1,1,1,1,1,1,1,4),(229.336263712055,
229.533886364582,230.032717973024,230.531549581466,231.529212798349,232.028044406791,
232.526876015233,233.025707623675,233.524539232116,234.023370840558,234.522202449,
235.021034057442,235.519865665884,235.619449019234),.UNSPECIFIED.);
#338=B_SPLINE_CURVE_WITH_KNOTS('',3,(#43764,#43765,#43766,#43767,#43768,
#43769,#43770,#43771,#43772,#43773,#43774,#43775,#43776,#43777,#43778,#43779,
#43780),.UNSPECIFIED.,.F.,.F.,(4,1,1,1,1,1,1,1,1,1,1,1,1,1,4),(229.336263712055,
229.464161279867,229.964108188151,230.464055096436,230.964002004721,231.463948913006,
231.963895821291,232.463842729576,232.96378963786,233.463736546145,233.96368345443,
234.463630362715,234.963577271,235.463524179285,235.619449019235),
 .UNSPECIFIED.);
#339=B_SPLINE_CURVE_WITH_KNOTS('',3,(#43785,#43786,#43787,#43788,#43789,
#43790,#43791,#43792,#43793,#43794,#43795,#43796,#43797,#43798,#43799),
 .UNSPECIFIED.,.F.,.F.,(4,1,1,1,1,1,1,1,1,1,1,1,4),(223.053078404875,223.547907063281,
224.545570280164,225.044401888606,225.543233497048,226.04206510549,226.540896713931,
227.039728322373,227.538559930815,228.037391539257,228.536223147699,229.03505475614,
229.336263712055),.UNSPECIFIED.);
#340=B_SPLINE_CURVE_WITH_KNOTS('',3,(#43800,#43801,#43802,#43803,#43804,
#43805,#43806,#43807,#43808,#43809,#43810,#43811,#43812,#43813,#43814,#43815),
 .UNSPECIFIED.,.F.,.F.,(4,1,1,1,1,1,1,1,1,1,1,1,1,4),(223.053078404875,
223.464798380448,223.964745288733,224.464692197018,224.964639105303,225.464586013588,
225.964532921873,226.464479830158,226.964426738442,227.464373646727,227.964320555012,
228.464267463297,228.964214371582,229.336263712055),.UNSPECIFIED.);
#341=B_SPLINE_CURVE_WITH_KNOTS('',3,(#43820,#43821,#43822,#43823,#43824,
#43825,#43826,#43827,#43828,#43829,#43830,#43831,#43832,#43833,#43834,#43835),
 .UNSPECIFIED.,.F.,.F.,(4,1,1,1,1,1,1,1,1,1,1,1,1,4),(216.769893097696,
217.561927761979,218.060759370421,218.559590978863,219.058422587305,219.557254195746,
220.056085804188,220.55491741263,221.053749021072,221.552580629514,222.051412237955,
222.550243846397,223.049075454839,223.053078404875),.UNSPECIFIED.);
#342=B_SPLINE_CURVE_WITH_KNOTS('',3,(#43836,#43837,#43838,#43839,#43840,
#43841,#43842,#43843,#43844,#43845,#43846,#43847,#43848,#43849,#43850,#43851,
#43852),.UNSPECIFIED.,.F.,.F.,(4,1,1,1,1,1,1,1,1,1,1,1,1,1,4),(216.769893097696,
216.965488572745,217.46543548103,217.965382389315,218.4653292976,218.965276205885,
219.46522311417,219.965170022455,220.465116930739,220.965063839024,221.465010747309,
221.964957655594,222.464904563879,222.964851472164,223.053078404875),
 .UNSPECIFIED.);
#343=B_SPLINE_CURVE_WITH_KNOTS('',3,(#43857,#43858,#43859,#43860,#43861,
#43862,#43863,#43864,#43865,#43866,#43867,#43868,#43869,#43870,#43871,#43872,
#43873),.UNSPECIFIED.,.F.,.F.,(4,1,1,1,1,1,1,1,1,1,1,1,1,1,4),(210.486707790516,
210.578285243794,211.077116852236,211.575948460678,212.07478006912,212.573611677561,
213.072443286003,213.571274894445,214.070106502887,214.568938111329,215.06776971977,
215.566601328212,216.065432936654,216.564264545096,216.769893097696),
 .UNSPECIFIED.);
#344=B_SPLINE_CURVE_WITH_KNOTS('',3,(#43874,#43875,#43876,#43877,#43878,
#43879,#43880,#43881,#43882,#43883,#43884,#43885,#43886,#43887,#43888,#43889),
 .UNSPECIFIED.,.F.,.F.,(4,1,1,1,1,1,1,1,1,1,1,1,1,4),(210.486707790516,
210.966125673327,211.466072581612,211.966019489897,212.465966398182,212.965913306467,
213.465860214752,213.965807123036,214.465754031321,214.965700939606,215.465647847891,
215.965594756176,216.465541664461,216.769893097696),.UNSPECIFIED.);
#345=B_SPLINE_CURVE_WITH_KNOTS('',3,(#43894,#43895,#43896,#43897,#43898,
#43899,#43900,#43901,#43902,#43903,#43904,#43905,#43906,#43907,#43908),
 .UNSPECIFIED.,.F.,.F.,(4,1,1,1,1,1,1,1,1,1,1,1,4),(204.203522483337,204.592305942493,
205.091137550935,205.589969159376,206.088800767818,206.58763237626,207.086463984702,
207.585295593144,208.084127201585,208.582958810027,209.081790418469,209.580622026911,
210.486707790516),.UNSPECIFIED.);
#346=B_SPLINE_CURVE_WITH_KNOTS('',3,(#43909,#43910,#43911,#43912,#43913,
#43914,#43915,#43916,#43917,#43918,#43919,#43920,#43921,#43922,#43923,#43924,
#43925),.UNSPECIFIED.,.F.,.F.,(4,1,1,1,1,1,1,1,1,1,1,1,1,1,4),(204.203522483337,
204.466815865624,204.966762773909,205.466709682194,205.966656590479,206.466603498764,
206.966550407049,207.466497315333,207.966444223618,208.466391131903,208.966338040188,
209.466284948473,209.966231856758,210.466178765043,210.486707790516),
 .UNSPECIFIED.);
#347=B_SPLINE_CURVE_WITH_KNOTS('',3,(#43930,#43931,#43932,#43933,#43934,
#43935,#43936,#43937,#43938,#43939,#43940,#43941,#43942,#43943,#43944,#43945),
 .UNSPECIFIED.,.F.,.F.,(4,1,1,1,1,1,1,1,1,1,1,1,1,4),(197.920337176157,
198.10749503275,198.606326641191,199.105158249633,199.603989858075,200.102821466517,
200.601653074959,201.1004846834,201.599316291842,202.098147900284,202.596979508726,
203.594642725609,204.093474334051,204.203522483337),.UNSPECIFIED.);
#348=B_SPLINE_CURVE_WITH_KNOTS('',3,(#43946,#43947,#43948,#43949,#43950,
#43951,#43952,#43953,#43954,#43955,#43956,#43957,#43958,#43959,#43960,#43961,
#43962),.UNSPECIFIED.,.F.,.F.,(4,1,1,1,1,1,1,1,1,1,1,1,1,1,4),(197.920337176157,
197.967506057921,198.467452966206,198.967399874491,199.467346782776,199.967293691061,
200.467240599346,200.967187507631,201.467134415915,201.9670813242,202.467028232485,
202.96697514077,203.466922049055,203.96686895734,204.203522483337),
 .UNSPECIFIED.);
#349=B_SPLINE_CURVE_WITH_KNOTS('',3,(#43967,#43968,#43969,#43970,#43971,
#43972,#43973,#43974,#43975,#43976,#43977,#43978,#43979,#43980,#43981),
 .UNSPECIFIED.,.F.,.F.,(4,1,1,1,1,1,1,1,1,1,1,1,4),(191.637151868978,192.121515731448,
192.62034733989,193.119178948332,193.618010556774,194.116842165215,194.615673773657,
195.114505382099,195.613336990541,196.611000207424,197.109831815866,197.608663424308,
197.920337176157),.UNSPECIFIED.);
#350=B_SPLINE_CURVE_WITH_KNOTS('',3,(#43982,#43983,#43984,#43985,#43986,
#43987,#43988,#43989,#43990,#43991,#43992,#43993,#43994,#43995,#43996,#43997),
 .UNSPECIFIED.,.F.,.F.,(4,1,1,1,1,1,1,1,1,1,1,1,1,4),(191.637151868978,
191.968143158503,192.468090066788,192.968036975073,193.467983883358,193.967930791643,
194.467877699928,194.967824608212,195.467771516497,195.967718424782,196.467665333067,
196.967612241352,197.467559149637,197.920337176157),.UNSPECIFIED.);
#351=B_SPLINE_CURVE_WITH_KNOTS('',3,(#44002,#44003,#44004,#44005,#44006,
#44007,#44008,#44009,#44010,#44011,#44012,#44013,#44014,#44015,#44016,#44017),
 .UNSPECIFIED.,.F.,.F.,(4,1,1,1,1,1,1,1,1,1,1,1,1,4),(185.353966561798,
185.636704821705,186.135536430147,186.634368038589,187.13319964703,187.632031255472,
188.130862863914,188.629694472356,189.627357689239,190.126189297681,190.625020906123,
191.123852514565,191.622684123006,191.637151868978),.UNSPECIFIED.);
#352=B_SPLINE_CURVE_WITH_KNOTS('',3,(#44018,#44019,#44020,#44021,#44022,
#44023,#44024,#44025,#44026,#44027,#44028,#44029,#44030,#44031,#44032,#44033,
#44034),.UNSPECIFIED.,.F.,.F.,(4,1,1,1,1,1,1,1,1,1,1,1,1,1,4),(185.353966561798,
185.4688333508,185.968780259085,186.46872716737,186.968674075655,187.46862098394,
187.968567892225,188.468514800509,188.968461708794,189.468408617079,189.968355525364,
190.468302433649,190.968249341934,191.468196250218,191.637151868978),
 .UNSPECIFIED.);
#353=B_SPLINE_CURVE_WITH_KNOTS('',3,(#44039,#44040,#44041,#44042,#44043,
#44044,#44045,#44046,#44047,#44048,#44049,#44050,#44051,#44052,#44053,#44054,
#44055,#44056,#44057,#44058,#44059,#44060,#44061,#44062,#44063),
 .UNSPECIFIED.,.F.,.F.,(4,3,3,3,3,3,3,3,4),(179.070781254618,179.91290911747,
180.755036980322,181.597164843174,182.439292706026,183.281420568878,184.12354843173,
184.965676294582,185.353966561798),.UNSPECIFIED.);
#354=B_SPLINE_CURVE_WITH_KNOTS('',3,(#44064,#44065,#44066,#44067,#44068,
#44069,#44070,#44071,#44072,#44073,#44074,#44075,#44076,#44077,#44078,#44079),
 .UNSPECIFIED.,.F.,.F.,(4,1,1,1,1,1,1,1,1,1,1,1,1,4),(179.070781254618,
179.469470451382,179.969417359667,180.469364267952,180.969311176237,181.469258084522,
181.969204992806,182.469151901091,182.969098809376,183.469045717661,183.968992625946,
184.468939534231,184.968886442515,185.353966561798),.UNSPECIFIED.);
#355=B_SPLINE_CURVE_WITH_KNOTS('',3,(#44084,#44085,#44086,#44087,#44088,
#44089,#44090,#44091,#44092,#44093,#44094,#44095,#44096,#44097,#44098),
 .UNSPECIFIED.,.F.,.F.,(4,1,1,1,1,1,1,1,1,1,1,1,4),(172.787595947439,173.16591461066,
173.664746219102,174.163577827544,174.662409435986,175.660072652869,176.158904261311,
176.657735869753,177.156567478195,177.655399086636,178.154230695078,178.65306230352,
179.070781254618),.UNSPECIFIED.);
#356=B_SPLINE_CURVE_WITH_KNOTS('',3,(#44099,#44100,#44101,#44102,#44103,
#44104,#44105,#44106,#44107,#44108,#44109,#44110,#44111,#44112,#44113,#44114,
#44115),.UNSPECIFIED.,.F.,.F.,(4,1,1,1,1,1,1,1,1,1,1,1,1,1,4),(172.787595947439,
172.970160643679,173.470107551964,173.970054460249,174.470001368534,174.969948276819,
175.469895185103,175.969842093388,176.469789001673,176.969735909958,177.469682818243,
177.969629726528,178.469576634813,178.969523543097,179.070781254618),
 .UNSPECIFIED.);
#357=B_SPLINE_CURVE_WITH_KNOTS('',3,(#44120,#44121,#44122,#44123,#44124,
#44125,#44126,#44127,#44128,#44129,#44130,#44131,#44132,#44133,#44134,#44135),
 .UNSPECIFIED.,.F.,.F.,(4,1,1,1,1,1,1,1,1,1,1,1,1,4),(166.504410640259,
166.681103700917,167.179935309359,167.678766917801,168.676430134684,169.175261743126,
169.674093351568,170.17292496001,170.671756568452,171.170588176893,171.669419785335,
172.168251393777,172.667083002219,172.787595947439),.UNSPECIFIED.);
#358=B_SPLINE_CURVE_WITH_KNOTS('',3,(#44136,#44137,#44138,#44139,#44140,
#44141,#44142,#44143,#44144,#44145,#44146,#44147,#44148,#44149,#44150,#44151),
 .UNSPECIFIED.,.F.,.F.,(4,1,1,1,1,1,1,1,1,1,1,1,1,4),(166.504410640259,
166.970797744261,167.470744652546,167.970691560831,168.470638469116,168.970585377401,
169.470532285685,169.97047919397,170.470426102255,170.97037301054,171.470319918825,
171.97026682711,172.470213735394,172.787595947439),.UNSPECIFIED.);
#359=B_SPLINE_CURVE_WITH_KNOTS('',3,(#44156,#44157,#44158,#44159,#44160,
#44161,#44162,#44163,#44164,#44165,#44166,#44167,#44168,#44169,#44170),
 .UNSPECIFIED.,.F.,.F.,(4,1,1,1,1,1,1,1,1,1,1,1,4),(160.22122533308,160.695124399616,
161.692787616499,162.191619224941,162.690450833383,163.189282441825,163.688114050267,
164.186945658708,164.68577726715,165.184608875592,165.683440484034,166.182272092475,
166.504410640259),.UNSPECIFIED.);
#360=B_SPLINE_CURVE_WITH_KNOTS('',3,(#44171,#44172,#44173,#44174,#44175,
#44176,#44177,#44178,#44179,#44180,#44181,#44182,#44183,#44184,#44185,#44186,
#44187),.UNSPECIFIED.,.F.,.F.,(4,1,1,1,1,1,1,1,1,1,1,1,1,1,4),(160.22122533308,
160.471487936558,160.971434844843,161.471381753128,161.971328661413,162.471275569698,
162.971222477982,163.471169386267,163.971116294552,164.471063202837,164.971010111122,
165.470957019407,165.970903927691,166.470850835976,166.504410640259),
 .UNSPECIFIED.);
#361=B_SPLINE_CURVE_WITH_KNOTS('',3,(#44192,#44193,#44194,#44195,#44196,
#44197,#44198,#44199,#44200,#44201,#44202,#44203,#44204,#44205,#44206,#44207),
 .UNSPECIFIED.,.F.,.F.,(4,1,1,1,1,1,1,1,1,1,1,1,1,4),(153.9380400259,154.709145098314,
155.207976706756,155.706808315198,156.20563992364,156.704471532082,157.203303140523,
157.702134748965,158.200966357407,158.699797965849,159.19862957429,159.697461182732,
160.196292791174,160.22122533308),.UNSPECIFIED.);
#362=B_SPLINE_CURVE_WITH_KNOTS('',3,(#44208,#44209,#44210,#44211,#44212,
#44213,#44214,#44215,#44216,#44217,#44218,#44219,#44220,#44221,#44222,#44223,
#44224),.UNSPECIFIED.,.F.,.F.,(4,1,1,1,1,1,1,1,1,1,1,1,1,1,4),(153.9380400259,
153.972178128855,154.47212503714,154.972071945425,155.47201885371,155.971965761995,
156.471912670279,156.971859578564,157.471806486849,157.971753395134,158.471700303419,
158.971647211704,159.471594119988,159.971541028273,160.22122533308),
 .UNSPECIFIED.);
#363=B_SPLINE_CURVE_WITH_KNOTS('',3,(#44229,#44230,#44231,#44232,#44233,
#44234,#44235,#44236,#44237,#44238,#44239,#44240,#44241,#44242,#44243,#44244,
#44245),.UNSPECIFIED.,.F.,.F.,(4,1,1,1,1,1,1,1,1,1,1,1,1,1,4),(147.654854718721,
147.725502580129,148.224334188571,148.723165797013,149.221997405455,149.720829013897,
150.219660622338,150.71849223078,151.217323839222,151.716155447664,152.214987056105,
152.713818664547,153.212650272989,153.711481881431,153.9380400259),
 .UNSPECIFIED.);
#364=B_SPLINE_CURVE_WITH_KNOTS('',3,(#44246,#44247,#44248,#44249,#44250,
#44251,#44252,#44253,#44254,#44255,#44256,#44257,#44258,#44259,#44260,#44261),
 .UNSPECIFIED.,.F.,.F.,(4,1,1,1,1,1,1,1,1,1,1,1,1,4),(147.654854718721,
147.972815229437,148.472762137722,148.972709046007,149.472655954292,149.972602862576,
150.472549770861,150.972496679146,151.472443587431,151.972390495716,152.472337404001,
152.972284312286,153.47223122057,153.9380400259),.UNSPECIFIED.);
#365=B_SPLINE_CURVE_WITH_KNOTS('',3,(#44266,#44267,#44268,#44269,#44270,
#44271,#44272,#44273,#44274,#44275,#44276,#44277,#44278,#44279),
 .UNSPECIFIED.,.F.,.F.,(4,1,1,1,1,1,1,1,1,1,1,4),(141.371669411541,141.739523278828,
142.737186495712,143.236018104153,143.734849712595,144.233681321037,144.732512929479,
145.231344537921,145.730176146362,146.229007754804,146.727839363246,147.654854718721),
 .UNSPECIFIED.);
#366=B_SPLINE_CURVE_WITH_KNOTS('',3,(#44280,#44281,#44282,#44283,#44284,
#44285,#44286,#44287,#44288,#44289,#44290,#44291,#44292,#44293,#44294,#44295,
#44296),.UNSPECIFIED.,.F.,.F.,(4,1,1,1,1,1,1,1,1,1,1,1,1,1,4),(141.371669411541,
141.473505421734,141.973452330019,142.473399238304,142.973346146589,143.473293054873,
143.973239963158,144.473186871443,144.973133779728,145.473080688013,145.973027596298,
146.472974504583,146.972921412867,147.472868321152,147.654854718721),
 .UNSPECIFIED.);
#367=B_SPLINE_CURVE_WITH_KNOTS('',3,(#44301,#44302,#44303,#44304,#44305,
#44306,#44307,#44308,#44309,#44310,#44311,#44312,#44313,#44314,#44315,#44316),
 .UNSPECIFIED.,.F.,.F.,(4,1,1,1,1,1,1,1,1,1,1,1,1,4),(135.088484104361,
135.753543977527,136.252375585968,136.75120719441,137.250038802852,137.748870411294,
138.247702019735,138.746533628177,139.245365236619,139.744196845061,140.243028453503,
140.741860061944,141.240691670386,141.371669411541),.UNSPECIFIED.);
#368=B_SPLINE_CURVE_WITH_KNOTS('',3,(#44317,#44318,#44319,#44320,#44321,
#44322,#44323,#44324,#44325,#44326,#44327,#44328,#44329,#44330),
 .UNSPECIFIED.,.F.,.F.,(4,1,1,1,1,1,1,1,1,1,1,4),(135.088484104361,135.474142522316,
135.974089430601,136.474036338886,136.973983247171,137.473930155455,137.97387706374,
138.473823972025,138.97377088031,139.97366469688,140.973558513449,141.371669411541),
 .UNSPECIFIED.);
#369=B_SPLINE_CURVE_WITH_KNOTS('',3,(#44335,#44336,#44337,#44338,#44339,
#44340,#44341,#44342,#44343,#44344,#44345,#44346,#44347,#44348,#44349,#44350),
 .UNSPECIFIED.,.F.,.F.,(4,1,1,1,1,1,1,1,1,1,1,1,1,4),(128.805298797182,
129.268733067783,129.767564676225,130.266396284667,130.765227893109,131.26405950155,
131.762891109992,132.261722718434,132.760554326876,133.259385935318,133.758217543759,
134.257049152201,134.755880760643,135.088484104361),.UNSPECIFIED.);
#370=B_SPLINE_CURVE_WITH_KNOTS('',3,(#44351,#44352,#44353,#44354,#44355,
#44356,#44357,#44358,#44359,#44360,#44361,#44362,#44363,#44364,#44365,#44366,
#44367),.UNSPECIFIED.,.F.,.F.,(4,1,1,1,1,1,1,1,1,1,1,1,1,1,4),(128.805298797182,
128.974832714613,129.474779622898,129.974726531183,130.474673439468,130.974620347752,
131.474567256037,131.974514164322,132.474461072607,132.974407980892,133.474354889177,
133.974301797461,134.474248705746,134.974195614031,135.088484104361),
 .UNSPECIFIED.);
#371=B_SPLINE_CURVE_WITH_KNOTS('',3,(#44372,#44373,#44374,#44375,#44376,
#44377,#44378,#44379,#44380,#44381,#44382,#44383,#44384,#44385,#44386,#44387),
 .UNSPECIFIED.,.F.,.F.,(4,1,1,1,1,1,1,1,1,1,1,1,1,4),(122.522113490002,
122.78392215804,123.282753766482,123.781585374924,124.280416983366,124.779248591807,
125.278080200249,125.776911808691,126.275743417133,126.774575025574,127.273406634016,
127.772238242458,128.769901459342,128.805298797182),.UNSPECIFIED.);
#372=B_SPLINE_CURVE_WITH_KNOTS('',3,(#44388,#44389,#44390,#44391,#44392,
#44393,#44394,#44395,#44396,#44397,#44398,#44399,#44400,#44401,#44402,#44403),
 .UNSPECIFIED.,.F.,.F.,(4,1,1,1,1,1,1,1,1,1,1,1,1,4),(122.522113490002,
122.975469815195,123.47541672348,123.975363631765,124.475310540049,124.975257448334,
125.475204356619,125.975151264904,126.475098173189,126.975045081474,127.474991989759,
127.974938898043,128.474885806328,128.805298797182),.UNSPECIFIED.);
#373=B_SPLINE_CURVE_WITH_KNOTS('',3,(#44408,#44409,#44410,#44411,#44412,
#44413,#44414,#44415,#44416,#44417,#44418,#44419,#44420,#44421,#44422,#44423),
 .UNSPECIFIED.,.F.,.F.,(4,1,1,1,1,1,1,1,1,1,1,1,1,4),(116.238928182823,
116.299111248297,116.797942856739,117.296774465181,117.795606073622,118.294437682064,
118.793269290506,119.292100898948,119.790932507389,120.289764115831,120.788595724273,
121.786258941157,122.285090549598,122.522113490002),.UNSPECIFIED.);
#374=B_SPLINE_CURVE_WITH_KNOTS('',3,(#44424,#44425,#44426,#44427,#44428,
#44429,#44430,#44431,#44432,#44433,#44434,#44435,#44436,#44437,#44438,#44439,
#44440),.UNSPECIFIED.,.F.,.F.,(4,1,1,1,1,1,1,1,1,1,1,1,1,1,4),(116.238928182823,
116.476160007492,116.976106915777,117.476053824062,117.976000732346,118.475947640631,
118.975894548916,119.475841457201,119.975788365486,120.475735273771,120.975682182056,
121.47562909034,121.975575998625,122.47552290691,122.522113490002),
 .UNSPECIFIED.);
#375=B_SPLINE_CURVE_WITH_KNOTS('',3,(#44445,#44446,#44447,#44448,#44449,
#44450,#44451,#44452,#44453,#44454,#44455,#44456,#44457,#44458,#44459),
 .UNSPECIFIED.,.F.,.F.,(4,1,1,1,1,1,1,1,1,1,1,1,4),(109.955742875643,110.313131946996,
110.811963555437,111.310795163879,111.809626772321,112.308458380763,112.807289989204,
113.306121597646,113.804953206088,114.802616422972,115.301448031413,115.800279639855,
116.238928182823),.UNSPECIFIED.);
#376=B_SPLINE_CURVE_WITH_KNOTS('',3,(#44460,#44461,#44462,#44463,#44464,
#44465,#44466,#44467,#44468,#44469,#44470,#44471,#44472,#44473,#44474,#44475,
#44476),.UNSPECIFIED.,.F.,.F.,(4,1,1,1,1,1,1,1,1,1,1,1,1,1,4),(109.955742875643,
109.976850199789,110.476797108074,110.976744016359,111.476690924644,111.976637832928,
112.476584741213,112.976531649498,113.476478557783,113.976425466068,114.476372374353,
114.976319282637,115.476266190922,115.976213099207,116.238928182823),
 .UNSPECIFIED.);
#377=B_SPLINE_CURVE_WITH_KNOTS('',3,(#44481,#44482,#44483,#44484,#44485,
#44486,#44487,#44488,#44489,#44490,#44491,#44492,#44493,#44494,#44495,#44496),
 .UNSPECIFIED.,.F.,.F.,(4,1,1,1,1,1,1,1,1,1,1,1,1,4),(103.672557568464,
103.828321037252,104.327152645694,104.825984254136,105.324815862578,105.823647471019,
106.322479079461,106.821310687903,107.818973904787,108.317805513228,108.81663712167,
109.315468730112,109.814300338554,109.955742875643),.UNSPECIFIED.);
#378=B_SPLINE_CURVE_WITH_KNOTS('',3,(#44497,#44498,#44499,#44500,#44501,
#44502,#44503,#44504,#44505,#44506,#44507,#44508,#44509,#44510,#44511,#44512),
 .UNSPECIFIED.,.F.,.F.,(4,1,1,1,1,1,1,1,1,1,1,1,1,4),(103.672557568464,
103.977487300371,104.477434208656,104.977381116941,105.477328025225,105.97727493351,
106.477221841795,106.97716875008,107.477115658365,107.97706256665,108.477009474934,
108.976956383219,109.476903291504,109.955742875643),.UNSPECIFIED.);
#379=B_SPLINE_CURVE_WITH_KNOTS('',3,(#44517,#44518,#44519,#44520,#44521,
#44522,#44523,#44524,#44525,#44526,#44527,#44528,#44529,#44530,#44531),
 .UNSPECIFIED.,.F.,.F.,(4,1,1,1,1,1,1,1,1,1,1,1,4),(97.3893722612839,97.8423417359509,
98.3411733443927,98.8400049528345,99.3388365612763,99.8376681697181,100.835331386602,
101.334162995043,101.832994603485,102.331826211927,102.830657820369,103.329489428811,
103.672557568464),.UNSPECIFIED.);
#380=B_SPLINE_CURVE_WITH_KNOTS('',3,(#44532,#44533,#44534,#44535,#44536,
#44537,#44538,#44539,#44540,#44541,#44542,#44543,#44544,#44545,#44546,#44547,
#44548),.UNSPECIFIED.,.F.,.F.,(4,1,1,1,1,1,1,1,1,1,1,1,1,1,4),(97.389372261284,
97.4781774926679,97.9781244009527,98.4780713092376,98.9780182175224,99.4779651258073,
99.9779120340921,100.477858942377,100.977805850662,101.477752758947,101.977699667231,
102.477646575516,102.977593483801,103.477540392086,103.672557568464),
 .UNSPECIFIED.);
#381=B_SPLINE_CURVE_WITH_KNOTS('',3,(#44553,#44554,#44555,#44556,#44557,
#44558,#44559,#44560,#44561,#44562,#44563,#44564,#44565,#44566,#44567,#44568),
 .UNSPECIFIED.,.F.,.F.,(4,1,1,1,1,1,1,1,1,1,1,1,1,4),(91.1061869541043,
91.3575308262077,91.8563624346495,92.3551940430913,92.8540256515331,93.8516888684167,
94.3505204768584,94.8493520853002,95.348183693742,95.8470153021838,96.3458469106256,
96.8446785190674,97.3435101275091,97.3893722612839),.UNSPECIFIED.);
#382=B_SPLINE_CURVE_WITH_KNOTS('',3,(#44569,#44570,#44571,#44572,#44573,
#44574,#44575,#44576,#44577,#44578,#44579,#44580,#44581,#44582,#44583,#44584),
 .UNSPECIFIED.,.F.,.F.,(4,1,1,1,1,1,1,1,1,1,1,1,1,4),(91.1061869541044,
91.4788145932498,91.9787615015346,92.4787084098195,92.9786553181043,93.4786022263891,
93.978549134674,94.4784960429588,94.9784429512437,95.4783898595285,95.9783367678134,
96.4782836760982,96.9782305843831,97.389372261284),.UNSPECIFIED.);
#383=B_SPLINE_CURVE_WITH_KNOTS('',3,(#44589,#44590,#44591,#44592,#44593,
#44594,#44595,#44596,#44597,#44598,#44599,#44600,#44601,#44602,#44603,#44604),
 .UNSPECIFIED.,.F.,.F.,(4,1,1,1,1,1,1,1,1,1,1,1,1,4),(84.8230016469247,
84.8727199164645,85.3715515249063,85.8703831333481,86.8680463502317,87.3668779586735,
87.8657095671152,88.364541175557,88.8633727839988,89.3622043924406,89.8610360008824,
90.3598676093242,90.8586992177659,91.1061869541043),.UNSPECIFIED.);
#384=B_SPLINE_CURVE_WITH_KNOTS('',3,(#44605,#44606,#44607,#44608,#44609,
#44610,#44611,#44612,#44613,#44614,#44615,#44616,#44617,#44618,#44619,#44620,
#44621),.UNSPECIFIED.,.F.,.F.,(4,1,1,1,1,1,1,1,1,1,1,1,1,1,4),(84.8230016469248,
84.9795047855468,85.4794516938317,85.9793986021165,86.4793455104013,86.9792924186862,
87.479239326971,87.9791862352559,88.4791331435407,88.9790800518255,89.4790269601104,
89.9789738683953,90.4789207766801,90.9788676849649,91.1061869541044),
 .UNSPECIFIED.);
#385=B_SPLINE_CURVE_WITH_KNOTS('',3,(#44626,#44627,#44628,#44629,#44630,
#44631,#44632,#44633,#44634,#44635,#44636,#44637,#44638,#44639,#44640),
 .UNSPECIFIED.,.F.,.F.,(4,1,1,1,1,1,1,1,1,1,1,1,4),(78.5398163397451,78.8867406151631,
79.8844038320467,80.3832354404885,80.8820670489303,81.380898657372,81.8797302658138,
82.3785618742556,82.8773934826974,83.3762250911392,83.875056699581,84.3738883080227,
84.8230016469247),.UNSPECIFIED.);
#386=B_SPLINE_CURVE_WITH_KNOTS('',3,(#44641,#44642,#44643,#44644,#44645,
#44646,#44647,#44648,#44649,#44650,#44651,#44652,#44653,#44654,#44655,#44656),
 .UNSPECIFIED.,.F.,.F.,(4,1,1,1,1,1,1,1,1,1,1,1,1,4),(78.5398163397452,
78.9801418861287,79.4800887944135,79.9800357026984,80.4799826109832,80.9799295192681,
81.4798764275529,81.9798233358378,82.4797702441226,82.9797171524074,83.4796640606923,
83.9796109689771,84.479557877262,84.8230016469248),.UNSPECIFIED.);
#387=B_SPLINE_CURVE_WITH_KNOTS('',3,(#44661,#44662,#44663,#44664,#44665,
#44666,#44667,#44668,#44669,#44670,#44671,#44672,#44673,#44674,#44675,#44676),
 .UNSPECIFIED.,.F.,.F.,(4,1,1,1,1,1,1,1,1,1,1,1,1,4),(72.2566310325655,
72.9007613138617,73.3995929223035,73.8984245307453,74.397256139187,74.8960877476288,
75.3949193560706,75.8937509645124,76.3925825729542,76.891414181396,77.3902457898378,
77.8890773982795,78.3879090067213,78.5398163397451),.UNSPECIFIED.);
#388=B_SPLINE_CURVE_WITH_KNOTS('',3,(#44677,#44678,#44679,#44680,#44681,
#44682,#44683,#44684,#44685,#44686,#44687,#44688,#44689,#44690,#44691,#44692,
#44693),.UNSPECIFIED.,.F.,.F.,(4,1,1,1,1,1,1,1,1,1,1,1,1,1,4),(72.2566310325657,
72.4808320784257,72.9807789867106,73.4807258949954,73.9806728032802,74.4806197115651,
74.98056661985,75.4805135281348,75.9804604364196,76.4804073447045,76.9803542529893,
77.4803011612742,77.980248069559,78.4801949778438,78.5398163397452),
 .UNSPECIFIED.);
#389=B_SPLINE_CURVE_WITH_KNOTS('',3,(#44698,#44699,#44700,#44701,#44702,
#44703,#44704,#44705,#44706,#44707,#44708,#44709,#44710,#44711,#44712,#44713),
 .UNSPECIFIED.,.F.,.F.,(4,1,1,1,1,1,1,1,1,1,1,1,1,4),(65.9734457253859,
66.4159504041185,66.9147820125603,67.4136136210021,67.9124452294438,68.4112768378856,
68.9101084463274,69.4089400547692,69.907771663211,70.4066032716528,70.9054348800946,
71.4042664885363,71.9030980969781,72.2566310325655),.UNSPECIFIED.);
#390=B_SPLINE_CURVE_WITH_KNOTS('',3,(#44714,#44715,#44716,#44717,#44718,
#44719,#44720,#44721,#44722,#44723,#44724,#44725,#44726,#44727,#44728,#44729,
#44730),.UNSPECIFIED.,.F.,.F.,(4,1,1,1,1,1,1,1,1,1,1,1,1,1,4),(65.973445725386,
65.9815222707228,66.4814691790076,66.9814160872924,67.4813629955773,67.9813099038621,
68.481256812147,68.9812037204318,69.4811506287167,69.9810975370015,70.4810444452864,
70.9809913535712,71.480938261856,71.9808851701409,72.2566310325657),
 .UNSPECIFIED.);
#391=B_SPLINE_CURVE_WITH_KNOTS('',3,(#44735,#44736,#44737,#44738,#44739,
#44740,#44741,#44742,#44743,#44744,#44745,#44746,#44747,#44748,#44749,#44750),
 .UNSPECIFIED.,.F.,.F.,(4,1,1,1,1,1,1,1,1,1,1,1,1,4),(59.6902604182064,
59.9311394943753,60.4299711028171,60.9288027112589,61.4276343197006,61.9264659281424,
62.4252975365842,62.924129145026,63.4229607534678,63.9217923619096,64.4206239703514,
64.9194555787931,65.9171187956767,65.9734457253859),.UNSPECIFIED.);
#392=B_SPLINE_CURVE_WITH_KNOTS('',3,(#44751,#44752,#44753,#44754,#44755,
#44756,#44757,#44758,#44759,#44760,#44761,#44762,#44763,#44764,#44765,#44766),
 .UNSPECIFIED.,.F.,.F.,(4,1,1,1,1,1,1,1,1,1,1,1,1,4),(59.6902604182065,
59.9821593713046,60.4821062795895,60.9820531878743,61.4820000961592,61.981947004444,
62.4818939127289,62.9818408210137,63.4817877292985,63.9817346375834,64.4816815458682,
64.9816284541531,65.4815753624379,65.973445725386),.UNSPECIFIED.);
#393=B_SPLINE_CURVE_WITH_KNOTS('',3,(#44771,#44772,#44773,#44774,#44775,
#44776,#44777,#44778,#44779,#44780,#44781,#44782,#44783,#44784,#44785,#44786),
 .UNSPECIFIED.,.F.,.F.,(4,1,1,1,1,1,1,1,1,1,1,1,1,4),(53.4070751110267,
53.4463285846321,53.9451601930739,54.4439918015157,54.9428234099574,55.4416550183992,
55.940486626841,56.4393182352828,56.9381498437246,57.4369814521664,57.9358130606082,
58.9334762774917,59.4323078859335,59.6902604182064),.UNSPECIFIED.);
#394=B_SPLINE_CURVE_WITH_KNOTS('',3,(#44787,#44788,#44789,#44790,#44791,
#44792,#44793,#44794,#44795,#44796,#44797,#44798,#44799,#44800,#44801,#44802,
#44803),.UNSPECIFIED.,.F.,.F.,(4,1,1,1,1,1,1,1,1,1,1,1,1,1,4),(53.4070751110269,
53.4828495636017,53.9827964718865,54.4827433801714,54.9826902884562,55.4826371967411,
55.9825841050259,56.4825310133107,56.9824779215956,57.4824248298804,57.9823717381653,
58.4823186464501,58.982265554735,59.4822124630198,59.6902604182065),
 .UNSPECIFIED.);
#395=B_SPLINE_CURVE_WITH_KNOTS('',3,(#44808,#44809,#44810,#44811,#44812,
#44813,#44814,#44815,#44816,#44817,#44818,#44819,#44820,#44821,#44822),
 .UNSPECIFIED.,.F.,.F.,(4,1,1,1,1,1,1,1,1,1,1,1,4),(47.1238898038472,47.4603492833307,
47.9591808917725,48.4580125002142,48.956844108656,49.4556757170978,49.9545073255396,
50.4533389339814,50.9521705424232,51.9498337593067,52.4486653677485,52.9474969761903,
53.4070751110267),.UNSPECIFIED.);
#396=B_SPLINE_CURVE_WITH_KNOTS('',3,(#44823,#44824,#44825,#44826,#44827,
#44828,#44829,#44830,#44831,#44832,#44833,#44834,#44835,#44836,#44837,#44838),
 .UNSPECIFIED.,.F.,.F.,(4,1,1,1,1,1,1,1,1,1,1,1,1,4),(47.1238898038473,
47.4834866641836,47.9834335724684,48.4833804807532,48.9833273890381,49.4832742973229,
49.9832212056078,50.4831681138926,50.9831150221775,51.4830619304623,51.9830088387471,
52.482955747032,52.9829026553168,53.4070751110269),.UNSPECIFIED.);
#397=B_SPLINE_CURVE_WITH_KNOTS('',3,(#44843,#44844,#44845,#44846,#44847,
#44848,#44849,#44850,#44851,#44852,#44853,#44854,#44855,#44856,#44857,#44858),
 .UNSPECIFIED.,.F.,.F.,(4,1,1,1,1,1,1,1,1,1,1,1,1,4),(40.8407044966676,
40.9755383735875,41.4743699820293,41.973201590471,42.4720331989128,42.9708648073546,
43.4696964157964,43.9685280242382,44.9661912411217,45.4650228495635,45.9638544580053,
46.4626860664471,46.9615176748889,47.1238898038472),.UNSPECIFIED.);
#398=B_SPLINE_CURVE_WITH_KNOTS('',3,(#44859,#44860,#44861,#44862,#44863,
#44864,#44865,#44866,#44867,#44868,#44869,#44870,#44871,#44872,#44873,#44874,
#44875),.UNSPECIFIED.,.F.,.F.,(4,1,1,1,1,1,1,1,1,1,1,1,1,1,4),(40.8407044966677,
40.9841768564806,41.4841237647654,41.9840706730503,42.4840175813351,42.98396448962,
43.4839113979048,43.9838583061896,44.4838052144745,44.9837521227593,45.4836990310442,
45.983645939329,46.4835928476139,46.9835397558987,47.1238898038473),
 .UNSPECIFIED.);
#399=B_SPLINE_CURVE_WITH_KNOTS('',3,(#44880,#44881,#44882,#44883,#44884,
#44885,#44886,#44887,#44888,#44889,#44890,#44891,#44892,#44893,#44894),
 .UNSPECIFIED.,.F.,.F.,(4,1,1,1,1,1,1,1,1,1,1,1,4),(34.557519189488,34.9895590722861,
35.4883906807278,35.9872222891696,36.4860538976114,36.9848855060532,37.9825487229368,
38.4813803313785,38.9802119398203,39.4790435482621,39.9778751567039,40.4767067651457,
40.8407044966676),.UNSPECIFIED.);
#400=B_SPLINE_CURVE_WITH_KNOTS('',3,(#44895,#44896,#44897,#44898,#44899,
#44900,#44901,#44902,#44903,#44904,#44905,#44906,#44907,#44908,#44909,#44910),
 .UNSPECIFIED.,.F.,.F.,(4,1,1,1,1,1,1,1,1,1,1,1,1,4),(34.5575191894881,
34.9848139570625,35.4847608653473,35.9847077736322,36.484654681917,36.9846015902018,
37.4845484984867,37.9844954067715,38.4844423150564,38.9843892233412,39.4843361316261,
39.9842830399109,40.4842299481957,40.8407044966677),.UNSPECIFIED.);
#401=B_SPLINE_CURVE_WITH_KNOTS('',3,(#44915,#44916,#44917,#44918,#44919,
#44920,#44921,#44922,#44923,#44924,#44925,#44926,#44927,#44928,#44929,#44930),
 .UNSPECIFIED.,.F.,.F.,(4,1,1,1,1,1,1,1,1,1,1,1,1,4),(28.2743338823084,
28.5047481625429,29.0035797709846,29.5024113794264,30.0012429878682,30.9989062047518,
31.4977378131936,31.9965694216353,32.4954010300771,32.9942326385189,33.4930642469607,
33.9918958554025,34.4907274638443,34.557519189488),.UNSPECIFIED.);
#402=B_SPLINE_CURVE_WITH_KNOTS('',3,(#44931,#44932,#44933,#44934,#44935,
#44936,#44937,#44938,#44939,#44940,#44941,#44942,#44943,#44944,#44945,#44946,
#44947),.UNSPECIFIED.,.F.,.F.,(4,1,1,1,1,1,1,1,1,1,1,1,1,1,4),(28.2743338823085,
28.4855041493595,28.9854510576443,29.4853979659292,29.985344874214,30.4852917824989,
30.9852386907837,31.4851855990686,31.9851325073534,32.4850794156383,32.9850263239231,
33.4849732322079,33.9849201404928,34.4848670487776,34.5575191894881),
 .UNSPECIFIED.);
#403=B_SPLINE_CURVE_WITH_KNOTS('',3,(#44952,#44953,#44954,#44955,#44956,
#44957,#44958,#44959,#44960,#44961,#44962,#44963,#44964,#44965,#44966,#44967),
 .UNSPECIFIED.,.F.,.F.,(4,1,1,1,1,1,1,1,1,1,1,1,1,4),(21.9911485751288,
22.0199372527997,22.5187688612414,23.0176004696832,24.0152636865668,24.5140952950086,
25.0129269034504,25.5117585118921,26.0105901203339,26.5094217287757,27.0082533372175,
27.5070849456593,28.0059165541011,28.2743338823084),.UNSPECIFIED.);
#404=B_SPLINE_CURVE_WITH_KNOTS('',3,(#44968,#44969,#44970,#44971,#44972,
#44973,#44974,#44975,#44976,#44977,#44978,#44979,#44980,#44981,#44982,#44983),
 .UNSPECIFIED.,.F.,.F.,(4,1,1,1,1,1,1,1,1,1,1,1,1,4),(21.9911485751289,
22.4861412499414,22.9860881582262,23.4860350665111,23.9859819747959,24.4859288830808,
24.9858757913656,25.4858226996504,25.9857696079353,26.4857165162201,26.985663424505,
27.4856103327898,27.9855572410747,28.2743338823085),.UNSPECIFIED.);
#405=B_SPLINE_CURVE_WITH_KNOTS('',3,(#44988,#44989,#44990,#44991,#44992,
#44993,#44994,#44995,#44996,#44997,#44998,#44999,#45000,#45001,#45002),
 .UNSPECIFIED.,.F.,.F.,(4,1,1,1,1,1,1,1,1,1,1,1,4),(15.7079632679492,16.0339579514982,
17.0316211683818,17.5304527768236,18.0292843852654,18.5281159937072,19.0269476021489,
19.5257792105907,20.0246108190325,20.5234424274743,21.0222740359161,21.5211056443579,
21.9911485751288),.UNSPECIFIED.);
#406=B_SPLINE_CURVE_WITH_KNOTS('',3,(#45003,#45004,#45005,#45006,#45007,
#45008,#45009,#45010,#45011,#45012,#45013,#45014,#45015,#45016,#45017,#45018,
#45019),.UNSPECIFIED.,.F.,.F.,(4,1,1,1,1,1,1,1,1,1,1,1,1,1,4),(15.7079632679493,
15.9868314422384,16.4867783505233,16.9867252588081,17.4866721670929,17.9866190753778,
18.4865659836626,18.9865128919475,19.4864598002323,19.9864067085172,20.486353616802,
20.9863005250869,21.4862474333717,21.9861943416565,21.9911485751289),
 .UNSPECIFIED.);
#407=B_SPLINE_CURVE_WITH_KNOTS('',3,(#45052,#45053,#45054,#45055,#45056,
#45057,#45058,#45059,#45060,#45061,#45062,#45063,#45064,#45065,#45066,#45067,
#45068,#45069,#45070,#45071,#45072,#45073,#45074,#45075,#45076,#45077,#45078,
#45079,#45080,#45081,#45082,#45083,#45084,#45085,#45086,#45087,#45088,#45089,
#45090,#45091,#45092,#45093,#45094,#45095,#45096,#45097,#45098,#45099,#45100,
#45101,#45102,#45103,#45104,#45105,#45106,#45107,#45108,#45109,#45110,#45111,
#45112),.UNSPECIFIED.,.F.,.F.,(4,3,3,3,3,3,3,3,3,3,3,3,3,3,3,3,3,3,3,3,
4),(-1.70371038777376,-1.57164896760842,-1.45968081939285,-1.42104956412851,
-1.38937747141726,-1.25766313377658,-1.18516797863899,-1.14888374991031,
-1.11514150461779,-0.984197499563139,-0.967682513226223,-0.845964405260809,
-0.78525894660507,-0.754188806238284,-0.728523041048962,-0.598532726708555,
-0.480810081364569,-0.419431608816291,-0.381410915251877,-0.356693156275484,
-0.245712839762795),.UNSPECIFIED.);
#408=B_SPLINE_CURVE_WITH_KNOTS('',3,(#45114,#45115,#45116,#45117,#45118,
#45119,#45120,#45121,#45122,#45123,#45124,#45125,#45126,#45127,#45128,#45129,
#45130,#45131,#45132,#45133,#45134,#45135,#45136,#45137,#45138,#45139,#45140,
#45141,#45142,#45143,#45144,#45145,#45146,#45147,#45148,#45149,#45150,#45151,
#45152,#45153,#45154,#45155,#45156,#45157,#45158,#45159,#45160,#45161,#45162),
 .UNSPECIFIED.,.F.,.F.,(4,3,3,3,3,3,3,3,3,3,3,3,3,3,3,3,4),(-1.16887606902948,
-1.04801251096666,-0.994206397697257,-0.946140023287794,-0.815780930032988,
-0.781046175157294,-0.751089839681922,-0.685421836778182,-0.554489283265102,
-0.46425321950904,-0.415674365158631,-0.389975975593583,-0.362776987536873,
-0.230336045464461,-0.193545028240855,-0.0612057741671412,-5.34073745228555E-5),
 .UNSPECIFIED.);
#409=B_SPLINE_CURVE_WITH_KNOTS('',3,(#47153,#47154,#47155,#47156,#47157,
#47158,#47159,#47160,#47161,#47162,#47163,#47164,#47165,#47166,#47167,#47168,
#47169,#47170,#47171,#47172,#47173,#47174),.UNSPECIFIED.,.F.,.F.,(4,3,3,
3,3,3,3,4),(-1.73957725076382,-1.61100415945136,-1.52396281589798,-1.48243222042214,
-1.45665092794175,-1.32808793138577,-1.26283878523785,-1.15068998546189),
 .UNSPECIFIED.);
#410=B_SPLINE_CURVE_WITH_KNOTS('',3,(#47175,#47176,#47177,#47178,#47179,
#47180,#47181,#47182,#47183,#47184,#47185,#47186,#47187,#47188,#47189,#47190,
#47191,#47192,#47193,#47194,#47195,#47196,#47197,#47198,#47199,#47200,#47201,
#47202,#47203,#47204,#47205,#47206,#47207,#47208),.UNSPECIFIED.,.F.,.F.,
(4,3,3,3,3,3,3,3,3,3,3,4),(-0.878140325105598,-0.777511794155485,-0.671462782584743,
-0.631586372873439,-0.604605941415006,-0.565413771014002,-0.456171084017733,
-0.390222098706532,-0.365207136260434,-0.340281065404979,-0.223557747407252,
-0.210417151407702),.UNSPECIFIED.);
#411=B_SPLINE_CURVE_WITH_KNOTS('',3,(#47210,#47211,#47212,#47213,#47214,
#47215,#47216,#47217,#47218,#47219,#47220),.UNSPECIFIED.,.F.,.F.,(4,1,1,
1,1,1,1,1,4),(12.043305083964,12.5421366924057,13.0409683008475,13.5397999092893,
14.0386315177311,14.5374631261729,15.0362947346147,15.5351263430564,15.7079632679492),
 .UNSPECIFIED.);
#412=B_SPLINE_CURVE_WITH_KNOTS('',3,(#47221,#47222,#47223,#47224,#47225,
#47226,#47227,#47228,#47229,#47230,#47231,#47232,#47233,#47234,#47235,#47236,
#47237,#47238,#47239,#47240,#47241,#47242,#47243,#47244,#47245,#47246,#47247,
#47248,#47249,#47250,#47251,#47252,#47253,#47254),.UNSPECIFIED.,.F.,.F.,
(4,3,3,3,3,3,3,3,3,3,3,4),(-0.873477877141213,-0.753141137816717,-0.635235160226647,
-0.592041969943734,-0.557997950910165,-0.446311798303827,-0.427982605240538,
-0.320986953930404,-0.284657590233497,-0.180950825577172,-0.0805654152611678,
0.),.UNSPECIFIED.);
#413=B_SPLINE_CURVE_WITH_KNOTS('',3,(#47255,#47256,#47257,#47258,#47259,
#47260,#47261,#47262,#47263,#47264,#47265,#47266,#47267,#47268,#47269,#47270,
#47271,#47272,#47273,#47274,#47275,#47276),.UNSPECIFIED.,.F.,.F.,(4,3,3,
3,3,3,3,4),(-264.186463227569,-263.881920865704,-263.383089257262,-262.884257648821,
-262.385426040379,-261.886594431937,-261.387762823495,-261.275255778348),
 .UNSPECIFIED.);
#414=B_SPLINE_CURVE_WITH_KNOTS('',3,(#47279,#47280,#47281,#47282,#47283,
#47284,#47285,#47286,#47287,#47288,#47289,#47290,#47291,#47292,#47293,#47294,
#47295,#47296,#47297),.UNSPECIFIED.,.F.,.F.,(4,3,3,3,3,3,4),(-1.43852457462426,
-1.3094245422137,-1.20010961474172,-1.15249379404292,-1.12530519830466,
-0.998964743453856,-0.966035327470543),.UNSPECIFIED.);
#415=B_SPLINE_CURVE_WITH_KNOTS('',3,(#47300,#47301,#47302,#47303,#47304,
#47305,#47306,#47307,#47308,#47309,#47310,#47311,#47312,#47313,#47314,#47315,
#47316,#47317,#47318,#47319,#47320,#47321,#47322,#47323,#47324,#47325,#47326,
#47327),.UNSPECIFIED.,.F.,.F.,(4,3,3,3,3,3,3,3,3,4),(-0.664303123679825,
-0.600044533881661,-0.572382428837333,-0.460522004544073,-0.429002315709467,
-0.3217517367821,-0.284511301345448,-0.180801420460334,-0.0803981151576599,
0.),.UNSPECIFIED.);
#416=B_SPLINE_CURVE_WITH_KNOTS('',3,(#49452,#49453,#49454,#49455,#49456,
#49457,#49458,#49459,#49460,#49461,#49462,#49463,#49464,#49465,#49466,#49467,
#49468,#49469,#49470,#49471,#49472,#49473,#49474,#49475,#49476,#49477,#49478,
#49479,#49480,#49481,#49482,#49483,#49484,#49485),.UNSPECIFIED.,.F.,.F.,
(4,3,3,3,3,3,3,3,3,3,3,4),(258.047800828882,258.472551583264,258.972498491549,
259.472445399834,259.972392308118,260.472339216403,260.972286124688,261.472233032973,
261.972179941258,262.472126849543,262.972073757828,263.226194462655),
 .UNSPECIFIED.);
#417=B_SPLINE_CURVE_WITH_KNOTS('',3,(#49487,#49488,#49489,#49490,#49491,
#49492,#49493,#49494,#49495,#49496,#49497,#49498,#49499,#49500,#49501,#49502,
#49503,#49504,#49505,#49506,#49507,#49508,#49509,#49510,#49511,#49512,#49513,
#49514,#49515,#49516,#49517,#49518,#49519,#49520,#49521,#49522,#49523),
 .UNSPECIFIED.,.F.,.F.,(4,3,3,3,3,3,3,3,3,3,3,3,4),(-0.878140325105315,
-0.777010465777669,-0.703471476437966,-0.636654823290452,-0.609982353575103,
-0.500671075341767,-0.483381692174221,-0.406298397291394,-0.367627872926269,
-0.343047565778001,-0.226089388522165,-0.105578325200182,0.),
 .UNSPECIFIED.);
#418=B_SPLINE_CURVE_WITH_KNOTS('',3,(#49524,#49525,#49526,#49527,#49528,
#49529,#49530,#49531,#49532,#49533,#49534,#49535,#49536,#49537,#49538,#49539),
 .UNSPECIFIED.,.F.,.F.,(4,1,1,1,1,1,1,1,1,1,1,1,1,4),(9.94784349116542,
9.98746854282029,10.4874154511051,10.98736235939,11.4873092676748,11.9872561759597,
12.4872030842445,12.9871499925294,13.4870969008142,13.987043809099,14.4869907173839,
14.9869376256687,15.4868845339536,15.7079632679493),.UNSPECIFIED.);
#419=B_SPLINE_CURVE_WITH_KNOTS('',3,(#49557,#49558,#49559,#49560,#49561,
#49562,#49563,#49564,#49565,#49566,#49567,#49568,#49569,#49570,#49571,#49572,
#49573,#49574),.UNSPECIFIED.,.F.,.F.,(4,2,2,2,2,2,2,2,4),(0.,0.0946120580087934,
0.189224116017587,0.283822945575014,0.378421775132442,0.473020604689869,
0.567619434247297,0.66223149225609,0.756843550264884),.UNSPECIFIED.);
#420=B_SPLINE_CURVE_WITH_KNOTS('',3,(#49585,#49586,#49587,#49588,#49589,
#49590,#49591,#49592,#49593,#49594,#49595,#49596,#49597,#49598,#49599,#49600,
#49601,#49602),.UNSPECIFIED.,.F.,.F.,(4,2,2,2,2,2,2,2,4),(-0.756843550264884,
-0.66223149225609,-0.567619434247297,-0.47302060468987,-0.378421775132442,
-0.283822945575015,-0.189224116017587,-0.0946120580087935,0.),
 .UNSPECIFIED.);
#421=B_SPLINE_CURVE_WITH_KNOTS('',3,(#49844,#49845,#49846,#49847,#49848,
#49849,#49850,#49851,#49852,#49853,#49854,#49855,#49856,#49857,#49858,#49859,
#49860,#49861),.UNSPECIFIED.,.F.,.F.,(4,2,2,2,2,2,2,2,4),(0.,0.33755490943604,
0.675109818872081,1.01195490866249,1.34879999845289,1.6856450882433,2.02249017803371,
2.36004508746975,2.69759999690579),.UNSPECIFIED.);
#422=B_SPLINE_CURVE_WITH_KNOTS('',3,(#49862,#49863,#49864,#49865,#49866,
#49867,#49868,#49869,#49870,#49871,#49872,#49873,#49874,#49875,#49876,#49877,
#49878,#49879),.UNSPECIFIED.,.F.,.F.,(4,2,2,2,2,2,2,2,4),(2.69759999690579,
3.03515490634183,3.37270981577787,3.70955490556828,4.04639999535868,4.38324508514909,
4.72009017493949,5.05764508437554,5.39519999381158),.UNSPECIFIED.);
#423=B_SPLINE_CURVE_WITH_KNOTS('',3,(#49882,#49883,#49884,#49885,#49886,
#49887,#49888,#49889,#49890,#49891,#49892,#49893,#49894,#49895,#49896,#49897,
#49898,#49899),.UNSPECIFIED.,.F.,.F.,(4,2,2,2,2,2,2,2,4),(0.,0.337554909436041,
0.675109818872083,1.01195490866249,1.34879999845289,1.6856450882433,2.0224901780337,
2.36004508746974,2.69759999690578),.UNSPECIFIED.);
#424=B_SPLINE_CURVE_WITH_KNOTS('',3,(#49900,#49901,#49902,#49903,#49904,
#49905,#49906,#49907,#49908,#49909,#49910,#49911,#49912,#49913,#49914,#49915,
#49916,#49917),.UNSPECIFIED.,.F.,.F.,(4,2,2,2,2,2,2,2,4),(2.69759999690578,
3.03515490634183,3.37270981577787,3.70955490556827,4.04639999535868,4.38324508514908,
4.72009017493949,5.05764508437553,5.39519999381157),.UNSPECIFIED.);
#425=B_SPLINE_CURVE_WITH_KNOTS('',3,(#49920,#49921,#49922,#49923,#49924,
#49925,#49926,#49927,#49928,#49929,#49930,#49931,#49932,#49933,#49934,#49935,
#49936,#49937),.UNSPECIFIED.,.F.,.F.,(4,2,2,2,2,2,2,2,4),(0.,0.337554909436041,
0.675109818872081,1.01195490866249,1.3487999984529,1.6856450882433,2.02249017803371,
2.36004508746975,2.69759999690579),.UNSPECIFIED.);
#426=B_SPLINE_CURVE_WITH_KNOTS('',3,(#49938,#49939,#49940,#49941,#49942,
#49943,#49944,#49945,#49946,#49947,#49948,#49949,#49950,#49951,#49952,#49953,
#49954,#49955),.UNSPECIFIED.,.F.,.F.,(4,2,2,2,2,2,2,2,4),(2.69759999690579,
3.03515490634183,3.37270981577787,3.70955490556828,4.04639999535869,4.3832450851491,
4.7200901749395,5.05764508437554,5.39519999381158),.UNSPECIFIED.);
#427=B_SPLINE_CURVE_WITH_KNOTS('',3,(#49958,#49959,#49960,#49961,#49962,
#49963,#49964,#49965,#49966,#49967,#49968,#49969,#49970,#49971,#49972,#49973,
#49974,#49975),.UNSPECIFIED.,.F.,.F.,(4,2,2,2,2,2,2,2,4),(0.,0.337554909436041,
0.675109818872081,1.01195490866249,1.3487999984529,1.6856450882433,2.02249017803371,
2.36004508746975,2.69759999690579),.UNSPECIFIED.);
#428=B_SPLINE_CURVE_WITH_KNOTS('',3,(#49976,#49977,#49978,#49979,#49980,
#49981,#49982,#49983,#49984,#49985,#49986,#49987,#49988,#49989,#49990,#49991,
#49992,#49993),.UNSPECIFIED.,.F.,.F.,(4,2,2,2,2,2,2,2,4),(2.69759999690579,
3.03515490634183,3.37270981577787,3.70955490556828,4.04639999535869,4.3832450851491,
4.72009017493951,5.05764508437555,5.39519999381159),.UNSPECIFIED.);
#429=B_SPLINE_CURVE_WITH_KNOTS('',3,(#50065,#50066,#50067,#50068,#50069,
#50070,#50071,#50072,#50073,#50074,#50075,#50076,#50077,#50078,#50079,#50080),
 .UNSPECIFIED.,.F.,.F.,(4,2,2,2,2,2,2,4),(-4.30443928379571,-4.2860545404295,
-4.18302089376354,-4.02031324727212,-3.73577474040229,-3.47881030687683,
-3.26117067957846,-3.22870524423984),.UNSPECIFIED.);
#430=B_SPLINE_CURVE_WITH_KNOTS('',3,(#50082,#50083,#50084,#50085,#50086,
#50087,#50088,#50089,#50090,#50091,#50092,#50093,#50094,#50095),
 .UNSPECIFIED.,.F.,.F.,(4,2,2,2,2,2,4),(-1.07597467085911,-1.02250399542755,
-0.791813858983204,-0.526066025069406,-0.242334063735881,-0.0987908890199728,
0.),.UNSPECIFIED.);
#431=B_SPLINE_CURVE_WITH_KNOTS('',3,(#50096,#50097,#50098,#50099,#50100,
#50101,#50102,#50103,#50104,#50105,#50106,#50107,#50108,#50109,#50110,#50111,
#50112,#50113,#50114,#50115,#50116,#50117,#50118,#50119),.UNSPECIFIED.,
 .F.,.F.,(4,2,2,2,2,2,2,2,2,2,2,4),(-3.22870524423984,-3.04034029687005,
-2.77983245466332,-2.48572420120637,-2.29812682077172,-2.18914179422406,
-2.09440056074871,-1.97639597697234,-1.7640763751916,-1.47308567187965,
-1.23740056701131,-1.07597467085911),.UNSPECIFIED.);
#432=B_SPLINE_CURVE_WITH_KNOTS('',3,(#50124,#50125,#50126,#50127,#50128,
#50129,#50130,#50131,#50132,#50133,#50134,#50135,#50136,#50137,#50138,#50139),
 .UNSPECIFIED.,.F.,.F.,(4,2,2,2,2,2,2,4),(-4.30443928376566,-4.28605454039955,
-4.18302089373508,-4.02031324724582,-3.73577474037948,-3.47881030685707,
-3.2611706795612,-3.22870524422297),.UNSPECIFIED.);
#433=B_SPLINE_CURVE_WITH_KNOTS('',3,(#50141,#50142,#50143,#50144,#50145,
#50146,#50147,#50148,#50149,#50150,#50151,#50152,#50153,#50154),
 .UNSPECIFIED.,.F.,.F.,(4,2,2,2,2,2,4),(-1.07597467085728,-1.02250399542586,
-0.791813858982145,-0.526066025068897,-0.242334063735757,-0.0987908890199458,
0.),.UNSPECIFIED.);
#434=B_SPLINE_CURVE_WITH_KNOTS('',3,(#50155,#50156,#50157,#50158,#50159,
#50160,#50161,#50162,#50163,#50164,#50165,#50166,#50167,#50168,#50169,#50170,
#50171,#50172,#50173,#50174,#50175,#50176,#50177,#50178),.UNSPECIFIED.,
 .F.,.F.,(4,2,2,2,2,2,2,2,2,2,2,4),(-3.22870524422297,-3.0403402968552,
-2.7798324546511,-2.48572420119689,-2.29812682076393,-2.18914179421705,
-2.09440056074233,-1.97639597696673,-1.76407637518704,-1.47308567187632,
-1.23740056700891,-1.07597467085728),.UNSPECIFIED.);
#435=B_SPLINE_CURVE_WITH_KNOTS('',3,(#50183,#50184,#50185,#50186,#50187,
#50188,#50189,#50190,#50191,#50192,#50193,#50194,#50195,#50196,#50197,#50198),
 .UNSPECIFIED.,.F.,.F.,(4,2,2,2,2,2,2,4),(-4.30443928371459,-4.28605454034862,
-4.18302089368667,-4.02031324720125,-3.73577474034113,-3.47881030682397,
-3.2611706795323,-3.22870524419465),.UNSPECIFIED.);
#436=B_SPLINE_CURVE_WITH_KNOTS('',3,(#50200,#50201,#50202,#50203,#50204,
#50205,#50206,#50207,#50208,#50209,#50210,#50211,#50212,#50213),
 .UNSPECIFIED.,.F.,.F.,(4,2,2,2,2,2,4),(-1.07597467085434,-1.02250399542317,
-0.791813858980425,-0.526066025068098,-0.242334063735552,-0.098790889019902,
0.),.UNSPECIFIED.);
#437=B_SPLINE_CURVE_WITH_KNOTS('',3,(#50214,#50215,#50216,#50217,#50218,
#50219,#50220,#50221,#50222,#50223,#50224,#50225,#50226,#50227,#50228,#50229,
#50230,#50231,#50232,#50233,#50234,#50235,#50236,#50237),.UNSPECIFIED.,
 .F.,.F.,(4,2,2,2,2,2,2,2,2,2,2,4),(-3.22870524419465,-3.04034029683025,
-2.77983245463047,-2.48572420118091,-2.2981268207507,-2.18914179420531,
-2.09440056073169,-1.97639597695723,-1.76407637517944,-1.47308567187093,
-1.23740056700507,-1.07597467085434),.UNSPECIFIED.);
#438=B_SPLINE_CURVE_WITH_KNOTS('',3,(#50242,#50243,#50244,#50245,#50246,
#50247,#50248,#50249,#50250,#50251,#50252,#50253,#50254,#50255,#50256,#50257),
 .UNSPECIFIED.,.F.,.F.,(4,2,2,2,2,2,2,4),(-4.30443928358367,-4.28605454021807,
-4.18302089356202,-4.02031324708534,-3.73577474023997,-3.47881030673541,
-3.26117067945383,-3.22870524411765),.UNSPECIFIED.);
#439=B_SPLINE_CURVE_WITH_KNOTS('',3,(#50259,#50260,#50261,#50262,#50263,
#50264,#50265,#50266,#50267,#50268,#50269,#50270,#50271,#50272),
 .UNSPECIFIED.,.F.,.F.,(4,2,2,2,2,2,4),(-1.07597467084362,-1.02250399541335,
-0.791813858973979,-0.526066025064686,-0.242334063734663,-0.0987908890197505,
0.),.UNSPECIFIED.);
#440=B_SPLINE_CURVE_WITH_KNOTS('',3,(#50273,#50274,#50275,#50276,#50277,
#50278,#50279,#50280,#50281,#50282,#50283,#50284,#50285,#50286,#50287,#50288,
#50289,#50290,#50291,#50292,#50293,#50294,#50295,#50296),.UNSPECIFIED.,
 .F.,.F.,(4,2,2,2,2,2,2,2,2,2,2,4),(-3.22870524411765,-3.04034029676145,
-2.77983245457245,-2.48572420113423,-2.29812682071072,-2.18914179416892,
-2.0944005606982,-1.976395976927,-1.76407637515459,-1.47308567185275,-1.23740056699153,
-1.07597467084362),.UNSPECIFIED.);
#441=B_SPLINE_CURVE_WITH_KNOTS('',3,(#50317,#50318,#50319,#50320,#50321,
#50322,#50323,#50324,#50325,#50326),.UNSPECIFIED.,.F.,.F.,(4,3,3,4),(-4.09274904019425,
-3.96636136242185,-2.97477102181639,-2.06120159751579),.UNSPECIFIED.);
#442=B_SPLINE_CURVE_WITH_KNOTS('',3,(#50329,#50330,#50331,#50332,#50333,
#50334,#50335),.UNSPECIFIED.,.F.,.F.,(4,3,4),(0.,0.991590340605456,1.11004521091126),
 .UNSPECIFIED.);
#443=B_SPLINE_CURVE_WITH_KNOTS('',3,(#50340,#50341,#50342,#50343,#50344,
#50345,#50346,#50347,#50348,#50349,#50350,#50351,#50352,#50353,#50354,#50355,
#50356,#50357,#50358,#50359,#50360,#50361),.UNSPECIFIED.,.F.,.F.,(4,3,3,
3,3,3,3,4),(-10.3759343473738,-9.91590340605462,-8.92431306544916,-7.9327227248437,
-6.94113238423824,-5.94954204363277,-4.95795170302731,-4.09274904019425),
 .UNSPECIFIED.);
#444=B_SPLINE_CURVE_WITH_KNOTS('',3,(#50362,#50363,#50364,#50365,#50366,
#50367,#50368,#50369,#50370,#50371,#50372,#50373,#50374,#50375,#50376,#50377,
#50378,#50379,#50380,#50381,#50382,#50383),.UNSPECIFIED.,.F.,.F.,(4,3,3,
3,3,3,3,4),(1.11004521091126,1.98318068121092,2.97477102181639,3.96636136242185,
4.95795170302731,5.94954204363278,6.94113238423824,7.39323051809085),
 .UNSPECIFIED.);
#445=B_SPLINE_CURVE_WITH_KNOTS('',3,(#50388,#50389,#50390,#50391,#50392,
#50393,#50394,#50395,#50396,#50397,#50398,#50399,#50400,#50401,#50402,#50403,
#50404,#50405,#50406,#50407,#50408,#50409),.UNSPECIFIED.,.F.,.F.,(4,3,3,
3,3,3,3,4),(-16.6591196545534,-15.8654454496874,-14.8738551090819,-13.8822647684765,
-12.890674427871,-11.8990840872655,-10.9074937466601,-10.3759343473738),
 .UNSPECIFIED.);
#446=B_SPLINE_CURVE_WITH_KNOTS('',3,(#50410,#50411,#50412,#50413,#50414,
#50415,#50416,#50417,#50418,#50419,#50420,#50421,#50422,#50423,#50424,#50425,
#50426,#50427,#50428,#50429,#50430,#50431),.UNSPECIFIED.,.F.,.F.,(4,3,3,
3,3,3,3,4),(7.39323051809085,7.9327227248437,8.92431306544916,9.91590340605462,
10.9074937466601,11.8990840872655,12.890674427871,13.6764158252704),
 .UNSPECIFIED.);
#447=B_SPLINE_CURVE_WITH_KNOTS('',3,(#50436,#50437,#50438,#50439,#50440,
#50441,#50442,#50443,#50444,#50445,#50446,#50447,#50448,#50449,#50450,#50451,
#50452,#50453,#50454,#50455,#50456,#50457,#50458,#50459,#50460),
 .UNSPECIFIED.,.F.,.F.,(4,3,3,3,3,3,3,3,4),(-22.942304961733,-22.8065778339256,
-21.8149874933202,-20.8233971527147,-19.8318068121092,-18.8402164715038,
-17.8486261308983,-16.8570357902929,-16.6591196545534),.UNSPECIFIED.);
#448=B_SPLINE_CURVE_WITH_KNOTS('',3,(#50461,#50462,#50463,#50464,#50465,
#50466,#50467,#50468,#50469,#50470,#50471,#50472,#50473,#50474,#50475,#50476,
#50477,#50478,#50479,#50480,#50481,#50482,#50483,#50484,#50485),
 .UNSPECIFIED.,.F.,.F.,(4,3,3,3,3,3,3,3,4),(13.6764158252704,13.8822647684765,
14.8738551090819,15.8654454496874,16.8570357902929,17.8486261308983,18.8402164715038,
19.8318068121093,19.95960113245),.UNSPECIFIED.);
#449=B_SPLINE_CURVE_WITH_KNOTS('',3,(#50490,#50491,#50492,#50493,#50494,
#50495,#50496,#50497,#50498,#50499,#50500,#50501,#50502,#50503,#50504,#50505,
#50506,#50507,#50508,#50509,#50510,#50511),.UNSPECIFIED.,.F.,.F.,(4,3,3,
3,3,3,3,4),(-29.2254902689126,-28.7561198775584,-27.7645295369529,-26.7729391963475,
-25.781348855742,-24.7897585151366,-23.7981681745311,-22.942304961733),
 .UNSPECIFIED.);
#450=B_SPLINE_CURVE_WITH_KNOTS('',3,(#50512,#50513,#50514,#50515,#50516,
#50517,#50518,#50519,#50520,#50521,#50522,#50523,#50524,#50525,#50526,#50527,
#50528,#50529,#50530,#50531,#50532,#50533),.UNSPECIFIED.,.F.,.F.,(4,3,3,
3,3,3,3,4),(19.95960113245,20.8233971527147,21.8149874933202,22.8065778339256,
23.7981681745311,24.7897585151366,25.781348855742,26.2427864396296),
 .UNSPECIFIED.);
#451=B_SPLINE_CURVE_WITH_KNOTS('',3,(#50538,#50539,#50540,#50541,#50542,
#50543,#50544,#50545,#50546,#50547,#50548,#50549,#50550,#50551,#50552,#50553,
#50554,#50555,#50556,#50557,#50558,#50559),.UNSPECIFIED.,.F.,.F.,(4,3,3,
3,3,3,3,4),(-35.5086755760922,-34.7056619211912,-33.7140715805857,-32.7224812399803,
-31.7308908993748,-30.7393005587693,-29.7477102181639,-29.2254902689126),
 .UNSPECIFIED.);
#452=B_SPLINE_CURVE_WITH_KNOTS('',3,(#50560,#50561,#50562,#50563,#50564,
#50565,#50566,#50567,#50568,#50569,#50570,#50571,#50572,#50573,#50574,#50575,
#50576,#50577,#50578,#50579,#50580,#50581),.UNSPECIFIED.,.F.,.F.,(4,3,3,
3,3,3,3,4),(26.2427864396296,26.7729391963475,27.7645295369529,28.7561198775584,
29.7477102181639,30.7393005587693,31.7308908993748,32.5259717468092),
 .UNSPECIFIED.);
#453=B_SPLINE_CURVE_WITH_KNOTS('',3,(#50586,#50587,#50588,#50589,#50590,
#50591,#50592,#50593,#50594,#50595,#50596,#50597,#50598,#50599,#50600,#50601,
#50602,#50603,#50604,#50605,#50606,#50607,#50608,#50609,#50610),
 .UNSPECIFIED.,.F.,.F.,(4,3,3,3,3,3,3,3,4),(-41.7918608832718,-41.6467943054294,
-40.655203964824,-39.6636136242185,-38.672023283613,-37.6804329430076,-36.6888426024021,
-35.6972522617966,-35.5086755760922),.UNSPECIFIED.);
#454=B_SPLINE_CURVE_WITH_KNOTS('',3,(#50611,#50612,#50613,#50614,#50615,
#50616,#50617,#50618,#50619,#50620,#50621,#50622,#50623,#50624,#50625,#50626,
#50627,#50628,#50629,#50630,#50631,#50632,#50633,#50634,#50635),
 .UNSPECIFIED.,.F.,.F.,(4,3,3,3,3,3,3,3,4),(32.5259717468092,32.7224812399802,
33.7140715805857,34.7056619211912,35.6972522617966,36.6888426024021,37.6804329430076,
38.672023283613,38.8091570539888),.UNSPECIFIED.);
#455=B_SPLINE_CURVE_WITH_KNOTS('',3,(#50640,#50641,#50642,#50643,#50644,
#50645,#50646,#50647,#50648,#50649,#50650,#50651,#50652,#50653,#50654,#50655,
#50656,#50657,#50658,#50659,#50660,#50661),.UNSPECIFIED.,.F.,.F.,(4,3,3,
3,3,3,3,4),(-48.0750461904514,-47.5963363490622,-46.6047460084567,-45.6131556678513,
-44.6215653272458,-43.6299749866404,-42.6383846460349,-41.7918608832718),
 .UNSPECIFIED.);
#456=B_SPLINE_CURVE_WITH_KNOTS('',3,(#50662,#50663,#50664,#50665,#50666,
#50667,#50668,#50669,#50670,#50671,#50672,#50673,#50674,#50675,#50676,#50677,
#50678,#50679,#50680,#50681,#50682,#50683),.UNSPECIFIED.,.F.,.F.,(4,3,3,
3,3,3,3,4),(38.8091570539888,39.6636136242185,40.6552039648239,41.6467943054294,
42.6383846460349,43.6299749866403,44.6215653272458,45.0923423611684),
 .UNSPECIFIED.);
#457=B_SPLINE_CURVE_WITH_KNOTS('',3,(#50688,#50689,#50690,#50691,#50692,
#50693,#50694,#50695,#50696,#50697,#50698,#50699,#50700,#50701,#50702,#50703,
#50704,#50705,#50706,#50707,#50708,#50709),.UNSPECIFIED.,.F.,.F.,(4,3,3,
3,3,3,3,4),(-54.358231497631,-53.545878392695,-52.5542880520895,-51.5626977114841,
-50.5711073708786,-49.5795170302731,-48.5879266896677,-48.0750461904514),
 .UNSPECIFIED.);
#458=B_SPLINE_CURVE_WITH_KNOTS('',3,(#50710,#50711,#50712,#50713,#50714,
#50715,#50716,#50717,#50718,#50719,#50720,#50721,#50722,#50723,#50724,#50725,
#50726,#50727,#50728,#50729,#50730,#50731),.UNSPECIFIED.,.F.,.F.,(4,3,3,
3,3,3,3,4),(45.0923423611684,45.6131556678513,46.6047460084567,47.5963363490622,
48.5879266896676,49.5795170302731,50.5711073708786,51.375527668348),
 .UNSPECIFIED.);
#459=B_SPLINE_CURVE_WITH_KNOTS('',3,(#50736,#50737,#50738,#50739,#50740,
#50741,#50742,#50743,#50744,#50745,#50746,#50747,#50748,#50749,#50750,#50751,
#50752,#50753,#50754,#50755,#50756,#50757,#50758,#50759,#50760),
 .UNSPECIFIED.,.F.,.F.,(4,3,3,3,3,3,3,3,4),(-60.6414168048105,-60.4870107769332,
-59.4954204363278,-58.5038300957223,-57.5122397551168,-56.5206494145114,
-55.5290590739059,-54.5374687333004,-54.358231497631),.UNSPECIFIED.);
#460=B_SPLINE_CURVE_WITH_KNOTS('',3,(#50761,#50762,#50763,#50764,#50765,
#50766,#50767,#50768,#50769,#50770,#50771,#50772,#50773,#50774,#50775,#50776,
#50777,#50778,#50779,#50780,#50781,#50782,#50783,#50784,#50785),
 .UNSPECIFIED.,.F.,.F.,(4,3,3,3,3,3,3,3,4),(51.375527668348,51.562697711484,
52.5542880520895,53.545878392695,54.5374687333004,55.5290590739059,56.5206494145114,
57.5122397551168,57.6587129755276),.UNSPECIFIED.);
#461=B_SPLINE_CURVE_WITH_KNOTS('',3,(#50790,#50791,#50792,#50793,#50794,
#50795,#50796,#50797,#50798,#50799,#50800,#50801,#50802,#50803,#50804,#50805,
#50806,#50807,#50808,#50809,#50810,#50811),.UNSPECIFIED.,.F.,.F.,(4,3,3,
3,3,3,3,4),(-66.9246021119901,-66.436552820566,-65.4449624799605,-64.4533721393551,
-63.4617817987496,-62.4701914581441,-61.4786011175387,-60.6414168048105),
 .UNSPECIFIED.);
#462=B_SPLINE_CURVE_WITH_KNOTS('',3,(#50812,#50813,#50814,#50815,#50816,
#50817,#50818,#50819,#50820,#50821,#50822,#50823,#50824,#50825,#50826,#50827,
#50828,#50829,#50830,#50831,#50832,#50833),.UNSPECIFIED.,.F.,.F.,(4,3,3,
3,3,3,3,4),(57.6587129755276,58.5038300957223,59.4954204363277,60.4870107769332,
61.4786011175387,62.4701914581441,63.4617817987496,63.9418982827072),
 .UNSPECIFIED.);
#463=B_SPLINE_CURVE_WITH_KNOTS('',3,(#50838,#50839,#50840,#50841,#50842,
#50843,#50844,#50845,#50846,#50847,#50848,#50849,#50850,#50851,#50852,#50853,
#50854,#50855,#50856,#50857,#50858,#50859),.UNSPECIFIED.,.F.,.F.,(4,3,3,
3,3,3,3,4),(-73.2077874191697,-72.3860948641988,-71.3945045235933,-70.4029141829878,
-69.4113238423824,-68.4197335017769,-67.4281431611715,-66.9246021119901),
 .UNSPECIFIED.);
#464=B_SPLINE_CURVE_WITH_KNOTS('',3,(#50860,#50861,#50862,#50863,#50864,
#50865,#50866,#50867,#50868,#50869,#50870,#50871,#50872,#50873,#50874,#50875,
#50876,#50877,#50878,#50879,#50880,#50881),.UNSPECIFIED.,.F.,.F.,(4,3,3,
3,3,3,3,4),(63.9418982827072,64.4533721393551,65.4449624799605,66.436552820566,
67.4281431611714,68.4197335017769,69.4113238423824,70.2250835898868),
 .UNSPECIFIED.);
#465=B_SPLINE_CURVE_WITH_KNOTS('',3,(#50886,#50887,#50888,#50889,#50890,
#50891,#50892,#50893,#50894,#50895,#50896,#50897,#50898,#50899,#50900,#50901,
#50902,#50903,#50904,#50905,#50906,#50907,#50908,#50909,#50910),
 .UNSPECIFIED.,.F.,.F.,(4,3,3,3,3,3,3,3,4),(-79.4909727263493,-79.327227248437,
-78.3356369078316,-77.3440465672261,-76.3524562266206,-75.3608658860151,
-74.3692755454097,-73.3776852048042,-73.2077874191697),.UNSPECIFIED.);
#466=B_SPLINE_CURVE_WITH_KNOTS('',3,(#50911,#50912,#50913,#50914,#50915,
#50916,#50917,#50918,#50919,#50920,#50921,#50922,#50923,#50924,#50925,#50926,
#50927,#50928,#50929,#50930,#50931,#50932,#50933,#50934,#50935),
 .UNSPECIFIED.,.F.,.F.,(4,3,3,3,3,3,3,3,4),(70.2250835898868,70.4029141829878,
71.3945045235933,72.3860948641988,73.3776852048042,74.3692755454097,75.3608658860151,
76.3524562266206,76.5082688970663),.UNSPECIFIED.);
#467=B_SPLINE_CURVE_WITH_KNOTS('',3,(#50940,#50941,#50942,#50943,#50944,
#50945,#50946,#50947,#50948,#50949,#50950,#50951,#50952,#50953,#50954,#50955,
#50956,#50957,#50958,#50959,#50960,#50961),.UNSPECIFIED.,.F.,.F.,(4,3,3,
3,3,3,3,4),(-85.7741580335289,-85.2767692920698,-84.2851789514643,-83.2935886108589,
-82.3019982702534,-81.3104079296479,-80.3188175890425,-79.4909727263493),
 .UNSPECIFIED.);
#468=B_SPLINE_CURVE_WITH_KNOTS('',3,(#50962,#50963,#50964,#50965,#50966,
#50967,#50968,#50969,#50970,#50971,#50972,#50973,#50974,#50975,#50976,#50977,
#50978,#50979,#50980,#50981,#50982,#50983),.UNSPECIFIED.,.F.,.F.,(4,3,3,
3,3,3,3,4),(76.5082688970663,77.3440465672261,78.3356369078315,79.327227248437,
80.3188175890425,81.3104079296479,82.3019982702534,82.7914542042459),
 .UNSPECIFIED.);
#469=B_SPLINE_CURVE_WITH_KNOTS('',3,(#50988,#50989,#50990,#50991,#50992,
#50993,#50994,#50995,#50996,#50997,#50998,#50999,#51000,#51001,#51002,#51003,
#51004,#51005,#51006,#51007,#51008,#51009),.UNSPECIFIED.,.F.,.F.,(4,3,3,
3,3,3,3,4),(-92.0573433407085,-91.2263113357026,-90.2347209950971,-89.2431306544916,
-88.2515403138862,-87.2599499732807,-86.2683596326753,-85.7741580335289),
 .UNSPECIFIED.);
#470=B_SPLINE_CURVE_WITH_KNOTS('',3,(#51010,#51011,#51012,#51013,#51014,
#51015,#51016,#51017,#51018,#51019,#51020,#51021,#51022,#51023,#51024,#51025,
#51026,#51027,#51028,#51029,#51030,#51031),.UNSPECIFIED.,.F.,.F.,(4,3,3,
3,3,3,3,4),(82.7914542042459,83.2935886108588,84.2851789514643,85.2767692920698,
86.2683596326752,87.2599499732807,88.2515403138862,89.0746395114255),
 .UNSPECIFIED.);
#471=B_SPLINE_CURVE_WITH_KNOTS('',3,(#51036,#51037,#51038,#51039,#51040,
#51041,#51042,#51043,#51044,#51045,#51046,#51047,#51048,#51049,#51050,#51051,
#51052,#51053,#51054,#51055,#51056,#51057,#51058,#51059,#51060),
 .UNSPECIFIED.,.F.,.F.,(4,3,3,3,3,3,3,3,4),(-98.3405286478881,-98.1674437199408,
-97.1758533793353,-96.1842630387299,-95.1926726981244,-94.201082357519,
-93.2094920169135,-92.217901676308,-92.0573433407085),.UNSPECIFIED.);
#472=B_SPLINE_CURVE_WITH_KNOTS('',3,(#51061,#51062,#51063,#51064,#51065,
#51066,#51067,#51068,#51069,#51070,#51071,#51072,#51073,#51074,#51075,#51076,
#51077,#51078,#51079,#51080,#51081,#51082,#51083,#51084,#51085),
 .UNSPECIFIED.,.F.,.F.,(4,3,3,3,3,3,3,3,4),(89.0746395114255,89.2431306544916,
90.2347209950971,91.2263113357025,92.217901676308,93.2094920169135,94.2010823575189,
95.1926726981244,95.3578248186051),.UNSPECIFIED.);
#473=B_SPLINE_CURVE_WITH_KNOTS('',3,(#51091,#51092,#51093,#51094,#51095,
#51096,#51097,#51098,#51099),.UNSPECIFIED.,.F.,.F.,(4,1,1,1,1,1,4),(103.672557568463,
103.833115904063,104.824706244668,105.816296585274,106.807886925879,107.799477266485,
108.713046690785),.UNSPECIFIED.);
#474=B_SPLINE_CURVE_WITH_KNOTS('',3,(#51102,#51103,#51104,#51105,#51106,
#51107,#51108),.UNSPECIFIED.,.F.,.F.,(4,1,1,1,4),(103.672557568463,104.498995788588,
105.490586129193,106.482176469799,107.473766810404),.UNSPECIFIED.);
#475=B_SPLINE_CURVE_WITH_KNOTS('',3,(#51113,#51114,#51115,#51116,#51117,
#51118,#51119,#51120,#51121,#51122),.UNSPECIFIED.,.F.,.F.,(4,1,1,1,1,1,
1,4),(97.3893722612836,97.8835738604299,98.8751642010353,99.8667545416408,
100.858344882246,101.849935222852,102.841525563457,103.672557568463),
 .UNSPECIFIED.);
#476=B_SPLINE_CURVE_WITH_KNOTS('',3,(#51123,#51124,#51125,#51126,#51127,
#51128,#51129,#51130,#51131,#51132,#51133),.UNSPECIFIED.,.F.,.F.,(4,1,1,
1,1,1,1,1,4),(97.3893722612836,97.5578634043496,98.549453744955,99.5410440855605,
100.532634426166,101.524224766771,102.515815107377,103.507405447982,103.672557568463),
 .UNSPECIFIED.);
#477=B_SPLINE_CURVE_WITH_KNOTS('',3,(#51138,#51139,#51140,#51141,#51142,
#51143,#51144,#51145,#51146,#51147),.UNSPECIFIED.,.F.,.F.,(4,1,1,1,1,1,
1,4),(91.106186954104,91.9340318167971,92.9256221574026,93.917212498008,
94.9088028386135,95.900393179219,96.8919835198244,97.3893722612836),
 .UNSPECIFIED.);
#478=B_SPLINE_CURVE_WITH_KNOTS('',3,(#51148,#51149,#51150,#51151,#51152,
#51153,#51154,#51155,#51156,#51157),.UNSPECIFIED.,.F.,.F.,(4,1,1,1,1,1,
1,4),(91.106186954104,91.6083213607168,92.5999117013223,93.5915020419277,
94.5830923825332,95.5746827231386,96.5662730637441,97.3893722612836),
 .UNSPECIFIED.);
#479=B_SPLINE_CURVE_WITH_KNOTS('',3,(#51162,#51163,#51164,#51165,#51166,
#51167,#51168,#51169,#51170,#51171,#51172),.UNSPECIFIED.,.F.,.F.,(4,1,1,
1,1,1,1,1,4),(84.8230016469244,84.9928994325589,85.9844897731643,86.9760801137698,
87.9676704543753,88.9592607949807,89.9508511355862,90.9424414761916,91.106186954104),
 .UNSPECIFIED.);
#480=B_SPLINE_CURVE_WITH_KNOTS('',3,(#51173,#51174,#51175,#51176,#51177,
#51178,#51179,#51180,#51181,#51182),.UNSPECIFIED.,.F.,.F.,(4,1,1,1,1,1,
1,4),(84.8230016469244,85.658779317084,86.6503696576895,87.6419599982949,
88.6335503389004,89.6251406795059,90.6167310201113,91.106186954104),
 .UNSPECIFIED.);
#481=B_SPLINE_CURVE_WITH_KNOTS('',3,(#51187,#51188,#51189,#51190,#51191,
#51192,#51193,#51194,#51195,#51196),.UNSPECIFIED.,.F.,.F.,(4,1,1,1,1,1,
1,4),(78.5398163397448,79.0433573889261,80.0349477295316,81.026538070137,
82.0181284107425,83.0097187513479,84.0013090919534,84.8230016469244),
 .UNSPECIFIED.);
#482=B_SPLINE_CURVE_WITH_KNOTS('',3,(#51197,#51198,#51199,#51200,#51201,
#51202,#51203,#51204,#51205,#51206,#51207),.UNSPECIFIED.,.F.,.F.,(4,1,1,
1,1,1,1,1,4),(78.5398163397448,78.7176469328458,79.7092372734512,80.7008276140567,
81.6924179546622,82.6840082952676,83.6755986358731,84.6671889764786,84.8230016469244),
 .UNSPECIFIED.);
#483=B_SPLINE_CURVE_WITH_KNOTS('',3,(#51212,#51213,#51214,#51215,#51216,
#51217,#51218,#51219,#51220,#51221),.UNSPECIFIED.,.F.,.F.,(4,1,1,1,1,1,
1,4),(72.2566310325652,73.0938153452933,74.0854056858988,75.0769960265042,
76.0685863671097,77.0601767077152,78.0517670483206,78.5398163397448),
 .UNSPECIFIED.);
#484=B_SPLINE_CURVE_WITH_KNOTS('',3,(#51222,#51223,#51224,#51225,#51226,
#51227,#51228,#51229,#51230,#51231),.UNSPECIFIED.,.F.,.F.,(4,1,1,1,1,1,
1,4),(72.2566310325652,72.768104889213,73.7596952298185,74.7512855704239,
75.7428759110294,76.7344662516349,77.7260565922403,78.5398163397448),
 .UNSPECIFIED.);
#485=B_SPLINE_CURVE_WITH_KNOTS('',3,(#51236,#51237,#51238,#51239,#51240,
#51241,#51242,#51243,#51244,#51245,#51246),.UNSPECIFIED.,.F.,.F.,(4,1,1,
1,1,1,1,1,4),(65.9734457253856,66.1526829610551,67.1442733016605,68.135863642266,
69.1274539828715,70.1190443234769,71.1106346640824,72.1022250046879,72.2566310325652),
 .UNSPECIFIED.);
#486=B_SPLINE_CURVE_WITH_KNOTS('',3,(#51247,#51248,#51249,#51250,#51251,
#51252,#51253,#51254,#51255,#51256),.UNSPECIFIED.,.F.,.F.,(4,1,1,1,1,1,
1,4),(65.9734457253856,66.8185628455802,67.8101531861857,68.8017435267912,
69.7933338673966,70.7849242080021,71.7765145486075,72.2566310325652),
 .UNSPECIFIED.);
#487=B_SPLINE_CURVE_WITH_KNOTS('',3,(#51261,#51262,#51263,#51264,#51265,
#51266,#51267,#51268,#51269,#51270),.UNSPECIFIED.,.F.,.F.,(4,1,1,1,1,1,
1,4),(59.690260418206,60.2031409174223,61.1947312580278,62.1863215986332,
63.1779119392387,64.1695022798442,65.1610926204496,65.9734457253856),
 .UNSPECIFIED.);
#488=B_SPLINE_CURVE_WITH_KNOTS('',3,(#51271,#51272,#51273,#51274,#51275,
#51276,#51277,#51278,#51279,#51280,#51281),.UNSPECIFIED.,.F.,.F.,(4,1,1,
1,1,1,1,1,4),(59.690260418206,59.877430461342,60.8690208019474,61.8606111425529,
62.8522014831584,63.8437918237638,64.8353821643693,65.8269725049748,65.9734457253856),
 .UNSPECIFIED.);
#489=B_SPLINE_CURVE_WITH_KNOTS('',3,(#51286,#51287,#51288,#51289,#51290,
#51291,#51292,#51293,#51294,#51295),.UNSPECIFIED.,.F.,.F.,(4,1,1,1,1,1,
1,4),(53.4070751110264,54.2535988737895,55.245189214395,56.2367795550005,
57.2283698956059,58.2199602362114,59.2115505768168,59.690260418206),
 .UNSPECIFIED.);
#490=B_SPLINE_CURVE_WITH_KNOTS('',3,(#51296,#51297,#51298,#51299,#51300,
#51301,#51302,#51303,#51304,#51305),.UNSPECIFIED.,.F.,.F.,(4,1,1,1,1,1,
1,4),(53.4070751110264,53.9278884177092,54.9194787583147,55.9110690989201,
56.9026594395256,57.8942497801311,58.8858401207365,59.690260418206),
 .UNSPECIFIED.);
#491=B_SPLINE_CURVE_WITH_KNOTS('',3,(#51310,#51311,#51312,#51313,#51314,
#51315,#51316,#51317,#51318,#51319,#51320),.UNSPECIFIED.,.F.,.F.,(4,1,1,
1,1,1,1,1,4),(47.1238898038469,47.3124664895513,48.3040568301568,49.2956471707622,
50.2872375113677,51.2788278519731,52.2704181925786,53.2620085331841,53.4070751110264),
 .UNSPECIFIED.);
#492=B_SPLINE_CURVE_WITH_KNOTS('',3,(#51321,#51322,#51323,#51324,#51325,
#51326,#51327,#51328,#51329,#51330),.UNSPECIFIED.,.F.,.F.,(4,1,1,1,1,1,
1,4),(47.1238898038468,47.9783463740764,48.9699367146819,49.9615270552874,
50.9531173958928,51.9447077364983,52.9362980771037,53.4070751110264),
 .UNSPECIFIED.);
#493=B_SPLINE_CURVE_WITH_KNOTS('',3,(#51335,#51336,#51337,#51338,#51339,
#51340,#51341,#51342,#51343,#51344),.UNSPECIFIED.,.F.,.F.,(4,1,1,1,1,1,
1,4),(40.8407044966673,41.3629244459185,42.354514786524,43.3461051271294,
44.3376954677349,45.3292858083404,46.3208761489458,47.1238898038469),
 .UNSPECIFIED.);
#494=B_SPLINE_CURVE_WITH_KNOTS('',3,(#51345,#51346,#51347,#51348,#51349,
#51350,#51351,#51352,#51353,#51354,#51355),.UNSPECIFIED.,.F.,.F.,(4,1,1,
1,1,1,1,1,4),(40.8407044966672,41.0372139898382,42.0288043304437,43.0203946710491,
44.0119850116546,45.0035753522601,45.9951656928655,46.986756033471,47.1238898038468),
 .UNSPECIFIED.);
#495=B_SPLINE_CURVE_WITH_KNOTS('',3,(#51360,#51361,#51362,#51363,#51364,
#51365,#51366,#51367,#51368,#51369),.UNSPECIFIED.,.F.,.F.,(4,1,1,1,1,1,
1,4),(34.5575191894877,35.4133824022857,36.4049727428912,37.3965630834967,
38.3881534241021,39.3797437647076,40.3713341053131,40.8407044966673),
 .UNSPECIFIED.);
#496=B_SPLINE_CURVE_WITH_KNOTS('',3,(#51370,#51371,#51372,#51373,#51374,
#51375,#51376,#51377,#51378,#51379),.UNSPECIFIED.,.F.,.F.,(4,1,1,1,1,1,
1,4),(34.5575191894877,35.0876719462054,36.0792622868109,37.0708526274164,
38.0624429680218,39.0540333086273,40.0456236492327,40.8407044966672),
 .UNSPECIFIED.);
#497=B_SPLINE_CURVE_WITH_KNOTS('',3,(#51384,#51385,#51386,#51387,#51388,
#51389,#51390,#51391,#51392,#51393,#51394),.UNSPECIFIED.,.F.,.F.,(4,1,1,
1,1,1,1,1,4),(28.2743338823081,28.4722500180475,29.463840358653,30.4554306992584,
31.4470210398639,32.4386113804694,33.4302017210748,34.4217920616803,34.5575191894877),
 .UNSPECIFIED.);
#498=B_SPLINE_CURVE_WITH_KNOTS('',3,(#51395,#51396,#51397,#51398,#51399,
#51400,#51401,#51402,#51403,#51404),.UNSPECIFIED.,.F.,.F.,(4,1,1,1,1,1,
1,4),(28.2743338823081,29.1381299025727,30.1297202431781,31.1213105837836,
32.112900924389,33.1044912649945,34.0960816056,34.5575191894877),
 .UNSPECIFIED.);
#499=B_SPLINE_CURVE_WITH_KNOTS('',3,(#51409,#51410,#51411,#51412,#51413,
#51414,#51415,#51416,#51417,#51418),.UNSPECIFIED.,.F.,.F.,(4,1,1,1,1,1,
1,4),(21.9911485751285,22.5227079744147,23.5142983150202,24.5058886556257,
25.4974789962311,26.4890693368366,27.480659677442,28.2743338823081),
 .UNSPECIFIED.);
#500=B_SPLINE_CURVE_WITH_KNOTS('',3,(#51419,#51420,#51421,#51422,#51423,
#51424,#51425,#51426,#51427,#51428,#51429),.UNSPECIFIED.,.F.,.F.,(4,1,1,
1,1,1,1,1,4),(21.9911485751285,22.1969975183344,23.1885878589399,24.1801781995453,
25.1717685401508,26.1633588807563,27.1549492213617,28.1465395619672,28.2743338823081),
 .UNSPECIFIED.);
#501=B_SPLINE_CURVE_WITH_KNOTS('',3,(#51434,#51435,#51436,#51437,#51438,
#51439,#51440,#51441,#51442,#51443),.UNSPECIFIED.,.F.,.F.,(4,1,1,1,1,1,
1,4),(15.7079632679489,16.573165930782,17.5647562713874,18.5563466119929,
19.5479369525983,20.5395272932038,21.5311176338093,21.9911485751285),
 .UNSPECIFIED.);
#502=B_SPLINE_CURVE_WITH_KNOTS('',3,(#51444,#51445,#51446,#51447,#51448,
#51449,#51450,#51451,#51452,#51453),.UNSPECIFIED.,.F.,.F.,(4,1,1,1,1,1,
1,4),(15.7079632679489,16.2474554747016,17.2390458153071,18.2306361559126,
19.222226496518,20.2138168371235,21.205407177729,21.9911485751285),
 .UNSPECIFIED.);
#503=B_SPLINE_CURVE_WITH_KNOTS('',3,(#51456,#51457,#51458,#51459,#51460,
#51461,#51462,#51463,#51464,#51465,#51466,#51467,#51468,#51469,#51470,#51471,
#51472,#51473,#51474,#51475,#51476,#51477,#51478,#51479,#51480,#51481,#51482,
#51483,#51484,#51485,#51486,#51487,#51488,#51489,#51490,#51491,#51492,#51493,
#51494,#51495,#51496,#51497,#51498,#51499,#51500,#51501,#51502,#51503,#51504,
#51505,#51506,#51507,#51508,#51509,#51510,#51511,#51512,#51513,#51514,#51515,
#51516),.UNSPECIFIED.,.F.,.F.,(4,3,3,3,3,3,3,3,3,3,3,3,3,3,3,3,3,3,3,3,
4),(-0.744397949170491,-0.718888480435814,-0.671065586721542,-0.646483273340718,
-0.600248581890479,-0.572968698430621,-0.555731357696308,-0.495420255894194,
-0.456580299181414,-0.439125670228373,-0.423945368768442,-0.376189396302194,
-0.32916572176442,-0.306302680888458,-0.285176397353076,-0.222891638647477,
-0.167168728985607,-0.151663890453069,-0.134867149404615,-0.0674335747023076,
0.),.UNSPECIFIED.);
#504=B_SPLINE_CURVE_WITH_KNOTS('',3,(#51521,#51522,#51523,#51524,#51525,
#51526,#51527,#51528,#51529,#51530,#51531,#51532,#51533,#51534,#51535,#51536,
#51537,#51538,#51539,#51540,#51541,#51542,#51543,#51544,#51545,#51546,#51547,
#51548,#51549,#51550,#51551,#51552,#51553,#51554,#51555,#51556,#51557,#51558,
#51559,#51560,#51561,#51562,#51563,#51564,#51565,#51566,#51567,#51568,#51569,
#51570,#51571,#51572,#51573,#51574,#51575,#51576,#51577,#51578,#51579,#51580,
#51581),.UNSPECIFIED.,.F.,.F.,(4,3,3,3,3,3,3,3,3,3,3,3,3,3,3,3,3,3,3,3,
4),(-0.741270768406373,-0.710653752603244,-0.663515400778915,-0.642552751532044,
-0.621528179181629,-0.557094712642544,-0.539607756557645,-0.476917461805843,
-0.415921284094216,-0.398576094285539,-0.383216406245164,-0.338950727439734,
-0.281486365585587,-0.260617405175195,-0.246177177084019,-0.184632882813014,
-0.134618480262488,-0.117250433969387,-0.0586252169846935,-0.00390747240475656,
0.),.UNSPECIFIED.);
#505=B_SPLINE_CURVE_WITH_KNOTS('',3,(#51994,#51995,#51996,#51997,#51998,
#51999,#52000),.UNSPECIFIED.,.F.,.F.,(4,3,4),(95.3578248186051,96.1842630387299,
97.0978324630305),.UNSPECIFIED.);
#506=B_SPLINE_CURVE_WITH_KNOTS('',3,(#52002,#52003,#52004,#52005,#52006,
#52007,#52008,#52009,#52010,#52011,#52012,#52013,#52014,#52015,#52016,#52017,
#52018,#52019,#52020,#52021,#52022,#52023,#52024,#52025,#52026,#52027,#52028,
#52029,#52030,#52031,#52032,#52033,#52034,#52035,#52036,#52037,#52038,#52039,
#52040,#52041,#52042,#52043,#52044,#52045,#52046,#52047,#52048,#52049,#52050,
#52051,#52052,#52053,#52054,#52055,#52056,#52057,#52058,#52059,#52060,#52061,
#52062),.UNSPECIFIED.,.F.,.F.,(4,3,3,3,3,3,3,3,3,3,3,3,3,3,3,3,3,3,3,3,
4),(-0.7443979491706,-0.718888480435923,-0.671065589306389,-0.646483278263035,
-0.600248517649804,-0.572968043327937,-0.555731292334261,-0.495420193045671,
-0.456580298674706,-0.439125676945103,-0.423945387737792,-0.376189396302257,
-0.329165721764475,-0.306302670249697,-0.285176394034303,-0.222891657896494,
-0.16716874342237,-0.151664010969902,-0.134867173180257,-0.0674335865901284,
0.),.UNSPECIFIED.);
#507=B_SPLINE_CURVE_WITH_KNOTS('',3,(#52063,#52064,#52065,#52066,#52067,
#52068,#52069,#52070,#52071),.UNSPECIFIED.,.F.,.F.,(4,1,1,1,1,1,4),(10.3759343473737,
11.2895037716743,12.2810941122798,13.2726844528853,14.2642747934907,15.2558651340962,
15.7079632679489),.UNSPECIFIED.);
#508=B_SPLINE_CURVE_WITH_KNOTS('',3,(#52077,#52078,#52079,#52080,#52081,
#52082,#52083,#52084,#52085,#52086,#52087,#52088,#52089,#52090,#52091,#52092,
#52093,#52094,#52095,#52096,#52097,#52098,#52099,#52100,#52101,#52102,#52103,
#52104,#52105,#52106,#52107,#52108,#52109,#52110,#52111,#52112,#52113,#52114,
#52115,#52116,#52117,#52118,#52119,#52120,#52121,#52122,#52123,#52124,#52125,
#52126,#52127,#52128,#52129,#52130,#52131,#52132,#52133,#52134,#52135,#52136,
#52137),.UNSPECIFIED.,.F.,.F.,(4,3,3,3,3,3,3,3,3,3,3,3,3,3,3,3,3,3,3,3,
4),(-0.741270768406355,-0.710653752603231,-0.663515385056919,-0.642552661274003,
-0.621528157125719,-0.557094687200405,-0.539607732337506,-0.476917424661932,
-0.415921204939973,-0.398576035954998,-0.383216387012519,-0.338950727439722,
-0.281486362115991,-0.260617409418295,-0.24617718206237,-0.184632886546777,
-0.134618488551931,-0.117250439398334,-0.0586252196991669,-0.00390755098249406,
0.),.UNSPECIFIED.);
#509=B_SPLINE_CURVE_WITH_KNOTS('',3,(#52140,#52141,#52142,#52143,#52144,
#52145,#52146,#52147),.UNSPECIFIED.,.F.,.F.,(4,1,1,1,1,4),(11.6152142277546,
12.6068045683601,13.5983949089656,14.589985249571,15.5815755901765,15.7079632679489),
 .UNSPECIFIED.);
#510=B_SPLINE_CURVE_WITH_KNOTS('',3,(#52560,#52561,#52562,#52563),
 .UNSPECIFIED.,.F.,.F.,(4,4),(-99.1590340605463,-98.3405286478881),
 .UNSPECIFIED.);
#511=B_SPLINE_CURVE_WITH_KNOTS('',3,(#53429,#53430,#53431,#53432,#53433,
#53434,#53435,#53436,#53437,#53438,#53439,#53440,#53441,#53442,#53443,#53444),
 .UNSPECIFIED.,.F.,.F.,(4,3,3,3,3,4),(-4.09254174883836,-3.97484940371104,
-3.47799322824716,-2.98113705278328,-2.4842808773194,-2.06980418878614),
 .UNSPECIFIED.);
#512=B_SPLINE_CURVE_WITH_KNOTS('',3,(#53447,#53448,#53449,#53450,#53451,
#53452,#53453,#53454,#53455,#53456),.UNSPECIFIED.,.F.,.F.,(4,3,3,4),(0.,
0.496856175463878,0.99371235092776,1.11885509353764),.UNSPECIFIED.);
#513=B_SPLINE_CURVE_WITH_KNOTS('',3,(#53461,#53462,#53463,#53464,#53465,
#53466,#53467,#53468,#53469,#53470,#53471,#53472,#53473,#53474,#53475,#53476,
#53477,#53478,#53479,#53480,#53481,#53482,#53483,#53484,#53485,#53486,#53487,
#53488,#53489,#53490,#53491,#53492,#53493,#53494,#53495,#53496,#53497,#53498,
#53499,#53500),.UNSPECIFIED.,.F.,.F.,(4,3,3,3,3,3,3,3,3,3,3,3,3,4),(-10.3757270560178,
-9.9371235092776,-9.44026733381373,-8.94341115834984,-8.44655498288596,
-7.94969880742208,-7.4528426319582,-6.95598645649432,-6.45913028103044,
-5.96227410556656,-5.46541793010268,-4.9685617546388,-4.47170557917492,
-4.09254174883836),.UNSPECIFIED.);
#514=B_SPLINE_CURVE_WITH_KNOTS('',3,(#53501,#53502,#53503,#53504,#53505,
#53506,#53507,#53508,#53509,#53510,#53511,#53512,#53513,#53514,#53515,#53516,
#53517,#53518,#53519,#53520,#53521,#53522,#53523,#53524,#53525,#53526,#53527,
#53528,#53529,#53530,#53531,#53532,#53533,#53534,#53535,#53536,#53537,#53538,
#53539,#53540),.UNSPECIFIED.,.F.,.F.,(4,3,3,3,3,3,3,3,3,3,3,3,3,4),(1.11885509353764,
1.49056852639164,1.98742470185552,2.4842808773194,2.98113705278328,3.47799322824716,
3.97484940371104,4.47170557917492,4.9685617546388,5.46541793010268,5.96227410556656,
6.45913028103044,6.95598645649432,7.40204040071725),.UNSPECIFIED.);
#515=B_SPLINE_CURVE_WITH_KNOTS('',3,(#53545,#53546,#53547,#53548,#53549,
#53550,#53551,#53552,#53553,#53554,#53555,#53556,#53557,#53558,#53559,#53560,
#53561,#53562,#53563,#53564,#53565,#53566,#53567,#53568,#53569,#53570,#53571,
#53572,#53573,#53574,#53575,#53576,#53577,#53578,#53579,#53580,#53581,#53582,
#53583,#53584,#53585,#53586,#53587),.UNSPECIFIED.,.F.,.F.,(4,3,3,3,3,3,
3,3,3,3,3,3,3,3,4),(-16.6589123631976,-16.396253790308,-15.8993976148442,
-15.4025414393803,-14.9056852639164,-14.4088290884525,-13.9119729129886,
-13.4151167375248,-12.9182605620609,-12.421404386597,-11.9245482111331,
-11.4276920356692,-10.9308358602054,-10.4339796847415,-10.3757270560178),
 .UNSPECIFIED.);
#516=B_SPLINE_CURVE_WITH_KNOTS('',3,(#53588,#53589,#53590,#53591,#53592,
#53593,#53594,#53595,#53596,#53597,#53598,#53599,#53600,#53601,#53602,#53603,
#53604,#53605,#53606,#53607,#53608,#53609,#53610,#53611,#53612,#53613,#53614,
#53615,#53616,#53617,#53618,#53619,#53620,#53621,#53622,#53623,#53624,#53625,
#53626,#53627,#53628,#53629,#53630),.UNSPECIFIED.,.F.,.F.,(4,3,3,3,3,3,
3,3,3,3,3,3,3,3,4),(7.40204040071725,7.4528426319582,7.94969880742208,8.44655498288596,
8.94341115834985,9.44026733381372,9.93712350927761,10.4339796847415,10.9308358602054,
11.4276920356693,11.9245482111331,12.421404386597,12.9182605620609,13.4151167375248,
13.6852257078967),.UNSPECIFIED.);
#517=B_SPLINE_CURVE_WITH_KNOTS('',3,(#53635,#53636,#53637,#53638,#53639,
#53640,#53641,#53642,#53643,#53644,#53645,#53646,#53647,#53648,#53649,#53650,
#53651,#53652,#53653,#53654,#53655,#53656,#53657,#53658,#53659,#53660,#53661,
#53662,#53663,#53664,#53665,#53666,#53667,#53668,#53669,#53670,#53671,#53672,
#53673,#53674,#53675,#53676,#53677),.UNSPECIFIED.,.F.,.F.,(4,3,3,3,3,3,
3,3,3,3,3,3,3,3,4),(-22.9420976703771,-22.8553840713385,-22.3585278958746,
-21.8616717204107,-21.3648155449468,-20.867959369483,-20.3711031940191,
-19.8742470185552,-19.3773908430913,-18.8805346676274,-18.3836784921636,
-17.8868223166997,-17.3899661412358,-16.8931099657719,-16.6589123631976),
 .UNSPECIFIED.);
#518=B_SPLINE_CURVE_WITH_KNOTS('',3,(#53678,#53679,#53680,#53681,#53682,
#53683,#53684,#53685,#53686,#53687,#53688,#53689,#53690,#53691,#53692,#53693,
#53694,#53695,#53696,#53697,#53698,#53699,#53700,#53701,#53702,#53703,#53704,
#53705,#53706,#53707,#53708,#53709,#53710,#53711,#53712,#53713,#53714,#53715,
#53716,#53717,#53718,#53719,#53720),.UNSPECIFIED.,.F.,.F.,(4,3,3,3,3,3,
3,3,3,3,3,3,3,3,4),(13.6852257078967,13.9119729129887,14.4088290884525,
14.9056852639164,15.4025414393803,15.8993976148442,16.3962537903081,16.8931099657719,
17.3899661412358,17.8868223166997,18.3836784921636,18.8805346676274,19.3773908430913,
19.8742470185552,19.9684110150765),.UNSPECIFIED.);
#519=B_SPLINE_CURVE_WITH_KNOTS('',3,(#53725,#53726,#53727,#53728,#53729,
#53730,#53731,#53732,#53733,#53734,#53735,#53736,#53737,#53738,#53739,#53740,
#53741,#53742,#53743,#53744,#53745,#53746,#53747,#53748,#53749,#53750,#53751,
#53752,#53753,#53754,#53755,#53756,#53757,#53758,#53759,#53760,#53761,#53762,
#53763,#53764),.UNSPECIFIED.,.F.,.F.,(4,3,3,3,3,3,3,3,3,3,3,3,3,4),(-29.2252829775566,
-28.8176581769051,-28.3208020014412,-27.8239458259773,-27.3270896505134,
-26.8302334750495,-26.3333772995857,-25.8365211241218,-25.3396649486579,
-24.842808773194,-24.3459525977301,-23.8490964222662,-23.3522402468024,
-22.9420976703771),.UNSPECIFIED.);
#520=B_SPLINE_CURVE_WITH_KNOTS('',3,(#53765,#53766,#53767,#53768,#53769,
#53770,#53771,#53772,#53773,#53774,#53775,#53776,#53777,#53778,#53779,#53780,
#53781,#53782,#53783,#53784,#53785,#53786,#53787,#53788,#53789,#53790,#53791,
#53792,#53793,#53794,#53795,#53796,#53797,#53798,#53799,#53800,#53801,#53802,
#53803,#53804),.UNSPECIFIED.,.F.,.F.,(4,3,3,3,3,3,3,3,3,3,3,3,3,4),(19.9684110150765,
20.3711031940191,20.867959369483,21.3648155449468,21.8616717204107,22.3585278958746,
22.8553840713385,23.3522402468024,23.8490964222662,24.3459525977301,24.842808773194,
25.3396649486579,25.8365211241218,26.251596322256),.UNSPECIFIED.);
#521=B_SPLINE_CURVE_WITH_KNOTS('',3,(#53809,#53810,#53811,#53812,#53813,
#53814,#53815,#53816,#53817,#53818,#53819,#53820,#53821,#53822,#53823,#53824,
#53825,#53826,#53827,#53828,#53829,#53830,#53831,#53832,#53833,#53834,#53835,
#53836,#53837,#53838,#53839,#53840,#53841,#53842,#53843,#53844,#53845,#53846,
#53847,#53848,#53849,#53850,#53851),.UNSPECIFIED.,.F.,.F.,(4,3,3,3,3,3,
3,3,3,3,3,3,3,3,4),(-35.5084682847363,-35.2767884579355,-34.7799322824716,
-34.2830761070077,-33.7862199315439,-33.28936375608,-32.7925075806161,-32.2956514051522,
-31.7987952296883,-31.3019390542245,-30.8050828787606,-30.3082267032967,
-29.8113705278328,-29.3145143523689,-29.2252829775566),.UNSPECIFIED.);
#522=B_SPLINE_CURVE_WITH_KNOTS('',3,(#53852,#53853,#53854,#53855,#53856,
#53857,#53858,#53859,#53860,#53861,#53862,#53863,#53864,#53865,#53866,#53867,
#53868,#53869,#53870,#53871,#53872,#53873,#53874,#53875,#53876,#53877,#53878,
#53879,#53880,#53881,#53882,#53883,#53884,#53885,#53886,#53887,#53888,#53889,
#53890,#53891,#53892,#53893,#53894),.UNSPECIFIED.,.F.,.F.,(4,3,3,3,3,3,
3,3,3,3,3,3,3,3,4),(26.251596322256,26.3333772995856,26.8302334750495,27.3270896505134,
27.8239458259773,28.3208020014412,28.817658176905,29.3145143523689,29.8113705278328,
30.3082267032967,30.8050828787606,31.3019390542244,31.7987952296883,32.2956514051522,
32.5347816294354),.UNSPECIFIED.);
#523=B_SPLINE_CURVE_WITH_KNOTS('',3,(#53899,#53900,#53901,#53902,#53903,
#53904,#53905,#53906,#53907,#53908,#53909,#53910,#53911,#53912,#53913,#53914,
#53915,#53916,#53917,#53918,#53919,#53920,#53921,#53922,#53923,#53924,#53925,
#53926,#53927,#53928,#53929,#53930,#53931,#53932,#53933,#53934,#53935,#53936,
#53937,#53938,#53939,#53940,#53941),.UNSPECIFIED.,.F.,.F.,(4,3,3,3,3,3,
3,3,3,3,3,3,3,3,4),(-41.7916535919158,-41.7359187389659,-41.2390625635021,
-40.7422063880382,-40.2453502125743,-39.7484940371104,-39.2516378616465,
-38.7547816861827,-38.2579255107188,-37.7610693352549,-37.264213159791,
-36.7673569843271,-36.2705008088633,-35.7736446333994,-35.5084682847363),
 .UNSPECIFIED.);
#524=B_SPLINE_CURVE_WITH_KNOTS('',3,(#53942,#53943,#53944,#53945,#53946,
#53947,#53948,#53949,#53950,#53951,#53952,#53953,#53954,#53955,#53956,#53957,
#53958,#53959,#53960,#53961,#53962,#53963,#53964,#53965,#53966,#53967,#53968,
#53969,#53970,#53971,#53972,#53973,#53974,#53975,#53976,#53977,#53978,#53979,
#53980,#53981,#53982,#53983,#53984),.UNSPECIFIED.,.F.,.F.,(4,3,3,3,3,3,
3,3,3,3,3,3,3,3,4),(32.5347816294354,32.7925075806161,33.28936375608,33.7862199315438,
34.2830761070077,34.7799322824716,35.2767884579355,35.7736446333994,36.2705008088632,
36.7673569843271,37.264213159791,37.7610693352549,38.2579255107188,38.7547816861826,
38.8179669366152),.UNSPECIFIED.);
#525=B_SPLINE_CURVE_WITH_KNOTS('',3,(#53989,#53990,#53991,#53992,#53993,
#53994,#53995,#53996,#53997,#53998,#53999,#54000,#54001,#54002,#54003,#54004,
#54005,#54006,#54007,#54008,#54009,#54010,#54011,#54012,#54013,#54014,#54015,
#54016,#54017,#54018,#54019,#54020,#54021,#54022,#54023,#54024,#54025,#54026,
#54027,#54028),.UNSPECIFIED.,.F.,.F.,(4,3,3,3,3,3,3,3,3,3,3,3,3,4),(-48.0748388990955,
-47.6981928445325,-47.2013366690686,-46.7044804936047,-46.2076243181409,
-45.710768142677,-45.2139119672131,-44.7170557917492,-44.2201996162853,
-43.7233434408215,-43.2264872653576,-42.7296310898937,-42.2327749144298,
-41.7916535919158),.UNSPECIFIED.);
#526=B_SPLINE_CURVE_WITH_KNOTS('',3,(#54029,#54030,#54031,#54032,#54033,
#54034,#54035,#54036,#54037,#54038,#54039,#54040,#54041,#54042,#54043,#54044,
#54045,#54046,#54047,#54048,#54049,#54050,#54051,#54052,#54053,#54054,#54055,
#54056,#54057,#54058,#54059,#54060,#54061,#54062,#54063,#54064,#54065,#54066,
#54067,#54068),.UNSPECIFIED.,.F.,.F.,(4,3,3,3,3,3,3,3,3,3,3,3,3,4),(38.8179669366152,
39.2516378616465,39.7484940371104,40.2453502125743,40.7422063880382,41.239062563502,
41.7359187389659,42.2327749144298,42.7296310898937,43.2264872653576,43.7233434408215,
44.2201996162853,44.7170557917492,45.1011522437947),.UNSPECIFIED.);
#527=B_SPLINE_CURVE_WITH_KNOTS('',3,(#54073,#54074,#54075,#54076,#54077,
#54078,#54079,#54080,#54081,#54082,#54083,#54084,#54085,#54086,#54087,#54088,
#54089,#54090,#54091,#54092,#54093,#54094,#54095,#54096,#54097,#54098,#54099,
#54100,#54101,#54102,#54103,#54104,#54105,#54106,#54107,#54108,#54109,#54110,
#54111,#54112,#54113,#54114,#54115),.UNSPECIFIED.,.F.,.F.,(4,3,3,3,3,3,
3,3,3,3,3,3,3,3,4),(-54.358024206275,-54.157323125563,-53.6604669500991,
-53.1636107746352,-52.6667545991713,-52.1698984237074,-51.6730422482436,
-51.1761860727797,-50.6793298973158,-50.1824737218519,-49.685617546388,
-49.1887613709242,-48.6919051954603,-48.1950490199964,-48.0748388990955),
 .UNSPECIFIED.);
#528=B_SPLINE_CURVE_WITH_KNOTS('',3,(#54116,#54117,#54118,#54119,#54120,
#54121,#54122,#54123,#54124,#54125,#54126,#54127,#54128,#54129,#54130,#54131,
#54132,#54133,#54134,#54135,#54136,#54137,#54138,#54139,#54140,#54141,#54142,
#54143,#54144,#54145,#54146,#54147,#54148,#54149,#54150,#54151,#54152,#54153,
#54154,#54155,#54156,#54157,#54158),.UNSPECIFIED.,.F.,.F.,(4,3,3,3,3,3,
3,3,3,3,3,3,3,3,4),(45.1011522437947,45.2139119672131,45.710768142677,46.2076243181408,
46.7044804936047,47.2013366690686,47.6981928445325,48.1950490199964,48.6919051954603,
49.1887613709241,49.685617546388,50.1824737218519,50.6793298973158,51.1761860727797,
51.3843375509744),.UNSPECIFIED.);
#529=B_SPLINE_CURVE_WITH_KNOTS('',3,(#54163,#54164,#54165,#54166,#54167,
#54168,#54169,#54170,#54171,#54172,#54173,#54174,#54175,#54176,#54177,#54178,
#54179,#54180,#54181,#54182,#54183,#54184,#54185,#54186,#54187,#54188,#54189,
#54190,#54191,#54192,#54193,#54194,#54195,#54196,#54197,#54198,#54199,#54200,
#54201,#54202,#54203,#54204,#54205),.UNSPECIFIED.,.F.,.F.,(4,3,3,3,3,3,
3,3,3,3,3,3,3,3,4),(-60.6412095134547,-60.6164534065934,-60.1195972311295,
-59.6227410556656,-59.1258848802018,-58.6290287047379,-58.132172529274,
-57.6353163538101,-57.1384601783463,-56.6416040028824,-56.1447478274185,
-55.6478916519546,-55.1510354764907,-54.6541793010268,-54.358024206275),
 .UNSPECIFIED.);
#530=B_SPLINE_CURVE_WITH_KNOTS('',3,(#54206,#54207,#54208,#54209,#54210,
#54211,#54212,#54213,#54214,#54215,#54216,#54217,#54218,#54219,#54220,#54221,
#54222,#54223,#54224,#54225,#54226,#54227,#54228,#54229,#54230,#54231,#54232,
#54233,#54234,#54235,#54236,#54237,#54238,#54239,#54240,#54241,#54242,#54243,
#54244,#54245,#54246,#54247,#54248),.UNSPECIFIED.,.F.,.F.,(4,3,3,3,3,3,
3,3,3,3,3,3,3,3,4),(51.3843375509744,51.6730422482435,52.1698984237074,
52.6667545991713,53.1636107746352,53.660466950099,54.1573231255629,54.6541793010268,
55.1510354764907,55.6478916519546,56.1447478274185,56.6416040028823,57.1384601783462,
57.6353163538101,57.6675228581539),.UNSPECIFIED.);
#531=B_SPLINE_CURVE_WITH_KNOTS('',3,(#54254,#54255,#54256,#54257,#54258,
#54259,#54260,#54261,#54262,#54263,#54264,#54265,#54266,#54267),
 .UNSPECIFIED.,.F.,.F.,(4,1,1,1,1,1,1,1,1,1,1,4),(65.9734457253856,66.2696008201374,
66.7664569956013,67.2633131710652,67.7601693465291,68.257025521993,68.7538816974568,
69.2507378729207,69.7475940483846,70.2444502238485,70.7413063993124,71.1557830878455),
 .UNSPECIFIED.);
#532=B_SPLINE_CURVE_WITH_KNOTS('',3,(#54270,#54271,#54272,#54273,#54274,
#54275,#54276,#54277,#54278,#54279,#54280),.UNSPECIFIED.,.F.,.F.,(4,1,1,
1,1,1,1,1,4),(65.9734457253856,66.4380953965057,66.9349515719695,67.4318077474334,
67.9286639228973,68.4255200983612,68.9223762738251,69.4192324492889,69.9160886247528),
 .UNSPECIFIED.);
#533=B_SPLINE_CURVE_WITH_KNOTS('',3,(#54285,#54286,#54287,#54288,#54289,
#54290,#54291,#54292,#54293,#54294,#54295,#54296,#54297,#54298,#54299,#54300,
#54301),.UNSPECIFIED.,.F.,.F.,(4,1,1,1,1,1,1,1,1,1,1,1,1,1,4),(59.6902604182061,
59.810470539107,60.3073267145709,60.8041828900348,61.3010390654986,61.7978952409625,
62.2947514164264,62.7916075918903,63.2884637673542,63.785319942818,64.2821761182819,
64.7790322937458,65.2758884692097,65.7727446446736,65.9734457253856),
 .UNSPECIFIED.);
#534=B_SPLINE_CURVE_WITH_KNOTS('',3,(#54302,#54303,#54304,#54305,#54306,
#54307,#54308,#54309,#54310,#54311,#54312,#54313,#54314,#54315,#54316,#54317,
#54318),.UNSPECIFIED.,.F.,.F.,(4,1,1,1,1,1,1,1,1,1,1,1,1,1,4),(59.6902604182061,
59.9789651154752,60.4758212909391,60.972677466403,61.4695336418669,61.9663898173307,
62.4632459927946,62.9601021682585,63.4569583437224,63.9538145191863,64.4506706946501,
64.947526870114,65.4443830455779,65.9412392210418,65.9734457253856),
 .UNSPECIFIED.);
#535=B_SPLINE_CURVE_WITH_KNOTS('',3,(#54323,#54324,#54325,#54326,#54327,
#54328,#54329,#54330,#54331,#54332,#54333,#54334,#54335,#54336,#54337,#54338),
 .UNSPECIFIED.,.F.,.F.,(4,1,1,1,1,1,1,1,1,1,1,1,1,4),(53.4070751110264,
53.8481964335404,54.3450526090043,54.8419087844682,55.3387649599321,55.8356211353959,
56.3324773108598,56.8293334863237,57.3261896617876,57.8230458372515,58.3199020127153,
58.8167581881792,59.3136143636431,59.6902604182061),.UNSPECIFIED.);
#536=B_SPLINE_CURVE_WITH_KNOTS('',3,(#54339,#54340,#54341,#54342,#54343,
#54344,#54345,#54346,#54347,#54348,#54349,#54350,#54351,#54352,#54353,#54354,
#54355),.UNSPECIFIED.,.F.,.F.,(4,1,1,1,1,1,1,1,1,1,1,1,1,1,4),(53.4070751110264,
53.5198348344448,54.0166910099087,54.5135471853725,55.0104033608364,55.5072595363003,
56.0041157117642,56.5009718872281,56.9978280626919,57.4946842381558,57.9915404136197,
58.4883965890836,58.9852527645475,59.4821089400113,59.6902604182061),
 .UNSPECIFIED.);
#537=B_SPLINE_CURVE_WITH_KNOTS('',3,(#54360,#54361,#54362,#54363,#54364,
#54365,#54366,#54367,#54368,#54369,#54370,#54371,#54372,#54373,#54374,#54375,
#54376),.UNSPECIFIED.,.F.,.F.,(4,1,1,1,1,1,1,1,1,1,1,1,1,1,4),(47.1238898038469,
47.38906615251,47.8859223279739,48.3827785034377,48.8796346789016,49.3764908543655,
49.8733470298294,50.3702032052933,50.8670593807571,51.363915556221,51.8607717316849,
52.3576279071488,52.8544840826127,53.3513402580765,53.4070751110264),
 .UNSPECIFIED.);
#538=B_SPLINE_CURVE_WITH_KNOTS('',3,(#54377,#54378,#54379,#54380,#54381,
#54382,#54383,#54384,#54385,#54386,#54387,#54388,#54389,#54390,#54391,#54392),
 .UNSPECIFIED.,.F.,.F.,(4,1,1,1,1,1,1,1,1,1,1,1,1,4),(47.1238898038469,
47.5575607288782,48.0544169043421,48.551273079806,49.0481292552699,49.5449854307337,
50.0418416061976,50.5386977816615,51.0355539571254,51.5324101325893,52.0292663080531,
52.526122483517,53.0229786589809,53.4070751110264),.UNSPECIFIED.);
#539=B_SPLINE_CURVE_WITH_KNOTS('',3,(#54397,#54398,#54399,#54400,#54401,
#54402,#54403,#54404,#54405,#54406,#54407,#54408,#54409,#54410,#54411,#54412,
#54413),.UNSPECIFIED.,.F.,.F.,(4,1,1,1,1,1,1,1,1,1,1,1,1,1,4),(40.8407044966674,
40.9299358714795,41.4267920469434,41.9236482224073,42.4205043978712,42.9173605733351,
43.4142167487989,43.9110729242628,44.4079290997267,44.9047852751906,45.4016414506545,
45.8984976261183,46.3953538015822,46.8922099770461,47.1238898038469),
 .UNSPECIFIED.);
#540=B_SPLINE_CURVE_WITH_KNOTS('',3,(#54414,#54415,#54416,#54417,#54418,
#54419,#54420,#54421,#54422,#54423,#54424,#54425,#54426,#54427,#54428,#54429,
#54430),.UNSPECIFIED.,.F.,.F.,(4,1,1,1,1,1,1,1,1,1,1,1,1,1,4),(40.8407044966672,
41.0984304478478,41.5952866233117,42.0921427987755,42.5889989742394,43.0858551497033,
43.5827113251672,44.0795675006311,44.5764236760949,45.0732798515588,45.5701360270227,
46.0669922024866,46.5638483779504,47.0607045534143,47.1238898038469),
 .UNSPECIFIED.);
#541=B_SPLINE_CURVE_WITH_KNOTS('',3,(#54435,#54436,#54437,#54438,#54439,
#54440,#54441,#54442,#54443,#54444,#54445,#54446,#54447,#54448,#54449,#54450),
 .UNSPECIFIED.,.F.,.F.,(4,1,1,1,1,1,1,1,1,1,1,1,1,4),(34.5575191894877,
34.967661765913,35.4645179413769,35.9613741168407,36.4582302923046,36.9550864677685,
37.4519426432324,37.9487988186963,38.4456549941601,38.942511169624,39.4393673450879,
39.9362235205518,40.4330796960157,40.8407044966674),.UNSPECIFIED.);
#542=B_SPLINE_CURVE_WITH_KNOTS('',3,(#54451,#54452,#54453,#54454,#54455,
#54456,#54457,#54458,#54459,#54460,#54461,#54462,#54463,#54464,#54465,#54466,
#54467),.UNSPECIFIED.,.F.,.F.,(4,1,1,1,1,1,1,1,1,1,1,1,1,1,4),(34.5575191894877,
34.6393001668173,35.1361563422812,35.6330125177451,36.129868693209,36.6267248686729,
37.1235810441367,37.6204372196006,38.1172933950645,38.6141495705284,39.1110057459923,
39.6078619214561,40.10471809692,40.6015742723839,40.8407044966672),
 .UNSPECIFIED.);
#543=B_SPLINE_CURVE_WITH_KNOTS('',3,(#54472,#54473,#54474,#54475,#54476,
#54477,#54478,#54479,#54480,#54481,#54482,#54483,#54484,#54485,#54486,#54487,
#54488),.UNSPECIFIED.,.F.,.F.,(4,1,1,1,1,1,1,1,1,1,1,1,1,1,4),(28.2743338823082,
28.5085314848825,29.0053876603464,29.5022438358103,29.9991000112742,30.495956186738,
30.9928123622019,31.4896685376658,31.9865247131297,32.4833808885936,32.9802370640574,
33.4770932395213,33.9739494149852,34.4708055904491,34.5575191894877),
 .UNSPECIFIED.);
#544=B_SPLINE_CURVE_WITH_KNOTS('',3,(#54489,#54490,#54491,#54492,#54493,
#54494,#54495,#54496,#54497,#54498,#54499,#54500,#54501,#54502,#54503,#54504),
 .UNSPECIFIED.,.F.,.F.,(4,1,1,1,1,1,1,1,1,1,1,1,1,4),(28.2743338823082,
28.6770260612508,29.1738822367147,29.6707384121785,30.1675945876424,30.6644507631063,
31.1613069385702,31.6581631140341,32.1550192894979,32.6518754649618,33.1487316404257,
33.6455878158896,34.1424439913535,34.5575191894877),.UNSPECIFIED.);
#545=B_SPLINE_CURVE_WITH_KNOTS('',3,(#54509,#54510,#54511,#54512,#54513,
#54514,#54515,#54516,#54517,#54518,#54519,#54520,#54521,#54522,#54523,#54524,
#54525),.UNSPECIFIED.,.F.,.F.,(4,1,1,1,1,1,1,1,1,1,1,1,1,1,4),(21.9911485751284,
22.0494012038521,22.546257379316,23.0431135547798,23.5399697302437,24.0368259057076,
24.5336820811715,25.0305382566354,25.5273944320992,26.0242506075631,26.521106783027,
27.0179629584909,27.5148191339548,28.0116753094186,28.2743338823082),
 .UNSPECIFIED.);
#546=B_SPLINE_CURVE_WITH_KNOTS('',3,(#54526,#54527,#54528,#54529,#54530,
#54531,#54532,#54533,#54534,#54535,#54536,#54537,#54538,#54539,#54540,#54541,
#54542),.UNSPECIFIED.,.F.,.F.,(4,1,1,1,1,1,1,1,1,1,1,1,1,1,4),(21.9911485751284,
22.2178957802203,22.7147519556842,23.2116081311481,23.708464306612,24.2053204820759,
24.7021766575397,25.1990328330036,25.6958890084675,26.1927451839314,26.6896013593953,
27.1864575348591,27.683313710323,28.1801698857869,28.2743338823082),
 .UNSPECIFIED.);
#547=B_SPLINE_CURVE_WITH_KNOTS('',3,(#54547,#54548,#54549,#54550,#54551,
#54552,#54553,#54554,#54555,#54556,#54557,#54558,#54559,#54560,#54561,#54562),
 .UNSPECIFIED.,.F.,.F.,(4,1,1,1,1,1,1,1,1,1,1,1,1,4),(15.707963267949,16.0871270982855,
16.5839832737494,17.0808394492133,17.5776956246772,18.074551800141,18.5714079756049,
19.0682641510688,19.5651203265327,20.0619765019966,20.5588326774604,21.0556888529243,
21.5525450283882,21.9911485751284),.UNSPECIFIED.);
#548=B_SPLINE_CURVE_WITH_KNOTS('',3,(#54563,#54564,#54565,#54566,#54567,
#54568,#54569,#54570,#54571,#54572,#54573,#54574,#54575,#54576,#54577,#54578,
#54579),.UNSPECIFIED.,.F.,.F.,(4,1,1,1,1,1,1,1,1,1,1,1,1,1,4),(15.707963267949,
15.7587654991899,16.2556216746538,16.7524778501176,17.2493340255815,17.7461902010454,
18.2430463765093,18.7399025519732,19.236758727437,19.7336149029009,20.2304710783648,
20.7273272538287,21.2241834292926,21.7210396047565,21.9911485751284),
 .UNSPECIFIED.);
#549=B_SPLINE_CURVE_WITH_KNOTS('',3,(#54583,#54584,#54585,#54586,#54587,
#54588),.UNSPECIFIED.,.F.,.F.,(4,2,4),(1.24930475438316,1.32474647948235,
1.35964937634907),.UNSPECIFIED.);
#550=B_SPLINE_CURVE_WITH_KNOTS('',3,(#54592,#54593,#54594,#54595,#54596,
#54597),.UNSPECIFIED.,.F.,.F.,(4,2,4),(2.01985300176811,2.05475589863482,
2.13019762373402),.UNSPECIFIED.);
#551=B_SPLINE_CURVE_WITH_KNOTS('',3,(#54601,#54602,#54603,#54604,#54605,
#54606),.UNSPECIFIED.,.F.,.F.,(4,2,4),(1.37814295771516,1.44140883836305,
1.62581583254081),.UNSPECIFIED.);
#552=B_SPLINE_CURVE_WITH_KNOTS('',3,(#54611,#54612,#54613,#54614,#54615,
#54616),.UNSPECIFIED.,.F.,.F.,(4,2,4),(0.304528093930702,0.488935088108449,
0.552200968756327),.UNSPECIFIED.);
#553=B_SPLINE_CURVE_WITH_KNOTS('',3,(#55126,#55127,#55128,#55129,#55130,
#55131,#55132,#55133,#55134,#55135,#55136,#55137,#55138,#55139,#55140,#55141,
#55142,#55143,#55144,#55145,#55146,#55147,#55148,#55149,#55150,#55151,#55152,
#55153,#55154,#55155,#55156,#55157,#55158,#55159,#55160,#55161,#55162,#55163,
#55164,#55165,#55166,#55167,#55168,#55169,#55170,#55171,#55172,#55173,#55174,
#55175,#55176,#55177,#55178,#55179,#55180,#55181,#55182,#55183,#55184,#55185,
#55186,#55187,#55188,#55189,#55190,#55191,#55192,#55193,#55194,#55195),
 .UNSPECIFIED.,.F.,.F.,(4,3,3,3,3,3,3,3,3,3,3,3,3,3,3,3,3,3,3,3,3,3,3,4),
(-1.12653966532784,-1.07791284579513,-1.00627166369148,-0.975917193634812,
-0.952635853583719,-0.87199198548212,-0.838272376334598,-0.807100731568119,
-0.791348117380521,-0.706129223773583,-0.652889761761131,-0.609381973014515,
-0.592572314772667,-0.515924705075137,-0.449963675677705,-0.408777239733258,
-0.38387026404303,-0.303419416195181,-0.252080587485408,-0.210187153834583,
-0.192153499962817,-0.113410122196938,-0.0362644966227604,0.),
 .UNSPECIFIED.);
#554=B_SPLINE_CURVE_WITH_KNOTS('',3,(#55196,#55197,#55198,#55199,#55200,
#55201,#55202,#55203,#55204,#55205,#55206,#55207,#55208),.UNSPECIFIED.,
 .F.,.F.,(4,3,3,3,4),(57.6675228581539,58.132172529274,58.6290287047379,
59.1258848802017,59.540361568735),.UNSPECIFIED.);
#555=B_SPLINE_CURVE_WITH_KNOTS('',3,(#55210,#55211,#55212,#55213,#55214,
#55215,#55216,#55217,#55218,#55219,#55220,#55221,#55222,#55223,#55224,#55225,
#55226,#55227,#55228,#55229,#55230,#55231,#55232,#55233,#55234,#55235,#55236,
#55237,#55238,#55239,#55240,#55241,#55242,#55243,#55244,#55245,#55246,#55247,
#55248,#55249,#55250,#55251,#55252,#55253,#55254,#55255,#55256,#55257,#55258,
#55259,#55260,#55261,#55262,#55263,#55264,#55265,#55266,#55267,#55268,#55269,
#55270,#55271,#55272,#55273,#55274,#55275,#55276,#55277,#55278,#55279,#55280,
#55281,#55282),.UNSPECIFIED.,.F.,.F.,(4,3,3,3,3,3,3,3,3,3,3,3,3,3,3,3,3,
3,3,3,3,3,3,3,4),(-1.13094109509753,-1.08988621442462,-1.02623856510858,
-0.99990765431054,-0.977647266785332,-0.906471441972912,-0.86986196121636,
-0.849824332611437,-0.835295617160493,-0.754157668591607,-0.69774970321115,
-0.665341988519394,-0.646352894702414,-0.568514140338012,-0.498888759264482,
-0.450432449598662,-0.43165692008954,-0.3454740206994,-0.290012616043892,
-0.246552828904893,-0.227983530411117,-0.208332983604929,-0.120797508811736,
-0.0326135798270653,0.),.UNSPECIFIED.);
#556=B_SPLINE_CURVE_WITH_KNOTS('',3,(#55283,#55284,#55285,#55286,#55287,
#55288,#55289,#55290,#55291,#55292,#55293,#55294,#55295,#55296),
 .UNSPECIFIED.,.F.,.F.,(4,1,1,1,1,1,1,1,1,1,1,4),(10.3757270560179,10.7902037445511,
11.287059920015,11.7839160954788,12.2807722709427,12.7776284464066,13.2744846218705,
13.7713407973344,14.2681969727983,14.7650531482621,15.261909323726,15.707963267949),
 .UNSPECIFIED.);
#557=B_SPLINE_CURVE_WITH_KNOTS('',3,(#55302,#55303,#55304,#55305,#55306,
#55307,#55308,#55309,#55310,#55311,#55312,#55313,#55314,#55315,#55316,#55317,
#55318,#55319,#55320,#55321,#55322,#55323,#55324,#55325,#55326,#55327,#55328,
#55329,#55330,#55331,#55332,#55333,#55334,#55335,#55336,#55337,#55338,#55339,
#55340,#55341,#55342,#55343,#55344,#55345,#55346,#55347,#55348,#55349,#55350,
#55351,#55352,#55353,#55354,#55355,#55356,#55357,#55358,#55359,#55360,#55361,
#55362,#55363,#55364,#55365,#55366,#55367,#55368,#55369,#55370,#55371),
 .UNSPECIFIED.,.F.,.F.,(4,3,3,3,3,3,3,3,3,3,3,3,3,3,3,3,3,3,3,3,3,3,3,4),
(-1.12653966532731,-1.07791284579463,-1.00627166369101,-0.975917194204177,
-0.95263585451432,-0.871991985947238,-0.838272377152255,-0.807100731340879,
-0.791348117380156,-0.706129223198138,-0.652889760315732,-0.609381971117541,
-0.592572311998026,-0.515924705075022,-0.449963675677601,-0.408777239776112,
-0.383870264177339,-0.303419423550715,-0.252080587485339,-0.210187156883604,
-0.192153502404281,-0.113410122957933,-0.0362644804108878,0.),
 .UNSPECIFIED.);
#558=B_SPLINE_CURVE_WITH_KNOTS('',3,(#55374,#55375,#55376,#55377,#55378,
#55379,#55380,#55381,#55382,#55383,#55384,#55385),.UNSPECIFIED.,.F.,.F.,
(4,1,1,1,1,1,1,1,1,4),(11.6154215191106,12.1122776945745,12.6091338700384,
13.1059900455022,13.6028462209661,14.09970239643,14.5965585718939,15.0934147473578,
15.5902709228216,15.707963267949),.UNSPECIFIED.);
#559=B_SPLINE_CURVE_WITH_KNOTS('',3,(#55895,#55896,#55897,#55898,#55899,
#55900,#55901,#55902,#55903,#55904,#55905,#55906,#55907,#55908,#55909,#55910,
#55911,#55912,#55913,#55914,#55915,#55916,#55917,#55918,#55919,#55920,#55921,
#55922,#55923,#55924,#55925,#55926,#55927,#55928,#55929,#55930,#55931,#55932,
#55933,#55934,#55935,#55936,#55937,#55938,#55939,#55940,#55941,#55942,#55943,
#55944,#55945,#55946,#55947,#55948,#55949,#55950,#55951,#55952,#55953,#55954,
#55955,#55956,#55957,#55958,#55959,#55960,#55961,#55962,#55963,#55964,#55965,
#55966,#55967),.UNSPECIFIED.,.F.,.F.,(4,3,3,3,3,3,3,3,3,3,3,3,3,3,3,3,3,
3,3,3,3,3,3,3,4),(-1.1309410950982,-1.08988621442528,-1.02623856510918,
-0.999907655386809,-0.977647267153864,-0.90647144215737,-0.869861961640259,
-0.849824333087064,-0.835295617160877,-0.754157668032784,-0.697749702842735,
-0.665341988113398,-0.646352894567368,-0.568514140338249,-0.498888759264689,
-0.450432451491543,-0.431656923063295,-0.345474023991194,-0.290012616044011,
-0.246552826042169,-0.227983526261251,-0.208332982535075,-0.12079751549492,
-0.032613578905637,0.),.UNSPECIFIED.);
#560=B_SPLINE_CURVE_WITH_KNOTS('',3,(#55968,#55969,#55970,#55971,#55972,
#55973,#55974),.UNSPECIFIED.,.F.,.F.,(4,3,4),(-61.6101657575211,-61.1133095820573,
-60.6412095134547),.UNSPECIFIED.);
#561=B_SPLINE_CURVE_WITH_KNOTS('',3,(#55977,#55978,#55979,#55980,#55981,
#55982,#55983,#55984,#55985,#55986,#55987,#55988,#55989,#55990,#55991),
 .UNSPECIFIED.,.F.,.F.,(4,2,2,2,3,2,4),(-1.19807229539725,-0.896265761725941,
-0.594459228054633,-0.297229614027317,0.,0.313277269702133,0.551840138348627),
 .UNSPECIFIED.);
#562=B_SPLINE_CURVE_WITH_KNOTS('',3,(#55999,#56000,#56001,#56002,#56003,
#56004,#56005,#56006,#56007,#56008,#56009,#56010,#56011,#56012),
 .UNSPECIFIED.,.F.,.F.,(4,2,2,2,2,2,4),(-2.9479847291431,-2.70942186049663,
-2.3961445907945,-2.09891497676718,-1.80168536273986,-1.49987882906855,
-1.19807229539725),.UNSPECIFIED.);
#563=B_SPLINE_CURVE_WITH_KNOTS('',3,(#56042,#56043,#56044,#56045,#56046,
#56047,#56048,#56049,#56050,#56051,#56052,#56053,#56054,#56055,#56056,#56057,
#56058,#56059,#56060,#56061,#56062,#56063,#56064,#56065,#56066,#56067),
 .UNSPECIFIED.,.F.,.F.,(4,2,2,2,2,2,2,2,2,2,2,2,4),(0.,0.379021281688117,
0.758042563376235,1.13697172150512,1.515900879634,1.89483003776288,2.27375919589176,
2.65278047757987,3.03180175926799,3.41082304095611,3.78984432264423,4.16877348077311,
4.54770263890199),.UNSPECIFIED.);
#564=B_SPLINE_CURVE_WITH_KNOTS('',3,(#56068,#56069,#56070,#56071,#56072,
#56073,#56074,#56075,#56076,#56077),.UNSPECIFIED.,.F.,.F.,(4,2,2,2,4),(4.54770263890199,
4.92663179703087,5.30556095515975,5.68458223684787,6.06360351853598),
 .UNSPECIFIED.);
#565=B_SPLINE_CURVE_WITH_KNOTS('',3,(#56093,#56094,#56095,#56096,#56097,
#56098,#56099,#56100,#56101,#56102),.UNSPECIFIED.,.F.,.F.,(4,3,3,4),(-4.09274904019424,
-3.99377421359647,-2.99533066019735,-2.06120159751578),.UNSPECIFIED.);
#566=B_SPLINE_CURVE_WITH_KNOTS('',3,(#56105,#56106,#56107,#56108,#56109,
#56110,#56111),.UNSPECIFIED.,.F.,.F.,(4,3,4),(0.,0.998443553399126,1.11004521091126),
 .UNSPECIFIED.);
#567=B_SPLINE_CURVE_WITH_KNOTS('',3,(#56116,#56117,#56118,#56119,#56120,
#56121,#56122,#56123,#56124,#56125,#56126,#56127,#56128,#56129,#56130,#56131,
#56132,#56133,#56134,#56135,#56136,#56137),.UNSPECIFIED.,.F.,.F.,(4,3,3,
3,3,3,3,4),(-10.3759343473738,-9.98443553399116,-8.98599198059205,-7.98754842719293,
-6.98910487379382,-5.9906613203947,-4.99221776699558,-4.09274904019424),
 .UNSPECIFIED.);
#568=B_SPLINE_CURVE_WITH_KNOTS('',3,(#56138,#56139,#56140,#56141,#56142,
#56143,#56144,#56145,#56146,#56147,#56148,#56149,#56150,#56151,#56152,#56153,
#56154,#56155,#56156,#56157,#56158,#56159),.UNSPECIFIED.,.F.,.F.,(4,3,3,
3,3,3,3,4),(1.11004521091126,1.99688710679824,2.99533066019736,3.99377421359647,
4.99221776699558,5.9906613203947,6.98910487379381,7.39323051809085),
 .UNSPECIFIED.);
#569=B_SPLINE_CURVE_WITH_KNOTS('',3,(#56164,#56165,#56166,#56167,#56168,
#56169,#56170,#56171,#56172,#56173,#56174,#56175,#56176,#56177,#56178,#56179,
#56180,#56181,#56182,#56183,#56184,#56185),.UNSPECIFIED.,.F.,.F.,(4,3,3,
3,3,3,3,4),(-16.6591196545534,-15.9750968543859,-14.9766533009867,-13.9782097475876,
-12.9797661941885,-11.9813226407894,-10.9828790873903,-10.3759343473738),
 .UNSPECIFIED.);
#570=B_SPLINE_CURVE_WITH_KNOTS('',3,(#56186,#56187,#56188,#56189,#56190,
#56191,#56192,#56193,#56194,#56195,#56196,#56197,#56198,#56199,#56200,#56201,
#56202,#56203,#56204,#56205,#56206,#56207),.UNSPECIFIED.,.F.,.F.,(4,3,3,
3,3,3,3,4),(7.39323051809085,7.98754842719293,8.98599198059204,9.98443553399115,
10.9828790873903,11.9813226407894,12.9797661941885,13.6764158252704),
 .UNSPECIFIED.);
#571=B_SPLINE_CURVE_WITH_KNOTS('',3,(#56212,#56213,#56214,#56215,#56216,
#56217,#56218,#56219,#56220,#56221,#56222,#56223,#56224,#56225,#56226,#56227,
#56228,#56229,#56230,#56231,#56232,#56233),.UNSPECIFIED.,.F.,.F.,(4,3,3,
3,3,3,3,4),(-22.942304961733,-21.9657581747806,-20.9673146213814,-19.9688710679823,
-18.9704275145832,-17.9719839611841,-16.973540407785,-16.6591196545534),
 .UNSPECIFIED.);
#572=B_SPLINE_CURVE_WITH_KNOTS('',3,(#56234,#56235,#56236,#56237,#56238,
#56239,#56240,#56241,#56242,#56243,#56244,#56245,#56246,#56247,#56248,#56249,
#56250,#56251,#56252,#56253,#56254,#56255),.UNSPECIFIED.,.F.,.F.,(4,3,3,
3,3,3,3,4),(13.6764158252704,13.9782097475876,14.9766533009867,15.9750968543859,
16.973540407785,17.9719839611841,18.9704275145832,19.95960113245),
 .UNSPECIFIED.);
#573=B_SPLINE_CURVE_WITH_KNOTS('',3,(#56260,#56261,#56262,#56263,#56264,
#56265,#56266,#56267,#56268,#56269,#56270,#56271,#56272,#56273,#56274,#56275,
#56276,#56277,#56278,#56279,#56280,#56281,#56282,#56283,#56284),
 .UNSPECIFIED.,.F.,.F.,(4,3,3,3,3,3,3,3,4),(-29.2254902689126,-28.9548630485744,
-27.9564194951753,-26.9579759417761,-25.959532388377,-24.9610888349779,
-23.9626452815788,-22.9642017281797,-22.942304961733),.UNSPECIFIED.);
#574=B_SPLINE_CURVE_WITH_KNOTS('',3,(#56285,#56286,#56287,#56288,#56289,
#56290,#56291,#56292,#56293,#56294,#56295,#56296,#56297,#56298,#56299,#56300,
#56301,#56302,#56303,#56304,#56305,#56306,#56307,#56308,#56309),
 .UNSPECIFIED.,.F.,.F.,(4,3,3,3,3,3,3,3,4),(19.95960113245,19.9688710679823,
20.9673146213814,21.9657581747806,22.9642017281797,23.9626452815788,24.9610888349779,
25.959532388377,26.2427864396296),.UNSPECIFIED.);
#575=B_SPLINE_CURVE_WITH_KNOTS('',3,(#56314,#56315,#56316,#56317,#56318,
#56319,#56320,#56321,#56322,#56323,#56324,#56325,#56326,#56327,#56328,#56329,
#56330,#56331,#56332,#56333,#56334,#56335),.UNSPECIFIED.,.F.,.F.,(4,3,3,
3,3,3,3,4),(-35.5086755760922,-34.9455243689691,-33.94708081557,-32.9486372621708,
-31.9501937087717,-30.9517501553726,-29.9533066019735,-29.2254902689126),
 .UNSPECIFIED.);
#576=B_SPLINE_CURVE_WITH_KNOTS('',3,(#56336,#56337,#56338,#56339,#56340,
#56341,#56342,#56343,#56344,#56345,#56346,#56347,#56348,#56349,#56350,#56351,
#56352,#56353,#56354,#56355,#56356,#56357),.UNSPECIFIED.,.F.,.F.,(4,3,3,
3,3,3,3,4),(26.2427864396296,26.9579759417761,27.9564194951753,28.9548630485744,
29.9533066019735,30.9517501553726,31.9501937087717,32.5259717468092),
 .UNSPECIFIED.);
#577=B_SPLINE_CURVE_WITH_KNOTS('',3,(#56362,#56363,#56364,#56365,#56366,
#56367,#56368,#56369,#56370,#56371,#56372,#56373,#56374,#56375,#56376,#56377,
#56378,#56379,#56380,#56381,#56382,#56383),.UNSPECIFIED.,.F.,.F.,(4,3,3,
3,3,3,3,4),(-41.7918608832718,-40.9361856893638,-39.9377421359646,-38.9392985825655,
-37.9408550291664,-36.9424114757673,-35.9439679223682,-35.5086755760922),
 .UNSPECIFIED.);
#578=B_SPLINE_CURVE_WITH_KNOTS('',3,(#56384,#56385,#56386,#56387,#56388,
#56389,#56390,#56391,#56392,#56393,#56394,#56395,#56396,#56397,#56398,#56399,
#56400,#56401,#56402,#56403,#56404,#56405),.UNSPECIFIED.,.F.,.F.,(4,3,3,
3,3,3,3,4),(32.5259717468092,32.9486372621708,33.9470808155699,34.9455243689691,
35.9439679223682,36.9424114757673,37.9408550291664,38.8091570539888),
 .UNSPECIFIED.);
#579=B_SPLINE_CURVE_WITH_KNOTS('',3,(#56410,#56411,#56412,#56413,#56414,
#56415,#56416,#56417,#56418,#56419,#56420,#56421,#56422,#56423,#56424,#56425,
#56426,#56427,#56428,#56429,#56430,#56431,#56432,#56433,#56434),
 .UNSPECIFIED.,.F.,.F.,(4,3,3,3,3,3,3,3,4),(-48.0750461904514,-47.9252905631576,
-46.9268470097585,-45.9284034563593,-44.9299599029602,-43.9315163495611,
-42.933072796162,-41.9346292427629,-41.7918608832718),.UNSPECIFIED.);
#580=B_SPLINE_CURVE_WITH_KNOTS('',3,(#56435,#56436,#56437,#56438,#56439,
#56440,#56441,#56442,#56443,#56444,#56445,#56446,#56447,#56448,#56449,#56450,
#56451,#56452,#56453,#56454,#56455,#56456,#56457,#56458,#56459),
 .UNSPECIFIED.,.F.,.F.,(4,3,3,3,3,3,3,3,4),(38.8091570539888,38.9392985825655,
39.9377421359646,40.9361856893638,41.9346292427629,42.933072796162,43.9315163495611,
44.9299599029602,45.0923423611684),.UNSPECIFIED.);
#581=B_SPLINE_CURVE_WITH_KNOTS('',3,(#56464,#56465,#56466,#56467,#56468,
#56469,#56470,#56471,#56472,#56473,#56474,#56475,#56476,#56477,#56478,#56479,
#56480,#56481,#56482,#56483,#56484,#56485),.UNSPECIFIED.,.F.,.F.,(4,3,3,
3,3,3,3,4),(-54.358231497631,-53.9159518835523,-52.9175083301532,-51.9190647767541,
-50.9206212233549,-49.9221776699558,-48.9237341165567,-48.0750461904514),
 .UNSPECIFIED.);
#582=B_SPLINE_CURVE_WITH_KNOTS('',3,(#56486,#56487,#56488,#56489,#56490,
#56491,#56492,#56493,#56494,#56495,#56496,#56497,#56498,#56499,#56500,#56501,
#56502,#56503,#56504,#56505,#56506,#56507),.UNSPECIFIED.,.F.,.F.,(4,3,3,
3,3,3,3,4),(45.0923423611684,45.9284034563593,46.9268470097585,47.9252905631576,
48.9237341165567,49.9221776699558,50.9206212233549,51.375527668348),
 .UNSPECIFIED.);
#583=B_SPLINE_CURVE_WITH_KNOTS('',3,(#56512,#56513,#56514,#56515,#56516,
#56517,#56518,#56519,#56520,#56521,#56522,#56523,#56524,#56525,#56526,#56527,
#56528,#56529,#56530,#56531,#56532,#56533),.UNSPECIFIED.,.F.,.F.,(4,3,3,
3,3,3,3,4),(-60.6414168048105,-59.906613203947,-58.9081696505479,-57.9097260971487,
-56.9112825437496,-55.9128389903505,-54.9143954369514,-54.358231497631),
 .UNSPECIFIED.);
#584=B_SPLINE_CURVE_WITH_KNOTS('',3,(#56534,#56535,#56536,#56537,#56538,
#56539,#56540,#56541,#56542,#56543,#56544,#56545,#56546,#56547,#56548,#56549,
#56550,#56551,#56552,#56553,#56554,#56555),.UNSPECIFIED.,.F.,.F.,(4,3,3,
3,3,3,3,4),(51.375527668348,51.919064776754,52.9175083301532,53.9159518835523,
54.9143954369514,55.9128389903505,56.9112825437496,57.6587129755276),
 .UNSPECIFIED.);
#585=B_SPLINE_CURVE_WITH_KNOTS('',3,(#56560,#56561,#56562,#56563,#56564,
#56565,#56566,#56567,#56568,#56569,#56570,#56571,#56572,#56573,#56574,#56575,
#56576,#56577,#56578,#56579,#56580,#56581,#56582,#56583,#56584),
 .UNSPECIFIED.,.F.,.F.,(4,3,3,3,3,3,3,3,4),(-66.9246021119901,-66.8957180777408,
-65.8972745243417,-64.8988309709426,-63.9003874175434,-62.9019438641443,
-61.9035003107452,-60.9050567573461,-60.6414168048105),.UNSPECIFIED.);
#586=B_SPLINE_CURVE_WITH_KNOTS('',3,(#56585,#56586,#56587,#56588,#56589,
#56590,#56591,#56592,#56593,#56594,#56595,#56596,#56597,#56598,#56599,#56600,
#56601,#56602,#56603,#56604,#56605,#56606,#56607,#56608,#56609),
 .UNSPECIFIED.,.F.,.F.,(4,3,3,3,3,3,3,3,4),(57.6587129755276,57.9097260971487,
58.9081696505479,59.906613203947,60.9050567573461,61.9035003107452,62.9019438641443,
63.9003874175434,63.9418982827071),.UNSPECIFIED.);
#587=B_SPLINE_CURVE_WITH_KNOTS('',3,(#56614,#56615,#56616,#56617,#56618,
#56619,#56620,#56621,#56622,#56623,#56624,#56625,#56626,#56627,#56628,#56629,
#56630,#56631,#56632,#56633,#56634,#56635),.UNSPECIFIED.,.F.,.F.,(4,3,3,
3,3,3,3,4),(-73.2077874191697,-72.8863793981355,-71.8879358447363,-70.8894922913372,
-69.8910487379381,-68.892605184539,-67.8941616311399,-66.9246021119901),
 .UNSPECIFIED.);
#588=B_SPLINE_CURVE_WITH_KNOTS('',3,(#56636,#56637,#56638,#56639,#56640,
#56641,#56642,#56643,#56644,#56645,#56646,#56647,#56648,#56649,#56650,#56651,
#56652,#56653,#56654,#56655,#56656,#56657),.UNSPECIFIED.,.F.,.F.,(4,3,3,
3,3,3,3,4),(63.9418982827071,64.8988309709426,65.8972745243417,66.8957180777408,
67.8941616311399,68.892605184539,69.8910487379381,70.2250835898868),
 .UNSPECIFIED.);
#589=B_SPLINE_CURVE_WITH_KNOTS('',3,(#56662,#56663,#56664,#56665,#56666,
#56667,#56668,#56669,#56670,#56671,#56672,#56673,#56674,#56675,#56676,#56677,
#56678,#56679,#56680,#56681,#56682,#56683),.UNSPECIFIED.,.F.,.F.,(4,3,3,
3,3,3,3,4),(-79.4909727263493,-78.8770407185302,-77.8785971651311,-76.8801536117319,
-75.8817100583328,-74.8832665049337,-73.8848229515346,-73.2077874191697),
 .UNSPECIFIED.);
#590=B_SPLINE_CURVE_WITH_KNOTS('',3,(#56684,#56685,#56686,#56687,#56688,
#56689,#56690,#56691,#56692,#56693,#56694,#56695,#56696,#56697,#56698,#56699,
#56700,#56701,#56702,#56703,#56704,#56705),.UNSPECIFIED.,.F.,.F.,(4,3,3,
3,3,3,3,4),(70.2250835898868,70.8894922913372,71.8879358447364,72.8863793981355,
73.8848229515346,74.8832665049337,75.8817100583328,76.5082688970663),
 .UNSPECIFIED.);
#591=B_SPLINE_CURVE_WITH_KNOTS('',3,(#56710,#56711,#56712,#56713,#56714,
#56715,#56716,#56717,#56718,#56719,#56720,#56721,#56722,#56723,#56724,#56725,
#56726,#56727,#56728,#56729,#56730,#56731),.UNSPECIFIED.,.F.,.F.,(4,3,3,
3,3,3,3,4),(-85.7741580335289,-84.8677020389249,-83.8692584855258,-82.8708149321266,
-81.8723713787275,-80.8739278253284,-79.8754842719293,-79.4909727263493),
 .UNSPECIFIED.);
#592=B_SPLINE_CURVE_WITH_KNOTS('',3,(#56732,#56733,#56734,#56735,#56736,
#56737,#56738,#56739,#56740,#56741,#56742,#56743,#56744,#56745,#56746,#56747,
#56748,#56749,#56750,#56751,#56752,#56753),.UNSPECIFIED.,.F.,.F.,(4,3,3,
3,3,3,3,4),(76.5082688970663,76.8801536117319,77.8785971651311,78.8770407185302,
79.8754842719293,80.8739278253284,81.8723713787275,82.7914542042459),
 .UNSPECIFIED.);
#593=B_SPLINE_CURVE_WITH_KNOTS('',3,(#56759,#56760,#56761,#56762,#56763,
#56764),.UNSPECIFIED.,.F.,.F.,(4,1,1,4),(97.3893722612836,97.4813598200786,
98.4798033734778,99.4139324361594),.UNSPECIFIED.);
#594=B_SPLINE_CURVE_WITH_KNOTS('',3,(#56767,#56768,#56769,#56770),
 .UNSPECIFIED.,.F.,.F.,(4,4),(97.3893722612836,98.1746525557784),
 .UNSPECIFIED.);
#595=B_SPLINE_CURVE_WITH_KNOTS('',3,(#56775,#56776,#56777,#56778,#56779,
#56780,#56781,#56782,#56783,#56784),.UNSPECIFIED.,.F.,.F.,(4,1,1,1,1,1,
1,4),(91.106186954104,91.4906984996839,92.4891420530831,93.4875856064822,
94.4860291598813,95.4844727132804,96.4829162666795,97.3893722612836),
 .UNSPECIFIED.);
#596=B_SPLINE_CURVE_WITH_KNOTS('',3,(#56785,#56786,#56787,#56788,#56789,
#56790,#56791,#56792,#56793,#56794,#56795),.UNSPECIFIED.,.F.,.F.,(4,1,1,
1,1,1,1,1,4),(91.106186954104,91.1855476819846,92.1839912353837,93.1824347887828,
94.1808783421819,95.1793218955811,96.1777654489802,97.1762090023793,97.3893722612836),
 .UNSPECIFIED.);
#597=B_SPLINE_CURVE_WITH_KNOTS('',3,(#56800,#56801,#56802,#56803,#56804,
#56805,#56806,#56807,#56808,#56809),.UNSPECIFIED.,.F.,.F.,(4,1,1,1,1,1,
1,4),(84.8230016469244,85.5000371792893,86.4984807326884,87.4969242860875,
88.4953678394866,89.4938113928857,90.4922549462848,91.106186954104),
 .UNSPECIFIED.);
#598=B_SPLINE_CURVE_WITH_KNOTS('',3,(#56810,#56811,#56812,#56813,#56814,
#56815,#56816,#56817,#56818,#56819),.UNSPECIFIED.,.F.,.F.,(4,1,1,1,1,1,
1,4),(84.8230016469244,85.1948863615899,86.193329914989,87.1917734683881,
88.1902170217872,89.1886605751864,90.1871041285855,91.106186954104),
 .UNSPECIFIED.);
#599=B_SPLINE_CURVE_WITH_KNOTS('',3,(#56824,#56825,#56826,#56827,#56828,
#56829,#56830,#56831,#56832,#56833),.UNSPECIFIED.,.F.,.F.,(4,1,1,1,1,1,
1,4),(78.5398163397448,79.5093758588945,80.5078194122937,81.5062629656928,
82.5047065190919,83.503150072491,84.5015936258901,84.8230016469244),
 .UNSPECIFIED.);
#600=B_SPLINE_CURVE_WITH_KNOTS('',3,(#56834,#56835,#56836,#56837,#56838,
#56839,#56840,#56841,#56842,#56843),.UNSPECIFIED.,.F.,.F.,(4,1,1,1,1,1,
1,4),(78.5398163397448,79.2042250411952,80.2026685945943,81.2011121479934,
82.1995557013926,83.1979992547917,84.1964428081908,84.8230016469244),
 .UNSPECIFIED.);
#601=B_SPLINE_CURVE_WITH_KNOTS('',3,(#56848,#56849,#56850,#56851,#56852,
#56853,#56854,#56855,#56856,#56857,#56858),.UNSPECIFIED.,.F.,.F.,(4,1,1,
1,1,1,1,1,4),(72.2566310325652,72.5202709851007,73.5187145384999,74.517158091899,
75.5156016452981,76.5140451986972,77.5124887520963,78.5109323054954,78.5398163397448),
 .UNSPECIFIED.);
#602=B_SPLINE_CURVE_WITH_KNOTS('',3,(#56859,#56860,#56861,#56862,#56863,
#56864,#56865,#56866,#56867,#56868),.UNSPECIFIED.,.F.,.F.,(4,1,1,1,1,1,
1,4),(72.2566310325652,73.2135637208005,74.2120072741996,75.2104508275987,
76.2088943809979,77.207337934397,78.2057814877961,78.5398163397448),
 .UNSPECIFIED.);
#603=B_SPLINE_CURVE_WITH_KNOTS('',3,(#56873,#56874,#56875,#56876,#56877,
#56878,#56879,#56880,#56881,#56882),.UNSPECIFIED.,.F.,.F.,(4,1,1,1,1,1,
1,4),(65.9734457253856,66.529609664706,67.5280532181052,68.5264967715043,
69.5249403249034,70.5233838783025,71.5218274317016,72.2566310325652),
 .UNSPECIFIED.);
#604=B_SPLINE_CURVE_WITH_KNOTS('',3,(#56883,#56884,#56885,#56886,#56887,
#56888,#56889,#56890,#56891,#56892,#56893),.UNSPECIFIED.,.F.,.F.,(4,1,1,
1,1,1,1,1,4),(65.9734457253856,66.2244588470067,67.2229024004058,68.2213459538049,
69.219789507204,70.2182330606032,71.2166766140023,72.2151201674014,72.2566310325652),
 .UNSPECIFIED.);
#605=B_SPLINE_CURVE_WITH_KNOTS('',3,(#56898,#56899,#56900,#56901,#56902,
#56903,#56904,#56905,#56906,#56907),.UNSPECIFIED.,.F.,.F.,(4,1,1,1,1,1,
1,4),(59.690260418206,60.5389483443114,61.5373918977105,62.5358354511096,
63.5342790045087,64.5327225579078,65.5311661113069,65.9734457253856),
 .UNSPECIFIED.);
#606=B_SPLINE_CURVE_WITH_KNOTS('',3,(#56908,#56909,#56910,#56911,#56912,
#56913,#56914,#56915,#56916,#56917),.UNSPECIFIED.,.F.,.F.,(4,1,1,1,1,1,
1,4),(59.690260418206,60.233797526612,61.2322410800111,62.2306846334102,
63.2291281868093,64.2275717402085,65.2260152936076,65.9734457253856),
 .UNSPECIFIED.);
#607=B_SPLINE_CURVE_WITH_KNOTS('',3,(#56922,#56923,#56924,#56925,#56926,
#56927,#56928,#56929,#56930,#56931,#56932),.UNSPECIFIED.,.F.,.F.,(4,1,1,
1,1,1,1,1,4),(53.4070751110264,53.5498434705175,54.5482870239167,55.5467305773158,
56.5451741307149,57.543617684114,58.5420612375131,59.5405047909122,59.690260418206),
 .UNSPECIFIED.);
#608=B_SPLINE_CURVE_WITH_KNOTS('',3,(#56933,#56934,#56935,#56936,#56937,
#56938,#56939,#56940,#56941,#56942),.UNSPECIFIED.,.F.,.F.,(4,1,1,1,1,1,
1,4),(53.4070751110264,54.2431362062173,55.2415797596164,56.2400233130155,
57.2384668664147,58.2369104198138,59.2353539732129,59.690260418206),
 .UNSPECIFIED.);
#609=B_SPLINE_CURVE_WITH_KNOTS('',3,(#56947,#56948,#56949,#56950,#56951,
#56952,#56953,#56954,#56955,#56956),.UNSPECIFIED.,.F.,.F.,(4,1,1,1,1,1,
1,4),(47.1238898038469,47.5591821501228,48.557625703522,49.5560692569211,
50.5545128103202,51.5529563637193,52.5513999171184,53.4070751110264),
 .UNSPECIFIED.);
#610=B_SPLINE_CURVE_WITH_KNOTS('',3,(#56957,#56958,#56959,#56960,#56961,
#56962,#56963,#56964,#56965,#56966,#56967),.UNSPECIFIED.,.F.,.F.,(4,1,1,
1,1,1,1,1,4),(47.1238898038468,47.2540313324235,48.2524748858226,49.2509184392217,
50.2493619926208,51.2478055460199,52.2462490994191,53.2446926528182,53.4070751110264),
 .UNSPECIFIED.);
#611=B_SPLINE_CURVE_WITH_KNOTS('',3,(#56972,#56973,#56974,#56975,#56976,
#56977,#56978,#56979,#56980,#56981),.UNSPECIFIED.,.F.,.F.,(4,1,1,1,1,1,
1,4),(40.8407044966673,41.5685208297281,42.5669643831273,43.5654079365264,
44.5638514899255,45.5622950433246,46.5607385967237,47.1238898038469),
 .UNSPECIFIED.);
#612=B_SPLINE_CURVE_WITH_KNOTS('',3,(#56982,#56983,#56984,#56985,#56986,
#56987,#56988,#56989,#56990,#56991),.UNSPECIFIED.,.F.,.F.,(4,1,1,1,1,1,
1,4),(40.8407044966672,41.2633700120288,42.2618135654279,43.260257118827,
44.2587006722261,45.2571442256253,46.2555877790244,47.1238898038468),
 .UNSPECIFIED.);
#613=B_SPLINE_CURVE_WITH_KNOTS('',3,(#56996,#56997,#56998,#56999,#57000,
#57001,#57002,#57003,#57004,#57005,#57006),.UNSPECIFIED.,.F.,.F.,(4,1,1,
1,1,1,1,1,4),(34.5575191894877,34.5794159559343,35.5778595093334,36.5763030627326,
37.5747466161317,38.5731901695308,39.5716337229299,40.570077276329,40.8407044966673),
 .UNSPECIFIED.);
#614=B_SPLINE_CURVE_WITH_KNOTS('',3,(#57007,#57008,#57009,#57010,#57011,
#57012,#57013,#57014,#57015,#57016),.UNSPECIFIED.,.F.,.F.,(4,1,1,1,1,1,
1,4),(34.5575191894877,35.2727086916341,36.2711522450332,37.2695957984323,
38.2680393518314,39.2664829052306,40.2649264586297,40.8407044966672),
 .UNSPECIFIED.);
#615=B_SPLINE_CURVE_WITH_KNOTS('',3,(#57021,#57022,#57023,#57024,#57025,
#57026,#57027,#57028,#57029,#57030),.UNSPECIFIED.,.F.,.F.,(4,1,1,1,1,1,
1,4),(28.2743338823081,28.5887546355396,29.5871981889387,30.5856417423379,
31.584085295737,32.5825288491361,33.5809724025352,34.5575191894877),
 .UNSPECIFIED.);
#616=B_SPLINE_CURVE_WITH_KNOTS('',3,(#57031,#57032,#57033,#57034,#57035,
#57036,#57037,#57038,#57039,#57040,#57041),.UNSPECIFIED.,.F.,.F.,(4,1,1,
1,1,1,1,1,4),(28.2743338823081,28.2836038178403,29.2820473712394,30.2804909246385,
31.2789344780376,32.2773780314368,33.2758215848359,34.274265138235,34.5575191894877),
 .UNSPECIFIED.);
#617=B_SPLINE_CURVE_WITH_KNOTS('',3,(#57046,#57047,#57048,#57049,#57050,
#57051,#57052,#57053,#57054,#57055),.UNSPECIFIED.,.F.,.F.,(4,1,1,1,1,1,
1,4),(21.9911485751285,22.5980933151449,23.596536868544,24.5949804219432,
25.5934239753423,26.5918675287414,27.5903110821405,28.2743338823081),
 .UNSPECIFIED.);
#618=B_SPLINE_CURVE_WITH_KNOTS('',3,(#57056,#57057,#57058,#57059,#57060,
#57061,#57062,#57063,#57064,#57065),.UNSPECIFIED.,.F.,.F.,(4,1,1,1,1,1,
1,4),(21.9911485751285,22.2929424974456,23.2913860508447,24.2898296042438,
25.2882731576429,26.2867167110421,27.2851602644412,28.2743338823081),
 .UNSPECIFIED.);
#619=B_SPLINE_CURVE_WITH_KNOTS('',3,(#57070,#57071,#57072,#57073,#57074,
#57075,#57076,#57077,#57078,#57079),.UNSPECIFIED.,.F.,.F.,(4,1,1,1,1,1,
1,4),(15.7079632679489,16.6074319947502,17.6058755481493,18.6043191015485,
19.6027626549476,20.6012062083467,21.5996497617458,21.9911485751285),
 .UNSPECIFIED.);
#620=B_SPLINE_CURVE_WITH_KNOTS('',3,(#57080,#57081,#57082,#57083,#57084,
#57085,#57086,#57087,#57088,#57089),.UNSPECIFIED.,.F.,.F.,(4,1,1,1,1,1,
1,4),(15.7079632679489,16.3022811770509,17.30072473045,18.2991682838491,
19.2976118372482,20.2960553906474,21.2944989440465,21.9911485751285),
 .UNSPECIFIED.);
#621=B_SPLINE_CURVE_WITH_KNOTS('',3,(#57463,#57464,#57465,#57466,#57467,
#57468,#57469,#57470,#57471,#57472,#57473,#57474,#57475,#57476,#57477,#57478,
#57479,#57480,#57481,#57482,#57483,#57484,#57485,#57486,#57487,#57488,#57489,
#57490,#57491,#57492,#57493,#57494,#57495,#57496,#57497,#57498,#57499,#57500,
#57501,#57502,#57503,#57504,#57505,#57506,#57507,#57508,#57509,#57510,#57511,
#57512,#57513,#57514,#57515,#57516,#57517,#57518,#57519,#57520,#57521,#57522,
#57523,#57524,#57525,#57526,#57527,#57528,#57529),.UNSPECIFIED.,.F.,.F.,
(4,3,3,3,3,3,3,3,3,3,3,3,3,3,3,3,3,3,3,3,3,3,4),(0.,0.0253593625170432,
0.0904989134578323,0.129428846004824,0.149433065046328,0.165907354496605,
0.229382007773891,0.27252109928886,0.293394884079185,0.307837377566809,
0.368130738221205,0.401938373833768,0.435421038291672,0.450805053840956,
0.511072272729441,0.551886900769997,0.571326828937518,0.587500892696757,
0.626725156815222,0.649859628114584,0.67177310859451,0.727376664730075,
0.744397949170617),.UNSPECIFIED.);
#622=B_SPLINE_CURVE_WITH_KNOTS('',3,(#57530,#57531,#57532,#57533,#57534,
#57535,#57536,#57537,#57538,#57539,#57540,#57541,#57542,#57543,#57544,#57545,
#57546,#57547,#57548),.UNSPECIFIED.,.F.,.F.,(4,3,3,3,3,3,4),(82.7914542042459,
82.8708149321266,83.8692584855257,84.8677020389248,85.866145592324,86.8645891457231,
87.7987182084047),.UNSPECIFIED.);
#623=B_SPLINE_CURVE_WITH_KNOTS('',3,(#57550,#57551,#57552,#57553,#57554,
#57555,#57556,#57557,#57558,#57559,#57560,#57561,#57562,#57563,#57564,#57565,
#57566,#57567,#57568,#57569,#57570,#57571,#57572,#57573,#57574,#57575,#57576,
#57577,#57578,#57579,#57580,#57581,#57582,#57583,#57584,#57585,#57586,#57587,
#57588,#57589,#57590,#57591,#57592,#57593,#57594,#57595,#57596,#57597,#57598,
#57599,#57600,#57601,#57602,#57603,#57604,#57605,#57606,#57607,#57608,#57609,
#57610,#57611,#57612,#57613,#57614,#57615,#57616),.UNSPECIFIED.,.F.,.F.,
(4,3,3,3,3,3,3,3,3,3,3,3,3,3,3,3,3,3,3,3,3,3,4),(-0.744397949170599,-0.723387897941471,
-0.677960034185854,-0.66030178031912,-0.64147849017529,-0.603260261907819,
-0.580027150555408,-0.559762047797058,-0.499485193698097,-0.461022451958816,
-0.43985149859123,-0.426322963973344,-0.378677517214829,-0.331342827562976,
-0.308500355626486,-0.284779303920441,-0.222455882654308,-0.166841911990731,
-0.151140787742428,-0.135611969270085,-0.0678059846350425,-0.00370004143489645,
0.),.UNSPECIFIED.);
#624=B_SPLINE_CURVE_WITH_KNOTS('',3,(#57617,#57618,#57619,#57620,#57621,
#57622,#57623,#57624,#57625),.UNSPECIFIED.,.F.,.F.,(4,1,1,1,1,1,4),(10.3759343473737,
11.3100634100553,12.3085069634544,13.3069505168535,14.3053940702527,15.3038376236518,
15.7079632679489),.UNSPECIFIED.);
#625=B_SPLINE_CURVE_WITH_KNOTS('',3,(#57631,#57632,#57633,#57634,#57635,
#57636,#57637,#57638,#57639,#57640,#57641,#57642,#57643,#57644,#57645,#57646,
#57647,#57648,#57649,#57650,#57651,#57652,#57653,#57654,#57655,#57656,#57657,
#57658,#57659,#57660,#57661,#57662,#57663,#57664,#57665,#57666,#57667,#57668,
#57669,#57670,#57671,#57672,#57673,#57674,#57675,#57676,#57677,#57678,#57679,
#57680,#57681,#57682,#57683,#57684,#57685,#57686,#57687,#57688,#57689,#57690,
#57691),.UNSPECIFIED.,.F.,.F.,(4,3,3,3,3,3,3,3,3,3,3,3,3,3,3,3,3,3,3,3,
4),(-0.741270768406348,-0.716021136741387,-0.669194981720871,-0.640215156661528,
-0.6210285893087,-0.556595143115658,-0.539229517462428,-0.476555392316448,
-0.415575701759323,-0.398642849264355,-0.383309668681598,-0.34141189657726,
-0.279171652021188,-0.261540829450543,-0.245638028402519,-0.184228521301889,
-0.133954283551423,-0.117989348492863,-0.0589946742464315,-0.00428452387123181,
0.),.UNSPECIFIED.);
#626=B_SPLINE_CURVE_WITH_KNOTS('',3,(#57694,#57695,#57696,#57697,#57698,
#57699,#57700,#57701),.UNSPECIFIED.,.F.,.F.,(4,1,1,1,1,4),(11.6152142277547,
12.6136577811538,13.6121013345529,14.610544887952,15.6089884413511,15.7079632679489),
 .UNSPECIFIED.);
#627=B_SPLINE_CURVE_WITH_KNOTS('',3,(#58075,#58076,#58077,#58078,#58079,
#58080,#58081,#58082,#58083,#58084,#58085,#58086,#58087,#58088,#58089,#58090,
#58091,#58092,#58093,#58094,#58095,#58096,#58097,#58098,#58099,#58100,#58101,
#58102,#58103,#58104,#58105,#58106,#58107,#58108,#58109,#58110,#58111,#58112,
#58113,#58114,#58115,#58116,#58117,#58118,#58119,#58120,#58121,#58122,#58123,
#58124,#58125,#58126,#58127,#58128,#58129,#58130,#58131,#58132,#58133,#58134,
#58135,#58136,#58137,#58138),.UNSPECIFIED.,.F.,.F.,(4,3,3,3,3,3,3,3,3,3,
3,3,3,3,3,3,3,3,3,3,3,4),(0.,0.0209429534522624,0.0766684167144569,0.114857042461602,
0.130015240255125,0.189163540276417,0.2330164052432,0.259452045032286,0.274991797225966,
0.336182683058267,0.364575000143549,0.39776591033518,0.413108590858586,
0.474256684030488,0.514077927074317,0.537085464827502,0.55363870076605,
0.600546717676118,0.627087614796531,0.653616921528325,0.718721003615383,
0.741270768406323),.UNSPECIFIED.);
#628=B_SPLINE_CURVE_WITH_KNOTS('',3,(#58139,#58140,#58141,#58142,#58143,
#58144,#58145,#58146,#58147,#58148,#58149,#58150,#58151,#58152,#58153,#58154),
 .UNSPECIFIED.,.F.,.F.,(4,3,3,3,3,4),(-89.8599198059205,-88.8614762525213,
-87.8630326991222,-86.8645891457231,-85.866145592324,-85.7741580335289),
 .UNSPECIFIED.);
#629=B_SPLINE_CURVE_WITH_KNOTS('',3,(#58316,#58317,#58318,#58319,#58320,
#58321,#58322,#58323,#58324,#58325,#58326,#58327,#58328,#58329,#58330,#58331),
 .UNSPECIFIED.,.F.,.F.,(4,3,3,3,3,4),(-4.09293042013071,-3.97270358331626,
-3.47611563540173,-2.9795276874872,-2.48293973957266,-2.074986472684),
 .UNSPECIFIED.);
#630=B_SPLINE_CURVE_WITH_KNOTS('',3,(#58334,#58335,#58336,#58337,#58338,
#58339,#58340,#58341,#58342,#58343),.UNSPECIFIED.,.F.,.F.,(4,3,3,4),(0.,
0.496587947914526,0.993175895829066,1.12364870614302),.UNSPECIFIED.);
#631=B_SPLINE_CURVE_WITH_KNOTS('',3,(#58348,#58349,#58350,#58351,#58352,
#58353,#58354,#58355,#58356,#58357,#58358,#58359,#58360,#58361,#58362,#58363,
#58364,#58365,#58366,#58367,#58368,#58369,#58370,#58371,#58372,#58373,#58374,
#58375,#58376,#58377,#58378,#58379,#58380,#58381,#58382,#58383,#58384,#58385,
#58386,#58387),.UNSPECIFIED.,.F.,.F.,(4,3,3,3,3,3,3,3,3,3,3,3,3,4),(-10.3761157273103,
-9.93175895829066,-9.43517101037613,-8.93858306246159,-8.44199511454706,
-7.94540716663253,-7.448819218718,-6.95223127080346,-6.45564332288893,-5.95905537497439,
-5.46246742705986,-4.96587947914533,-4.4692915312308,-4.09293042013071),
 .UNSPECIFIED.);
#632=B_SPLINE_CURVE_WITH_KNOTS('',3,(#58388,#58389,#58390,#58391,#58392,
#58393,#58394,#58395,#58396,#58397,#58398,#58399,#58400,#58401,#58402,#58403,
#58404,#58405,#58406,#58407,#58408,#58409,#58410,#58411,#58412,#58413,#58414,
#58415,#58416,#58417,#58418,#58419,#58420,#58421,#58422,#58423,#58424,#58425,
#58426,#58427),.UNSPECIFIED.,.F.,.F.,(4,3,3,3,3,3,3,3,3,3,3,3,3,4),(1.12364870614302,
1.4897638437436,1.98635179165813,2.48293973957267,2.9795276874872,3.47611563540173,
3.97270358331626,4.4692915312308,4.96587947914533,5.46246742705986,5.95905537497439,
6.45564332288893,6.95223127080346,7.40683401332261),.UNSPECIFIED.);
#633=B_SPLINE_CURVE_WITH_KNOTS('',3,(#58432,#58433,#58434,#58435,#58436,
#58437,#58438,#58439,#58440,#58441,#58442,#58443,#58444,#58445,#58446,#58447,
#58448,#58449,#58450,#58451,#58452,#58453,#58454,#58455,#58456,#58457,#58458,
#58459,#58460,#58461,#58462,#58463,#58464,#58465,#58466,#58467,#58468,#58469,
#58470,#58471,#58472,#58473,#58474),.UNSPECIFIED.,.F.,.F.,(4,3,3,3,3,3,
3,3,3,3,3,3,3,3,4),(-16.6593010344899,-16.3874022811796,-15.8908143332651,
-15.3942263853505,-14.897638437436,-14.4010504895215,-13.9044625416069,
-13.4078745936924,-12.9112866457779,-12.4146986978633,-11.9181107499488,
-11.4215228020343,-10.9249348541197,-10.4283469062052,-10.3761157273103),
 .UNSPECIFIED.);
#634=B_SPLINE_CURVE_WITH_KNOTS('',3,(#58475,#58476,#58477,#58478,#58479,
#58480,#58481,#58482,#58483,#58484,#58485,#58486,#58487,#58488,#58489,#58490,
#58491,#58492,#58493,#58494,#58495,#58496,#58497,#58498,#58499,#58500,#58501,
#58502,#58503,#58504,#58505,#58506,#58507,#58508,#58509,#58510,#58511,#58512,
#58513,#58514,#58515,#58516,#58517),.UNSPECIFIED.,.F.,.F.,(4,3,3,3,3,3,
3,3,3,3,3,3,3,3,4),(7.40683401332261,7.44881921871799,7.94540716663252,
8.44199511454706,8.93858306246159,9.43517101037612,9.93175895829065,10.4283469062052,
10.9249348541197,11.4215228020343,11.9181107499488,12.4146986978633,12.9112866457779,
13.4078745936924,13.6900193205022),.UNSPECIFIED.);
#635=B_SPLINE_CURVE_WITH_KNOTS('',3,(#58522,#58523,#58524,#58525,#58526,
#58527,#58528,#58529,#58530,#58531,#58532,#58533,#58534,#58535,#58536,#58537,
#58538,#58539,#58540,#58541,#58542,#58543,#58544,#58545,#58546,#58547,#58548,
#58549,#58550,#58551,#58552,#58553,#58554,#58555,#58556,#58557,#58558,#58559,
#58560,#58561,#58562,#58563,#58564),.UNSPECIFIED.,.F.,.F.,(4,3,3,3,3,3,
3,3,3,3,3,3,3,3,4),(-22.9424863416695,-22.8430456040685,-22.346457656154,
-21.8498697082395,-21.3532817603249,-20.8566938124104,-20.3601058644958,
-19.8635179165813,-19.3669299686668,-18.8703420207523,-18.3737540728377,
-17.8771661249232,-17.3805781770087,-16.8839902290941,-16.6593010344899),
 .UNSPECIFIED.);
#636=B_SPLINE_CURVE_WITH_KNOTS('',3,(#58565,#58566,#58567,#58568,#58569,
#58570,#58571,#58572,#58573,#58574,#58575,#58576,#58577,#58578,#58579,#58580,
#58581,#58582,#58583,#58584,#58585,#58586,#58587,#58588,#58589,#58590,#58591,
#58592,#58593,#58594,#58595,#58596,#58597,#58598,#58599,#58600,#58601,#58602,
#58603,#58604,#58605,#58606,#58607),.UNSPECIFIED.,.F.,.F.,(4,3,3,3,3,3,
3,3,3,3,3,3,3,3,4),(13.6900193205022,13.9044625416069,14.4010504895214,
14.897638437436,15.3942263853505,15.8908143332651,16.3874022811796,16.8839902290941,
17.3805781770086,17.8771661249232,18.3737540728377,18.8703420207522,19.3669299686668,
19.8635179165813,19.9732046276818),.UNSPECIFIED.);
#637=B_SPLINE_CURVE_WITH_KNOTS('',3,(#58612,#58613,#58614,#58615,#58616,
#58617,#58618,#58619,#58620,#58621,#58622,#58623,#58624,#58625,#58626,#58627,
#58628,#58629,#58630,#58631,#58632,#58633,#58634,#58635,#58636,#58637,#58638,
#58639,#58640,#58641,#58642,#58643,#58644,#58645,#58646,#58647,#58648,#58649,
#58650,#58651),.UNSPECIFIED.,.F.,.F.,(4,3,3,3,3,3,3,3,3,3,3,3,3,4),(-29.225671648849,
-28.8021009790429,-28.3055130311284,-27.8089250832139,-27.3123371352993,
-26.8157491873848,-26.3191612394702,-25.8225732915557,-25.3259853436412,
-24.8293973957266,-24.3328094478121,-23.8362214998976,-23.3396335519831,
-22.9424863416695),.UNSPECIFIED.);
#638=B_SPLINE_CURVE_WITH_KNOTS('',3,(#58652,#58653,#58654,#58655,#58656,
#58657,#58658,#58659,#58660,#58661,#58662,#58663,#58664,#58665,#58666,#58667,
#58668,#58669,#58670,#58671,#58672,#58673,#58674,#58675,#58676,#58677,#58678,
#58679,#58680,#58681,#58682,#58683,#58684,#58685,#58686,#58687,#58688,#58689,
#58690,#58691),.UNSPECIFIED.,.F.,.F.,(4,3,3,3,3,3,3,3,3,3,3,3,3,4),(19.9732046276818,
20.3601058644958,20.8566938124104,21.3532817603249,21.8498697082394,22.346457656154,
22.8430456040685,23.339633551983,23.8362214998976,24.3328094478121,24.8293973957266,
25.3259853436412,25.8225732915557,26.2563899348614),.UNSPECIFIED.);
#639=B_SPLINE_CURVE_WITH_KNOTS('',3,(#58696,#58697,#58698,#58699,#58700,
#58701,#58702,#58703,#58704,#58705,#58706,#58707,#58708,#58709,#58710,#58711,
#58712,#58713,#58714,#58715,#58716,#58717,#58718,#58719,#58720,#58721,#58722,
#58723,#58724,#58725,#58726,#58727,#58728,#58729,#58730,#58731,#58732,#58733,
#58734,#58735,#58736,#58737,#58738),.UNSPECIFIED.,.F.,.F.,(4,3,3,3,3,3,
3,3,3,3,3,3,3,3,4),(-35.5088569560286,-35.2577443019318,-34.7611563540173,
-34.2645684061028,-33.7679804581882,-33.2713925102737,-32.7748045623592,
-32.2782166144446,-31.7816286665301,-31.2850407186156,-30.788452770701,
-30.2918648227865,-29.795276874872,-29.2986889269574,-29.225671648849),
 .UNSPECIFIED.);
#640=B_SPLINE_CURVE_WITH_KNOTS('',3,(#58739,#58740,#58741,#58742,#58743,
#58744,#58745,#58746,#58747,#58748,#58749,#58750,#58751,#58752,#58753,#58754,
#58755,#58756,#58757,#58758,#58759,#58760,#58761,#58762,#58763,#58764,#58765,
#58766,#58767,#58768,#58769,#58770,#58771,#58772,#58773,#58774,#58775,#58776,
#58777,#58778,#58779,#58780,#58781),.UNSPECIFIED.,.F.,.F.,(4,3,3,3,3,3,
3,3,3,3,3,3,3,3,4),(26.2563899348614,26.3191612394702,26.8157491873848,
27.3123371352993,27.8089250832138,28.3055130311284,28.8021009790429,29.2986889269574,
29.795276874872,30.2918648227865,30.788452770701,31.2850407186156,31.7816286665301,
32.2782166144446,32.5395752420409),.UNSPECIFIED.);
#641=B_SPLINE_CURVE_WITH_KNOTS('',3,(#58786,#58787,#58788,#58789,#58790,
#58791,#58792,#58793,#58794,#58795,#58796,#58797,#58798,#58799,#58800,#58801,
#58802,#58803,#58804,#58805,#58806,#58807,#58808,#58809,#58810,#58811,#58812,
#58813,#58814,#58815,#58816,#58817,#58818,#58819,#58820,#58821,#58822,#58823,
#58824,#58825,#58826,#58827,#58828),.UNSPECIFIED.,.F.,.F.,(4,3,3,3,3,3,
3,3,3,3,3,3,3,3,4),(-41.7920422632082,-41.7133876248208,-41.2167996769062,
-40.7202117289917,-40.2236237810772,-39.7270358331626,-39.2304478852481,
-38.7338599373336,-38.237271989419,-37.7406840415045,-37.24409609359,-36.7475081456754,
-36.2509201977609,-35.7543322498464,-35.5088569560286),.UNSPECIFIED.);
#642=B_SPLINE_CURVE_WITH_KNOTS('',3,(#58829,#58830,#58831,#58832,#58833,
#58834,#58835,#58836,#58837,#58838,#58839,#58840,#58841,#58842,#58843,#58844,
#58845,#58846,#58847,#58848,#58849,#58850,#58851,#58852,#58853,#58854,#58855,
#58856,#58857,#58858,#58859,#58860,#58861,#58862,#58863,#58864,#58865,#58866,
#58867,#58868,#58869,#58870,#58871),.UNSPECIFIED.,.F.,.F.,(4,3,3,3,3,3,
3,3,3,3,3,3,3,3,4),(32.5395752420409,32.7748045623592,33.2713925102737,
33.7679804581882,34.2645684061028,34.7611563540173,35.2577443019318,35.7543322498464,
36.2509201977609,36.7475081456754,37.24409609359,37.7406840415045,38.237271989419,
38.7338599373336,38.8227605492205),.UNSPECIFIED.);
#643=B_SPLINE_CURVE_WITH_KNOTS('',3,(#58876,#58877,#58878,#58879,#58880,
#58881,#58882,#58883,#58884,#58885,#58886,#58887,#58888,#58889,#58890,#58891,
#58892,#58893,#58894,#58895,#58896,#58897,#58898,#58899,#58900,#58901,#58902,
#58903,#58904,#58905,#58906,#58907,#58908,#58909,#58910,#58911,#58912,#58913,
#58914,#58915),.UNSPECIFIED.,.F.,.F.,(4,3,3,3,3,3,3,3,3,3,3,3,3,4),(-48.0752275703878,
-47.6724429997952,-47.1758550518806,-46.6792671039661,-46.1826791560516,
-45.686091208137,-45.1895032602225,-44.692915312308,-44.1963273643934,-43.6997394164789,
-43.2031514685644,-42.7065635206498,-42.2099755727353,-41.7920422632082),
 .UNSPECIFIED.);
#644=B_SPLINE_CURVE_WITH_KNOTS('',3,(#58916,#58917,#58918,#58919,#58920,
#58921,#58922,#58923,#58924,#58925,#58926,#58927,#58928,#58929,#58930,#58931,
#58932,#58933,#58934,#58935,#58936,#58937,#58938,#58939,#58940,#58941,#58942,
#58943,#58944,#58945,#58946,#58947,#58948,#58949,#58950,#58951,#58952,#58953,
#58954,#58955),.UNSPECIFIED.,.F.,.F.,(4,3,3,3,3,3,3,3,3,3,3,3,3,4),(38.8227605492205,
39.2304478852481,39.7270358331626,40.2236237810772,40.7202117289917,41.2167996769062,
41.7133876248208,42.2099755727353,42.7065635206498,43.2031514685644,43.6997394164789,
44.1963273643934,44.692915312308,45.1059458564001),.UNSPECIFIED.);
#645=B_SPLINE_CURVE_WITH_KNOTS('',3,(#58960,#58961,#58962,#58963,#58964,
#58965,#58966,#58967,#58968,#58969,#58970,#58971,#58972,#58973,#58974,#58975,
#58976,#58977,#58978,#58979,#58980,#58981,#58982,#58983,#58984,#58985,#58986,
#58987,#58988,#58989,#58990,#58991,#58992,#58993,#58994,#58995,#58996,#58997,
#58998,#58999,#59000,#59001,#59002),.UNSPECIFIED.,.F.,.F.,(4,3,3,3,3,3,
3,3,3,3,3,3,3,3,4),(-54.3584128775674,-54.1280863226841,-53.6314983747696,
-53.134910426855,-52.6383224789405,-52.141734531026,-51.6451465831114,-51.1485586351969,
-50.6519706872824,-50.1553827393678,-49.6587947914533,-49.1622068435388,
-48.6656188956242,-48.1690309477097,-48.0752275703878),.UNSPECIFIED.);
#646=B_SPLINE_CURVE_WITH_KNOTS('',3,(#59003,#59004,#59005,#59006,#59007,
#59008,#59009,#59010,#59011,#59012,#59013,#59014,#59015,#59016,#59017,#59018,
#59019,#59020,#59021,#59022,#59023,#59024,#59025,#59026,#59027,#59028,#59029,
#59030,#59031,#59032,#59033,#59034,#59035,#59036,#59037,#59038,#59039,#59040,
#59041,#59042,#59043,#59044,#59045),.UNSPECIFIED.,.F.,.F.,(4,3,3,3,3,3,
3,3,3,3,3,3,3,3,4),(45.1059458564001,45.1895032602225,45.686091208137,46.1826791560515,
46.6792671039661,47.1758550518806,47.6724429997951,48.1690309477097,48.6656188956242,
49.1622068435387,49.6587947914533,50.1553827393678,50.6519706872824,51.1485586351969,
51.3891311635797),.UNSPECIFIED.);
#647=B_SPLINE_CURVE_WITH_KNOTS('',3,(#59050,#59051,#59052,#59053,#59054,
#59055,#59056,#59057,#59058,#59059,#59060,#59061,#59062,#59063,#59064,#59065,
#59066,#59067,#59068,#59069,#59070,#59071,#59072,#59073,#59074,#59075,#59076,
#59077,#59078,#59079,#59080,#59081,#59082,#59083,#59084,#59085,#59086,#59087,
#59088,#59089,#59090,#59091,#59092),.UNSPECIFIED.,.F.,.F.,(4,3,3,3,3,3,
3,3,3,3,3,3,3,3,4),(-60.641598184747,-60.583729645573,-60.0871416976585,
-59.590553749744,-59.0939658018294,-58.5973778539149,-58.1007899060003,
-57.6042019580858,-57.1076140101713,-56.6110260622567,-56.1144381143422,
-55.6178501664277,-55.1212622185132,-54.6246742705986,-54.3584128775674),
 .UNSPECIFIED.);
#648=B_SPLINE_CURVE_WITH_KNOTS('',3,(#59093,#59094,#59095,#59096,#59097,
#59098,#59099,#59100,#59101,#59102,#59103,#59104,#59105,#59106,#59107,#59108,
#59109,#59110,#59111,#59112,#59113,#59114,#59115,#59116,#59117,#59118,#59119,
#59120,#59121,#59122,#59123,#59124,#59125,#59126,#59127,#59128,#59129,#59130,
#59131,#59132,#59133,#59134,#59135),.UNSPECIFIED.,.F.,.F.,(4,3,3,3,3,3,
3,3,3,3,3,3,3,3,4),(51.3891311635797,51.6451465831114,52.1417345310259,
52.6383224789405,53.134910426855,53.6314983747695,54.1280863226841,54.6246742705986,
55.1212622185132,55.6178501664277,56.1144381143422,56.6110260622567,57.1076140101713,
57.6042019580858,57.6723164707593),.UNSPECIFIED.);
#649=B_SPLINE_CURVE_WITH_KNOTS('',3,(#59140,#59141,#59142,#59143,#59144,
#59145,#59146,#59147,#59148,#59149,#59150,#59151,#59152,#59153,#59154,#59155,
#59156,#59157,#59158,#59159,#59160,#59161,#59162,#59163,#59164,#59165,#59166,
#59167,#59168,#59169,#59170,#59171,#59172,#59173,#59174,#59175,#59176,#59177,
#59178,#59179),.UNSPECIFIED.,.F.,.F.,(4,3,3,3,3,3,3,3,3,3,3,3,3,4),(-66.9247834919266,
-66.5427850205474,-66.0461970726329,-65.5496091247183,-65.0530211768038,
-64.5564332288893,-64.0598452809748,-63.5632573330602,-63.0666693851457,
-62.5700814372311,-62.0734934893166,-61.5769055414021,-61.0803175934875,
-60.641598184747),.UNSPECIFIED.);
#650=B_SPLINE_CURVE_WITH_KNOTS('',3,(#59180,#59181,#59182,#59183,#59184,
#59185,#59186,#59187,#59188,#59189,#59190,#59191,#59192,#59193,#59194,#59195,
#59196,#59197,#59198,#59199,#59200,#59201,#59202,#59203,#59204,#59205,#59206,
#59207,#59208,#59209,#59210,#59211,#59212,#59213,#59214,#59215,#59216,#59217,
#59218,#59219),.UNSPECIFIED.,.F.,.F.,(4,3,3,3,3,3,3,3,3,3,3,3,3,4),(57.6723164707593,
58.1007899060003,58.5973778539149,59.0939658018294,59.5905537497439,60.0871416976585,
60.583729645573,61.0803175934875,61.5769055414021,62.0734934893166,62.5700814372311,
63.0666693851457,63.5632573330602,63.9555017779389),.UNSPECIFIED.);
#651=B_SPLINE_CURVE_WITH_KNOTS('',3,(#59224,#59225,#59226,#59227,#59228,
#59229,#59230,#59231,#59232,#59233,#59234,#59235,#59236,#59237,#59238,#59239,
#59240,#59241,#59242,#59243,#59244,#59245,#59246,#59247,#59248,#59249,#59250,
#59251,#59252,#59253,#59254,#59255,#59256,#59257,#59258,#59259,#59260,#59261,
#59262,#59263,#59264,#59265,#59266),.UNSPECIFIED.,.F.,.F.,(4,3,3,3,3,3,
3,3,3,3,3,3,3,3,4),(-73.2079687991062,-72.9984283434363,-72.5018403955218,
-72.0052524476073,-71.5086644996927,-71.0120765517782,-70.5154886038637,
-70.0189006559491,-69.5223127080346,-69.0257247601201,-68.5291368122056,
-68.032548864291,-67.5359609163765,-67.0393729684619,-66.9247834919266),
 .UNSPECIFIED.);
#652=B_SPLINE_CURVE_WITH_KNOTS('',3,(#59267,#59268,#59269,#59270,#59271,
#59272,#59273,#59274,#59275,#59276,#59277,#59278,#59279,#59280,#59281,#59282,
#59283,#59284,#59285,#59286,#59287,#59288,#59289,#59290,#59291,#59292,#59293,
#59294,#59295,#59296,#59297,#59298,#59299,#59300,#59301,#59302,#59303,#59304,
#59305,#59306,#59307,#59308,#59309),.UNSPECIFIED.,.F.,.F.,(4,3,3,3,3,3,
3,3,3,3,3,3,3,3,4),(63.9555017779389,64.0598452809747,64.5564332288893,
65.0530211768038,65.5496091247183,66.0461970726329,66.5427850205474,67.0393729684619,
67.5359609163765,68.032548864291,68.5291368122055,69.0257247601201,69.5223127080346,
70.0189006559491,70.2386870851185),.UNSPECIFIED.);
#653=B_SPLINE_CURVE_WITH_KNOTS('',3,(#59314,#59315,#59316,#59317,#59318,
#59319,#59320,#59321,#59322,#59323,#59324,#59325,#59326,#59327,#59328,#59329,
#59330,#59331,#59332,#59333,#59334,#59335,#59336,#59337,#59338,#59339,#59340,
#59341,#59342,#59343,#59344,#59345,#59346,#59347,#59348,#59349,#59350,#59351,
#59352,#59353,#59354,#59355,#59356),.UNSPECIFIED.,.F.,.F.,(4,3,3,3,3,3,
3,3,3,3,3,3,3,3,4),(-79.4911541062858,-79.4540716663253,-78.9574837184107,
-78.4608957704962,-77.9643078225817,-77.4677198746671,-76.9711319267526,
-76.4745439788381,-75.9779560309235,-75.481368083009,-74.9847801350945,
-74.4881921871799,-73.9916042392654,-73.4950162913509,-73.2079687991062),
 .UNSPECIFIED.);
#654=B_SPLINE_CURVE_WITH_KNOTS('',3,(#59357,#59358,#59359,#59360,#59361,
#59362,#59363,#59364,#59365,#59366,#59367,#59368,#59369,#59370,#59371,#59372,
#59373,#59374,#59375,#59376,#59377,#59378,#59379,#59380,#59381,#59382,#59383,
#59384,#59385,#59386,#59387,#59388,#59389,#59390,#59391,#59392,#59393,#59394,
#59395,#59396,#59397,#59398,#59399),.UNSPECIFIED.,.F.,.F.,(4,3,3,3,3,3,
3,3,3,3,3,3,3,3,4),(70.2386870851185,70.5154886038637,71.0120765517782,
71.5086644996927,72.0052524476073,72.5018403955218,72.9984283434363,73.4950162913509,
73.9916042392654,74.4881921871799,74.9847801350944,75.481368083009,75.9779560309235,
76.474543978838,76.5218723922981),.UNSPECIFIED.);
#655=B_SPLINE_CURVE_WITH_KNOTS('',3,(#59404,#59405,#59406,#59407,#59408,
#59409,#59410,#59411,#59412,#59413,#59414,#59415,#59416,#59417,#59418,#59419,
#59420,#59421,#59422,#59423,#59424,#59425,#59426,#59427,#59428,#59429,#59430,
#59431,#59432,#59433,#59434,#59435,#59436,#59437,#59438,#59439,#59440,#59441,
#59442,#59443),.UNSPECIFIED.,.F.,.F.,(4,3,3,3,3,3,3,3,3,3,3,3,3,4),(-85.7743394134654,
-85.4131270412997,-84.9165390933851,-84.4199511454706,-83.9233631975561,
-83.4267752496415,-82.930187301727,-82.4335993538125,-81.9370114058979,
-81.4404234579834,-80.9438355100689,-80.4472475621543,-79.9506596142398,
-79.4911541062858),.UNSPECIFIED.);
#656=B_SPLINE_CURVE_WITH_KNOTS('',3,(#59444,#59445,#59446,#59447,#59448,
#59449,#59450,#59451,#59452,#59453,#59454,#59455,#59456,#59457,#59458,#59459,
#59460,#59461,#59462,#59463,#59464,#59465,#59466,#59467,#59468,#59469,#59470,
#59471,#59472,#59473,#59474,#59475,#59476,#59477,#59478,#59479,#59480,#59481,
#59482,#59483),.UNSPECIFIED.,.F.,.F.,(4,3,3,3,3,3,3,3,3,3,3,3,3,4),(76.5218723922981,
76.9711319267526,77.4677198746671,77.9643078225816,78.4608957704962,78.9574837184107,
79.4540716663252,79.9506596142398,80.4472475621543,80.9438355100688,81.4404234579834,
81.9370114058979,82.4335993538124,82.8050576994777),.UNSPECIFIED.);
#657=B_SPLINE_CURVE_WITH_KNOTS('',3,(#59488,#59489,#59490,#59491,#59492,
#59493,#59494,#59495,#59496,#59497,#59498,#59499,#59500,#59501,#59502,#59503,
#59504,#59505,#59506,#59507,#59508,#59509,#59510,#59511,#59512,#59513,#59514,
#59515,#59516,#59517,#59518,#59519,#59520,#59521,#59522,#59523,#59524,#59525,
#59526,#59527,#59528,#59529,#59530),.UNSPECIFIED.,.F.,.F.,(4,3,3,3,3,3,
3,3,3,3,3,3,3,3,4),(-92.057524720645,-91.8687703641886,-91.3721824162741,
-90.8755944683595,-90.379006520445,-89.8824185725305,-89.3858306246159,
-88.8892426767014,-88.3926547287869,-87.8960667808723,-87.3994788329578,
-86.9028908850433,-86.4063029371287,-85.9097149892142,-85.7743394134654),
 .UNSPECIFIED.);
#658=B_SPLINE_CURVE_WITH_KNOTS('',3,(#59531,#59532,#59533,#59534,#59535,
#59536,#59537,#59538,#59539,#59540,#59541,#59542,#59543,#59544,#59545,#59546,
#59547,#59548,#59549,#59550,#59551,#59552,#59553,#59554,#59555,#59556,#59557,
#59558,#59559,#59560,#59561,#59562,#59563,#59564,#59565,#59566,#59567,#59568,
#59569,#59570,#59571,#59572,#59573),.UNSPECIFIED.,.F.,.F.,(4,3,3,3,3,3,
3,3,3,3,3,3,3,3,4),(82.8050576994777,82.930187301727,83.4267752496415,83.923363197556,
84.4199511454706,84.9165390933851,85.4131270412996,85.9097149892142,86.4063029371287,
86.9028908850432,87.3994788329578,87.8960667808723,88.3926547287869,88.8892426767014,
89.0882430066573),.UNSPECIFIED.);
#659=B_SPLINE_CURVE_WITH_KNOTS('',3,(#59578,#59579,#59580,#59581,#59582,
#59583,#59584,#59585,#59586,#59587,#59588,#59589,#59590,#59591,#59592,#59593,
#59594,#59595,#59596,#59597,#59598,#59599,#59600,#59601,#59602,#59603,#59604,
#59605,#59606,#59607,#59608,#59609,#59610,#59611,#59612,#59613,#59614,#59615,
#59616,#59617,#59618,#59619,#59620),.UNSPECIFIED.,.F.,.F.,(4,3,3,3,3,3,
3,3,3,3,3,3,3,3,4),(-98.3407100278246,-98.3244136870775,-97.827825739163,
-97.3312377912485,-96.8346498433339,-96.3380618954194,-95.8414739475049,
-95.3448859995903,-94.8482980516758,-94.3517101037612,-93.8551221558467,
-93.3585342079322,-92.8619462600177,-92.3653583121031,-92.057524720645),
 .UNSPECIFIED.);
#660=B_SPLINE_CURVE_WITH_KNOTS('',3,(#59621,#59622,#59623,#59624,#59625,
#59626,#59627,#59628,#59629,#59630,#59631,#59632,#59633,#59634,#59635,#59636,
#59637,#59638,#59639,#59640,#59641,#59642,#59643,#59644,#59645,#59646,#59647,
#59648,#59649,#59650,#59651,#59652,#59653,#59654,#59655,#59656,#59657,#59658,
#59659,#59660,#59661,#59662,#59663),.UNSPECIFIED.,.F.,.F.,(4,3,3,3,3,3,
3,3,3,3,3,3,3,3,4),(89.0882430066573,89.3858306246159,89.8824185725304,
90.379006520445,90.8755944683595,91.372182416274,91.8687703641886,92.3653583121031,
92.8619462600176,93.3585342079322,93.8551221558467,94.3517101037612,94.8482980516758,
95.3448859995903,95.3714283138369),.UNSPECIFIED.);
#661=B_SPLINE_CURVE_WITH_KNOTS('',3,(#59668,#59669,#59670,#59671,#59672,
#59673,#59674,#59675,#59676,#59677,#59678,#59679,#59680,#59681,#59682,#59683,
#59684,#59685,#59686,#59687,#59688,#59689,#59690,#59691,#59692,#59693,#59694,
#59695,#59696,#59697,#59698,#59699,#59700,#59701,#59702,#59703,#59704,#59705,
#59706,#59707),.UNSPECIFIED.,.F.,.F.,(4,3,3,3,3,3,3,3,3,3,3,3,3,4),(-104.623895335004,
-104.283469062052,-103.786881114137,-103.290293166223,-102.793705218308,
-102.297117270394,-101.800529322479,-101.303941374565,-100.80735342665,
-100.310765478736,-99.8141775308211,-99.3175895829066,-98.821001634992,
-98.3407100278246),.UNSPECIFIED.);
#662=B_SPLINE_CURVE_WITH_KNOTS('',3,(#59708,#59709,#59710,#59711,#59712,
#59713,#59714,#59715,#59716,#59717,#59718,#59719,#59720,#59721,#59722,#59723,
#59724,#59725,#59726,#59727,#59728,#59729,#59730,#59731,#59732,#59733,#59734,
#59735,#59736,#59737,#59738,#59739,#59740,#59741,#59742,#59743,#59744,#59745,
#59746,#59747),.UNSPECIFIED.,.F.,.F.,(4,3,3,3,3,3,3,3,3,3,3,3,3,4),(95.3714283138369,
95.8414739475048,96.3380618954194,96.8346498433339,97.3312377912484,97.827825739163,
98.3244136870775,98.821001634992,99.3175895829065,99.8141775308211,100.310765478736,
100.80735342665,101.303941374565,101.654613621016),.UNSPECIFIED.);
#663=B_SPLINE_CURVE_WITH_KNOTS('',3,(#59752,#59753,#59754,#59755,#59756,
#59757,#59758,#59759,#59760,#59761,#59762,#59763,#59764,#59765,#59766,#59767,
#59768,#59769,#59770,#59771,#59772,#59773,#59774,#59775,#59776,#59777,#59778,
#59779,#59780,#59781,#59782,#59783,#59784,#59785,#59786,#59787,#59788,#59789,
#59790,#59791,#59792,#59793,#59794),.UNSPECIFIED.,.F.,.F.,(4,3,3,3,3,3,
3,3,3,3,3,3,3,3,4),(-110.907080642184,-110.739112384941,-110.242524437026,
-109.745936489112,-109.249348541197,-108.752760593283,-108.256172645368,
-107.759584697454,-107.262996749539,-106.766408801625,-106.26982085371,
-105.773232905796,-105.276644957881,-104.780057009966,-104.623895335004),
 .UNSPECIFIED.);
#664=B_SPLINE_CURVE_WITH_KNOTS('',3,(#59795,#59796,#59797,#59798,#59799,
#59800,#59801,#59802,#59803,#59804,#59805,#59806,#59807,#59808,#59809,#59810,
#59811,#59812,#59813,#59814,#59815,#59816,#59817,#59818,#59819,#59820,#59821,
#59822,#59823,#59824,#59825,#59826,#59827,#59828,#59829,#59830,#59831,#59832,
#59833,#59834,#59835,#59836,#59837),.UNSPECIFIED.,.F.,.F.,(4,3,3,3,3,3,
3,3,3,3,3,3,3,3,4),(101.654613621016,101.800529322479,102.297117270394,
102.793705218308,103.290293166223,103.786881114137,104.283469062052,104.780057009966,
105.276644957881,105.773232905795,106.26982085371,106.766408801625,107.262996749539,
107.759584697454,107.937798928196),.UNSPECIFIED.);
#665=B_SPLINE_CURVE_WITH_KNOTS('',3,(#59842,#59843,#59844,#59845,#59846,
#59847,#59848,#59849,#59850,#59851,#59852,#59853,#59854,#59855,#59856,#59857,
#59858,#59859,#59860,#59861,#59862,#59863,#59864,#59865,#59866,#59867,#59868,
#59869,#59870,#59871,#59872,#59873,#59874,#59875,#59876,#59877,#59878,#59879,
#59880,#59881),.UNSPECIFIED.,.F.,.F.,(4,3,3,3,3,3,3,3,3,3,3,3,3,4),(-117.190265949363,
-116.698167759915,-116.201579812001,-115.704991864086,-115.208403916172,
-114.711815968257,-114.215228020343,-113.718640072428,-113.222052124514,
-112.725464176599,-112.228876228684,-111.73228828077,-111.235700332855,
-110.907080642184),.UNSPECIFIED.);
#666=B_SPLINE_CURVE_WITH_KNOTS('',3,(#59882,#59883,#59884,#59885,#59886,
#59887,#59888,#59889,#59890,#59891,#59892,#59893,#59894,#59895,#59896,#59897,
#59898,#59899,#59900,#59901,#59902,#59903,#59904,#59905,#59906,#59907,#59908,
#59909,#59910,#59911,#59912,#59913,#59914,#59915,#59916,#59917,#59918,#59919,
#59920,#59921,#59922,#59923,#59924),.UNSPECIFIED.,.F.,.F.,(4,3,3,3,3,3,
3,3,3,3,3,3,3,3,4),(107.937798928196,108.256172645368,108.752760593283,
109.249348541197,109.745936489112,110.242524437026,110.739112384941,111.235700332855,
111.73228828077,112.228876228684,112.725464176599,113.222052124513,113.718640072428,
114.215228020343,114.220984235376),.UNSPECIFIED.);
#667=B_SPLINE_CURVE_WITH_KNOTS('',3,(#59929,#59930,#59931,#59932,#59933,
#59934,#59935,#59936,#59937,#59938,#59939,#59940,#59941,#59942,#59943,#59944,
#59945,#59946,#59947,#59948,#59949,#59950,#59951,#59952,#59953,#59954,#59955,
#59956,#59957,#59958,#59959,#59960,#59961,#59962,#59963,#59964,#59965,#59966,
#59967,#59968,#59969,#59970,#59971),.UNSPECIFIED.,.F.,.F.,(4,3,3,3,3,3,
3,3,3,3,3,3,3,3,4),(-123.473451256543,-123.153811082804,-122.65722313489,
-122.160635186975,-121.664047239061,-121.167459291146,-120.670871343231,
-120.174283395317,-119.677695447402,-119.181107499488,-118.684519551573,
-118.187931603659,-117.691343655744,-117.19475570783,-117.190265949363),
 .UNSPECIFIED.);
#668=B_SPLINE_CURVE_WITH_KNOTS('',3,(#59972,#59973,#59974,#59975,#59976,
#59977,#59978,#59979,#59980,#59981,#59982,#59983,#59984,#59985,#59986,#59987,
#59988,#59989,#59990,#59991,#59992,#59993,#59994,#59995,#59996,#59997,#59998,
#59999,#60000,#60001,#60002,#60003,#60004,#60005,#60006,#60007,#60008,#60009,
#60010,#60011),.UNSPECIFIED.,.F.,.F.,(4,3,3,3,3,3,3,3,3,3,3,3,3,4),(114.220984235376,
114.711815968257,115.208403916172,115.704991864086,116.201579812001,116.698167759915,
117.19475570783,117.691343655744,118.187931603659,118.684519551573,119.181107499488,
119.677695447402,120.174283395317,120.504169542555),.UNSPECIFIED.);
#669=B_SPLINE_CURVE_WITH_KNOTS('',3,(#60017,#60018,#60019,#60020,#60021),
 .UNSPECIFIED.,.F.,.F.,(4,1,4),(135.088484104361,135.265431878537,135.673385145426),
 .UNSPECIFIED.);
#670=B_SPLINE_CURVE_WITH_KNOTS('',3,(#60027,#60028,#60029,#60030,#60031,
#60032,#60033,#60034,#60035,#60036,#60037,#60038,#60039,#60040,#60041,#60042,
#60043),.UNSPECIFIED.,.F.,.F.,(4,1,1,1,1,1,1,1,1,1,1,1,1,1,4),(128.805298797182,
128.809788555648,129.306376503562,129.802964451477,130.299552399392,130.796140347306,
131.292728295221,131.789316243135,132.28590419105,132.782492138964,133.279080086879,
133.775668034793,134.272255982708,134.768843930622,135.088484104361),
 .UNSPECIFIED.);
#671=B_SPLINE_CURVE_WITH_KNOTS('',3,(#60046,#60047,#60048,#60049,#60050,
#60051,#60052,#60053,#60054,#60055,#60056,#60057,#60058,#60059,#60060),
 .UNSPECIFIED.,.F.,.F.,(4,1,1,1,1,1,1,1,1,1,1,1,4),(128.805298797182,128.972000597858,
129.468588545772,129.965176493687,130.461764441601,130.958352389516,131.45494033743,
131.951528285345,132.448116233259,132.944704181174,133.441292129088,133.937880077003,
134.434468024917),.UNSPECIFIED.);
#672=B_SPLINE_CURVE_WITH_KNOTS('',3,(#60065,#60066,#60067,#60068,#60069,
#60070,#60071,#60072,#60073,#60074,#60075,#60076,#60077,#60078,#60079,#60080),
 .UNSPECIFIED.,.F.,.F.,(4,1,1,1,1,1,1,1,1,1,1,1,1,4),(122.522113490002,
122.850733180674,123.347321128588,123.843909076503,124.340497024417,124.837084972332,
125.333672920246,125.830260868161,126.326848816075,126.82343676399,127.320024711904,
127.816612659819,128.313200607733,128.805298797182),.UNSPECIFIED.);
#673=B_SPLINE_CURVE_WITH_KNOTS('',3,(#60081,#60082,#60083,#60084,#60085,
#60086,#60087,#60088,#60089,#60090,#60091,#60092,#60093,#60094,#60095,#60096),
 .UNSPECIFIED.,.F.,.F.,(4,1,1,1,1,1,1,1,1,1,1,1,1,4),(122.522113490002,
123.012945222883,123.509533170798,124.006121118712,124.502709066627,124.999297014541,
125.495884962456,125.99247291037,126.489060858285,126.985648806199,127.482236754114,
127.978824702029,128.475412649943,128.805298797182),.UNSPECIFIED.);
#674=B_SPLINE_CURVE_WITH_KNOTS('',3,(#60101,#60102,#60103,#60104,#60105,
#60106,#60107,#60108,#60109,#60110,#60111,#60112,#60113,#60114,#60115,#60116,
#60117),.UNSPECIFIED.,.F.,.F.,(4,1,1,1,1,1,1,1,1,1,1,1,1,1,4),(116.238928182822,
116.395089857785,116.891677805699,117.388265753614,117.884853701528,118.381441649443,
118.878029597357,119.374617545272,119.871205493186,120.367793441101,120.864381389015,
121.36096933693,121.857557284844,122.354145232759,122.522113490002),
 .UNSPECIFIED.);
#675=B_SPLINE_CURVE_WITH_KNOTS('',3,(#60118,#60119,#60120,#60121,#60122,
#60123,#60124,#60125,#60126,#60127,#60128,#60129,#60130,#60131,#60132,#60133,
#60134),.UNSPECIFIED.,.F.,.F.,(4,1,1,1,1,1,1,1,1,1,1,1,1,1,4),(116.238928182822,
116.557301899994,117.053889847909,117.550477795823,118.047065743738,118.543653691652,
119.040241639567,119.536829587481,120.033417535396,120.530005483311,121.026593431225,
121.52318137914,122.019769327054,122.516357274969,122.522113490002),
 .UNSPECIFIED.);
#676=B_SPLINE_CURVE_WITH_KNOTS('',3,(#60139,#60140,#60141,#60142,#60143,
#60144,#60145,#60146,#60147,#60148,#60149,#60150,#60151,#60152,#60153,#60154),
 .UNSPECIFIED.,.F.,.F.,(4,1,1,1,1,1,1,1,1,1,1,1,1,4),(109.955742875643,
110.43603448281,110.932622430725,111.429210378639,111.925798326554,112.422386274468,
112.918974222383,113.415562170297,113.912150118212,114.408738066126,114.905326014041,
115.401913961956,115.89850190987,116.238928182822),.UNSPECIFIED.);
#677=B_SPLINE_CURVE_WITH_KNOTS('',3,(#60155,#60156,#60157,#60158,#60159,
#60160,#60161,#60162,#60163,#60164,#60165,#60166,#60167,#60168,#60169,#60170,
#60171),.UNSPECIFIED.,.F.,.F.,(4,1,1,1,1,1,1,1,1,1,1,1,1,1,4),(109.955742875643,
110.101658577105,110.59824652502,111.094834472934,111.591422420849,112.088010368763,
112.584598316678,113.081186264593,113.577774212507,114.074362160422,114.570950108336,
115.067538056251,115.564126004165,116.06071395208,116.238928182822),
 .UNSPECIFIED.);
#678=B_SPLINE_CURVE_WITH_KNOTS('',3,(#60176,#60177,#60178,#60179,#60180,
#60181,#60182,#60183,#60184,#60185,#60186,#60187,#60188,#60189,#60190,#60191,
#60192),.UNSPECIFIED.,.F.,.F.,(4,1,1,1,1,1,1,1,1,1,1,1,1,1,4),(103.672557568463,
103.980391159921,104.476979107836,104.97356705575,105.470155003665,105.966742951579,
106.463330899494,106.959918847408,107.456506795323,107.953094743238,108.449682691152,
108.946270639067,109.442858586981,109.939446534896,109.955742875643),
 .UNSPECIFIED.);
#679=B_SPLINE_CURVE_WITH_KNOTS('',3,(#60193,#60194,#60195,#60196,#60197,
#60198,#60199,#60200,#60201,#60202,#60203,#60204,#60205,#60206,#60207,#60208),
 .UNSPECIFIED.,.F.,.F.,(4,1,1,1,1,1,1,1,1,1,1,1,1,4),(103.672557568463,
104.142603202131,104.639191150046,105.13577909796,105.632367045875,106.128954993789,
106.625542941704,107.122130889618,107.618718837533,108.115306785447,108.611894733362,
109.108482681276,109.605070629191,109.955742875643),.UNSPECIFIED.);
#680=B_SPLINE_CURVE_WITH_KNOTS('',3,(#60213,#60214,#60215,#60216,#60217,
#60218,#60219,#60220,#60221,#60222,#60223,#60224,#60225,#60226,#60227,#60228,
#60229),.UNSPECIFIED.,.F.,.F.,(4,1,1,1,1,1,1,1,1,1,1,1,1,1,4),(97.3893722612836,
97.5247478370324,98.0213357849469,98.5179237328614,99.014511680776,99.5110996286905,
100.007687576605,100.50427552452,101.000863472434,101.497451420349,101.994039368263,
102.490627316178,102.987215264092,103.483803212007,103.672557568463),
 .UNSPECIFIED.);
#681=B_SPLINE_CURVE_WITH_KNOTS('',3,(#60230,#60231,#60232,#60233,#60234,
#60235,#60236,#60237,#60238,#60239,#60240,#60241,#60242,#60243,#60244,#60245,
#60246),.UNSPECIFIED.,.F.,.F.,(4,1,1,1,1,1,1,1,1,1,1,1,1,1,4),(97.3893722612835,
97.686959879242,98.1835478271566,98.6801357750711,99.1767237229856,99.6733116709002,
100.169899618815,100.666487566729,101.163075514644,101.659663462558,102.156251410473,
102.652839358387,103.149427306302,103.646015254216,103.672557568463),
 .UNSPECIFIED.);
#682=B_SPLINE_CURVE_WITH_KNOTS('',3,(#60251,#60252,#60253,#60254,#60255,
#60256,#60257,#60258,#60259,#60260,#60261,#60262,#60263,#60264,#60265,#60266),
 .UNSPECIFIED.,.F.,.F.,(4,1,1,1,1,1,1,1,1,1,1,1,1,4),(91.106186954104,91.565692462058,
92.0622804099725,92.558868357887,93.0554563058016,93.5520442537161,94.0486322016306,
94.5452201495452,95.0418080974597,95.5383960453742,96.0349839932888,96.5315719412033,
97.0281598891178,97.3893722612836),.UNSPECIFIED.);
#683=B_SPLINE_CURVE_WITH_KNOTS('',3,(#60267,#60268,#60269,#60270,#60271,
#60272,#60273,#60274,#60275,#60276,#60277,#60278,#60279,#60280,#60281,#60282,
#60283),.UNSPECIFIED.,.F.,.F.,(4,1,1,1,1,1,1,1,1,1,1,1,1,1,4),(91.106186954104,
91.2313165563531,91.7279045042677,92.2244924521822,92.7210804000967,93.2176683480112,
93.7142562959258,94.2108442438403,94.7074321917548,95.2040201396694,95.7006080875839,
96.1971960354985,96.693783983413,97.1903719313275,97.3893722612835),
 .UNSPECIFIED.);
#684=B_SPLINE_CURVE_WITH_KNOTS('',3,(#60288,#60289,#60290,#60291,#60292,
#60293,#60294,#60295,#60296,#60297,#60298,#60299,#60300,#60301,#60302,#60303,
#60304),.UNSPECIFIED.,.F.,.F.,(4,1,1,1,1,1,1,1,1,1,1,1,1,1,4),(84.8230016469244,
85.110049139169,85.6066370870836,86.1032250349981,86.5998129829126,87.0964009308272,
87.5929888787417,88.0895768266562,88.5861647745708,89.0827527224853,89.5793406703998,
90.0759286183144,90.5725165662289,91.0691045141434,91.106186954104),
 .UNSPECIFIED.);
#685=B_SPLINE_CURVE_WITH_KNOTS('',3,(#60305,#60306,#60307,#60308,#60309,
#60310,#60311,#60312,#60313,#60314,#60315,#60316,#60317,#60318,#60319,#60320),
 .UNSPECIFIED.,.F.,.F.,(4,1,1,1,1,1,1,1,1,1,1,1,1,4),(84.8230016469244,
85.2722611813787,85.7688491292933,86.2654370772078,86.7620250251223,87.2586129730369,
87.7552009209514,88.2517888688659,88.7483768167804,89.244964764695,89.7415527126095,
90.2381406605241,90.7347286084386,91.106186954104),.UNSPECIFIED.);
#686=B_SPLINE_CURVE_WITH_KNOTS('',3,(#60325,#60326,#60327,#60328,#60329,
#60330,#60331,#60332,#60333,#60334,#60335,#60336,#60337,#60338,#60339,#60340,
#60341),.UNSPECIFIED.,.F.,.F.,(4,1,1,1,1,1,1,1,1,1,1,1,1,1,4),(78.5398163397448,
78.6544058162801,79.1509937641947,79.6475817121092,80.1441696600237,80.6407576079382,
81.1373455558528,81.6339335037673,82.1305214516818,82.6271093995964,83.1236973475109,
83.6202852954254,84.11687324334,84.6134611912545,84.8230016469244),
 .UNSPECIFIED.);
#687=B_SPLINE_CURVE_WITH_KNOTS('',3,(#60342,#60343,#60344,#60345,#60346,
#60347,#60348,#60349,#60350,#60351,#60352,#60353,#60354,#60355,#60356,#60357,
#60358),.UNSPECIFIED.,.F.,.F.,(4,1,1,1,1,1,1,1,1,1,1,1,1,1,4),(78.5398163397448,
78.8166178584898,79.3132058064043,79.8097937543189,80.3063817022334,80.8029696501479,
81.2995575980625,81.796145545977,82.2927334938915,82.7893214418061,83.2859093897206,
83.7824973376351,84.2790852855497,84.7756732334642,84.8230016469244),
 .UNSPECIFIED.);
#688=B_SPLINE_CURVE_WITH_KNOTS('',3,(#60363,#60364,#60365,#60366,#60367,
#60368,#60369,#60370,#60371,#60372,#60373,#60374,#60375,#60376,#60377,#60378),
 .UNSPECIFIED.,.F.,.F.,(4,1,1,1,1,1,1,1,1,1,1,1,1,4),(72.2566310325652,
72.6953504413057,73.1919383892203,73.6885263371348,74.1851142850493,74.6817022329639,
75.1782901808784,75.6748781287929,76.1714660767074,76.668054024622,77.1646419725365,
77.661229920451,78.1578178683656,78.5398163397448),.UNSPECIFIED.);
#689=B_SPLINE_CURVE_WITH_KNOTS('',3,(#60379,#60380,#60381,#60382,#60383,
#60384,#60385,#60386,#60387,#60388,#60389,#60390,#60391,#60392,#60393,#60394,
#60395),.UNSPECIFIED.,.F.,.F.,(4,1,1,1,1,1,1,1,1,1,1,1,1,1,4),(72.2566310325652,
72.3609745356009,72.8575624835154,73.3541504314299,73.8507383793445,74.347326327259,
74.8439142751735,75.3405022230881,75.8370901710026,76.3336781189171,76.8302660668317,
77.3268540147462,77.8234419626607,78.3200299105753,78.5398163397448),
 .UNSPECIFIED.);
#690=B_SPLINE_CURVE_WITH_KNOTS('',3,(#60400,#60401,#60402,#60403,#60404,
#60405,#60406,#60407,#60408,#60409,#60410,#60411,#60412,#60413,#60414,#60415,
#60416),.UNSPECIFIED.,.F.,.F.,(4,1,1,1,1,1,1,1,1,1,1,1,1,1,4),(65.9734457253856,
66.2397071184168,66.7362950663313,67.2328830142459,67.7294709621604,68.2260589100749,
68.7226468579895,69.219234805904,69.7158227538185,70.2124107017331,70.7089986496476,
71.2055865975621,71.7021745454767,72.1987624933912,72.2566310325652),
 .UNSPECIFIED.);
#691=B_SPLINE_CURVE_WITH_KNOTS('',3,(#60417,#60418,#60419,#60420,#60421,
#60422,#60423,#60424,#60425,#60426,#60427,#60428,#60429,#60430,#60431,#60432),
 .UNSPECIFIED.,.F.,.F.,(4,1,1,1,1,1,1,1,1,1,1,1,1,4),(65.9734457253856,
66.4019191606265,66.898507108541,67.3950950564555,67.8916830043701,68.3882709522846,
68.8848589001991,69.3814468481137,69.8780347960282,70.3746227439427,70.8712106918573,
71.3677986397718,71.8643865876863,72.2566310325652),.UNSPECIFIED.);
#692=B_SPLINE_CURVE_WITH_KNOTS('',3,(#60437,#60438,#60439,#60440,#60441,
#60442,#60443,#60444,#60445,#60446,#60447,#60448,#60449,#60450,#60451,#60452,
#60453),.UNSPECIFIED.,.F.,.F.,(4,1,1,1,1,1,1,1,1,1,1,1,1,1,4),(59.690260418206,
59.7840637955279,60.2806517434424,60.7772396913569,61.2738276392715,61.770415587186,
62.2670035351005,62.7635914830151,63.2601794309296,63.7567673788441,64.2533553267587,
64.7499432746732,65.2465312225877,65.7431191705023,65.9734457253856),
 .UNSPECIFIED.);
#693=B_SPLINE_CURVE_WITH_KNOTS('',3,(#60454,#60455,#60456,#60457,#60458,
#60459,#60460,#60461,#60462,#60463,#60464,#60465,#60466,#60467,#60468,#60469,
#60470),.UNSPECIFIED.,.F.,.F.,(4,1,1,1,1,1,1,1,1,1,1,1,1,1,4),(59.690260418206,
59.9462758377375,60.4428637856521,60.9394517335666,61.4360396814811,61.9326276293957,
62.4292155773102,62.9258035252248,63.4223914731393,63.9189794210538,64.4155673689683,
64.9121553168829,65.4087432647974,65.9053312127119,65.9734457253856),
 .UNSPECIFIED.);
#694=B_SPLINE_CURVE_WITH_KNOTS('',3,(#60475,#60476,#60477,#60478,#60479,
#60480,#60481,#60482,#60483,#60484,#60485,#60486,#60487,#60488,#60489,#60490),
 .UNSPECIFIED.,.F.,.F.,(4,1,1,1,1,1,1,1,1,1,1,1,1,4),(53.4070751110264,
53.8250084205535,54.321596368468,54.8181843163825,55.3147722642971,55.8113602122116,
56.3079481601261,56.8045361080407,57.3011240559552,57.7977120038697,58.2942999517843,
58.7908878996988,59.2874758476133,59.690260418206),.UNSPECIFIED.);
#695=B_SPLINE_CURVE_WITH_KNOTS('',3,(#60491,#60492,#60493,#60494,#60495,
#60496,#60497,#60498,#60499,#60500,#60501,#60502,#60503,#60504,#60505,#60506,
#60507),.UNSPECIFIED.,.F.,.F.,(4,1,1,1,1,1,1,1,1,1,1,1,1,1,4),(53.4070751110264,
53.4906325148486,53.9872204627632,54.4838084106777,54.9803963585922,55.4769843065068,
55.9735722544213,56.4701602023358,56.9667481502504,57.4633360981649,57.9599240460794,
58.456511993994,58.9530999419085,59.449687889823,59.690260418206),
 .UNSPECIFIED.);
#696=B_SPLINE_CURVE_WITH_KNOTS('',3,(#60512,#60513,#60514,#60515,#60516,
#60517,#60518,#60519,#60520,#60521,#60522,#60523,#60524,#60525,#60526,#60527,
#60528),.UNSPECIFIED.,.F.,.F.,(4,1,1,1,1,1,1,1,1,1,1,1,1,1,4),(47.1238898038468,
47.3693650976645,47.8659530455791,48.3625409934936,48.8591289414081,49.3557168893227,
49.8523048372372,50.3488927851517,50.8454807330663,51.3420686809808,51.8386566288953,
52.3352445768099,52.8318325247244,53.3284204726389,53.4070751110264),
 .UNSPECIFIED.);
#697=B_SPLINE_CURVE_WITH_KNOTS('',3,(#60529,#60530,#60531,#60532,#60533,
#60534,#60535,#60536,#60537,#60538,#60539,#60540,#60541,#60542,#60543,#60544),
 .UNSPECIFIED.,.F.,.F.,(4,1,1,1,1,1,1,1,1,1,1,1,1,4),(47.1238898038468,
47.5315771398742,48.0281650877888,48.5247530357033,49.0213409836178,49.5179289315324,
50.0145168794469,50.5111048273614,51.007692775276,51.5042807231905,52.000868671105,
52.4974566190196,52.9940445669341,53.4070751110264),.UNSPECIFIED.);
#698=B_SPLINE_CURVE_WITH_KNOTS('',3,(#60549,#60550,#60551,#60552,#60553,
#60554,#60555,#60556,#60557,#60558,#60559,#60560,#60561,#60562,#60563,#60564,
#60565),.UNSPECIFIED.,.F.,.F.,(4,1,1,1,1,1,1,1,1,1,1,1,1,1,4),(40.8407044966673,
40.9137217747756,41.4103097226902,41.9068976706047,42.4034856185192,42.9000735664337,
43.3966615143483,43.8932494622628,44.3898374101773,44.8864253580919,45.3830133060064,
45.8796012539209,46.3761892018355,46.87277714975,47.1238898038468),
 .UNSPECIFIED.);
#699=B_SPLINE_CURVE_WITH_KNOTS('',3,(#60566,#60567,#60568,#60569,#60570,
#60571,#60572,#60573,#60574,#60575,#60576,#60577,#60578,#60579,#60580,#60581,
#60582),.UNSPECIFIED.,.F.,.F.,(4,1,1,1,1,1,1,1,1,1,1,1,1,1,4),(40.8407044966672,
41.0759338169853,41.5725217648998,42.0691097128144,42.5656976607289,43.0622856086434,
43.558873556558,44.0554615044725,44.552049452387,45.0486374003016,45.5452253482161,
46.0418132961306,46.5384012440452,47.0349891919597,47.1238898038468),
 .UNSPECIFIED.);
#700=B_SPLINE_CURVE_WITH_KNOTS('',3,(#60587,#60588,#60589,#60590,#60591,
#60592,#60593,#60594,#60595,#60596,#60597,#60598,#60599,#60600,#60601,#60602),
 .UNSPECIFIED.,.F.,.F.,(4,1,1,1,1,1,1,1,1,1,1,1,1,4),(34.5575191894877,
34.9546663998012,35.4512543477158,35.9478422956303,36.4444302435448,36.9410181914593,
37.4376061393739,37.9341940872884,38.430782035203,38.9273699831175,39.423957931032,
39.9205458789466,40.4171338268611,40.8407044966673),.UNSPECIFIED.);
#701=B_SPLINE_CURVE_WITH_KNOTS('',3,(#60603,#60604,#60605,#60606,#60607,
#60608,#60609,#60610,#60611,#60612,#60613,#60614,#60615,#60616,#60617,#60618,
#60619),.UNSPECIFIED.,.F.,.F.,(4,1,1,1,1,1,1,1,1,1,1,1,1,1,4),(34.5575191894876,
34.6202904940964,35.1168784420109,35.6134663899254,36.11005433784,36.6066422857545,
37.103230233669,37.5998181815836,38.0964061294981,38.5929940774126,39.0895820253272,
39.5861699732417,40.0827579211562,40.5793458690708,40.8407044966672),
 .UNSPECIFIED.);
#702=B_SPLINE_CURVE_WITH_KNOTS('',3,(#60624,#60625,#60626,#60627,#60628,
#60629,#60630,#60631,#60632,#60633,#60634,#60635,#60636,#60637,#60638,#60639,
#60640),.UNSPECIFIED.,.F.,.F.,(4,1,1,1,1,1,1,1,1,1,1,1,1,1,4),(28.2743338823081,
28.4990230769123,28.9956110248268,29.4921989727414,29.9887869206559,30.4853748685704,
30.981962816485,31.4785507643995,31.975138712314,32.4717266602286,32.9683146081431,
33.4649025560576,33.9614905039722,34.4580784518867,34.5575191894877),
 .UNSPECIFIED.);
#703=B_SPLINE_CURVE_WITH_KNOTS('',3,(#60641,#60642,#60643,#60644,#60645,
#60646,#60647,#60648,#60649,#60650,#60651,#60652,#60653,#60654,#60655,#60656),
 .UNSPECIFIED.,.F.,.F.,(4,1,1,1,1,1,1,1,1,1,1,1,1,4),(28.274333882308,28.661235119122,
29.1578230670365,29.6544110149511,30.1509989628656,30.6475869107801,31.1441748586947,
31.6407628066092,32.1373507545237,32.6339387024382,33.1305266503528,33.6271145982673,
34.1237025461818,34.5575191894876),.UNSPECIFIED.);
#704=B_SPLINE_CURVE_WITH_KNOTS('',3,(#60661,#60662,#60663,#60664,#60665,
#60666,#60667,#60668,#60669,#60670,#60671,#60672,#60673,#60674,#60675,#60676,
#60677),.UNSPECIFIED.,.F.,.F.,(4,1,1,1,1,1,1,1,1,1,1,1,1,1,4),(21.9911485751285,
22.0433797540234,22.5399677019379,23.0365556498524,23.533143597767,24.0297315456815,
24.526319493596,25.0229074415106,25.5194953894251,26.0160833373396,26.5126712852542,
27.0092592331687,27.5058471810832,28.0024351289978,28.2743338823081),
 .UNSPECIFIED.);
#705=B_SPLINE_CURVE_WITH_KNOTS('',3,(#60678,#60679,#60680,#60681,#60682,
#60683,#60684,#60685,#60686,#60687,#60688,#60689,#60690,#60691,#60692,#60693,
#60694),.UNSPECIFIED.,.F.,.F.,(4,1,1,1,1,1,1,1,1,1,1,1,1,1,4),(21.9911485751285,
22.2055917962331,22.7021797441476,23.1987676920621,23.6953556399767,24.1919435878912,
24.6885315358057,25.1851194837203,25.6817074316348,26.1782953795493,26.6748833274639,
27.1714712753784,27.6680592232929,28.1646471712075,28.274333882308),
 .UNSPECIFIED.);
#706=B_SPLINE_CURVE_WITH_KNOTS('',3,(#60699,#60700,#60701,#60702,#60703,
#60704,#60705,#60706,#60707,#60708,#60709,#60710,#60711,#60712,#60713,#60714),
 .UNSPECIFIED.,.F.,.F.,(4,1,1,1,1,1,1,1,1,1,1,1,1,4),(15.7079632679489,
16.084324379049,16.5809123269635,17.077500274878,17.5740882227926,18.0706761707071,
18.5672641186216,19.0638520665362,19.5604400144507,20.0570279623652,20.5536159102798,
21.0502038581943,21.5467918061088,21.9911485751285),.UNSPECIFIED.);
#707=B_SPLINE_CURVE_WITH_KNOTS('',3,(#60715,#60716,#60717,#60718,#60719,
#60720,#60721,#60722,#60723,#60724,#60725,#60726,#60727,#60728,#60729,#60730,
#60731),.UNSPECIFIED.,.F.,.F.,(4,1,1,1,1,1,1,1,1,1,1,1,1,1,4),(15.7079632679489,
15.7499484733441,16.2465364212587,16.7431243691732,17.2397123170877,17.7363002650023,
18.2328882129168,18.7294761608313,19.2260641087459,19.7226520566604,20.2192400045749,
20.7158279524895,21.212415900404,21.7090038483185,21.9911485751285),
 .UNSPECIFIED.);
#708=B_SPLINE_CURVE_WITH_KNOTS('',3,(#61761,#61762,#61763,#61764,#61765,
#61766,#61767,#61768,#61769,#61770,#61771,#61772,#61773,#61774,#61775,#61776,
#61777,#61778,#61779,#61780,#61781,#61782,#61783,#61784,#61785,#61786,#61787,
#61788,#61789,#61790,#61791,#61792,#61793,#61794,#61795,#61796,#61797,#61798,
#61799,#61800,#61801,#61802,#61803,#61804,#61805,#61806,#61807,#61808,#61809,
#61810,#61811,#61812,#61813,#61814,#61815,#61816,#61817,#61818,#61819,#61820,
#61821,#61822,#61823,#61824,#61825,#61826,#61827,#61828,#61829,#61830,#61831,
#61832,#61833,#61834,#61835,#61836),.UNSPECIFIED.,.F.,.F.,(4,3,3,3,3,3,
3,3,3,3,3,3,3,3,3,3,3,3,3,3,3,3,3,3,3,4),(-1.52870610664534,-1.45875428118923,
-1.36271669471793,-1.32921490599004,-1.30256164282083,-1.18858278906243,
-1.14799636029883,-1.11926343500615,-1.09549660338738,-1.07460393530403,
-0.96768361724423,-0.861785228504725,-0.833450674047083,-0.811863192114468,
-0.703084143195483,-0.61351376138071,-0.562609972317118,-0.542202235390156,
-0.440214809144416,-0.344802615936392,-0.29702980114962,-0.270112033817159,
-0.247220523001207,-0.1471419036383,-0.0490185288914403,0.),
 .UNSPECIFIED.);
#709=B_SPLINE_CURVE_WITH_KNOTS('',3,(#61837,#61838,#61839,#61840,#61841,
#61842,#61843,#61844,#61845,#61846,#61847,#61848,#61849,#61850,#61851,#61852,
#61853,#61854,#61855,#61856,#61857,#61858,#61859,#61860,#61861),
 .UNSPECIFIED.,.F.,.F.,(4,3,3,3,3,3,3,3,4),(120.504169542555,120.670871343231,
121.167459291146,121.664047239061,122.160635186975,122.65722313489,123.153811082804,
123.650399030719,124.058352297607),.UNSPECIFIED.);
#710=B_SPLINE_CURVE_WITH_KNOTS('',3,(#61863,#61864,#61865,#61866,#61867,
#61868,#61869,#61870,#61871,#61872,#61873,#61874,#61875,#61876,#61877,#61878,
#61879,#61880,#61881,#61882,#61883,#61884,#61885,#61886,#61887,#61888,#61889,
#61890,#61891,#61892,#61893,#61894,#61895,#61896,#61897,#61898,#61899,#61900,
#61901,#61902,#61903,#61904,#61905,#61906,#61907,#61908,#61909,#61910,#61911,
#61912,#61913,#61914,#61915,#61916,#61917,#61918,#61919,#61920,#61921,#61922,
#61923,#61924,#61925,#61926,#61927,#61928,#61929,#61930,#61931,#61932,#61933,
#61934,#61935),.UNSPECIFIED.,.F.,.F.,(4,3,3,3,3,3,3,3,3,3,3,3,3,3,3,3,3,
3,3,3,3,3,3,3,4),(-1.5337369924875,-1.47310339793522,-1.38616089135255,
-1.35553579127592,-1.32729232344809,-1.22631284752631,-1.18227376682654,
-1.1511716128867,-1.12533337160453,-1.02273077361868,-0.95087425227154,
-0.895171890823101,-0.873398340368991,-0.763527429133733,-0.669727116015181,
-0.613941195435186,-0.58473597398091,-0.476777077099686,-0.388326176659527,
-0.338096679615524,-0.310206788241938,-0.28811604023779,-0.178935998268544,
-0.0688709899600637,0.),.UNSPECIFIED.);
#711=B_SPLINE_CURVE_WITH_KNOTS('',3,(#61936,#61937,#61938,#61939,#61940,
#61941,#61942,#61943,#61944,#61945,#61946,#61947,#61948,#61949),
 .UNSPECIFIED.,.F.,.F.,(4,1,1,1,1,1,1,1,1,1,1,4),(10.3761157273101,10.7840689941988,
11.2806569421133,11.7772448900279,12.2738328379424,12.7704207858569,13.2670087337715,
13.763596681686,14.2601846296005,14.7567725775151,15.2533605254296,15.7079632679489),
 .UNSPECIFIED.);
#712=B_SPLINE_CURVE_WITH_KNOTS('',3,(#61955,#61956,#61957,#61958,#61959,
#61960,#61961,#61962,#61963,#61964,#61965,#61966,#61967,#61968,#61969,#61970,
#61971,#61972,#61973,#61974,#61975,#61976,#61977,#61978,#61979,#61980,#61981,
#61982,#61983,#61984,#61985,#61986,#61987,#61988,#61989,#61990,#61991,#61992,
#61993,#61994,#61995,#61996,#61997,#61998,#61999,#62000,#62001,#62002,#62003,
#62004,#62005,#62006,#62007,#62008,#62009,#62010,#62011,#62012,#62013,#62014,
#62015,#62016,#62017,#62018,#62019,#62020,#62021,#62022,#62023,#62024,#62025,
#62026,#62027,#62028,#62029,#62030),.UNSPECIFIED.,.F.,.F.,(4,3,3,3,3,3,
3,3,3,3,3,3,3,3,3,3,3,3,3,3,3,3,3,3,3,4),(-1.52870610664514,-1.45875428118896,
-1.36271669471769,-1.32921490384452,-1.30256164016884,-1.18858278773635,
-1.1479963595685,-1.11926343453104,-1.09549660342904,-1.07460393530387,
-0.967683620479759,-0.861785252473329,-0.833450706753318,-0.811863217327338,
-0.70308414319544,-0.613513761380673,-0.562609973423642,-0.542202235080821,
-0.440214783048228,-0.344802615936372,-0.29702979072875,-0.270111989456298,
-0.247220519065303,-0.147141901650714,-0.0490185840864301,0.),
 .UNSPECIFIED.);
#713=B_SPLINE_CURVE_WITH_KNOTS('',3,(#62033,#62034,#62035,#62036,#62037,
#62038,#62039,#62040,#62041,#62042,#62043,#62044),.UNSPECIFIED.,.F.,.F.,
(4,1,1,1,1,1,1,1,1,4),(11.6150328478182,12.1116207957327,12.6082087436472,
13.1047966915618,13.6013846394763,14.0979725873908,14.5945605353054,15.0911484832199,
15.5877364311344,15.7079632679489),.UNSPECIFIED.);
#714=B_SPLINE_CURVE_WITH_KNOTS('',3,(#63074,#63075,#63076,#63077,#63078,
#63079,#63080,#63081,#63082,#63083,#63084,#63085,#63086,#63087,#63088,#63089,
#63090,#63091,#63092,#63093,#63094,#63095,#63096,#63097,#63098,#63099,#63100,
#63101,#63102,#63103,#63104,#63105,#63106,#63107,#63108,#63109,#63110,#63111,
#63112,#63113,#63114,#63115,#63116,#63117,#63118,#63119,#63120,#63121,#63122,
#63123,#63124,#63125,#63126,#63127,#63128,#63129,#63130,#63131,#63132,#63133,
#63134,#63135,#63136,#63137,#63138,#63139,#63140,#63141,#63142,#63143,#63144,
#63145,#63146),.UNSPECIFIED.,.F.,.F.,(4,3,3,3,3,3,3,3,3,3,3,3,3,3,3,3,3,
3,3,3,3,3,3,3,4),(-1.5337369924876,-1.47310339793536,-1.38616089135267,
-1.35553578686801,-1.32729232205323,-1.22631284682892,-1.18227376953103,
-1.15117161312205,-1.12533337160461,-1.02273077778506,-0.950874246236159,
-0.895171881876995,-0.873398336433576,-0.763527429133767,-0.669727116015206,
-0.613941186551684,-0.584735970127757,-0.476777077545073,-0.388326176659522,
-0.338096682547795,-0.310206794898333,-0.288116047041532,-0.178935969781343,
-0.0688709821527319,0.),.UNSPECIFIED.);
#715=B_SPLINE_CURVE_WITH_KNOTS('',3,(#63147,#63148,#63149,#63150,#63151,
#63152,#63153,#63154,#63155,#63156,#63157,#63158,#63159,#63160,#63161,#63162,
#63163,#63164,#63165),.UNSPECIFIED.,.F.,.F.,(4,3,3,3,3,3,4),(-126.133338770291,
-125.636750822377,-125.140162874462,-124.643574926548,-124.146986978633,
-123.650399030719,-123.473451256543),.UNSPECIFIED.);
#716=B_SPLINE_CURVE_WITH_KNOTS('',3,(#63548,#63549,#63550,#63551,#63552,
#63553,#63554,#63555,#63556,#63557,#63558,#63559,#63560,#63561,#63562,#63563),
 .UNSPECIFIED.,.F.,.F.,(4,3,3,3,3,4),(-4.09254174883827,-3.99528148587419,
-3.49587130013992,-2.99646111440564,-2.49705092867137,-2.06980418878615),
 .UNSPECIFIED.);
#717=B_SPLINE_CURVE_WITH_KNOTS('',3,(#63566,#63567,#63568,#63569,#63570,
#63571,#63572,#63573,#63574,#63575),.UNSPECIFIED.,.F.,.F.,(4,3,3,4),(0.,
0.499410185734265,0.998820371468536,1.11885509353751),.UNSPECIFIED.);
#718=B_SPLINE_CURVE_WITH_KNOTS('',3,(#63580,#63581,#63582,#63583,#63584,
#63585,#63586,#63587,#63588,#63589,#63590,#63591,#63592,#63593,#63594,#63595,
#63596,#63597,#63598,#63599,#63600,#63601,#63602,#63603,#63604,#63605,#63606,
#63607,#63608,#63609,#63610,#63611,#63612,#63613,#63614,#63615,#63616,#63617,
#63618,#63619),.UNSPECIFIED.,.F.,.F.,(4,3,3,3,3,3,3,3,3,3,3,3,3,4),(-10.3757270560179,
-9.98820371468548,-9.48879352895121,-8.98938334321694,-8.48997315748266,
-7.99056297174839,-7.49115278601411,-6.99174260027984,-6.49233241454556,
-5.99292222881129,-5.49351204307701,-4.99410185734274,-4.49469167160847,
-4.09254174883827),.UNSPECIFIED.);
#719=B_SPLINE_CURVE_WITH_KNOTS('',3,(#63620,#63621,#63622,#63623,#63624,
#63625,#63626,#63627,#63628,#63629,#63630,#63631,#63632,#63633,#63634,#63635,
#63636,#63637,#63638,#63639,#63640,#63641,#63642,#63643,#63644,#63645,#63646,
#63647,#63648,#63649,#63650,#63651,#63652,#63653,#63654,#63655,#63656,#63657,
#63658,#63659),.UNSPECIFIED.,.F.,.F.,(4,3,3,3,3,3,3,3,3,3,3,3,3,4),(1.11885509353751,
1.49823055720281,1.99764074293709,2.49705092867136,2.99646111440564,3.49587130013992,
3.99528148587419,4.49469167160847,4.99410185734275,5.49351204307702,5.9929222288113,
6.49233241454557,6.99174260027985,7.40204040071709),.UNSPECIFIED.);
#720=B_SPLINE_CURVE_WITH_KNOTS('',3,(#63664,#63665,#63666,#63667,#63668,
#63669,#63670,#63671,#63672,#63673,#63674,#63675,#63676,#63677,#63678,#63679,
#63680,#63681,#63682,#63683,#63684,#63685,#63686,#63687,#63688,#63689,#63690,
#63691,#63692,#63693,#63694,#63695,#63696,#63697,#63698,#63699,#63700,#63701,
#63702,#63703,#63704,#63705,#63706),.UNSPECIFIED.,.F.,.F.,(4,3,3,3,3,3,
3,3,3,3,3,3,3,3,4),(-16.6589123631974,-16.480536129231,-15.9811259434968,
-15.4817157577625,-14.9823055720282,-14.4828953862939,-13.9834852005597,
-13.4840750148254,-12.9846648290911,-12.4852546433568,-11.9858444576226,
-11.4864342718883,-10.987024086154,-10.4876139004198,-10.3757270560179),
 .UNSPECIFIED.);
#721=B_SPLINE_CURVE_WITH_KNOTS('',3,(#63707,#63708,#63709,#63710,#63711,
#63712,#63713,#63714,#63715,#63716,#63717,#63718,#63719,#63720,#63721,#63722,
#63723,#63724,#63725,#63726,#63727,#63728,#63729,#63730,#63731,#63732,#63733,
#63734,#63735,#63736,#63737,#63738,#63739,#63740,#63741,#63742,#63743,#63744,
#63745,#63746,#63747,#63748,#63749),.UNSPECIFIED.,.F.,.F.,(4,3,3,3,3,3,
3,3,3,3,3,3,3,3,4),(7.40204040071709,7.49115278601413,7.9905629717484,8.48997315748267,
8.98938334321695,9.48879352895122,9.98820371468549,10.4876139004198,10.987024086154,
11.4864342718883,11.9858444576226,12.4852546433569,12.9846648290911,13.4840750148254,
13.6852257078967),.UNSPECIFIED.);
#722=B_SPLINE_CURVE_WITH_KNOTS('',3,(#63754,#63755,#63756,#63757,#63758,
#63759,#63760,#63761,#63762,#63763,#63764,#63765,#63766,#63767,#63768,#63769,
#63770,#63771,#63772,#63773,#63774,#63775,#63776,#63777,#63778,#63779,#63780,
#63781,#63782,#63783,#63784,#63785,#63786,#63787,#63788,#63789,#63790,#63791,
#63792,#63793),.UNSPECIFIED.,.F.,.F.,(4,3,3,3,3,3,3,3,3,3,3,3,3,4),(-22.942097670377,
-22.4734583580423,-21.9740481723081,-21.4746379865738,-20.9752278008395,
-20.4758176151052,-19.976407429371,-19.4769972436367,-18.9775870579024,
-18.4781768721681,-17.9787666864339,-17.4793565006996,-16.9799463149653,
-16.6589123631974),.UNSPECIFIED.);
#723=B_SPLINE_CURVE_WITH_KNOTS('',3,(#63794,#63795,#63796,#63797,#63798,
#63799,#63800,#63801,#63802,#63803,#63804,#63805,#63806,#63807,#63808,#63809,
#63810,#63811,#63812,#63813,#63814,#63815,#63816,#63817,#63818,#63819,#63820,
#63821,#63822,#63823,#63824,#63825,#63826,#63827,#63828,#63829,#63830,#63831,
#63832,#63833),.UNSPECIFIED.,.F.,.F.,(4,3,3,3,3,3,3,3,3,3,3,3,3,4),(13.6852257078967,
13.9834852005597,14.482895386294,14.9823055720282,15.4817157577625,15.9811259434968,
16.480536129231,16.9799463149653,17.4793565006996,17.9787666864339,18.4781768721681,
18.9775870579024,19.4769972436367,19.9684110150763),.UNSPECIFIED.);
#724=B_SPLINE_CURVE_WITH_KNOTS('',3,(#63838,#63839,#63840,#63841,#63842,
#63843,#63844,#63845,#63846,#63847,#63848,#63849,#63850,#63851,#63852,#63853,
#63854,#63855,#63856,#63857,#63858,#63859,#63860,#63861,#63862,#63863,#63864,
#63865,#63866,#63867,#63868,#63869,#63870,#63871,#63872,#63873,#63874,#63875,
#63876,#63877,#63878,#63879,#63880),.UNSPECIFIED.,.F.,.F.,(4,3,3,3,3,3,
3,3,3,3,3,3,3,3,4),(-29.2252829775566,-28.9657907725879,-28.4663805868536,
-27.9669704011194,-27.4675602153851,-26.9681500296508,-26.4687398439165,
-25.9693296581823,-25.469919472448,-24.9705092867137,-24.4710991009794,
-23.9716889152452,-23.4722787295109,-22.9728685437766,-22.942097670377),
 .UNSPECIFIED.);
#725=B_SPLINE_CURVE_WITH_KNOTS('',3,(#63881,#63882,#63883,#63884,#63885,
#63886,#63887,#63888,#63889,#63890,#63891,#63892,#63893,#63894,#63895,#63896,
#63897,#63898,#63899,#63900,#63901,#63902,#63903,#63904,#63905,#63906,#63907,
#63908,#63909,#63910,#63911,#63912,#63913,#63914,#63915,#63916,#63917,#63918,
#63919,#63920,#63921,#63922,#63923),.UNSPECIFIED.,.F.,.F.,(4,3,3,3,3,3,
3,3,3,3,3,3,3,3,4),(19.9684110150763,19.9764074293709,20.4758176151052,
20.9752278008395,21.4746379865738,21.974048172308,22.4734583580423,22.9728685437766,
23.4722787295109,23.9716889152451,24.4710991009794,24.9705092867137,25.469919472448,
25.9693296581822,26.2515963222559),.UNSPECIFIED.);
#726=B_SPLINE_CURVE_WITH_KNOTS('',3,(#63928,#63929,#63930,#63931,#63932,
#63933,#63934,#63935,#63936,#63937,#63938,#63939,#63940,#63941,#63942,#63943,
#63944,#63945,#63946,#63947,#63948,#63949,#63950,#63951,#63952,#63953,#63954,
#63955,#63956,#63957,#63958,#63959,#63960,#63961,#63962,#63963,#63964,#63965,
#63966,#63967,#63968,#63969,#63970),.UNSPECIFIED.,.F.,.F.,(4,3,3,3,3,3,
3,3,3,3,3,3,3,3,4),(-35.5084682847362,-35.4581231871335,-34.9587130013992,
-34.4593028156649,-33.9598926299306,-33.4604824441964,-32.9610722584621,
-32.4616620727278,-31.9622518869935,-31.4628417012593,-30.963431515525,
-30.4640213297907,-29.9646111440564,-29.4652009583222,-29.2252829775566),
 .UNSPECIFIED.);
#727=B_SPLINE_CURVE_WITH_KNOTS('',3,(#63971,#63972,#63973,#63974,#63975,
#63976,#63977,#63978,#63979,#63980,#63981,#63982,#63983,#63984,#63985,#63986,
#63987,#63988,#63989,#63990,#63991,#63992,#63993,#63994,#63995,#63996,#63997,
#63998,#63999,#64000,#64001,#64002,#64003,#64004,#64005,#64006,#64007,#64008,
#64009,#64010,#64011,#64012,#64013),.UNSPECIFIED.,.F.,.F.,(4,3,3,3,3,3,
3,3,3,3,3,3,3,3,4),(26.2515963222559,26.4687398439165,26.9681500296508,
27.4675602153851,27.9669704011193,28.4663805868536,28.9657907725879,29.4652009583222,
29.9646111440564,30.4640213297907,30.963431515525,31.4628417012593,31.9622518869935,
32.4616620727278,32.5347816294354),.UNSPECIFIED.);
#728=B_SPLINE_CURVE_WITH_KNOTS('',3,(#64018,#64019,#64020,#64021,#64022,
#64023,#64024,#64025,#64026,#64027,#64028,#64029,#64030,#64031,#64032,#64033,
#64034,#64035,#64036,#64037,#64038,#64039,#64040,#64041,#64042,#64043,#64044,
#64045,#64046,#64047,#64048,#64049,#64050,#64051,#64052,#64053,#64054,#64055,
#64056,#64057),.UNSPECIFIED.,.F.,.F.,(4,3,3,3,3,3,3,3,3,3,3,3,3,4),(-41.7916535919158,
-41.4510454159447,-40.9516352302105,-40.4522250444762,-39.9528148587419,
-39.4534046730076,-38.9539944872734,-38.4545843015391,-37.9551741158048,
-37.4557639300706,-36.9563537443363,-36.456943558602,-35.9575333728677,
-35.5084682847362),.UNSPECIFIED.);
#729=B_SPLINE_CURVE_WITH_KNOTS('',3,(#64058,#64059,#64060,#64061,#64062,
#64063,#64064,#64065,#64066,#64067,#64068,#64069,#64070,#64071,#64072,#64073,
#64074,#64075,#64076,#64077,#64078,#64079,#64080,#64081,#64082,#64083,#64084,
#64085,#64086,#64087,#64088,#64089,#64090,#64091,#64092,#64093,#64094,#64095,
#64096,#64097),.UNSPECIFIED.,.F.,.F.,(4,3,3,3,3,3,3,3,3,3,3,3,3,4),(32.5347816294354,
32.9610722584621,33.4604824441964,33.9598926299306,34.4593028156649,34.9587130013992,
35.4581231871335,35.9575333728677,36.456943558602,36.9563537443363,37.4557639300705,
37.9551741158048,38.4545843015391,38.817966936615),.UNSPECIFIED.);
#730=B_SPLINE_CURVE_WITH_KNOTS('',3,(#64102,#64103,#64104,#64105,#64106,
#64107,#64108,#64109,#64110,#64111,#64112,#64113,#64114,#64115,#64116,#64117,
#64118,#64119,#64120,#64121,#64122,#64123,#64124,#64125,#64126,#64127,#64128,
#64129,#64130,#64131,#64132,#64133,#64134,#64135,#64136,#64137,#64138,#64139,
#64140,#64141,#64142,#64143,#64144),.UNSPECIFIED.,.F.,.F.,(4,3,3,3,3,3,
3,3,3,3,3,3,3,3,4),(-48.0748388990954,-47.9433778304903,-47.443967644756,
-46.9445574590218,-46.4451472732875,-45.9457370875532,-45.4463269018189,
-44.9469167160847,-44.4475065303504,-43.9480963446161,-43.4486861588818,
-42.9492759731476,-42.4498657874133,-41.950455601679,-41.7916535919158),
 .UNSPECIFIED.);
#731=B_SPLINE_CURVE_WITH_KNOTS('',3,(#64145,#64146,#64147,#64148,#64149,
#64150,#64151,#64152,#64153,#64154,#64155,#64156,#64157,#64158,#64159,#64160,
#64161,#64162,#64163,#64164,#64165,#64166,#64167,#64168,#64169,#64170,#64171,
#64172,#64173,#64174,#64175,#64176,#64177,#64178,#64179,#64180,#64181,#64182,
#64183,#64184,#64185,#64186,#64187),.UNSPECIFIED.,.F.,.F.,(4,3,3,3,3,3,
3,3,3,3,3,3,3,3,4),(38.817966936615,38.9539944872734,39.4534046730076,39.9528148587419,
40.4522250444762,40.9516352302105,41.4510454159447,41.950455601679,42.4498657874133,
42.9492759731476,43.4486861588818,43.9480963446161,44.4475065303504,44.9469167160847,
45.1011522437946),.UNSPECIFIED.);
#732=B_SPLINE_CURVE_WITH_KNOTS('',3,(#64192,#64193,#64194,#64195,#64196,
#64197,#64198,#64199,#64200,#64201,#64202,#64203,#64204,#64205,#64206,#64207,
#64208,#64209,#64210,#64211,#64212,#64213,#64214,#64215,#64216,#64217,#64218,
#64219,#64220,#64221,#64222,#64223,#64224,#64225,#64226,#64227,#64228,#64229,
#64230,#64231),.UNSPECIFIED.,.F.,.F.,(4,3,3,3,3,3,3,3,3,3,3,3,3,4),(-54.358024206275,
-53.9363000593016,-53.4368898735673,-52.937479687833,-52.4380695020988,
-51.9386593163645,-51.4392491306302,-50.939838944896,-50.4404287591617,
-49.9410185734274,-49.4416083876931,-48.9421982019589,-48.4427880162246,
-48.0748388990954),.UNSPECIFIED.);
#733=B_SPLINE_CURVE_WITH_KNOTS('',3,(#64232,#64233,#64234,#64235,#64236,
#64237,#64238,#64239,#64240,#64241,#64242,#64243,#64244,#64245,#64246,#64247,
#64248,#64249,#64250,#64251,#64252,#64253,#64254,#64255,#64256,#64257,#64258,
#64259,#64260,#64261,#64262,#64263,#64264,#64265,#64266,#64267,#64268,#64269,
#64270,#64271),.UNSPECIFIED.,.F.,.F.,(4,3,3,3,3,3,3,3,3,3,3,3,3,4),(45.1011522437946,
45.4463269018189,45.9457370875532,46.4451472732875,46.9445574590218,47.443967644756,
47.9433778304903,48.4427880162246,48.9421982019588,49.4416083876931,49.9410185734274,
50.4404287591617,50.9398389448959,51.3843375509742),.UNSPECIFIED.);
#734=B_SPLINE_CURVE_WITH_KNOTS('',3,(#64276,#64277,#64278,#64279,#64280,
#64281,#64282,#64283,#64284,#64285,#64286,#64287,#64288,#64289,#64290,#64291,
#64292,#64293,#64294,#64295,#64296,#64297,#64298,#64299,#64300,#64301,#64302,
#64303,#64304,#64305,#64306,#64307,#64308,#64309,#64310,#64311,#64312,#64313,
#64314,#64315,#64316,#64317,#64318),.UNSPECIFIED.,.F.,.F.,(4,3,3,3,3,3,
3,3,3,3,3,3,3,3,4),(-60.6412095134546,-60.4286324738472,-59.9292222881129,
-59.4298121023786,-58.9304019166443,-58.4309917309101,-57.9315815451758,
-57.4321713594415,-56.9327611737072,-56.433350987973,-55.9339408022387,
-55.4345306165044,-54.9351204307702,-54.4357102450359,-54.358024206275),
 .UNSPECIFIED.);
#735=B_SPLINE_CURVE_WITH_KNOTS('',3,(#64319,#64320,#64321,#64322,#64323,
#64324,#64325,#64326,#64327,#64328,#64329,#64330,#64331,#64332,#64333,#64334,
#64335,#64336,#64337,#64338,#64339,#64340,#64341,#64342,#64343,#64344,#64345,
#64346,#64347,#64348,#64349,#64350,#64351,#64352,#64353,#64354,#64355,#64356,
#64357,#64358,#64359,#64360,#64361),.UNSPECIFIED.,.F.,.F.,(4,3,3,3,3,3,
3,3,3,3,3,3,3,3,4),(51.3843375509742,51.4392491306302,51.9386593163645,
52.4380695020988,52.937479687833,53.4368898735673,53.9363000593016,54.4357102450359,
54.9351204307701,55.4345306165044,55.9339408022387,56.433350987973,56.9327611737072,
57.4321713594415,57.6675228581538),.UNSPECIFIED.);
#736=B_SPLINE_CURVE_WITH_KNOTS('',3,(#64366,#64367,#64368,#64369,#64370,
#64371,#64372,#64373,#64374,#64375,#64376,#64377,#64378,#64379,#64380,#64381,
#64382,#64383,#64384,#64385,#64386,#64387,#64388,#64389,#64390,#64391,#64392,
#64393,#64394,#64395,#64396,#64397,#64398,#64399,#64400,#64401,#64402,#64403,
#64404,#64405,#64406,#64407,#64408),.UNSPECIFIED.,.F.,.F.,(4,3,3,3,3,3,
3,3,3,3,3,3,3,3,4),(-66.9243948206342,-66.9209648883927,-66.4215547026584,
-65.9221445169242,-65.4227343311899,-64.9233241454556,-64.4239139597213,
-63.9245037739871,-63.4250935882528,-62.9256834025185,-62.4262732167843,
-61.92686303105,-61.4274528453157,-60.9280426595814,-60.6412095134546),
 .UNSPECIFIED.);
#737=B_SPLINE_CURVE_WITH_KNOTS('',3,(#64409,#64410,#64411,#64412,#64413,
#64414,#64415,#64416,#64417,#64418,#64419,#64420,#64421,#64422,#64423,#64424,
#64425,#64426,#64427,#64428,#64429,#64430,#64431,#64432,#64433,#64434,#64435,
#64436,#64437,#64438,#64439,#64440,#64441,#64442,#64443,#64444,#64445,#64446,
#64447,#64448,#64449,#64450,#64451),.UNSPECIFIED.,.F.,.F.,(4,3,3,3,3,3,
3,3,3,3,3,3,3,3,4),(57.6675228581538,57.9315815451758,58.4309917309101,
58.9304019166443,59.4298121023786,59.9292222881129,60.4286324738472,60.9280426595814,
61.4274528453157,61.92686303105,62.4262732167843,62.9256834025185,63.4250935882528,
63.9245037739871,63.9507081653334),.UNSPECIFIED.);
#738=B_SPLINE_CURVE_WITH_KNOTS('',3,(#64456,#64457,#64458,#64459,#64460,
#64461,#64462,#64463,#64464,#64465,#64466,#64467,#64468,#64469,#64470,#64471,
#64472,#64473,#64474,#64475,#64476,#64477,#64478,#64479,#64480,#64481,#64482,
#64483,#64484,#64485,#64486,#64487,#64488,#64489,#64490,#64491,#64492,#64493,
#64494,#64495),.UNSPECIFIED.,.F.,.F.,(4,3,3,3,3,3,3,3,3,3,3,3,3,4),(-73.2075801278138,
-72.913887117204,-72.4144769314697,-71.9150667457355,-71.4156565600012,
-70.9162463742669,-70.4168361885326,-69.9174260027984,-69.4180158170641,
-68.9186056313298,-68.4191954455955,-67.9197852598613,-67.420375074127,
-66.9243948206342),.UNSPECIFIED.);
#739=B_SPLINE_CURVE_WITH_KNOTS('',3,(#64496,#64497,#64498,#64499,#64500,
#64501,#64502,#64503,#64504,#64505,#64506,#64507,#64508,#64509,#64510,#64511,
#64512,#64513,#64514,#64515,#64516,#64517,#64518,#64519,#64520,#64521,#64522,
#64523,#64524,#64525,#64526,#64527,#64528,#64529,#64530,#64531,#64532,#64533,
#64534,#64535),.UNSPECIFIED.,.F.,.F.,(4,3,3,3,3,3,3,3,3,3,3,3,3,4),(63.9507081653334,
64.4239139597213,64.9233241454556,65.4227343311899,65.9221445169242,66.4215547026584,
66.9209648883927,67.420375074127,67.9197852598613,68.4191954455955,68.9186056313298,
69.4180158170641,69.9174260027984,70.233893472513),.UNSPECIFIED.);
#740=B_SPLINE_CURVE_WITH_KNOTS('',3,(#64540,#64541,#64542,#64543,#64544,
#64545,#64546,#64547,#64548,#64549,#64550,#64551,#64552,#64553,#64554,#64555,
#64556,#64557,#64558,#64559,#64560,#64561,#64562,#64563,#64564,#64565,#64566,
#64567,#64568,#64569,#64570,#64571,#64572,#64573,#64574,#64575,#64576,#64577,
#64578,#64579,#64580,#64581,#64582),.UNSPECIFIED.,.F.,.F.,(4,3,3,3,3,3,
3,3,3,3,3,3,3,3,4),(-79.4907654349934,-79.4062195317496,-78.9068093460153,
-78.407399160281,-77.9079889745468,-77.4085787888125,-76.9091686030782,
-76.4097584173439,-75.9103482316097,-75.4109380458754,-74.9115278601411,
-74.4121176744069,-73.9127074886726,-73.4132973029383,-73.2075801278138),
 .UNSPECIFIED.);
#741=B_SPLINE_CURVE_WITH_KNOTS('',3,(#64583,#64584,#64585,#64586,#64587,
#64588,#64589,#64590,#64591,#64592,#64593,#64594,#64595,#64596,#64597,#64598,
#64599,#64600,#64601,#64602,#64603,#64604,#64605,#64606,#64607,#64608,#64609,
#64610,#64611,#64612,#64613,#64614,#64615,#64616,#64617,#64618,#64619,#64620,
#64621,#64622,#64623,#64624,#64625),.UNSPECIFIED.,.F.,.F.,(4,3,3,3,3,3,
3,3,3,3,3,3,3,3,4),(70.233893472513,70.4168361885326,70.9162463742669,71.4156565600012,
71.9150667457354,72.4144769314697,72.913887117204,73.4132973029382,73.9127074886725,
74.4121176744068,74.9115278601411,75.4109380458754,75.9103482316096,76.4097584173439,
76.5170787796926),.UNSPECIFIED.);
#742=B_SPLINE_CURVE_WITH_KNOTS('',3,(#64630,#64631,#64632,#64633,#64634,
#64635,#64636,#64637,#64638,#64639,#64640,#64641,#64642,#64643,#64644,#64645,
#64646,#64647,#64648,#64649,#64650,#64651,#64652,#64653,#64654,#64655,#64656,
#64657,#64658,#64659,#64660,#64661,#64662,#64663,#64664,#64665,#64666,#64667,
#64668,#64669),.UNSPECIFIED.,.F.,.F.,(4,3,3,3,3,3,3,3,3,3,3,3,3,4),(-85.773950742173,
-85.3991417605609,-84.8997315748266,-84.4003213890923,-83.900911203358,
-83.4015010176238,-82.9020908318895,-82.4026806461552,-81.9032704604209,
-81.4038602746867,-80.9044500889524,-80.4050399032181,-79.9056297174838,
-79.4907654349934),.UNSPECIFIED.);
#743=B_SPLINE_CURVE_WITH_KNOTS('',3,(#64670,#64671,#64672,#64673,#64674,
#64675,#64676,#64677,#64678,#64679,#64680,#64681,#64682,#64683,#64684,#64685,
#64686,#64687,#64688,#64689,#64690,#64691,#64692,#64693,#64694,#64695,#64696,
#64697,#64698,#64699,#64700,#64701,#64702,#64703,#64704,#64705,#64706,#64707,
#64708,#64709),.UNSPECIFIED.,.F.,.F.,(4,3,3,3,3,3,3,3,3,3,3,3,3,4),(76.5170787796926,
76.9091686030782,77.4085787888124,77.9079889745467,78.407399160281,78.9068093460153,
79.4062195317496,79.9056297174838,80.4050399032181,80.9044500889524,81.4038602746867,
81.9032704604209,82.4026806461552,82.8002640868722),.UNSPECIFIED.);
#744=B_SPLINE_CURVE_WITH_KNOTS('',3,(#64714,#64715,#64716,#64717,#64718,
#64719,#64720,#64721,#64722,#64723,#64724,#64725,#64726,#64727,#64728,#64729,
#64730,#64731,#64732,#64733,#64734,#64735,#64736,#64737,#64738,#64739,#64740,
#64741,#64742,#64743,#64744,#64745,#64746,#64747,#64748,#64749,#64750,#64751,
#64752,#64753,#64754,#64755,#64756),.UNSPECIFIED.,.F.,.F.,(4,3,3,3,3,3,
3,3,3,3,3,3,3,3,4),(-92.0571360493526,-91.8914741751064,-91.3920639893721,
-90.8926538036379,-90.3932436179036,-89.8938334321693,-89.3944232464351,
-88.8950130607008,-88.3956028749665,-87.8961926892322,-87.396782503498,
-86.8973723177637,-86.3979621320294,-85.8985519462951,-85.773950742173),
 .UNSPECIFIED.);
#745=B_SPLINE_CURVE_WITH_KNOTS('',3,(#64757,#64758,#64759,#64760,#64761,
#64762,#64763,#64764,#64765,#64766,#64767,#64768,#64769,#64770,#64771,#64772,
#64773,#64774,#64775,#64776,#64777,#64778,#64779,#64780,#64781,#64782,#64783,
#64784,#64785,#64786,#64787,#64788,#64789,#64790,#64791,#64792,#64793,#64794,
#64795,#64796,#64797,#64798,#64799),.UNSPECIFIED.,.F.,.F.,(4,3,3,3,3,3,
3,3,3,3,3,3,3,3,4),(82.8002640868722,82.9020908318895,83.4015010176238,
83.900911203358,84.4003213890923,84.8997315748266,85.3991417605608,85.8985519462951,
86.3979621320294,86.8973723177637,87.3967825034979,87.8961926892322,88.3956028749665,
88.8950130607008,89.0834493940518),.UNSPECIFIED.);
#746=B_SPLINE_CURVE_WITH_KNOTS('',3,(#64804,#64805,#64806,#64807,#64808,
#64809,#64810,#64811,#64812,#64813,#64814,#64815,#64816,#64817,#64818,#64819,
#64820,#64821,#64822,#64823,#64824,#64825,#64826,#64827,#64828,#64829,#64830,
#64831,#64832,#64833,#64834,#64835,#64836,#64837,#64838,#64839,#64840,#64841,
#64842,#64843),.UNSPECIFIED.,.F.,.F.,(4,3,3,3,3,3,3,3,3,3,3,3,3,4),(-98.3403213565321,
-97.8843964039177,-97.3849862181834,-96.8855760324492,-96.3861658467149,
-95.8867556609806,-95.3873454752463,-94.8879352895121,-94.3885251037778,
-93.8891149180435,-93.3897047323093,-92.890294546575,-92.3908843608407,
-92.0571360493526),.UNSPECIFIED.);
#747=B_SPLINE_CURVE_WITH_KNOTS('',3,(#64844,#64845,#64846,#64847,#64848,
#64849,#64850,#64851,#64852,#64853,#64854,#64855,#64856,#64857,#64858,#64859,
#64860,#64861,#64862,#64863,#64864,#64865,#64866,#64867,#64868,#64869,#64870,
#64871,#64872,#64873,#64874,#64875,#64876,#64877,#64878,#64879,#64880,#64881,
#64882,#64883),.UNSPECIFIED.,.F.,.F.,(4,3,3,3,3,3,3,3,3,3,3,3,3,4),(89.0834493940518,
89.394423246435,89.8938334321693,90.3932436179036,90.8926538036378,91.3920639893721,
91.8914741751064,92.3908843608407,92.8902945465749,93.3897047323092,93.8891149180435,
94.3885251037778,94.887935289512,95.3666347012314),.UNSPECIFIED.);
#748=B_SPLINE_CURVE_WITH_KNOTS('',3,(#64888,#64889,#64890,#64891,#64892,
#64893,#64894,#64895,#64896,#64897,#64898,#64899,#64900,#64901,#64902,#64903,
#64904,#64905,#64906,#64907,#64908,#64909,#64910,#64911,#64912,#64913,#64914,
#64915,#64916,#64917,#64918,#64919,#64920,#64921,#64922,#64923,#64924,#64925,
#64926,#64927,#64928,#64929,#64930),.UNSPECIFIED.,.F.,.F.,(4,3,3,3,3,3,
3,3,3,3,3,3,3,3,4),(-104.623506663712,-104.376728818463,-103.877318632729,
-103.377908446995,-102.87849826126,-102.379088075526,-101.879677889792,
-101.380267704058,-100.880857518323,-100.381447332589,-99.8820371468548,
-99.3826269611206,-98.8832167753863,-98.383806589652,-98.3403213565321),
 .UNSPECIFIED.);
#749=B_SPLINE_CURVE_WITH_KNOTS('',3,(#64931,#64932,#64933,#64934,#64935,
#64936,#64937,#64938,#64939,#64940,#64941,#64942,#64943,#64944,#64945,#64946,
#64947,#64948,#64949,#64950,#64951,#64952,#64953,#64954,#64955,#64956,#64957,
#64958,#64959,#64960,#64961,#64962,#64963,#64964,#64965,#64966,#64967,#64968,
#64969,#64970,#64971,#64972,#64973),.UNSPECIFIED.,.F.,.F.,(4,3,3,3,3,3,
3,3,3,3,3,3,3,3,4),(95.3666347012314,95.3873454752463,95.8867556609806,
96.3861658467149,96.8855760324491,97.3849862181834,97.8843964039177,98.383806589652,
98.8832167753862,99.3826269611205,99.8820371468548,100.381447332589,100.880857518323,
101.380267704058,101.649820008411),.UNSPECIFIED.);
#750=B_SPLINE_CURVE_WITH_KNOTS('',3,(#64978,#64979,#64980,#64981,#64982,
#64983,#64984,#64985,#64986,#64987,#64988,#64989,#64990,#64991,#64992,#64993,
#64994,#64995,#64996,#64997,#64998,#64999,#65000,#65001,#65002,#65003,#65004,
#65005,#65006,#65007,#65008,#65009,#65010,#65011,#65012,#65013,#65014,#65015,
#65016,#65017,#65018,#65019,#65020),.UNSPECIFIED.,.F.,.F.,(4,3,3,3,3,3,
3,3,3,3,3,3,3,3,4),(-110.906691970891,-110.869061233009,-110.369651047275,
-109.87024086154,-109.370830675806,-108.871420490072,-108.372010304337,
-107.872600118603,-107.373189932869,-106.873779747135,-106.3743695614,-105.874959375666,
-105.375549189932,-104.876139004198,-104.623506663712),.UNSPECIFIED.);
#751=B_SPLINE_CURVE_WITH_KNOTS('',3,(#65021,#65022,#65023,#65024,#65025,
#65026,#65027,#65028,#65029,#65030,#65031,#65032,#65033,#65034,#65035,#65036,
#65037,#65038,#65039,#65040,#65041,#65042,#65043,#65044,#65045,#65046,#65047,
#65048,#65049,#65050,#65051,#65052,#65053,#65054,#65055,#65056,#65057,#65058,
#65059,#65060,#65061,#65062,#65063),.UNSPECIFIED.,.F.,.F.,(4,3,3,3,3,3,
3,3,3,3,3,3,3,3,4),(101.649820008411,101.879677889792,102.379088075526,
102.87849826126,103.377908446995,103.877318632729,104.376728818463,104.876139004198,
105.375549189932,105.874959375666,106.3743695614,106.873779747135,107.373189932869,
107.872600118603,107.933005315591),.UNSPECIFIED.);
#752=B_SPLINE_CURVE_WITH_KNOTS('',3,(#65068,#65069,#65070,#65071,#65072,
#65073,#65074,#65075,#65076,#65077,#65078,#65079,#65080,#65081,#65082,#65083,
#65084,#65085,#65086,#65087,#65088,#65089,#65090,#65091,#65092,#65093,#65094,
#65095,#65096,#65097,#65098,#65099,#65100,#65101,#65102,#65103,#65104,#65105,
#65106,#65107),.UNSPECIFIED.,.F.,.F.,(4,3,3,3,3,3,3,3,3,3,3,3,3,4),(-117.189877278071,
-116.86198346182,-116.362573276086,-115.863163090352,-115.363752904617,
-114.864342718883,-114.364932533149,-113.865522347414,-113.36611216168,
-112.866701975946,-112.367291790212,-111.867881604477,-111.368471418743,
-110.906691970891),.UNSPECIFIED.);
#753=B_SPLINE_CURVE_WITH_KNOTS('',3,(#65108,#65109,#65110,#65111,#65112,
#65113,#65114,#65115,#65116,#65117,#65118,#65119,#65120,#65121,#65122,#65123,
#65124,#65125,#65126,#65127,#65128,#65129,#65130,#65131,#65132,#65133,#65134,
#65135,#65136,#65137,#65138,#65139,#65140,#65141,#65142,#65143,#65144,#65145,
#65146,#65147),.UNSPECIFIED.,.F.,.F.,(4,3,3,3,3,3,3,3,3,3,3,3,3,4),(107.933005315591,
108.372010304337,108.871420490072,109.370830675806,109.87024086154,110.369651047275,
110.869061233009,111.368471418743,111.867881604477,112.367291790212,112.866701975946,
113.36611216168,113.865522347414,114.21619062277),.UNSPECIFIED.);
#754=B_SPLINE_CURVE_WITH_KNOTS('',3,(#65152,#65153,#65154,#65155,#65156,
#65157,#65158,#65159,#65160,#65161,#65162,#65163,#65164,#65165,#65166,#65167,
#65168,#65169,#65170,#65171,#65172,#65173,#65174,#65175,#65176,#65177,#65178,
#65179,#65180,#65181,#65182,#65183,#65184,#65185,#65186,#65187,#65188,#65189,
#65190,#65191,#65192,#65193,#65194),.UNSPECIFIED.,.F.,.F.,(4,3,3,3,3,3,
3,3,3,3,3,3,3,3,4),(-123.473062585251,-123.354315876366,-122.854905690631,
-122.355495504897,-121.856085319163,-121.356675133429,-120.857264947694,
-120.35785476196,-119.858444576226,-119.359034390492,-118.859624204757,
-118.360214019023,-117.860803833289,-117.361393647554,-117.189877278071),
 .UNSPECIFIED.);
#755=B_SPLINE_CURVE_WITH_KNOTS('',3,(#65195,#65196,#65197,#65198,#65199,
#65200,#65201,#65202,#65203,#65204,#65205,#65206,#65207,#65208,#65209,#65210,
#65211,#65212,#65213,#65214,#65215,#65216,#65217,#65218,#65219,#65220,#65221,
#65222,#65223,#65224,#65225,#65226,#65227,#65228,#65229,#65230,#65231,#65232,
#65233,#65234,#65235,#65236,#65237),.UNSPECIFIED.,.F.,.F.,(4,3,3,3,3,3,
3,3,3,3,3,3,3,3,4),(114.21619062277,114.364932533149,114.864342718883,115.363752904617,
115.863163090352,116.362573276086,116.86198346182,117.361393647554,117.860803833289,
118.360214019023,118.859624204757,119.359034390491,119.858444576226,120.35785476196,
120.49937592995),.UNSPECIFIED.);
#756=B_SPLINE_CURVE_WITH_KNOTS('',3,(#65242,#65243,#65244,#65245,#65246,
#65247,#65248,#65249,#65250,#65251,#65252,#65253,#65254,#65255,#65256,#65257,
#65258,#65259,#65260,#65261,#65262,#65263,#65264,#65265,#65266,#65267,#65268,
#65269,#65270,#65271,#65272,#65273,#65274,#65275,#65276,#65277,#65278,#65279,
#65280,#65281),.UNSPECIFIED.,.F.,.F.,(4,3,3,3,3,3,3,3,3,3,3,3,3,4),(-129.75624789243,
-129.347238105177,-128.847827919443,-128.348417733708,-127.849007547974,
-127.34959736224,-126.850187176506,-126.350776990771,-125.851366805037,
-125.351956619303,-124.852546433569,-124.353136247834,-123.8537260621,-123.473062585251),
 .UNSPECIFIED.);
#757=B_SPLINE_CURVE_WITH_KNOTS('',3,(#65282,#65283,#65284,#65285,#65286,
#65287,#65288,#65289,#65290,#65291,#65292,#65293,#65294,#65295,#65296,#65297,
#65298,#65299,#65300,#65301,#65302,#65303,#65304,#65305,#65306,#65307,#65308,
#65309,#65310,#65311,#65312,#65313,#65314,#65315,#65316,#65317,#65318,#65319,
#65320,#65321),.UNSPECIFIED.,.F.,.F.,(4,3,3,3,3,3,3,3,3,3,3,3,3,4),(120.49937592995,
120.857264947694,121.356675133429,121.856085319163,122.355495504897,122.854905690631,
123.354315876366,123.8537260621,124.353136247834,124.852546433568,125.351956619303,
125.851366805037,126.350776990771,126.782561237129),.UNSPECIFIED.);
#758=B_SPLINE_CURVE_WITH_KNOTS('',3,(#65326,#65327,#65328,#65329,#65330,
#65331,#65332,#65333,#65334,#65335,#65336,#65337,#65338,#65339,#65340,#65341,
#65342,#65343,#65344,#65345,#65346,#65347,#65348,#65349,#65350,#65351,#65352,
#65353,#65354,#65355,#65356,#65357,#65358,#65359,#65360,#65361,#65362,#65363,
#65364,#65365,#65366,#65367,#65368),.UNSPECIFIED.,.F.,.F.,(4,3,3,3,3,3,
3,3,3,3,3,3,3,3,4),(-136.03943319961,-135.839570519723,-135.340160333988,
-134.840750148254,-134.34133996252,-133.841929776785,-133.342519591051,
-132.843109405317,-132.343699219583,-131.844289033848,-131.344878848114,
-130.84546866238,-130.346058476646,-129.846648290911,-129.75624789243),
 .UNSPECIFIED.);
#759=B_SPLINE_CURVE_WITH_KNOTS('',3,(#65369,#65370,#65371,#65372,#65373,
#65374,#65375,#65376,#65377,#65378,#65379,#65380,#65381,#65382,#65383,#65384,
#65385,#65386,#65387,#65388,#65389,#65390,#65391,#65392,#65393,#65394,#65395,
#65396,#65397,#65398,#65399,#65400,#65401,#65402,#65403,#65404,#65405,#65406,
#65407,#65408,#65409,#65410,#65411),.UNSPECIFIED.,.F.,.F.,(4,3,3,3,3,3,
3,3,3,3,3,3,3,3,4),(126.782561237129,126.850187176506,127.34959736224,127.849007547974,
128.348417733708,128.847827919443,129.347238105177,129.846648290911,130.346058476646,
130.84546866238,131.344878848114,131.844289033848,132.343699219583,132.843109405317,
133.065746544309),.UNSPECIFIED.);
#760=B_SPLINE_CURVE_WITH_KNOTS('',3,(#65416,#65417,#65418,#65419,#65420,
#65421,#65422,#65423,#65424,#65425,#65426,#65427,#65428,#65429,#65430,#65431,
#65432,#65433,#65434,#65435,#65436,#65437,#65438,#65439,#65440,#65441,#65442,
#65443,#65444,#65445,#65446,#65447,#65448,#65449,#65450,#65451,#65452,#65453,
#65454,#65455),.UNSPECIFIED.,.F.,.F.,(4,3,3,3,3,3,3,3,3,3,3,3,3,4),(-142.322618506789,
-141.832492748534,-141.3330825628,-140.833672377065,-140.334262191331,-139.834852005597,
-139.335441819862,-138.836031634128,-138.336621448394,-137.83721126266,
-137.337801076925,-136.838390891191,-136.338980705457,-136.03943319961),
 .UNSPECIFIED.);
#761=B_SPLINE_CURVE_WITH_KNOTS('',3,(#65456,#65457,#65458,#65459,#65460,
#65461,#65462,#65463,#65464,#65465,#65466,#65467,#65468,#65469,#65470,#65471,
#65472,#65473,#65474,#65475,#65476,#65477,#65478,#65479,#65480,#65481,#65482,
#65483,#65484,#65485,#65486,#65487,#65488,#65489,#65490,#65491,#65492,#65493,
#65494,#65495,#65496,#65497,#65498),.UNSPECIFIED.,.F.,.F.,(4,3,3,3,3,3,
3,3,3,3,3,3,3,3,4),(133.065746544309,133.342519591051,133.841929776785,
134.34133996252,134.840750148254,135.340160333988,135.839570519723,136.338980705457,
136.838390891191,137.337801076925,137.83721126266,138.336621448394,138.836031634128,
139.335441819862,139.348931851488),.UNSPECIFIED.);
#762=B_SPLINE_CURVE_WITH_KNOTS('',3,(#65504,#65505,#65506,#65507,#65508,
#65509,#65510,#65511,#65512,#65513,#65514,#65515,#65516,#65517,#65518),
 .UNSPECIFIED.,.F.,.F.,(4,1,1,1,1,1,1,1,1,1,1,1,4),(147.65485471872,147.954402224568,
148.453812410302,148.953222596036,149.45263278177,149.952042967505,150.451453153239,
150.950863338973,151.450273524707,151.949683710442,152.449093896176,152.94850408191,
153.375750821795),.UNSPECIFIED.);
#763=B_SPLINE_CURVE_WITH_KNOTS('',3,(#65521,#65522,#65523,#65524,#65525,
#65526,#65527,#65528,#65529,#65530,#65531,#65532),.UNSPECIFIED.,.F.,.F.,
(4,1,1,1,1,1,1,1,1,4),(147.65485471872,148.140774872828,148.640185058563,
149.139595244297,149.639005430031,150.138415615766,150.6378258015,151.137235987234,
151.636646172968,152.136056358703),.UNSPECIFIED.);
#764=B_SPLINE_CURVE_WITH_KNOTS('',3,(#65537,#65538,#65539,#65540,#65541,
#65542,#65543,#65544,#65545,#65546,#65547,#65548,#65549,#65550,#65551,#65552,
#65553),.UNSPECIFIED.,.F.,.F.,(4,1,1,1,1,1,1,1,1,1,1,1,1,1,4),(141.371669411541,
141.462069810022,141.961479995756,142.46089018149,142.960300367225,143.459710552959,
143.959120738693,144.458530924428,144.957941110162,145.457351295896,145.95676148163,
146.456171667365,146.955581853099,147.454992038833,147.65485471872),
 .UNSPECIFIED.);
#765=B_SPLINE_CURVE_WITH_KNOTS('',3,(#65554,#65555,#65556,#65557,#65558,
#65559,#65560,#65561,#65562,#65563,#65564,#65565,#65566,#65567,#65568,#65569,
#65570),.UNSPECIFIED.,.F.,.F.,(4,1,1,1,1,1,1,1,1,1,1,1,1,1,4),(141.371669411541,
141.648442458283,142.147852644017,142.647262829751,143.146673015486,143.64608320122,
144.145493386954,144.644903572689,145.144313758423,145.643723944157,146.143134129891,
146.642544315626,147.14195450136,147.641364687094,147.65485471872),
 .UNSPECIFIED.);
#766=B_SPLINE_CURVE_WITH_KNOTS('',3,(#65575,#65576,#65577,#65578,#65579,
#65580,#65581,#65582,#65583,#65584,#65585,#65586,#65587,#65588,#65589,#65590),
 .UNSPECIFIED.,.F.,.F.,(4,1,1,1,1,1,1,1,1,1,1,1,1,4),(135.088484104361,
135.469147581211,135.968557766945,136.467967952679,136.967378138413,137.466788324148,
137.966198509882,138.465608695616,138.965018881351,139.464429067085,139.963839252819,
140.463249438553,140.962659624288,141.371669411541),.UNSPECIFIED.);
#767=B_SPLINE_CURVE_WITH_KNOTS('',3,(#65591,#65592,#65593,#65594,#65595,
#65596,#65597,#65598,#65599,#65600,#65601,#65602,#65603,#65604,#65605,#65606,
#65607),.UNSPECIFIED.,.F.,.F.,(4,1,1,1,1,1,1,1,1,1,1,1,1,1,4),(135.088484104361,
135.156110043737,135.655520229472,136.154930415206,136.65434060094,137.153750786674,
137.653160972409,138.152571158143,138.651981343877,139.151391529612,139.650801715346,
140.15021190108,140.649622086814,141.149032272549,141.371669411541),
 .UNSPECIFIED.);
#768=B_SPLINE_CURVE_WITH_KNOTS('',3,(#65612,#65613,#65614,#65615,#65616,
#65617,#65618,#65619,#65620,#65621,#65622,#65623,#65624,#65625,#65626,#65627,
#65628),.UNSPECIFIED.,.F.,.F.,(4,1,1,1,1,1,1,1,1,1,1,1,1,1,4),(128.805298797182,
128.976815166665,129.476225352399,129.975635538134,130.475045723868,130.974455909602,
131.473866095336,131.973276281071,132.472686466805,132.972096652539,133.471506838274,
133.970917024008,134.470327209742,134.969737395476,135.088484104361),
 .UNSPECIFIED.);
#769=B_SPLINE_CURVE_WITH_KNOTS('',3,(#65629,#65630,#65631,#65632,#65633,
#65634,#65635,#65636,#65637,#65638,#65639,#65640,#65641,#65642,#65643,#65644),
 .UNSPECIFIED.,.F.,.F.,(4,1,1,1,1,1,1,1,1,1,1,1,1,4),(128.805298797182,
129.163187814926,129.66259800066,130.162008186395,130.661418372129,131.160828557863,
131.660238743597,132.159648929332,132.659059115066,133.1584693008,133.657879486535,
134.157289672269,134.656699858003,135.088484104361),.UNSPECIFIED.);
#770=B_SPLINE_CURVE_WITH_KNOTS('',3,(#65649,#65650,#65651,#65652,#65653,
#65654,#65655,#65656,#65657,#65658,#65659,#65660,#65661,#65662,#65663,#65664),
 .UNSPECIFIED.,.F.,.F.,(4,1,1,1,1,1,1,1,1,1,1,1,1,4),(122.522113490002,
122.983892937854,123.483303123588,123.982713309322,124.482123495057,124.981533680791,
125.480943866525,125.980354052259,126.479764237994,126.979174423728,127.478584609462,
127.977994795197,128.477404980931,128.805298797182),.UNSPECIFIED.);
#771=B_SPLINE_CURVE_WITH_KNOTS('',3,(#65665,#65666,#65667,#65668,#65669,
#65670,#65671,#65672,#65673,#65674,#65675,#65676,#65677,#65678,#65679,#65680,
#65681),.UNSPECIFIED.,.F.,.F.,(4,1,1,1,1,1,1,1,1,1,1,1,1,1,4),(122.522113490002,
122.67085540038,123.170265586115,123.669675771849,124.169085957583,124.668496143318,
125.167906329052,125.667316514786,126.16672670052,126.666136886255,127.165547071989,
127.664957257723,128.164367443458,128.663777629192,128.805298797182),
 .UNSPECIFIED.);
#772=B_SPLINE_CURVE_WITH_KNOTS('',3,(#65686,#65687,#65688,#65689,#65690,
#65691,#65692,#65693,#65694,#65695,#65696,#65697,#65698,#65699,#65700,#65701,
#65702),.UNSPECIFIED.,.F.,.F.,(4,1,1,1,1,1,1,1,1,1,1,1,1,1,4),(116.238928182822,
116.491560523308,116.990970709043,117.490380894777,117.989791080511,118.489201266245,
118.98861145198,119.488021637714,119.987431823448,120.486842009182,120.986252194917,
121.485662380651,121.985072566385,122.48448275212,122.522113490002),
 .UNSPECIFIED.);
#773=B_SPLINE_CURVE_WITH_KNOTS('',3,(#65703,#65704,#65705,#65706,#65707,
#65708,#65709,#65710,#65711,#65712,#65713,#65714,#65715,#65716,#65717,#65718),
 .UNSPECIFIED.,.F.,.F.,(4,1,1,1,1,1,1,1,1,1,1,1,1,4),(116.238928182822,
116.677933171569,117.177343357303,117.676753543038,118.176163728772,118.675573914506,
119.174984100241,119.674394285975,120.173804471709,120.673214657443,121.172624843178,
121.672035028912,122.171445214646,122.522113490002),.UNSPECIFIED.);
#774=B_SPLINE_CURVE_WITH_KNOTS('',3,(#65723,#65724,#65725,#65726,#65727,
#65728,#65729,#65730,#65731,#65732,#65733,#65734,#65735,#65736,#65737,#65738,
#65739),.UNSPECIFIED.,.F.,.F.,(4,1,1,1,1,1,1,1,1,1,1,1,1,1,4),(109.955742875643,
109.999228108763,110.498638294497,110.998048480231,111.497458665965,111.9968688517,
112.496279037434,112.995689223168,113.495099408903,113.994509594637,114.493919780371,
114.993329966105,115.49274015184,115.992150337574,116.238928182822),
 .UNSPECIFIED.);
#775=B_SPLINE_CURVE_WITH_KNOTS('',3,(#65740,#65741,#65742,#65743,#65744,
#65745,#65746,#65747,#65748,#65749,#65750,#65751,#65752,#65753,#65754,#65755,
#65756),.UNSPECIFIED.,.F.,.F.,(4,1,1,1,1,1,1,1,1,1,1,1,1,1,4),(109.955742875643,
110.185600757024,110.685010942758,111.184421128492,111.683831314226,112.183241499961,
112.682651685695,113.182061871429,113.681472057164,114.180882242898,114.680292428632,
115.179702614366,115.679112800101,116.178522985835,116.238928182822),
 .UNSPECIFIED.);
#776=B_SPLINE_CURVE_WITH_KNOTS('',3,(#65761,#65762,#65763,#65764,#65765,
#65766,#65767,#65768,#65769,#65770,#65771,#65772,#65773,#65774,#65775,#65776),
 .UNSPECIFIED.,.F.,.F.,(4,1,1,1,1,1,1,1,1,1,1,1,1,4),(103.672557568463,
104.006305879951,104.505716065686,105.00512625142,105.504536437154,106.003946622888,
106.503356808623,107.002766994357,107.502177180091,108.001587365826,108.50099755156,
109.000407737294,109.499817923028,109.955742875643),.UNSPECIFIED.);
#777=B_SPLINE_CURVE_WITH_KNOTS('',3,(#65777,#65778,#65779,#65780,#65781,
#65782,#65783,#65784,#65785,#65786,#65787,#65788,#65789,#65790,#65791,#65792,
#65793),.UNSPECIFIED.,.F.,.F.,(4,1,1,1,1,1,1,1,1,1,1,1,1,1,4),(103.672557568463,
103.693268342478,104.192678528212,104.692088713947,105.191498899681,105.690909085415,
106.190319271149,106.689729456884,107.189139642618,107.688549828352,108.187960014087,
108.687370199821,109.186780385555,109.686190571289,109.955742875643),
 .UNSPECIFIED.);
#778=B_SPLINE_CURVE_WITH_KNOTS('',3,(#65798,#65799,#65800,#65801,#65802,
#65803,#65804,#65805,#65806,#65807,#65808,#65809,#65810,#65811,#65812,#65813,
#65814),.UNSPECIFIED.,.F.,.F.,(4,1,1,1,1,1,1,1,1,1,1,1,1,1,4),(97.3893722612836,
97.5139734654058,98.0133836511401,98.5127938368744,99.0122040226086,99.5116142083429,
100.011024394077,100.510434579811,101.009844765546,101.50925495128,102.008665137014,
102.508075322749,103.007485508483,103.506895694217,103.672557568463),
 .UNSPECIFIED.);
#779=B_SPLINE_CURVE_WITH_KNOTS('',3,(#65815,#65816,#65817,#65818,#65819,
#65820,#65821,#65822,#65823,#65824,#65825,#65826,#65827,#65828,#65829,#65830),
 .UNSPECIFIED.,.F.,.F.,(4,1,1,1,1,1,1,1,1,1,1,1,1,4),(97.3893722612836,
97.7003461136668,98.1997562994011,98.6991664851353,99.1985766708696,99.6979868566039,
100.197397042338,100.696807228072,101.196217413807,101.695627599541,102.195037785275,
102.69444797101,103.193858156744,103.672557568463),.UNSPECIFIED.);
#780=B_SPLINE_CURVE_WITH_KNOTS('',3,(#65835,#65836,#65837,#65838,#65839,
#65840,#65841,#65842,#65843,#65844,#65845,#65846,#65847,#65848,#65849,#65850),
 .UNSPECIFIED.,.F.,.F.,(4,1,1,1,1,1,1,1,1,1,1,1,1,4),(91.106186954104,91.5210512365945,
92.0204614223288,92.5198716080631,93.0192817937973,93.5186919795316,94.0181021652659,
94.5175123510002,95.0169225367344,95.5163327224687,96.015742908203,96.5151530939373,
97.0145632796715,97.3893722612836),.UNSPECIFIED.);
#781=B_SPLINE_CURVE_WITH_KNOTS('',3,(#65851,#65852,#65853,#65854,#65855,
#65856,#65857,#65858,#65859,#65860,#65861,#65862,#65863,#65864,#65865,#65866,
#65867),.UNSPECIFIED.,.F.,.F.,(4,1,1,1,1,1,1,1,1,1,1,1,1,1,4),(91.106186954104,
91.2080136991212,91.7074238848555,92.2068340705898,92.7062442563241,93.2056544420583,
93.7050646277926,94.2044748135269,94.7038849992611,95.2032951849954,95.7027053707297,
96.202115556464,96.7015257421982,97.2009359279325,97.3893722612836),
 .UNSPECIFIED.);
#782=B_SPLINE_CURVE_WITH_KNOTS('',3,(#65872,#65873,#65874,#65875,#65876,
#65877,#65878,#65879,#65880,#65881,#65882,#65883,#65884,#65885,#65886,#65887,
#65888),.UNSPECIFIED.,.F.,.F.,(4,1,1,1,1,1,1,1,1,1,1,1,1,1,4),(84.8230016469244,
85.028718822049,85.5281290077832,86.0275391935175,86.5269493792518,87.0263595649861,
87.5257697507203,88.0251799364546,88.5245901221889,89.0240003079231,89.5234104936574,
90.0228206793917,90.522230865126,91.0216410508603,91.106186954104),
 .UNSPECIFIED.);
#783=B_SPLINE_CURVE_WITH_KNOTS('',3,(#65889,#65890,#65891,#65892,#65893,
#65894,#65895,#65896,#65897,#65898,#65899,#65900,#65901,#65902,#65903,#65904),
 .UNSPECIFIED.,.F.,.F.,(4,1,1,1,1,1,1,1,1,1,1,1,1,4),(84.8230016469244,
85.2150914703099,85.7145016560442,86.2139118417785,86.7133220275128,87.212732213247,
87.7121423989813,88.2115525847156,88.7109627704499,89.2103729561841,89.7097831419184,
90.2091933276527,90.7086035133869,91.106186954104),.UNSPECIFIED.);
#784=B_SPLINE_CURVE_WITH_KNOTS('',3,(#65909,#65910,#65911,#65912,#65913,
#65914,#65915,#65916,#65917,#65918,#65919,#65920,#65921,#65922,#65923,#65924),
 .UNSPECIFIED.,.F.,.F.,(4,1,1,1,1,1,1,1,1,1,1,1,1,4),(78.5398163397448,
79.0357965932377,79.5352067789719,80.0346169647062,80.5340271504405,81.0334373361748,
81.532847521909,82.0322577076433,82.5316678933776,83.0310780791119,83.5304882648461,
84.0298984505804,84.5293086363147,84.8230016469244),.UNSPECIFIED.);
#785=B_SPLINE_CURVE_WITH_KNOTS('',3,(#65925,#65926,#65927,#65928,#65929,
#65930,#65931,#65932,#65933,#65934,#65935,#65936,#65937,#65938,#65939,#65940,
#65941),.UNSPECIFIED.,.F.,.F.,(4,1,1,1,1,1,1,1,1,1,1,1,1,1,4),(78.5398163397448,
78.7227590557644,79.2221692414986,79.7215794272329,80.2209896129672,80.7203997987015,
81.2198099844358,81.71922017017,82.2186303559043,82.7180405416386,83.2174507273728,
83.7168609131071,84.2162710988414,84.7156812845757,84.8230016469244),
 .UNSPECIFIED.);
#786=B_SPLINE_CURVE_WITH_KNOTS('',3,(#65946,#65947,#65948,#65949,#65950,
#65951,#65952,#65953,#65954,#65955,#65956,#65957,#65958,#65959,#65960,#65961,
#65962),.UNSPECIFIED.,.F.,.F.,(4,1,1,1,1,1,1,1,1,1,1,1,1,1,4),(72.2566310325653,
72.5434641786921,73.0428743644264,73.5422845501607,74.0416947358949,74.5411049216292,
75.0405151073635,75.5399252930978,76.039335478832,76.5387456645663,77.0381558503006,
77.5375660360349,78.0369762217691,78.5363864075034,78.5398163397448),
 .UNSPECIFIED.);
#787=B_SPLINE_CURVE_WITH_KNOTS('',3,(#65963,#65964,#65965,#65966,#65967,
#65968,#65969,#65970,#65971,#65972,#65973,#65974,#65975,#65976,#65977,#65978),
 .UNSPECIFIED.,.F.,.F.,(4,1,1,1,1,1,1,1,1,1,1,1,1,4),(72.2566310325653,
72.7298368269531,73.2292470126874,73.7286571984216,74.2280673841559,74.7274775698902,
75.2268877556245,75.7262979413587,76.225708127093,76.7251183128273,77.2245284985616,
77.7239386842958,78.2233488700301,78.5398163397448),.UNSPECIFIED.);
#788=B_SPLINE_CURVE_WITH_KNOTS('',3,(#65983,#65984,#65985,#65986,#65987,
#65988,#65989,#65990,#65991,#65992,#65993,#65994,#65995,#65996,#65997,#65998,
#65999),.UNSPECIFIED.,.F.,.F.,(4,1,1,1,1,1,1,1,1,1,1,1,1,1,4),(65.9734457253856,
66.0511317641465,66.5505419498808,67.0499521356151,67.5493623213494,68.0487725070836,
68.5481826928179,69.0475928785522,69.5470030642865,70.0464132500207,70.545823435755,
71.0452336214893,71.5446438072236,72.0440539929578,72.2566310325653),
 .UNSPECIFIED.);
#789=B_SPLINE_CURVE_WITH_KNOTS('',3,(#66000,#66001,#66002,#66003,#66004,
#66005,#66006,#66007,#66008,#66009,#66010,#66011,#66012,#66013,#66014,#66015,
#66016),.UNSPECIFIED.,.F.,.F.,(4,1,1,1,1,1,1,1,1,1,1,1,1,1,4),(65.9734457253856,
66.2375044124075,66.7369145981418,67.2363247838761,67.7357349696103,68.2351451553446,
68.7345553410789,69.2339655268132,69.7333757125475,70.2327858982817,70.732196084016,
71.2316062697503,71.7310164554845,72.2304266412188,72.2566310325653),
 .UNSPECIFIED.);
#790=B_SPLINE_CURVE_WITH_KNOTS('',3,(#66021,#66022,#66023,#66024,#66025,
#66026,#66027,#66028,#66029,#66030,#66031,#66032,#66033,#66034,#66035,#66036),
 .UNSPECIFIED.,.F.,.F.,(4,1,1,1,1,1,1,1,1,1,1,1,1,4),(59.6902604182061,
60.0582095353353,60.5576197210695,61.0570299068038,61.5564400925381,62.0558502782724,
62.5552604640066,63.0546706497409,63.5540808354752,64.0534910212095,64.5529012069437,
65.052311392678,65.5517215784123,65.9734457253856),.UNSPECIFIED.);
#791=B_SPLINE_CURVE_WITH_KNOTS('',3,(#66037,#66038,#66039,#66040,#66041,
#66042,#66043,#66044,#66045,#66046,#66047,#66048,#66049,#66050,#66051,#66052,
#66053),.UNSPECIFIED.,.F.,.F.,(4,1,1,1,1,1,1,1,1,1,1,1,1,1,4),(59.6902604182061,
59.745171997862,60.2445821835963,60.7439923693305,61.2434025550648,61.7428127407991,
62.2422229265333,62.7416331122676,63.2410432980019,63.7404534837362,64.2398636694704,
64.7392738552047,65.238684040939,65.7380942266733,65.9734457253856),
 .UNSPECIFIED.);
#792=B_SPLINE_CURVE_WITH_KNOTS('',3,(#66058,#66059,#66060,#66061,#66062,
#66063,#66064,#66065,#66066,#66067,#66068,#66069,#66070,#66071,#66072,#66073,
#66074),.UNSPECIFIED.,.F.,.F.,(4,1,1,1,1,1,1,1,1,1,1,1,1,1,4),(53.4070751110265,
53.5658771207897,54.065287306524,54.5646974922582,55.0641076779925,55.5635178637268,
56.0629280494611,56.5623382351953,57.0617484209296,57.5611586066639,58.0605687923982,
58.5599789781324,59.0593891638667,59.558799349601,59.6902604182061),
 .UNSPECIFIED.);
#793=B_SPLINE_CURVE_WITH_KNOTS('',3,(#66075,#66076,#66077,#66078,#66079,
#66080,#66081,#66082,#66083,#66084,#66085,#66086,#66087,#66088,#66089,#66090),
 .UNSPECIFIED.,.F.,.F.,(4,1,1,1,1,1,1,1,1,1,1,1,1,4),(53.4070751110265,
53.7522497690507,54.251659954785,54.7510701405192,55.2504803262535,55.7498905119878,
56.2493006977221,56.7487108834563,57.2481210691906,57.7475312549249,58.2469414406592,
58.7463516263934,59.2457618121277,59.6902604182061),.UNSPECIFIED.);
#794=B_SPLINE_CURVE_WITH_KNOTS('',3,(#66095,#66096,#66097,#66098,#66099,
#66100,#66101,#66102,#66103,#66104,#66105,#66106,#66107,#66108,#66109,#66110),
 .UNSPECIFIED.,.F.,.F.,(4,1,1,1,1,1,1,1,1,1,1,1,1,4),(47.1238898038469,
47.5729548919784,48.0723650777127,48.571775263447,49.0711854491812,49.5705956349155,
50.0700058206498,50.5694160063841,51.0688261921183,51.5682363778526,52.0676465635869,
52.5670567493211,53.0664669350554,53.4070751110265),.UNSPECIFIED.);
#795=B_SPLINE_CURVE_WITH_KNOTS('',3,(#66111,#66112,#66113,#66114,#66115,
#66116,#66117,#66118,#66119,#66120,#66121,#66122,#66123,#66124,#66125,#66126,
#66127),.UNSPECIFIED.,.F.,.F.,(4,1,1,1,1,1,1,1,1,1,1,1,1,1,4),(47.1238898038469,
47.2599173545051,47.7593275402394,48.2587377259737,48.758147911708,49.2575580974422,
49.7569682831765,50.2563784689108,50.755788654645,51.2551988403793,51.7546090261136,
52.2540192118479,52.7534293975821,53.2528395833164,53.4070751110265),
 .UNSPECIFIED.);
#796=B_SPLINE_CURVE_WITH_KNOTS('',3,(#66132,#66133,#66134,#66135,#66136,
#66137,#66138,#66139,#66140,#66141,#66142,#66143,#66144,#66145,#66146,#66147,
#66148),.UNSPECIFIED.,.F.,.F.,(4,1,1,1,1,1,1,1,1,1,1,1,1,1,4),(40.8407044966673,
41.0806224774328,41.5800326631671,42.0794428489014,42.5788530346357,43.0782632203699,
43.5776734061042,44.0770835918385,44.5764937775728,45.075903963307,45.5753141490413,
46.0747243347756,46.5741345205099,47.0735447062441,47.1238898038469),
 .UNSPECIFIED.);
#797=B_SPLINE_CURVE_WITH_KNOTS('',3,(#66149,#66150,#66151,#66152,#66153,
#66154,#66155,#66156,#66157,#66158,#66159,#66160,#66161,#66162,#66163,#66164),
 .UNSPECIFIED.,.F.,.F.,(4,1,1,1,1,1,1,1,1,1,1,1,1,4),(40.8407044966673,
41.2669951256938,41.7664053114281,42.2658154971624,42.7652256828967,43.2646358686309,
43.7640460543652,44.2634562400995,44.7628664258338,45.262276611568,45.7616867973023,
46.2610969830366,46.7605071687709,47.1238898038469),.UNSPECIFIED.);
#798=B_SPLINE_CURVE_WITH_KNOTS('',3,(#66169,#66170,#66171,#66172,#66173,
#66174,#66175,#66176,#66177,#66178,#66179,#66180,#66181,#66182,#66183,#66184,
#66185),.UNSPECIFIED.,.F.,.F.,(4,1,1,1,1,1,1,1,1,1,1,1,1,1,4),(34.5575191894877,
34.5882900628873,35.0877002486216,35.5871104343558,36.0865206200901,36.5859308058244,
37.0853409915587,37.5847511772929,38.0841613630272,38.5835715487615,39.0829817344957,
39.58239192023,40.0818021059643,40.5812122916986,40.8407044966673),
 .UNSPECIFIED.);
#799=B_SPLINE_CURVE_WITH_KNOTS('',3,(#66186,#66187,#66188,#66189,#66190,
#66191,#66192,#66193,#66194,#66195,#66196,#66197,#66198,#66199,#66200,#66201,
#66202),.UNSPECIFIED.,.F.,.F.,(4,1,1,1,1,1,1,1,1,1,1,1,1,1,4),(34.5575191894877,
34.7746627111483,35.2740728968826,35.7734830826168,36.2728932683511,36.7723034540854,
37.2717136398197,37.7711238255539,38.2705340112882,38.7699441970225,39.2693543827567,
39.768764568491,40.2681747542253,40.7675849399596,40.8407044966673),
 .UNSPECIFIED.);
#800=B_SPLINE_CURVE_WITH_KNOTS('',3,(#66207,#66208,#66209,#66210,#66211,
#66212,#66213,#66214,#66215,#66216,#66217,#66218,#66219,#66220,#66221,#66222),
 .UNSPECIFIED.,.F.,.F.,(4,1,1,1,1,1,1,1,1,1,1,1,1,4),(28.2743338823081,
28.595367834076,29.0947780198103,29.5941882055445,30.0935983912788,30.5930085770131,
31.0924187627474,31.5918289484816,32.0912391342159,32.5906493199502,33.0900595056845,
33.5894696914187,34.088879877153,34.5575191894877),.UNSPECIFIED.);
#801=B_SPLINE_CURVE_WITH_KNOTS('',3,(#66223,#66224,#66225,#66226,#66227,
#66228,#66229,#66230,#66231,#66232,#66233,#66234,#66235,#66236,#66237,#66238,
#66239),.UNSPECIFIED.,.F.,.F.,(4,1,1,1,1,1,1,1,1,1,1,1,1,1,4),(28.2743338823081,
28.2823302966027,28.781740482337,29.2811506680713,29.7805608538055,30.2799710395398,
30.7793812252741,31.2787914110084,31.7782015967426,32.2776117824769,32.7770219682112,
33.2764321539455,33.7758423396797,34.275252525414,34.5575191894877),
 .UNSPECIFIED.);
#802=B_SPLINE_CURVE_WITH_KNOTS('',3,(#66244,#66245,#66246,#66247,#66248,
#66249,#66250,#66251,#66252,#66253,#66254,#66255,#66256,#66257,#66258,#66259,
#66260),.UNSPECIFIED.,.F.,.F.,(4,1,1,1,1,1,1,1,1,1,1,1,1,1,4),(21.9911485751285,
22.1030354195304,22.6024456052647,23.101855790999,23.6012659767333,24.1006761624675,
24.6000863482018,25.0994965339361,25.5989067196703,26.0983169054046,26.5977270911389,
27.0971372768732,27.5965474626074,28.0959576483417,28.2743338823081),
 .UNSPECIFIED.);
#803=B_SPLINE_CURVE_WITH_KNOTS('',3,(#66261,#66262,#66263,#66264,#66265,
#66266,#66267,#66268,#66269,#66270,#66271,#66272,#66273,#66274,#66275,#66276),
 .UNSPECIFIED.,.F.,.F.,(4,1,1,1,1,1,1,1,1,1,1,1,1,4),(21.9911485751285,
22.2894080677914,22.7888182535257,23.28822843926,23.7876386249943,24.2870488107285,
24.7864589964628,25.2858691821971,25.7852793679313,26.2846895536656,26.7840997393999,
27.2835099251342,27.7829201108684,28.2743338823081),.UNSPECIFIED.);
#804=B_SPLINE_CURVE_WITH_KNOTS('',3,(#66281,#66282,#66283,#66284,#66285,
#66286,#66287,#66288,#66289,#66290,#66291,#66292,#66293,#66294,#66295,#66296),
 .UNSPECIFIED.,.F.,.F.,(4,1,1,1,1,1,1,1,1,1,1,1,1,4),(15.7079632679489,
16.1101131907191,16.6095233764534,17.1089335621877,17.608343747922,18.1077539336562,
18.6071641193905,19.1065743051248,19.6059844908591,20.1053946765933,20.6048048623276,
21.1042150480619,21.6036252337962,21.9911485751285),.UNSPECIFIED.);
#805=B_SPLINE_CURVE_WITH_KNOTS('',3,(#66297,#66298,#66299,#66300,#66301,
#66302,#66303,#66304,#66305,#66306,#66307,#66308,#66309,#66310,#66311,#66312,
#66313),.UNSPECIFIED.,.F.,.F.,(4,1,1,1,1,1,1,1,1,1,1,1,1,1,4),(15.7079632679489,
15.7970756532459,16.2964858389801,16.7958960247144,17.2953062104487,17.794716396183,
18.2941265819172,18.7935367676515,19.2929469533858,19.7923571391201,20.2917673248543,
20.7911775105886,21.2905876963229,21.7899978820572,21.9911485751285),
 .UNSPECIFIED.);
#806=B_SPLINE_CURVE_WITH_KNOTS('',3,(#67479,#67480,#67481,#67482,#67483,
#67484,#67485,#67486,#67487,#67488,#67489,#67490,#67491,#67492,#67493,#67494,
#67495,#67496,#67497,#67498,#67499,#67500,#67501,#67502,#67503,#67504,#67505,
#67506,#67507,#67508,#67509,#67510,#67511,#67512,#67513,#67514,#67515,#67516,
#67517,#67518,#67519,#67520,#67521,#67522,#67523,#67524,#67525,#67526,#67527,
#67528,#67529,#67530,#67531,#67532,#67533,#67534,#67535,#67536,#67537,#67538,
#67539,#67540,#67541,#67542,#67543,#67544,#67545,#67546,#67547,#67548),
 .UNSPECIFIED.,.F.,.F.,(4,3,3,3,3,3,3,3,3,3,3,3,3,3,3,3,3,3,3,3,3,3,3,4),
(-1.12653966532777,-1.08393007696725,-1.01186793859792,-0.979479106883256,
-0.956116981122905,-0.875899252306419,-0.82547163350704,-0.8061866417097,
-0.795681523489932,-0.710458657553849,-0.62620775347041,-0.607006915743544,
-0.586923413382426,-0.518700915770662,-0.451188877692257,-0.412581476881461,
-0.394181574045281,-0.313650449653669,-0.253407622478392,-0.210833150163061,
-0.193782661020163,-0.115040611558608,-0.0378484817361047,0.),
 .UNSPECIFIED.);
#807=B_SPLINE_CURVE_WITH_KNOTS('',3,(#67549,#67550,#67551,#67552,#67553,
#67554,#67555,#67556,#67557,#67558,#67559,#67560,#67561,#67562,#67563,#67564),
 .UNSPECIFIED.,.F.,.F.,(4,3,3,3,3,4),(139.348931851488,139.834852005597,
140.334262191331,140.833672377065,141.3330825628,141.760329302685),
 .UNSPECIFIED.);
#808=B_SPLINE_CURVE_WITH_KNOTS('',3,(#67566,#67567,#67568,#67569,#67570,
#67571,#67572,#67573,#67574,#67575,#67576,#67577,#67578,#67579,#67580,#67581,
#67582,#67583,#67584,#67585,#67586,#67587,#67588,#67589,#67590,#67591,#67592,
#67593,#67594,#67595,#67596,#67597,#67598,#67599,#67600,#67601,#67602,#67603,
#67604,#67605,#67606,#67607,#67608,#67609,#67610,#67611,#67612,#67613,#67614,
#67615,#67616,#67617,#67618,#67619,#67620,#67621,#67622,#67623,#67624,#67625,
#67626,#67627,#67628,#67629,#67630,#67631,#67632,#67633,#67634,#67635,#67636,
#67637,#67638),.UNSPECIFIED.,.F.,.F.,(4,3,3,3,3,3,3,3,3,3,3,3,3,3,3,3,3,
3,3,3,3,3,3,3,4),(-1.13094109509784,-1.09499881239214,-1.03107752332609,
-1.00370431748061,-0.983750389109266,-0.911532022618602,-0.881102070346245,
-0.860943270171285,-0.839313656127939,-0.758239088642718,-0.705009903366053,
-0.662463525867964,-0.643629991304747,-0.571319967865515,-0.50135866204052,
-0.457365025783336,-0.433111592060782,-0.34693419716568,-0.291474744565535,
-0.247356571073232,-0.228207082344636,-0.208365914759508,-0.120835935788132,
-0.0326428575257076,0.),.UNSPECIFIED.);
#809=B_SPLINE_CURVE_WITH_KNOTS('',3,(#67639,#67640,#67641,#67642,#67643,
#67644,#67645,#67646,#67647,#67648,#67649,#67650,#67651,#67652),
 .UNSPECIFIED.,.F.,.F.,(4,1,1,1,1,1,1,1,1,1,1,4),(10.3757270560179,10.8029737959031,
11.3023839816374,11.8017941673717,12.301204353106,12.8006145388402,13.3000247245745,
13.7994349103088,14.298845096043,14.7982552817773,15.2976654675116,15.7079632679489),
 .UNSPECIFIED.);
#810=B_SPLINE_CURVE_WITH_KNOTS('',3,(#67658,#67659,#67660,#67661,#67662,
#67663,#67664,#67665,#67666,#67667,#67668,#67669,#67670,#67671,#67672,#67673,
#67674,#67675,#67676,#67677,#67678,#67679,#67680,#67681,#67682,#67683,#67684,
#67685,#67686,#67687,#67688,#67689,#67690,#67691,#67692,#67693,#67694,#67695,
#67696,#67697,#67698,#67699,#67700,#67701,#67702,#67703,#67704,#67705,#67706,
#67707,#67708,#67709,#67710,#67711,#67712,#67713,#67714,#67715,#67716,#67717,
#67718,#67719,#67720,#67721,#67722,#67723,#67724,#67725,#67726,#67727),
 .UNSPECIFIED.,.F.,.F.,(4,3,3,3,3,3,3,3,3,3,3,3,3,3,3,3,3,3,3,3,3,3,3,4),
(-1.12653966532772,-1.08393007696717,-1.01186793859786,-0.979479105150202,
-0.956116979414424,-0.875899251452182,-0.825471633444292,-0.806186641683957,
-0.795681523489941,-0.710458660083624,-0.626207772623579,-0.607006965671262,
-0.586923425467474,-0.51870091577066,-0.45118883434751,-0.412581370547731,
-0.394181524461002,-0.313650379586371,-0.253407622478375,-0.210833136397955,
-0.193782655965201,-0.11504060523123,-0.0378485150221377,0.),
 .UNSPECIFIED.);
#811=B_SPLINE_CURVE_WITH_KNOTS('',3,(#67730,#67731,#67732,#67733,#67734,
#67735,#67736,#67737,#67738,#67739,#67740,#67741),.UNSPECIFIED.,.F.,.F.,
(4,1,1,1,1,1,1,1,1,4),(11.6154215191107,12.1148317048449,12.6142418905792,
13.1136520763135,13.6130622620478,14.112472447782,14.6118826335163,15.1112928192506,
15.6107030049849,15.7079632679489),.UNSPECIFIED.);
#812=B_SPLINE_CURVE_WITH_KNOTS('',3,(#68907,#68908,#68909,#68910,#68911,
#68912,#68913,#68914,#68915,#68916,#68917,#68918,#68919,#68920,#68921,#68922,
#68923,#68924,#68925,#68926,#68927,#68928,#68929,#68930,#68931,#68932,#68933,
#68934,#68935,#68936,#68937,#68938,#68939,#68940,#68941,#68942,#68943,#68944,
#68945,#68946,#68947,#68948,#68949,#68950,#68951,#68952,#68953,#68954,#68955,
#68956,#68957,#68958,#68959,#68960,#68961,#68962,#68963,#68964,#68965,#68966,
#68967,#68968,#68969,#68970,#68971,#68972,#68973,#68974,#68975,#68976,#68977,
#68978,#68979),.UNSPECIFIED.,.F.,.F.,(4,3,3,3,3,3,3,3,3,3,3,3,3,3,3,3,3,
3,3,3,3,3,3,3,4),(-1.13094109509794,-1.09499881239224,-1.03107752332618,
-1.00370431382378,-0.983750382690077,-0.911532019409036,-0.881102067268382,
-0.860943264422037,-0.839313656127995,-0.758239093290739,-0.705009897535087,
-0.662463517590346,-0.643629976777734,-0.571319967865571,-0.501358662040571,
-0.457365024033757,-0.43311159034779,-0.346934199158609,-0.291474744565571,
-0.247356575879909,-0.228207098197964,-0.208365917531837,-0.120835914342496,
-0.032642851524005,0.),.UNSPECIFIED.);
#813=B_SPLINE_CURVE_WITH_KNOTS('',3,(#68980,#68981,#68982,#68983,#68984,
#68985,#68986,#68987,#68988,#68989,#68990,#68991,#68992),.UNSPECIFIED.,
 .F.,.F.,(4,3,3,3,4),(-143.830133491471,-143.330723305737,-142.831313120002,
-142.331902934268,-142.322618506789),.UNSPECIFIED.);
#814=B_SPLINE_CURVE_WITH_KNOTS('',3,(#69071,#69072,#69073,#69074,#69075,
#69076,#69077,#69078,#69079,#69080),.UNSPECIFIED.,.F.,.F.,(4,3,3,4),(-4.09323272002467,
-3.99580125629983,-2.99685094222487,-2.06652207565085),.UNSPECIFIED.);
#815=B_SPLINE_CURVE_WITH_KNOTS('',3,(#69083,#69084,#69085,#69086,#69087,
#69088,#69089,#69090,#69091,#69092),.UNSPECIFIED.,.F.,.F.,(4,3,3,4),(0.,
0.499475157037477,0.998950314074958,1.1148820092159),.UNSPECIFIED.);
#816=B_SPLINE_CURVE_WITH_KNOTS('',3,(#69097,#69098,#69099,#69100,#69101,
#69102,#69103,#69104,#69105,#69106,#69107,#69108,#69109,#69110,#69111,#69112,
#69113,#69114,#69115,#69116,#69117,#69118),.UNSPECIFIED.,.F.,.F.,(4,3,3,
3,3,3,3,4),(-10.3764180272043,-9.98950314074957,-8.99055282667461,-7.99160251259965,
-6.9926521985247,-5.99370188444974,-4.99475157037478,-4.09323272002467),
 .UNSPECIFIED.);
#817=B_SPLINE_CURVE_WITH_KNOTS('',3,(#69119,#69120,#69121,#69122,#69123,
#69124,#69125,#69126,#69127,#69128,#69129,#69130,#69131,#69132,#69133,#69134,
#69135,#69136,#69137,#69138,#69139,#69140),.UNSPECIFIED.,.F.,.F.,(4,3,3,
3,3,3,3,4),(1.1148820092159,1.99790062814991,2.99685094222487,3.99580125629982,
4.99475157037478,5.99370188444973,6.99265219852469,7.39806731639549),
 .UNSPECIFIED.);
#818=B_SPLINE_CURVE_WITH_KNOTS('',3,(#69145,#69146,#69147,#69148,#69149,
#69150,#69151,#69152,#69153,#69154,#69155,#69156,#69157,#69158,#69159,#69160,
#69161,#69162,#69163,#69164,#69165,#69166),.UNSPECIFIED.,.F.,.F.,(4,3,3,
3,3,3,3,4),(-16.6596033343838,-15.9832050251993,-14.9842547111244,-13.9853043970494,
-12.9863540829744,-11.9874037688995,-10.9884534548245,-10.3764180272043),
 .UNSPECIFIED.);
#819=B_SPLINE_CURVE_WITH_KNOTS('',3,(#69167,#69168,#69169,#69170,#69171,
#69172,#69173,#69174,#69175,#69176,#69177,#69178,#69179,#69180,#69181,#69182,
#69183,#69184,#69185,#69186,#69187,#69188),.UNSPECIFIED.,.F.,.F.,(4,3,3,
3,3,3,3,4),(7.39806731639549,7.99160251259965,8.99055282667461,9.98950314074957,
10.9884534548245,11.9874037688995,12.9863540829744,13.6812526235751),
 .UNSPECIFIED.);
#820=B_SPLINE_CURVE_WITH_KNOTS('',3,(#69193,#69194,#69195,#69196,#69197,
#69198,#69199,#69200,#69201,#69202,#69203,#69204,#69205,#69206,#69207,#69208,
#69209,#69210,#69211,#69212,#69213,#69214),.UNSPECIFIED.,.F.,.F.,(4,3,3,
3,3,3,3,4),(-22.9427886415634,-21.976906909649,-20.9779565955741,-19.9790062814991,
-18.9800559674242,-17.9811056533492,-16.9821553392743,-16.6596033343838),
 .UNSPECIFIED.);
#821=B_SPLINE_CURVE_WITH_KNOTS('',3,(#69215,#69216,#69217,#69218,#69219,
#69220,#69221,#69222,#69223,#69224,#69225,#69226,#69227,#69228,#69229,#69230,
#69231,#69232,#69233,#69234,#69235,#69236),.UNSPECIFIED.,.F.,.F.,(4,3,3,
3,3,3,3,4),(13.6812526235751,13.9853043970494,14.9842547111244,15.9832050251993,
16.9821553392743,17.9811056533492,18.9800559674242,19.9644379307546),
 .UNSPECIFIED.);
#822=B_SPLINE_CURVE_WITH_KNOTS('',3,(#69241,#69242,#69243,#69244,#69245,
#69246,#69247,#69248,#69249,#69250,#69251,#69252,#69253,#69254,#69255,#69256,
#69257,#69258,#69259,#69260,#69261,#69262,#69263,#69264,#69265),
 .UNSPECIFIED.,.F.,.F.,(4,3,3,3,3,3,3,3,4),(-29.225973948743,-28.9695591081737,
-27.9706087940988,-26.9716584800238,-25.9727081659489,-24.9737578518739,
-23.974807537799,-22.975857223724,-22.9427886415634),.UNSPECIFIED.);
#823=B_SPLINE_CURVE_WITH_KNOTS('',3,(#69266,#69267,#69268,#69269,#69270,
#69271,#69272,#69273,#69274,#69275,#69276,#69277,#69278,#69279,#69280,#69281,
#69282,#69283,#69284,#69285,#69286,#69287,#69288,#69289,#69290),
 .UNSPECIFIED.,.F.,.F.,(4,3,3,3,3,3,3,3,4),(19.9644379307546,19.9790062814991,
20.9779565955741,21.976906909649,22.975857223724,23.974807537799,24.9737578518739,
25.9727081659489,26.2476232379342),.UNSPECIFIED.);
#824=B_SPLINE_CURVE_WITH_KNOTS('',3,(#69295,#69296,#69297,#69298,#69299,
#69300,#69301,#69302,#69303,#69304,#69305,#69306,#69307,#69308,#69309,#69310,
#69311,#69312,#69313,#69314,#69315,#69316),.UNSPECIFIED.,.F.,.F.,(4,3,3,
3,3,3,3,4),(-35.5091592559226,-34.9632609926235,-33.9643106785485,-32.9653603644736,
-31.9664100503986,-30.9674597363237,-29.9685094222487,-29.225973948743),
 .UNSPECIFIED.);
#825=B_SPLINE_CURVE_WITH_KNOTS('',3,(#69317,#69318,#69319,#69320,#69321,
#69322,#69323,#69324,#69325,#69326,#69327,#69328,#69329,#69330,#69331,#69332,
#69333,#69334,#69335,#69336,#69337,#69338),.UNSPECIFIED.,.F.,.F.,(4,3,3,
3,3,3,3,4),(26.2476232379342,26.9716584800238,27.9706087940988,28.9695591081738,
29.9685094222487,30.9674597363237,31.9664100503986,32.5308085451138),
 .UNSPECIFIED.);
#826=B_SPLINE_CURVE_WITH_KNOTS('',3,(#69343,#69344,#69345,#69346,#69347,
#69348,#69349,#69350,#69351,#69352,#69353,#69354,#69355,#69356,#69357,#69358,
#69359,#69360,#69361,#69362,#69363,#69364),.UNSPECIFIED.,.F.,.F.,(4,3,3,
3,3,3,3,4),(-41.7923445631022,-40.9569628770732,-39.9580125629983,-38.9590622489233,
-37.9601119348484,-36.9611616207734,-35.9622113066984,-35.5091592559226),
 .UNSPECIFIED.);
#827=B_SPLINE_CURVE_WITH_KNOTS('',3,(#69365,#69366,#69367,#69368,#69369,
#69370,#69371,#69372,#69373,#69374,#69375,#69376,#69377,#69378,#69379,#69380,
#69381,#69382,#69383,#69384,#69385,#69386),.UNSPECIFIED.,.F.,.F.,(4,3,3,
3,3,3,3,4),(32.5308085451138,32.9653603644736,33.9643106785485,34.9632609926235,
35.9622113066984,36.9611616207734,37.9601119348484,38.8139938522934),
 .UNSPECIFIED.);
#828=B_SPLINE_CURVE_WITH_KNOTS('',3,(#69391,#69392,#69393,#69394,#69395,
#69396,#69397,#69398,#69399,#69400,#69401,#69402,#69403,#69404,#69405,#69406,
#69407,#69408,#69409,#69410,#69411,#69412,#69413,#69414,#69415),
 .UNSPECIFIED.,.F.,.F.,(4,3,3,3,3,3,3,3,4),(-48.0755298702818,-47.9496150755979,
-46.950664761523,-45.951714447448,-44.9527641333731,-43.9538138192981,-42.9548635052232,
-41.9559131911482,-41.7923445631022),.UNSPECIFIED.);
#829=B_SPLINE_CURVE_WITH_KNOTS('',3,(#69416,#69417,#69418,#69419,#69420,
#69421,#69422,#69423,#69424,#69425,#69426,#69427,#69428,#69429,#69430,#69431,
#69432,#69433,#69434,#69435,#69436,#69437,#69438,#69439,#69440),
 .UNSPECIFIED.,.F.,.F.,(4,3,3,3,3,3,3,3,4),(38.8139938522934,38.9590622489233,
39.9580125629983,40.9569628770732,41.9559131911482,42.9548635052232,43.9538138192981,
44.9527641333731,45.097179159473),.UNSPECIFIED.);
#830=B_SPLINE_CURVE_WITH_KNOTS('',3,(#69445,#69446,#69447,#69448,#69449,
#69450,#69451,#69452,#69453,#69454,#69455,#69456,#69457,#69458,#69459,#69460,
#69461,#69462,#69463,#69464,#69465,#69466),.UNSPECIFIED.,.F.,.F.,(4,3,3,
3,3,3,3,4),(-54.3587151774614,-53.9433169600477,-52.9443666459727,-51.9454163318978,
-50.9464660178228,-49.9475157037478,-48.9485653896729,-48.0755298702818),
 .UNSPECIFIED.);
#831=B_SPLINE_CURVE_WITH_KNOTS('',3,(#69467,#69468,#69469,#69470,#69471,
#69472,#69473,#69474,#69475,#69476,#69477,#69478,#69479,#69480,#69481,#69482,
#69483,#69484,#69485,#69486,#69487,#69488),.UNSPECIFIED.,.F.,.F.,(4,3,3,
3,3,3,3,4),(45.097179159473,45.951714447448,46.950664761523,47.9496150755979,
48.9485653896729,49.9475157037478,50.9464660178228,51.3803644666526),
 .UNSPECIFIED.);
#832=B_SPLINE_CURVE_WITH_KNOTS('',3,(#69493,#69494,#69495,#69496,#69497,
#69498,#69499,#69500,#69501,#69502,#69503,#69504,#69505,#69506,#69507,#69508,
#69509,#69510,#69511,#69512,#69513,#69514),.UNSPECIFIED.,.F.,.F.,(4,3,3,
3,3,3,3,4),(-60.641900484641,-59.9370188444974,-58.9380685304225,-57.9391182163475,
-56.9401679022725,-55.9412175881976,-54.9422672741226,-54.3587151774614),
 .UNSPECIFIED.);
#833=B_SPLINE_CURVE_WITH_KNOTS('',3,(#69515,#69516,#69517,#69518,#69519,
#69520,#69521,#69522,#69523,#69524,#69525,#69526,#69527,#69528,#69529,#69530,
#69531,#69532,#69533,#69534,#69535,#69536),.UNSPECIFIED.,.F.,.F.,(4,3,3,
3,3,3,3,4),(51.3803644666526,51.9454163318978,52.9443666459727,53.9433169600477,
54.9422672741226,55.9412175881976,56.9401679022725,57.6635497738322),
 .UNSPECIFIED.);
#834=B_SPLINE_CURVE_WITH_KNOTS('',3,(#69541,#69542,#69543,#69544,#69545,
#69546,#69547,#69548,#69549,#69550,#69551,#69552,#69553,#69554,#69555,#69556,
#69557,#69558,#69559,#69560,#69561,#69562),.UNSPECIFIED.,.F.,.F.,(4,3,3,
3,3,3,3,4),(-66.9250857918206,-65.9307207289471,-64.9317704148722,-63.9328201007972,
-62.9338697867223,-61.9349194726473,-60.9359691585724,-60.641900484641),
 .UNSPECIFIED.);
#835=B_SPLINE_CURVE_WITH_KNOTS('',3,(#69563,#69564,#69565,#69566,#69567,
#69568,#69569,#69570,#69571,#69572,#69573,#69574,#69575,#69576,#69577,#69578,
#69579,#69580,#69581,#69582,#69583,#69584,#69585,#69586,#69587),
 .UNSPECIFIED.,.F.,.F.,(4,3,3,3,3,3,3,3,4),(57.6635497738322,57.9391182163475,
58.9380685304225,59.9370188444974,60.9359691585724,61.9349194726473,62.9338697867223,
63.9328201007973,63.9467350810118),.UNSPECIFIED.);
#836=B_SPLINE_CURVE_WITH_KNOTS('',3,(#69592,#69593,#69594,#69595,#69596,
#69597,#69598,#69599,#69600,#69601,#69602,#69603,#69604,#69605,#69606,#69607,
#69608,#69609,#69610,#69611,#69612,#69613,#69614,#69615,#69616),
 .UNSPECIFIED.,.F.,.F.,(4,3,3,3,3,3,3,3,4),(-73.2082710990002,-72.9233729274718,
-71.9244226133969,-70.9254722993219,-69.926521985247,-68.927571671172,-67.928621357097,
-66.9296710430221,-66.9250857918206),.UNSPECIFIED.);
#837=B_SPLINE_CURVE_WITH_KNOTS('',3,(#69617,#69618,#69619,#69620,#69621,
#69622,#69623,#69624,#69625,#69626,#69627,#69628,#69629,#69630,#69631,#69632,
#69633,#69634,#69635,#69636,#69637,#69638),.UNSPECIFIED.,.F.,.F.,(4,3,3,
3,3,3,3,4),(63.9467350810118,64.9317704148722,65.9307207289472,66.9296710430221,
67.9286213570971,68.927571671172,69.926521985247,70.2299203881914),
 .UNSPECIFIED.);
#838=B_SPLINE_CURVE_WITH_KNOTS('',3,(#69643,#69644,#69645,#69646,#69647,
#69648,#69649,#69650,#69651,#69652,#69653,#69654,#69655,#69656,#69657,#69658,
#69659,#69660,#69661,#69662,#69663,#69664),.UNSPECIFIED.,.F.,.F.,(4,3,3,
3,3,3,3,4),(-79.4914564061798,-78.9170748119216,-77.9181244978466,-76.9191741837717,
-75.9202238696967,-74.9212735556218,-73.9223232415468,-73.2082710990002),
 .UNSPECIFIED.);
#839=B_SPLINE_CURVE_WITH_KNOTS('',3,(#69665,#69666,#69667,#69668,#69669,
#69670,#69671,#69672,#69673,#69674,#69675,#69676,#69677,#69678,#69679,#69680,
#69681,#69682,#69683,#69684,#69685,#69686),.UNSPECIFIED.,.F.,.F.,(4,3,3,
3,3,3,3,4),(70.2299203881914,70.925472299322,71.9244226133969,72.9233729274719,
73.9223232415468,74.9212735556218,75.9202238696967,76.513105695371),
 .UNSPECIFIED.);
#840=B_SPLINE_CURVE_WITH_KNOTS('',3,(#69691,#69692,#69693,#69694,#69695,
#69696,#69697,#69698,#69699,#69700,#69701,#69702,#69703,#69704,#69705,#69706,
#69707,#69708,#69709,#69710,#69711,#69712),.UNSPECIFIED.,.F.,.F.,(4,3,3,
3,3,3,3,4),(-85.7746417133593,-84.9107766963713,-83.9118263822964,-82.9128760682214,
-81.9139257541465,-80.9149754400715,-79.9160251259965,-79.4914564061798),
 .UNSPECIFIED.);
#841=B_SPLINE_CURVE_WITH_KNOTS('',3,(#69713,#69714,#69715,#69716,#69717,
#69718,#69719,#69720,#69721,#69722,#69723,#69724,#69725,#69726,#69727,#69728,
#69729,#69730,#69731,#69732,#69733,#69734),.UNSPECIFIED.,.F.,.F.,(4,3,3,
3,3,3,3,4),(76.513105695371,76.9191741837717,77.9181244978466,78.9170748119216,
79.9160251259966,80.9149754400715,81.9139257541465,82.7962910025506),
 .UNSPECIFIED.);
#842=B_SPLINE_CURVE_WITH_KNOTS('',3,(#69739,#69740,#69741,#69742,#69743,
#69744,#69745,#69746,#69747,#69748,#69749,#69750,#69751,#69752,#69753,#69754,
#69755,#69756,#69757,#69758,#69759,#69760,#69761,#69762,#69763),
 .UNSPECIFIED.,.F.,.F.,(4,3,3,3,3,3,3,3,4),(-92.057827020539,-91.903428894896,
-90.9044785808211,-89.9055282667461,-88.9065779526712,-87.9076276385962,
-86.9086773245212,-85.9097270104463,-85.7746417133593),.UNSPECIFIED.);
#843=B_SPLINE_CURVE_WITH_KNOTS('',3,(#69764,#69765,#69766,#69767,#69768,
#69769,#69770,#69771,#69772,#69773,#69774,#69775,#69776,#69777,#69778,#69779,
#69780,#69781,#69782,#69783,#69784,#69785,#69786,#69787,#69788),
 .UNSPECIFIED.,.F.,.F.,(4,3,3,3,3,3,3,3,4),(82.7962910025506,82.9128760682214,
83.9118263822964,84.9107766963714,85.9097270104463,86.9086773245213,87.9076276385962,
88.9065779526712,89.0794763097302),.UNSPECIFIED.);
#844=B_SPLINE_CURVE_WITH_KNOTS('',3,(#69793,#69794,#69795,#69796,#69797,
#69798,#69799,#69800,#69801,#69802,#69803,#69804,#69805,#69806,#69807,#69808,
#69809,#69810,#69811,#69812,#69813,#69814),.UNSPECIFIED.,.F.,.F.,(4,3,3,
3,3,3,3,4),(-98.3410123277185,-97.8971307793458,-96.8981804652708,-95.8992301511959,
-94.9002798371209,-93.9013295230459,-92.902379208971,-92.057827020539),
 .UNSPECIFIED.);
#845=B_SPLINE_CURVE_WITH_KNOTS('',3,(#69815,#69816,#69817,#69818,#69819,
#69820,#69821,#69822,#69823,#69824,#69825,#69826,#69827,#69828,#69829,#69830,
#69831,#69832,#69833,#69834,#69835,#69836),.UNSPECIFIED.,.F.,.F.,(4,3,3,
3,3,3,3,4),(89.0794763097302,89.9055282667461,90.9044785808211,91.903428894896,
92.902379208971,93.901329523046,94.9002798371209,95.3626616169097),
 .UNSPECIFIED.);
#846=B_SPLINE_CURVE_WITH_KNOTS('',3,(#69841,#69842,#69843,#69844,#69845,
#69846,#69847,#69848,#69849,#69850,#69851,#69852,#69853,#69854,#69855,#69856,
#69857,#69858,#69859,#69860,#69861,#69862),.UNSPECIFIED.,.F.,.F.,(4,3,3,
3,3,3,3,4),(-104.624197634898,-103.890832663796,-102.891882349721,-101.892932035646,
-100.893981721571,-99.8950314074957,-98.8960810934207,-98.3410123277185),
 .UNSPECIFIED.);
#847=B_SPLINE_CURVE_WITH_KNOTS('',3,(#69863,#69864,#69865,#69866,#69867,
#69868,#69869,#69870,#69871,#69872,#69873,#69874,#69875,#69876,#69877,#69878,
#69879,#69880,#69881,#69882,#69883,#69884),.UNSPECIFIED.,.F.,.F.,(4,3,3,
3,3,3,3,4),(95.3626616169097,95.8992301511959,96.8981804652708,97.8971307793458,
98.8960810934207,99.8950314074957,100.893981721571,101.645846924089),
 .UNSPECIFIED.);
#848=B_SPLINE_CURVE_WITH_KNOTS('',3,(#69889,#69890,#69891,#69892,#69893,
#69894,#69895,#69896,#69897,#69898,#69899,#69900,#69901,#69902,#69903,#69904,
#69905,#69906,#69907,#69908,#69909,#69910,#69911,#69912,#69913),
 .UNSPECIFIED.,.F.,.F.,(4,3,3,3,3,3,3,3,4),(-110.907382942078,-110.88348486232,
-109.884534548245,-108.88558423417,-107.886633920095,-106.88768360602,-105.888733291945,
-104.88978297787,-104.624197634898),.UNSPECIFIED.);
#849=B_SPLINE_CURVE_WITH_KNOTS('',3,(#69914,#69915,#69916,#69917,#69918,
#69919,#69920,#69921,#69922,#69923,#69924,#69925,#69926,#69927,#69928,#69929,
#69930,#69931,#69932,#69933,#69934,#69935,#69936,#69937,#69938),
 .UNSPECIFIED.,.F.,.F.,(4,3,3,3,3,3,3,3,4),(101.645846924089,101.892932035646,
102.891882349721,103.890832663795,104.88978297787,105.888733291945,106.88768360602,
107.886633920095,107.929032231269),.UNSPECIFIED.);
#850=B_SPLINE_CURVE_WITH_KNOTS('',3,(#69943,#69944,#69945,#69946,#69947,
#69948,#69949,#69950,#69951,#69952,#69953,#69954,#69955,#69956,#69957,#69958,
#69959,#69960,#69961,#69962,#69963,#69964),.UNSPECIFIED.,.F.,.F.,(4,3,3,
3,3,3,3,4),(-117.190568249257,-116.87718674677,-115.878236432695,-114.87928611862,
-113.880335804545,-112.88138549047,-111.882435176395,-110.907382942078),
 .UNSPECIFIED.);
#851=B_SPLINE_CURVE_WITH_KNOTS('',3,(#69965,#69966,#69967,#69968,#69969,
#69970,#69971,#69972,#69973,#69974,#69975,#69976,#69977,#69978,#69979,#69980,
#69981,#69982,#69983,#69984,#69985,#69986),.UNSPECIFIED.,.F.,.F.,(4,3,3,
3,3,3,3,4),(107.929032231269,108.88558423417,109.884534548245,110.88348486232,
111.882435176395,112.88138549047,113.880335804545,114.212217538449),
 .UNSPECIFIED.);
#852=B_SPLINE_CURVE_WITH_KNOTS('',3,(#69991,#69992,#69993,#69994,#69995,
#69996,#69997,#69998,#69999,#70000,#70001,#70002,#70003,#70004,#70005,#70006,
#70007,#70008,#70009,#70010,#70011,#70012),.UNSPECIFIED.,.F.,.F.,(4,3,3,
3,3,3,3,4),(-123.473753556437,-122.87088863122,-121.871938317145,-120.87298800307,
-119.874037688995,-118.87508737492,-117.876137060845,-117.190568249257),
 .UNSPECIFIED.);
#853=B_SPLINE_CURVE_WITH_KNOTS('',3,(#70013,#70014,#70015,#70016,#70017,
#70018,#70019,#70020,#70021,#70022,#70023,#70024,#70025,#70026,#70027,#70028,
#70029,#70030,#70031,#70032,#70033,#70034),.UNSPECIFIED.,.F.,.F.,(4,3,3,
3,3,3,3,4),(114.212217538449,114.87928611862,115.878236432695,116.87718674677,
117.876137060845,118.87508737492,119.874037688995,120.495402845628),
 .UNSPECIFIED.);
#854=B_SPLINE_CURVE_WITH_KNOTS('',3,(#70039,#70040,#70041,#70042,#70043,
#70044,#70045,#70046,#70047,#70048,#70049,#70050,#70051,#70052,#70053,#70054,
#70055,#70056,#70057,#70058,#70059,#70060),.UNSPECIFIED.,.F.,.F.,(4,3,3,
3,3,3,3,4),(-129.756938863617,-128.864590515669,-127.865640201594,-126.86668988752,
-125.867739573445,-124.86878925937,-123.869838945295,-123.473753556437),
 .UNSPECIFIED.);
#855=B_SPLINE_CURVE_WITH_KNOTS('',3,(#70061,#70062,#70063,#70064,#70065,
#70066,#70067,#70068,#70069,#70070,#70071,#70072,#70073,#70074,#70075,#70076,
#70077,#70078,#70079,#70080,#70081,#70082),.UNSPECIFIED.,.F.,.F.,(4,3,3,
3,3,3,3,4),(120.495402845628,120.87298800307,121.871938317145,122.87088863122,
123.869838945295,124.86878925937,125.867739573445,126.778588152808),
 .UNSPECIFIED.);
#856=B_SPLINE_CURVE_WITH_KNOTS('',3,(#70087,#70088,#70089,#70090,#70091,
#70092,#70093,#70094,#70095,#70096,#70097,#70098,#70099,#70100,#70101,#70102,
#70103,#70104,#70105,#70106,#70107,#70108,#70109,#70110,#70111),
 .UNSPECIFIED.,.F.,.F.,(4,3,3,3,3,3,3,3,4),(-136.040124170796,-135.857242714194,
-134.858292400119,-133.859342086044,-132.860391771969,-131.861441457894,
-130.862491143819,-129.863540829744,-129.756938863617),.UNSPECIFIED.);
#857=B_SPLINE_CURVE_WITH_KNOTS('',3,(#70112,#70113,#70114,#70115,#70116,
#70117,#70118,#70119,#70120,#70121,#70122,#70123,#70124,#70125,#70126,#70127,
#70128,#70129,#70130,#70131,#70132,#70133,#70134,#70135,#70136),
 .UNSPECIFIED.,.F.,.F.,(4,3,3,3,3,3,3,3,4),(126.778588152808,126.86668988752,
127.865640201594,128.864590515669,129.863540829744,130.862491143819,131.861441457894,
132.860391771969,133.061773459987),.UNSPECIFIED.);
#858=B_SPLINE_CURVE_WITH_KNOTS('',3,(#70141,#70142,#70143,#70144,#70145,
#70146,#70147,#70148,#70149,#70150,#70151,#70152,#70153,#70154,#70155,#70156,
#70157,#70158,#70159,#70160,#70161,#70162),.UNSPECIFIED.,.F.,.F.,(4,3,3,
3,3,3,3,4),(-142.323309477976,-141.850944598644,-140.851994284569,-139.853043970494,
-138.854093656419,-137.855143342344,-136.856193028269,-136.040124170796),
 .UNSPECIFIED.);
#859=B_SPLINE_CURVE_WITH_KNOTS('',3,(#70163,#70164,#70165,#70166,#70167,
#70168,#70169,#70170,#70171,#70172,#70173,#70174,#70175,#70176,#70177,#70178,
#70179,#70180,#70181,#70182,#70183,#70184),.UNSPECIFIED.,.F.,.F.,(4,3,3,
3,3,3,3,4),(133.061773459987,133.859342086044,134.858292400119,135.857242714194,
136.856193028269,137.855143342344,138.854093656419,139.344958767167),
 .UNSPECIFIED.);
#860=B_SPLINE_CURVE_WITH_KNOTS('',3,(#70190,#70191,#70192,#70193,#70194),
 .UNSPECIFIED.,.F.,.F.,(4,1,4),(153.9380400259,154.464625460643,155.394954327217),
 .UNSPECIFIED.);
#861=B_SPLINE_CURVE_WITH_KNOTS('',3,(#70197,#70198,#70199,#70200),
 .UNSPECIFIED.,.F.,.F.,(4,4),(153.9380400259,154.156641806497),
 .UNSPECIFIED.);
#862=B_SPLINE_CURVE_WITH_KNOTS('',3,(#70205,#70206,#70207,#70208,#70209,
#70210,#70211,#70212,#70213,#70214),.UNSPECIFIED.,.F.,.F.,(4,1,1,1,1,1,
1,4),(147.65485471872,148.470923576193,149.469873890268,150.468824204343,
151.467774518418,152.466724832493,153.465675146568,153.9380400259),
 .UNSPECIFIED.);
#863=B_SPLINE_CURVE_WITH_KNOTS('',3,(#70215,#70216,#70217,#70218,#70219,
#70220,#70221,#70222,#70223,#70224,#70225),.UNSPECIFIED.,.F.,.F.,(4,1,1,
1,1,1,1,1,4),(147.65485471872,148.162939922047,149.161890236122,150.160840550197,
151.159790864272,152.158741178347,153.157691492422,153.65716664946,153.9380400259),
 .UNSPECIFIED.);
#864=B_SPLINE_CURVE_WITH_KNOTS('',3,(#70230,#70231,#70232,#70233,#70234,
#70235,#70236,#70237,#70238,#70239,#70240),.UNSPECIFIED.,.F.,.F.,(4,1,1,
1,1,1,1,1,4),(141.371669411541,141.478271377669,142.477221691744,143.476172005819,
144.475122319894,145.474072633968,146.473022948043,147.471973262118,147.65485471872),
 .UNSPECIFIED.);
#865=B_SPLINE_CURVE_WITH_KNOTS('',3,(#70241,#70242,#70243,#70244,#70245,
#70246,#70247,#70248,#70249,#70250),.UNSPECIFIED.,.F.,.F.,(4,1,1,1,1,1,
1,4),(141.371669411541,142.169238037598,143.168188351673,144.167138665748,
145.166088979822,146.165039293897,147.163989607972,147.65485471872),
 .UNSPECIFIED.);
#866=B_SPLINE_CURVE_WITH_KNOTS('',3,(#70255,#70256,#70257,#70258,#70259,
#70260,#70261,#70262,#70263,#70264),.UNSPECIFIED.,.F.,.F.,(4,1,1,1,1,1,
1,4),(135.088484104361,135.484569493219,136.483519807294,137.482470121369,
138.481420435444,139.480370749519,140.479321063594,141.371669411541),
 .UNSPECIFIED.);
#867=B_SPLINE_CURVE_WITH_KNOTS('',3,(#70265,#70266,#70267,#70268,#70269,
#70270,#70271,#70272,#70273,#70274,#70275),.UNSPECIFIED.,.F.,.F.,(4,1,1,
1,1,1,1,1,4),(135.088484104361,135.176585839073,136.175536153148,137.174486467223,
138.173436781298,139.172387095373,140.171337409448,141.170287723523,141.371669411541),
 .UNSPECIFIED.);
#868=B_SPLINE_CURVE_WITH_KNOTS('',3,(#70280,#70281,#70282,#70283,#70284,
#70285,#70286,#70287,#70288,#70289),.UNSPECIFIED.,.F.,.F.,(4,1,1,1,1,1,
1,4),(128.805298797182,129.490867608769,130.489817922844,131.488768236919,
132.487718550994,133.486668865069,134.485619179144,135.088484104361),
 .UNSPECIFIED.);
#869=B_SPLINE_CURVE_WITH_KNOTS('',3,(#70290,#70291,#70292,#70293,#70294,
#70295,#70296,#70297,#70298,#70299),.UNSPECIFIED.,.F.,.F.,(4,1,1,1,1,1,
1,4),(128.805298797182,129.182883954623,130.181834268698,131.180784582773,
132.179734896848,133.178685210923,134.177635524998,135.088484104361),
 .UNSPECIFIED.);
#870=B_SPLINE_CURVE_WITH_KNOTS('',3,(#70304,#70305,#70306,#70307,#70308,
#70309,#70310,#70311,#70312,#70313),.UNSPECIFIED.,.F.,.F.,(4,1,1,1,1,1,
1,4),(122.522113490002,123.497165724319,124.496116038394,125.495066352469,
126.494016666544,127.492966980619,128.491917294694,128.805298797182),
 .UNSPECIFIED.);
#871=B_SPLINE_CURVE_WITH_KNOTS('',3,(#70314,#70315,#70316,#70317,#70318,
#70319,#70320,#70321,#70322,#70323),.UNSPECIFIED.,.F.,.F.,(4,1,1,1,1,1,
1,4),(122.522113490002,123.189182070173,124.188132384248,125.187082698323,
126.186033012398,127.184983326473,128.183933640548,128.805298797182),
 .UNSPECIFIED.);
#872=B_SPLINE_CURVE_WITH_KNOTS('',3,(#70328,#70329,#70330,#70331,#70332,
#70333,#70334,#70335,#70336,#70337,#70338),.UNSPECIFIED.,.F.,.F.,(4,1,1,
1,1,1,1,1,4),(116.238928182822,116.504513525795,117.50346383987,118.502414153945,
119.50136446802,120.500314782095,121.49926509617,122.498215410244,122.522113490002),
 .UNSPECIFIED.);
#873=B_SPLINE_CURVE_WITH_KNOTS('',3,(#70339,#70340,#70341,#70342,#70343,
#70344,#70345,#70346,#70347,#70348),.UNSPECIFIED.,.F.,.F.,(4,1,1,1,1,1,
1,4),(116.238928182822,117.195480185724,118.194430499799,119.193380813874,
120.192331127949,121.191281442024,122.190231756098,122.522113490002),
 .UNSPECIFIED.);
#874=B_SPLINE_CURVE_WITH_KNOTS('',3,(#70353,#70354,#70355,#70356,#70357,
#70358,#70359,#70360,#70361,#70362),.UNSPECIFIED.,.F.,.F.,(4,1,1,1,1,1,
1,4),(109.955742875643,110.510811641345,111.50976195542,112.508712269495,
113.50766258357,114.506612897645,115.50556321172,116.238928182822),
 .UNSPECIFIED.);
#875=B_SPLINE_CURVE_WITH_KNOTS('',3,(#70363,#70364,#70365,#70366,#70367,
#70368,#70369,#70370,#70371,#70372,#70373),.UNSPECIFIED.,.F.,.F.,(4,1,1,
1,1,1,1,1,4),(109.955742875643,110.202827987199,111.201778301274,112.200728615349,
113.199678929424,114.198629243499,115.197579557574,116.196529871649,116.238928182822),
 .UNSPECIFIED.);
#876=B_SPLINE_CURVE_WITH_KNOTS('',3,(#70378,#70379,#70380,#70381,#70382,
#70383,#70384,#70385,#70386,#70387),.UNSPECIFIED.,.F.,.F.,(4,1,1,1,1,1,
1,4),(103.672557568463,104.517109756895,105.51606007097,106.515010385045,
107.51396069912,108.512911013195,109.51186132727,109.955742875643),
 .UNSPECIFIED.);
#877=B_SPLINE_CURVE_WITH_KNOTS('',3,(#70388,#70389,#70390,#70391,#70392,
#70393,#70394,#70395,#70396,#70397),.UNSPECIFIED.,.F.,.F.,(4,1,1,1,1,1,
1,4),(103.672557568463,104.209126102749,105.208076416824,106.207026730899,
107.205977044974,108.204927359049,109.203877673124,109.955742875643),
 .UNSPECIFIED.);
#878=B_SPLINE_CURVE_WITH_KNOTS('',3,(#70402,#70403,#70404,#70405,#70406,
#70407,#70408,#70409,#70410,#70411,#70412),.UNSPECIFIED.,.F.,.F.,(4,1,1,
1,1,1,1,1,4),(97.3893722612836,97.5244575583706,98.5234078724455,99.5223581865205,
100.521308500595,101.52025881467,102.519209128745,103.51815944282,103.672557568463),
 .UNSPECIFIED.);
#879=B_SPLINE_CURVE_WITH_KNOTS('',3,(#70413,#70414,#70415,#70416,#70417,
#70418,#70419,#70420,#70421,#70422),.UNSPECIFIED.,.F.,.F.,(4,1,1,1,1,1,
1,4),(97.3893722612836,98.2154242182995,99.2143745323745,100.213324846449,
101.212275160524,102.211225474599,103.210175788674,103.672557568463),
 .UNSPECIFIED.);
#880=B_SPLINE_CURVE_WITH_KNOTS('',3,(#70427,#70428,#70429,#70430,#70431,
#70432,#70433,#70434,#70435,#70436),.UNSPECIFIED.,.F.,.F.,(4,1,1,1,1,1,
1,4),(91.106186954104,91.5307556739208,92.5297059879958,93.5286563020707,
94.5276066161457,95.5265569302206,96.5255072442956,97.3893722612836),
 .UNSPECIFIED.);
#881=B_SPLINE_CURVE_WITH_KNOTS('',3,(#70437,#70438,#70439,#70440,#70441,
#70442,#70443,#70444,#70445,#70446,#70447),.UNSPECIFIED.,.F.,.F.,(4,1,1,
1,1,1,1,1,4),(91.106186954104,91.2227720197748,92.2217223338498,93.2206726479247,
94.2196229619997,95.2185732760747,96.2175235901496,97.2164739042246,97.3893722612836),
 .UNSPECIFIED.);
#882=B_SPLINE_CURVE_WITH_KNOTS('',3,(#70452,#70453,#70454,#70455,#70456,
#70457,#70458,#70459,#70460,#70461),.UNSPECIFIED.,.F.,.F.,(4,1,1,1,1,1,
1,4),(84.8230016469244,85.5370537894711,86.536004103546,87.534954417621,
88.5339047316959,89.5328550457709,90.5318053598459,91.106186954104),
 .UNSPECIFIED.);
#883=B_SPLINE_CURVE_WITH_KNOTS('',3,(#70462,#70463,#70464,#70465,#70466,
#70467,#70468,#70469,#70470,#70471),.UNSPECIFIED.,.F.,.F.,(4,1,1,1,1,1,
1,4),(84.8230016469244,85.2290701353251,86.2280204494,87.226970763475,88.2259210775499,
89.2248713916249,90.2238217056999,91.106186954104),.UNSPECIFIED.);
#884=B_SPLINE_CURVE_WITH_KNOTS('',3,(#70476,#70477,#70478,#70479,#70480,
#70481,#70482,#70483,#70484,#70485,#70486),.UNSPECIFIED.,.F.,.F.,(4,1,1,
1,1,1,1,1,4),(78.5398163397448,78.5444015909464,79.5433519050213,80.5423022190963,
81.5412525331712,82.5402028472462,83.5391531613212,84.5381034753961,84.8230016469244),
 .UNSPECIFIED.);
#885=B_SPLINE_CURVE_WITH_KNOTS('',3,(#70487,#70488,#70489,#70490,#70491,
#70492,#70493,#70494,#70495,#70496),.UNSPECIFIED.,.F.,.F.,(4,1,1,1,1,1,
1,4),(78.5398163397448,79.2353682508753,80.2343185649503,81.2332688790252,
82.2322191931002,83.2311695071752,84.2301198212501,84.8230016469244),
 .UNSPECIFIED.);
#886=B_SPLINE_CURVE_WITH_KNOTS('',3,(#70501,#70502,#70503,#70504,#70505,
#70506,#70507,#70508,#70509,#70510),.UNSPECIFIED.,.F.,.F.,(4,1,1,1,1,1,
1,4),(72.2566310325653,72.5506997064966,73.5496500205716,74.5486003346466,
75.5475506487215,76.5465009627965,77.5454512768714,78.5398163397448),
 .UNSPECIFIED.);
#887=B_SPLINE_CURVE_WITH_KNOTS('',3,(#70511,#70512,#70513,#70514,#70515,
#70516,#70517,#70518,#70519,#70520),.UNSPECIFIED.,.F.,.F.,(4,1,1,1,1,1,
1,4),(72.2566310325653,73.2416663664256,74.2406166805006,75.2395669945755,
76.2385173086505,77.2374676227254,78.2364179368004,78.5398163397448),
 .UNSPECIFIED.);
#888=B_SPLINE_CURVE_WITH_KNOTS('',3,(#70525,#70526,#70527,#70528,#70529,
#70530,#70531,#70532,#70533,#70534),.UNSPECIFIED.,.F.,.F.,(4,1,1,1,1,1,
1,4),(65.9734457253856,66.5569978220469,67.5559481361219,68.5548984501968,
69.5538487642718,70.5527990783467,71.5517493924217,72.2566310325653),
 .UNSPECIFIED.);
#889=B_SPLINE_CURVE_WITH_KNOTS('',3,(#70535,#70536,#70537,#70538,#70539,
#70540,#70541,#70542,#70543,#70544,#70545),.UNSPECIFIED.,.F.,.F.,(4,1,1,
1,1,1,1,1,4),(65.9734457253856,66.2490141679009,67.2479644819759,68.2469147960508,
69.2458651101258,70.2448154242007,71.2437657382757,72.2427160523506,72.2566310325653),
 .UNSPECIFIED.);
#890=B_SPLINE_CURVE_WITH_KNOTS('',3,(#70550,#70551,#70552,#70553,#70554,
#70555,#70556,#70557,#70558,#70559),.UNSPECIFIED.,.F.,.F.,(4,1,1,1,1,1,
1,4),(59.6902604182061,60.5632959375972,61.5622462516721,62.5611965657471,
63.560146879822,64.559097193897,65.5580475079719,65.9734457253856),
 .UNSPECIFIED.);
#891=B_SPLINE_CURVE_WITH_KNOTS('',3,(#70560,#70561,#70562,#70563,#70564,
#70565,#70566,#70567,#70568,#70569),.UNSPECIFIED.,.F.,.F.,(4,1,1,1,1,1,
1,4),(59.6902604182061,60.2553122834511,61.2542625975261,62.2532129116011,
63.252163225676,64.251113539751,65.2500638538259,65.9734457253856),
 .UNSPECIFIED.);
#892=B_SPLINE_CURVE_WITH_KNOTS('',3,(#70574,#70575,#70576,#70577,#70578,
#70579,#70580,#70581,#70582,#70583,#70584),.UNSPECIFIED.,.F.,.F.,(4,1,1,
1,1,1,1,1,4),(53.4070751110265,53.5706437390725,54.5695940531474,55.5685443672224,
56.5674946812973,57.5664449953723,58.5653953094472,59.5643456235222,59.6902604182061),
 .UNSPECIFIED.);
#893=B_SPLINE_CURVE_WITH_KNOTS('',3,(#70585,#70586,#70587,#70588,#70589,
#70590,#70591,#70592,#70593,#70594),.UNSPECIFIED.,.F.,.F.,(4,1,1,1,1,1,
1,4),(53.4070751110265,54.2616103990014,55.2605607130764,56.2595110271513,
57.2584613412263,58.2574116553012,59.2563619693762,59.6902604182061),
 .UNSPECIFIED.);
#894=B_SPLINE_CURVE_WITH_KNOTS('',3,(#70599,#70600,#70601,#70602,#70603,
#70604,#70605,#70606,#70607,#70608),.UNSPECIFIED.,.F.,.F.,(4,1,1,1,1,1,
1,4),(47.1238898038469,47.5769418546227,48.5758921686977,49.5748424827726,
50.5737927968476,51.5727431109225,52.5716934249975,53.4070751110265),
 .UNSPECIFIED.);
#895=B_SPLINE_CURVE_WITH_KNOTS('',3,(#70609,#70610,#70611,#70612,#70613,
#70614,#70615,#70616,#70617,#70618,#70619),.UNSPECIFIED.,.F.,.F.,(4,1,1,
1,1,1,1,1,4),(47.1238898038469,47.2689582004767,48.2679085145517,49.2668588286266,
50.2658091427016,51.2647594567765,52.2637097708515,53.2626600849265,53.4070751110265),
 .UNSPECIFIED.);
#896=B_SPLINE_CURVE_WITH_KNOTS('',3,(#70624,#70625,#70626,#70627,#70628,
#70629,#70630,#70631,#70632,#70633),.UNSPECIFIED.,.F.,.F.,(4,1,1,1,1,1,
1,4),(40.8407044966673,41.583239970173,42.5821902842479,43.5811405983229,
44.5800909123978,45.5790412264728,46.5779915405478,47.1238898038469),
 .UNSPECIFIED.);
#897=B_SPLINE_CURVE_WITH_KNOTS('',3,(#70634,#70635,#70636,#70637,#70638,
#70639,#70640,#70641,#70642,#70643),.UNSPECIFIED.,.F.,.F.,(4,1,1,1,1,1,
1,4),(40.8407044966673,41.275256316027,42.2742066301019,43.2731569441769,
44.2721072582518,45.2710575723268,46.2700078864018,47.1238898038469),
 .UNSPECIFIED.);
#898=B_SPLINE_CURVE_WITH_KNOTS('',3,(#70648,#70649,#70650,#70651,#70652,
#70653,#70654,#70655,#70656,#70657,#70658),.UNSPECIFIED.,.F.,.F.,(4,1,1,
1,1,1,1,1,4),(34.5575191894877,34.5905877716483,35.5895380857232,36.5884883997982,
37.5874387138731,38.5863890279481,39.5853393420231,40.584289656098,40.8407044966673),
 .UNSPECIFIED.);
#899=B_SPLINE_CURVE_WITH_KNOTS('',3,(#70659,#70660,#70661,#70662,#70663,
#70664,#70665,#70666,#70667,#70668),.UNSPECIFIED.,.F.,.F.,(4,1,1,1,1,1,
1,4),(34.5575191894877,35.2815544315772,36.2805047456522,37.2794550597271,
38.2784053738021,39.2773556878771,40.276306001952,40.8407044966673),
 .UNSPECIFIED.);
#900=B_SPLINE_CURVE_WITH_KNOTS('',3,(#70673,#70674,#70675,#70676,#70677,
#70678,#70679,#70680,#70681,#70682),.UNSPECIFIED.,.F.,.F.,(4,1,1,1,1,1,
1,4),(28.2743338823081,28.5968858871985,29.5958362012735,30.5947865153485,
31.5937368294234,32.5926871434984,33.5916374575733,34.5575191894877),
 .UNSPECIFIED.);
#901=B_SPLINE_CURVE_WITH_KNOTS('',3,(#70683,#70684,#70685,#70686,#70687,
#70688,#70689,#70690,#70691,#70692,#70693),.UNSPECIFIED.,.F.,.F.,(4,1,1,
1,1,1,1,1,4),(28.2743338823081,28.2889022330525,29.2878525471275,30.2868028612024,
31.2857531752774,32.2847034893524,33.2836538034273,34.2826041175023,34.5575191894877),
 .UNSPECIFIED.);
#902=B_SPLINE_CURVE_WITH_KNOTS('',3,(#70698,#70699,#70700,#70701,#70702,
#70703,#70704,#70705,#70706,#70707),.UNSPECIFIED.,.F.,.F.,(4,1,1,1,1,1,
1,4),(21.9911485751285,22.6031840027488,23.6021343168238,24.6010846308987,
25.6000349449737,26.5989852590486,27.5979355731236,28.2743338823081),
 .UNSPECIFIED.);
#903=B_SPLINE_CURVE_WITH_KNOTS('',3,(#70708,#70709,#70710,#70711,#70712,
#70713,#70714,#70715,#70716,#70717),.UNSPECIFIED.,.F.,.F.,(4,1,1,1,1,1,
1,4),(21.9911485751285,22.2952003486028,23.2941506626778,24.2931009767527,
25.2920512908277,26.2910016049026,27.2899519189776,28.2743338823081),
 .UNSPECIFIED.);
#904=B_SPLINE_CURVE_WITH_KNOTS('',3,(#70722,#70723,#70724,#70725,#70726,
#70727,#70728,#70729,#70730,#70731),.UNSPECIFIED.,.F.,.F.,(4,1,1,1,1,1,
1,4),(15.7079632679489,16.6094821182991,17.608432432374,18.607382746449,
19.6063330605239,20.6052833745989,21.6042336886738,21.9911485751285),
 .UNSPECIFIED.);
#905=B_SPLINE_CURVE_WITH_KNOTS('',3,(#70732,#70733,#70734,#70735,#70736,
#70737,#70738,#70739,#70740,#70741),.UNSPECIFIED.,.F.,.F.,(4,1,1,1,1,1,
1,4),(15.7079632679489,16.3014984641531,17.300448778228,18.299399092303,
19.2983494063779,20.2972997204529,21.2962500345278,21.9911485751285),
 .UNSPECIFIED.);
#906=B_SPLINE_CURVE_WITH_KNOTS('',3,(#70744,#70745,#70746,#70747,#70748,
#70749,#70750,#70751,#70752,#70753,#70754,#70755,#70756,#70757,#70758,#70759,
#70760,#70761,#70762,#70763,#70764,#70765,#70766,#70767,#70768,#70769,#70770,
#70771,#70772,#70773,#70774,#70775,#70776,#70777,#70778,#70779,#70780,#70781,
#70782,#70783,#70784,#70785,#70786,#70787,#70788,#70789,#70790,#70791,#70792,
#70793,#70794,#70795,#70796,#70797,#70798,#70799,#70800,#70801,#70802,#70803,
#70804,#70805,#70806,#70807,#70808,#70809,#70810),.UNSPECIFIED.,.F.,.F.,
(4,3,3,3,3,3,3,3,3,3,3,3,3,3,3,3,3,3,3,3,3,3,4),(-0.937740963081735,-0.909444112452461,
-0.855149209379619,-0.831654357878427,-0.809449311278671,-0.761645733327119,
-0.730551867932484,-0.705074189312176,-0.633394121071644,-0.589005347555876,
-0.552912288548607,-0.535870541484316,-0.475136415046823,-0.416990908171079,
-0.376787680507578,-0.359453625478781,-0.285000662182822,-0.242554387543848,
-0.201877636725584,-0.176408609773167,-0.0995863267715526,-0.0229337643123042,
0.),.UNSPECIFIED.);
#907=B_SPLINE_CURVE_WITH_KNOTS('',3,(#70815,#70816,#70817,#70818,#70819,
#70820,#70821,#70822,#70823,#70824,#70825,#70826,#70827,#70828,#70829,#70830,
#70831,#70832,#70833,#70834,#70835,#70836,#70837,#70838,#70839,#70840,#70841,
#70842,#70843,#70844,#70845,#70846,#70847,#70848,#70849,#70850,#70851,#70852,
#70853,#70854,#70855,#70856,#70857,#70858,#70859,#70860,#70861,#70862,#70863,
#70864,#70865,#70866,#70867,#70868,#70869,#70870,#70871,#70872,#70873,#70874,
#70875,#70876,#70877,#70878,#70879,#70880,#70881),.UNSPECIFIED.,.F.,.F.,
(4,3,3,3,3,3,3,3,3,3,3,3,3,3,3,3,3,3,3,3,3,3,4),(-0.933975894023042,-0.900245581901252,
-0.841487335486281,-0.810148385431822,-0.789962965850525,-0.713494202946813,
-0.685815600115485,-0.669124534079921,-0.594769089731299,-0.522304386990161,
-0.504106714065163,-0.485285714178158,-0.430179610581482,-0.367158525801107,
-0.338157301636647,-0.316837385332554,-0.246631602421699,-0.209998276425139,
-0.170573737200308,-0.149754029067211,-0.0814335283124309,-0.0148091980626577,
0.),.UNSPECIFIED.);
#908=B_SPLINE_CURVE_WITH_KNOTS('',3,(#71486,#71487,#71488,#71489,#71490,
#71491,#71492,#71493,#71494,#71495,#71496,#71497,#71498,#71499,#71500,#71501),
 .UNSPECIFIED.,.F.,.F.,(4,3,3,3,3,4),(139.344958767167,139.853043970494,
140.851994284569,141.850944598644,142.849894912719,143.780223779293),
 .UNSPECIFIED.);
#909=B_SPLINE_CURVE_WITH_KNOTS('',3,(#71503,#71504,#71505,#71506,#71507,
#71508,#71509,#71510,#71511,#71512,#71513,#71514,#71515,#71516,#71517,#71518,
#71519,#71520,#71521,#71522,#71523,#71524,#71525,#71526,#71527,#71528,#71529,
#71530,#71531,#71532,#71533,#71534,#71535,#71536,#71537,#71538,#71539,#71540,
#71541,#71542,#71543,#71544,#71545,#71546,#71547,#71548,#71549,#71550,#71551,
#71552,#71553,#71554,#71555,#71556,#71557,#71558,#71559,#71560,#71561,#71562,
#71563,#71564,#71565,#71566,#71567,#71568,#71569),.UNSPECIFIED.,.F.,.F.,
(4,3,3,3,3,3,3,3,3,3,3,3,3,3,3,3,3,3,3,3,3,3,4),(-0.937740963081788,-0.9094441124525,
-0.855149214466471,-0.831654450328588,-0.809449338817702,-0.761644037980892,
-0.730548230053358,-0.705074381737659,-0.633394334161421,-0.589005671228396,
-0.552912642218538,-0.535870789585526,-0.475136415046854,-0.416990908171107,
-0.37678761967171,-0.359453594967343,-0.285000689052183,-0.242554387543867,
-0.201877627854406,-0.176408608557775,-0.099585852352597,-0.0229334512306372,
0.),.UNSPECIFIED.);
#910=B_SPLINE_CURVE_WITH_KNOTS('',3,(#71570,#71571,#71572,#71573,#71574,
#71575,#71576,#71577,#71578),.UNSPECIFIED.,.F.,.F.,(4,1,1,1,1,1,4),(10.3764180272042,
11.3067468937783,12.3056972078532,13.3046475219282,14.3035978360031,15.3025481500781,
15.7079632679489),.UNSPECIFIED.);
#911=B_SPLINE_CURVE_WITH_KNOTS('',3,(#71584,#71585,#71586,#71587,#71588,
#71589,#71590,#71591,#71592,#71593,#71594,#71595,#71596,#71597,#71598,#71599,
#71600,#71601,#71602,#71603,#71604,#71605,#71606,#71607,#71608,#71609,#71610,
#71611,#71612,#71613,#71614,#71615,#71616,#71617,#71618,#71619,#71620,#71621,
#71622,#71623,#71624,#71625,#71626,#71627,#71628,#71629,#71630,#71631,#71632,
#71633,#71634,#71635,#71636,#71637,#71638,#71639,#71640,#71641,#71642,#71643,
#71644,#71645,#71646,#71647,#71648,#71649,#71650),.UNSPECIFIED.,.F.,.F.,
(4,3,3,3,3,3,3,3,3,3,3,3,3,3,3,3,3,3,3,3,3,3,4),(-0.933975894023119,-0.900245581901347,
-0.841487335486366,-0.81014833836286,-0.789962871427875,-0.713494038275052,
-0.685815425544487,-0.669124316437155,-0.594768735347489,-0.522303851190798,
-0.504103096333425,-0.48528515314046,-0.430179610581495,-0.367160405393276,
-0.338159869684524,-0.316837865674906,-0.246632351097073,-0.209998276425132,
-0.170573792092408,-0.149754039276966,-0.0814335090852424,-0.0148090667643755,
0.),.UNSPECIFIED.);
#912=B_SPLINE_CURVE_WITH_KNOTS('',3,(#71653,#71654,#71655,#71656,#71657,
#71658,#71659,#71660,#71661),.UNSPECIFIED.,.F.,.F.,(4,1,1,1,1,1,4),(11.6147305479243,
12.1142057049618,12.6136808619992,13.6126311760742,14.6115814901491,15.6105318042241,
15.7079632679489),.UNSPECIFIED.);
#913=B_SPLINE_CURVE_WITH_KNOTS('',3,(#72266,#72267,#72268,#72269,#72270,
#72271,#72272,#72273,#72274,#72275,#72276,#72277,#72278,#72279,#72280,#72281),
 .UNSPECIFIED.,.F.,.F.,(4,3,3,3,3,4),(-145.846745854944,-145.347270697906,
-144.847795540869,-143.848845226794,-142.849894912719,-142.323309477976),
 .UNSPECIFIED.);
#914=B_SPLINE_CURVE_WITH_KNOTS('',3,(#73088,#73089,#73090,#73091,#73092,
#73093,#73094,#73095,#73096,#73097),.UNSPECIFIED.,.F.,.F.,(4,3,3,4),(-4.09293042013066,
-3.9801412930946,-2.98510596982095,-2.06863817490914),.UNSPECIFIED.);
#915=B_SPLINE_CURVE_WITH_KNOTS('',3,(#73100,#73101,#73102,#73103,#73104,
#73105,#73106),.UNSPECIFIED.,.F.,.F.,(4,3,4),(0.,0.995035323273648,1.11730040836815),
 .UNSPECIFIED.);
#916=B_SPLINE_CURVE_WITH_KNOTS('',3,(#73111,#73112,#73113,#73114,#73115,
#73116,#73117,#73118,#73119,#73120,#73121,#73122,#73123,#73124,#73125,#73126,
#73127,#73128,#73129,#73130,#73131,#73132),.UNSPECIFIED.,.F.,.F.,(4,3,3,
3,3,3,3,4),(-10.3761157273103,-9.9503532327365,-8.95531790946285,-7.9602825861892,
-6.96524726291555,-5.9702119396419,-4.97517661636825,-4.09293042013066),
 .UNSPECIFIED.);
#917=B_SPLINE_CURVE_WITH_KNOTS('',3,(#73133,#73134,#73135,#73136,#73137,
#73138,#73139,#73140,#73141,#73142,#73143,#73144,#73145,#73146,#73147,#73148,
#73149,#73150,#73151,#73152,#73153,#73154),.UNSPECIFIED.,.F.,.F.,(4,3,3,
3,3,3,3,4),(1.11730040836815,1.9900706465473,2.98510596982095,3.9801412930946,
4.97517661636825,5.9702119396419,6.96524726291555,7.40048571554773),
 .UNSPECIFIED.);
#918=B_SPLINE_CURVE_WITH_KNOTS('',3,(#73159,#73160,#73161,#73162,#73163,
#73164,#73165,#73166,#73167,#73168,#73169,#73170,#73171,#73172,#73173,#73174,
#73175,#73176,#73177,#73178,#73179,#73180),.UNSPECIFIED.,.F.,.F.,(4,3,3,
3,3,3,3,4),(-16.6593010344898,-15.9205651723784,-14.9255298491048,-13.9304945258311,
-12.9354592025574,-11.9404238792838,-10.9453885560101,-10.3761157273103),
 .UNSPECIFIED.);
#919=B_SPLINE_CURVE_WITH_KNOTS('',3,(#73181,#73182,#73183,#73184,#73185,
#73186,#73187,#73188,#73189,#73190,#73191,#73192,#73193,#73194,#73195,#73196,
#73197,#73198,#73199,#73200,#73201,#73202),.UNSPECIFIED.,.F.,.F.,(4,3,3,
3,3,3,3,4),(7.40048571554773,7.9602825861892,8.95531790946285,9.95035323273651,
10.9453885560102,11.9404238792838,12.9354592025575,13.6836710227273),
 .UNSPECIFIED.);
#920=B_SPLINE_CURVE_WITH_KNOTS('',3,(#73207,#73208,#73209,#73210,#73211,
#73212,#73213,#73214,#73215,#73216,#73217,#73218,#73219,#73220,#73221,#73222,
#73223,#73224,#73225,#73226,#73227,#73228,#73229,#73230,#73231),
 .UNSPECIFIED.,.F.,.F.,(4,3,3,3,3,3,3,3,4),(-22.9424863416694,-22.885812435294,
-21.8907771120203,-20.8957417887467,-19.900706465473,-18.9056711421993,
-17.9106358189257,-16.9156004956521,-16.6593010344898),.UNSPECIFIED.);
#921=B_SPLINE_CURVE_WITH_KNOTS('',3,(#73232,#73233,#73234,#73235,#73236,
#73237,#73238,#73239,#73240,#73241,#73242,#73243,#73244,#73245,#73246,#73247,
#73248,#73249,#73250,#73251,#73252,#73253,#73254,#73255,#73256),
 .UNSPECIFIED.,.F.,.F.,(4,3,3,3,3,3,3,3,4),(13.6836710227273,13.9304945258311,
14.9255298491048,15.9205651723784,16.9156004956521,17.9106358189257,18.9056711421993,
19.900706465473,19.9668563299069),.UNSPECIFIED.);
#922=B_SPLINE_CURVE_WITH_KNOTS('',3,(#73261,#73262,#73263,#73264,#73265,
#73266,#73267,#73268,#73269,#73270,#73271,#73272,#73273,#73274,#73275,#73276,
#73277,#73278,#73279,#73280,#73281,#73282),.UNSPECIFIED.,.F.,.F.,(4,3,3,
3,3,3,3,4),(-29.225671648849,-28.8560243749359,-27.8609890516622,-26.8659537283885,
-25.8709184051149,-24.8758830818412,-23.8808477585676,-22.9424863416694),
 .UNSPECIFIED.);
#923=B_SPLINE_CURVE_WITH_KNOTS('',3,(#73283,#73284,#73285,#73286,#73287,
#73288,#73289,#73290,#73291,#73292,#73293,#73294,#73295,#73296,#73297,#73298,
#73299,#73300,#73301,#73302,#73303,#73304),.UNSPECIFIED.,.F.,.F.,(4,3,3,
3,3,3,3,4),(19.9668563299069,20.8957417887466,21.8907771120203,22.8858124352939,
23.8808477585676,24.8758830818412,25.8709184051149,26.2500416370865),
 .UNSPECIFIED.);
#924=B_SPLINE_CURVE_WITH_KNOTS('',3,(#73309,#73310,#73311,#73312,#73313,
#73314,#73315,#73316,#73317,#73318,#73319,#73320,#73321,#73322,#73323,#73324,
#73325,#73326,#73327,#73328,#73329,#73330),.UNSPECIFIED.,.F.,.F.,(4,3,3,
3,3,3,3,4),(-35.5088569560286,-34.8262363145777,-33.8312009913041,-32.8361656680304,
-31.8411303447568,-30.8460950214831,-29.8510596982095,-29.225671648849),
 .UNSPECIFIED.);
#925=B_SPLINE_CURVE_WITH_KNOTS('',3,(#73331,#73332,#73333,#73334,#73335,
#73336,#73337,#73338,#73339,#73340,#73341,#73342,#73343,#73344,#73345,#73346,
#73347,#73348,#73349,#73350,#73351,#73352),.UNSPECIFIED.,.F.,.F.,(4,3,3,
3,3,3,3,4),(26.2500416370865,26.8659537283885,27.8609890516622,28.8560243749358,
29.8510596982095,30.8460950214831,31.8411303447568,32.5332269442661),
 .UNSPECIFIED.);
#926=B_SPLINE_CURVE_WITH_KNOTS('',3,(#73357,#73358,#73359,#73360,#73361,
#73362,#73363,#73364,#73365,#73366,#73367,#73368,#73369,#73370,#73371,#73372,
#73373,#73374,#73375,#73376,#73377,#73378),.UNSPECIFIED.,.F.,.F.,(4,3,3,
3,3,3,3,4),(-41.7920422632082,-40.7964482542196,-39.801412930946,-38.8063776076723,
-37.8113422843987,-36.8163069611251,-35.8212716378514,-35.5088569560286),
 .UNSPECIFIED.);
#927=B_SPLINE_CURVE_WITH_KNOTS('',3,(#73379,#73380,#73381,#73382,#73383,
#73384,#73385,#73386,#73387,#73388,#73389,#73390,#73391,#73392,#73393,#73394,
#73395,#73396,#73397,#73398,#73399,#73400,#73401,#73402,#73403),
 .UNSPECIFIED.,.F.,.F.,(4,3,3,3,3,3,3,3,4),(32.5332269442661,32.8361656680304,
33.8312009913041,34.8262363145777,35.8212716378514,36.816306961125,37.8113422843987,
38.8063776076723,38.8164122514457),.UNSPECIFIED.);
#928=B_SPLINE_CURVE_WITH_KNOTS('',3,(#73408,#73409,#73410,#73411,#73412,
#73413,#73414,#73415,#73416,#73417,#73418,#73419,#73420,#73421,#73422,#73423,
#73424,#73425,#73426,#73427,#73428,#73429),.UNSPECIFIED.,.F.,.F.,(4,3,3,
3,3,3,3,4),(-48.0752275703878,-47.7616955171352,-46.7666601938616,-45.7716248705879,
-44.7765895473142,-43.7815542240406,-42.7865189007669,-41.7920422632082),
 .UNSPECIFIED.);
#929=B_SPLINE_CURVE_WITH_KNOTS('',3,(#73430,#73431,#73432,#73433,#73434,
#73435,#73436,#73437,#73438,#73439,#73440,#73441,#73442,#73443,#73444,#73445,
#73446,#73447,#73448,#73449,#73450,#73451),.UNSPECIFIED.,.F.,.F.,(4,3,3,
3,3,3,3,4),(38.8164122514457,39.801412930946,40.7964482542196,41.7914835774933,
42.7865189007669,43.7815542240406,44.7765895473143,45.0995975586253),
 .UNSPECIFIED.);
#930=B_SPLINE_CURVE_WITH_KNOTS('',3,(#73456,#73457,#73458,#73459,#73460,
#73461,#73462,#73463,#73464,#73465,#73466,#73467,#73468,#73469,#73470,#73471,
#73472,#73473,#73474,#73475,#73476,#73477),.UNSPECIFIED.,.F.,.F.,(4,3,3,
3,3,3,3,4),(-54.3584128775674,-53.7319074567771,-52.7368721335034,-51.7418368102298,
-50.7468014869562,-49.7517661636825,-48.7567308404089,-48.0752275703878),
 .UNSPECIFIED.);
#931=B_SPLINE_CURVE_WITH_KNOTS('',3,(#73478,#73479,#73480,#73481,#73482,
#73483,#73484,#73485,#73486,#73487,#73488,#73489,#73490,#73491,#73492,#73493,
#73494,#73495,#73496,#73497,#73498,#73499),.UNSPECIFIED.,.F.,.F.,(4,3,3,
3,3,3,3,4),(45.0995975586253,45.7716248705879,46.7666601938615,47.7616955171352,
48.7567308404088,49.7517661636825,50.7468014869561,51.3827828658048),
 .UNSPECIFIED.);
#932=B_SPLINE_CURVE_WITH_KNOTS('',3,(#73504,#73505,#73506,#73507,#73508,
#73509,#73510,#73511,#73512,#73513,#73514,#73515,#73516,#73517,#73518,#73519,
#73520,#73521,#73522,#73523,#73524,#73525),.UNSPECIFIED.,.F.,.F.,(4,3,3,
3,3,3,3,4),(-60.641598184747,-59.702119396419,-58.7070840731453,-57.7120487498717,
-56.7170134265981,-55.7219781033244,-54.7269427800508,-54.3584128775674),
 .UNSPECIFIED.);
#933=B_SPLINE_CURVE_WITH_KNOTS('',3,(#73526,#73527,#73528,#73529,#73530,
#73531,#73532,#73533,#73534,#73535,#73536,#73537,#73538,#73539,#73540,#73541,
#73542,#73543,#73544,#73545,#73546,#73547),.UNSPECIFIED.,.F.,.F.,(4,3,3,
3,3,3,3,4),(51.3827828658048,51.7418368102298,52.7368721335034,53.7319074567771,
54.7269427800507,55.7219781033244,56.717013426598,57.6659681729844),
 .UNSPECIFIED.);
#934=B_SPLINE_CURVE_WITH_KNOTS('',3,(#73552,#73553,#73554,#73555,#73556,
#73557,#73558,#73559,#73560,#73561,#73562,#73563,#73564,#73565,#73566,#73567,
#73568,#73569,#73570,#73571,#73572,#73573,#73574,#73575,#73576),
 .UNSPECIFIED.,.F.,.F.,(4,3,3,3,3,3,3,3,4),(-66.9247834919266,-66.6673666593345,
-65.6723313360609,-64.6772960127873,-63.6822606895136,-62.6872253662399,
-61.6921900429663,-60.6971547196927,-60.641598184747),.UNSPECIFIED.);
#935=B_SPLINE_CURVE_WITH_KNOTS('',3,(#73577,#73578,#73579,#73580,#73581,
#73582,#73583,#73584,#73585,#73586,#73587,#73588,#73589,#73590,#73591,#73592,
#73593,#73594,#73595,#73596,#73597,#73598,#73599,#73600,#73601),
 .UNSPECIFIED.,.F.,.F.,(4,3,3,3,3,3,3,3,4),(57.6659681729844,57.7120487498717,
58.7070840731453,59.702119396419,60.6971547196927,61.6921900429663,62.68722536624,
63.6822606895136,63.949153480164),.UNSPECIFIED.);
#936=B_SPLINE_CURVE_WITH_KNOTS('',3,(#73606,#73607,#73608,#73609,#73610,
#73611,#73612,#73613,#73614,#73615,#73616,#73617,#73618,#73619,#73620,#73621,
#73622,#73623,#73624,#73625,#73626,#73627),.UNSPECIFIED.,.F.,.F.,(4,3,3,
3,3,3,3,4),(-73.2079687991062,-72.6375785989764,-71.6425432757028,-70.6475079524291,
-69.6524726291555,-68.6574373058818,-67.6624019826082,-66.9247834919266),
 .UNSPECIFIED.);
#937=B_SPLINE_CURVE_WITH_KNOTS('',3,(#73628,#73629,#73630,#73631,#73632,
#73633,#73634,#73635,#73636,#73637,#73638,#73639,#73640,#73641,#73642,#73643,
#73644,#73645,#73646,#73647,#73648,#73649),.UNSPECIFIED.,.F.,.F.,(4,3,3,
3,3,3,3,4),(63.949153480164,64.6772960127873,65.6723313360609,66.6673666593345,
67.6624019826082,68.6574373058818,69.6524726291555,70.2323387873436),
 .UNSPECIFIED.);
#938=B_SPLINE_CURVE_WITH_KNOTS('',3,(#73654,#73655,#73656,#73657,#73658,
#73659,#73660,#73661,#73662,#73663,#73664,#73665,#73666,#73667,#73668,#73669,
#73670,#73671,#73672,#73673,#73674,#73675),.UNSPECIFIED.,.F.,.F.,(4,3,3,
3,3,3,3,4),(-79.4911541062857,-78.6077905386183,-77.6127552153447,-76.6177198920711,
-75.6226845687974,-74.6276492455237,-73.6326139222501,-73.2079687991062),
 .UNSPECIFIED.);
#939=B_SPLINE_CURVE_WITH_KNOTS('',3,(#73676,#73677,#73678,#73679,#73680,
#73681,#73682,#73683,#73684,#73685,#73686,#73687,#73688,#73689,#73690,#73691,
#73692,#73693,#73694,#73695,#73696,#73697),.UNSPECIFIED.,.F.,.F.,(4,3,3,
3,3,3,3,4),(70.2323387873436,70.6475079524291,71.6425432757028,72.6375785989764,
73.6326139222501,74.6276492455237,75.6226845687974,76.5155240945232),
 .UNSPECIFIED.);
#940=B_SPLINE_CURVE_WITH_KNOTS('',3,(#73702,#73703,#73704,#73705,#73706,
#73707,#73708,#73709,#73710,#73711,#73712,#73713,#73714,#73715,#73716,#73717,
#73718,#73719,#73720,#73721,#73722,#73723,#73724,#73725,#73726),
 .UNSPECIFIED.,.F.,.F.,(4,3,3,3,3,3,3,3,4),(-85.7743394134653,-85.5730378015339,
-84.5780024782602,-83.5829671549866,-82.587931831713,-81.5928965084393,
-80.5978611851656,-79.602825861892,-79.4911541062857),.UNSPECIFIED.);
#941=B_SPLINE_CURVE_WITH_KNOTS('',3,(#73727,#73728,#73729,#73730,#73731,
#73732,#73733,#73734,#73735,#73736,#73737,#73738,#73739,#73740,#73741,#73742,
#73743,#73744,#73745,#73746,#73747,#73748,#73749,#73750,#73751),
 .UNSPECIFIED.,.F.,.F.,(4,3,3,3,3,3,3,3,4),(76.5155240945232,76.617719892071,
77.6127552153447,78.6077905386183,79.602825861892,80.5978611851656,81.5928965084393,
82.5879318317129,82.7987094017028),.UNSPECIFIED.);
#942=B_SPLINE_CURVE_WITH_KNOTS('',3,(#73756,#73757,#73758,#73759,#73760,
#73761,#73762,#73763,#73764,#73765,#73766,#73767,#73768,#73769,#73770,#73771,
#73772,#73773,#73774,#73775,#73776,#73777),.UNSPECIFIED.,.F.,.F.,(4,3,3,
3,3,3,3,4),(-92.0575247206449,-91.5432497411758,-90.5482144179021,-89.5531790946285,
-88.5581437713548,-87.5631084480812,-86.5680731248076,-85.7743394134653),
 .UNSPECIFIED.);
#943=B_SPLINE_CURVE_WITH_KNOTS('',3,(#73778,#73779,#73780,#73781,#73782,
#73783,#73784,#73785,#73786,#73787,#73788,#73789,#73790,#73791,#73792,#73793,
#73794,#73795,#73796,#73797,#73798,#73799),.UNSPECIFIED.,.F.,.F.,(4,3,3,
3,3,3,3,4),(82.7987094017028,83.5829671549866,84.5780024782602,85.5730378015339,
86.5680731248075,87.5631084480812,88.5581437713548,89.0818947088824),
 .UNSPECIFIED.);
#944=B_SPLINE_CURVE_WITH_KNOTS('',3,(#73804,#73805,#73806,#73807,#73808,
#73809,#73810,#73811,#73812,#73813,#73814,#73815,#73816,#73817,#73818,#73819,
#73820,#73821,#73822,#73823,#73824,#73825),.UNSPECIFIED.,.F.,.F.,(4,3,3,
3,3,3,3,4),(-98.3407100278245,-97.5134616808177,-96.518426357544,-95.5233910342704,
-94.5283557109967,-93.5333203877231,-92.5382850644494,-92.0575247206449),
 .UNSPECIFIED.);
#945=B_SPLINE_CURVE_WITH_KNOTS('',3,(#73826,#73827,#73828,#73829,#73830,
#73831,#73832,#73833,#73834,#73835,#73836,#73837,#73838,#73839,#73840,#73841,
#73842,#73843,#73844,#73845,#73846,#73847),.UNSPECIFIED.,.F.,.F.,(4,3,3,
3,3,3,3,4),(89.0818947088824,89.5531790946285,90.5482144179021,91.5432497411758,
92.5382850644494,93.5333203877231,94.5283557109967,95.365080016062),
 .UNSPECIFIED.);
#946=B_SPLINE_CURVE_WITH_KNOTS('',3,(#73852,#73853,#73854,#73855,#73856,
#73857,#73858,#73859,#73860,#73861,#73862,#73863,#73864,#73865,#73866,#73867,
#73868,#73869,#73870,#73871,#73872,#73873,#73874,#73875,#73876),
 .UNSPECIFIED.,.F.,.F.,(4,3,3,3,3,3,3,3,4),(-104.623895335004,-104.478708943733,
-103.48367362046,-102.488638297186,-101.493602973912,-100.498567650639,
-99.503532327365,-98.5084970040914,-98.3407100278245),.UNSPECIFIED.);
#947=B_SPLINE_CURVE_WITH_KNOTS('',3,(#73877,#73878,#73879,#73880,#73881,
#73882,#73883,#73884,#73885,#73886,#73887,#73888,#73889,#73890,#73891,#73892,
#73893,#73894,#73895,#73896,#73897,#73898,#73899,#73900,#73901),
 .UNSPECIFIED.,.F.,.F.,(4,3,3,3,3,3,3,3,4),(95.365080016062,95.5233910342704,
96.518426357544,97.5134616808177,98.5084970040913,99.503532327365,100.498567650639,
101.493602973912,101.648265323242),.UNSPECIFIED.);
#948=B_SPLINE_CURVE_WITH_KNOTS('',3,(#73906,#73907,#73908,#73909,#73910,
#73911,#73912,#73913,#73914,#73915,#73916,#73917,#73918,#73919,#73920,#73921,
#73922,#73923,#73924,#73925,#73926,#73927),.UNSPECIFIED.,.F.,.F.,(4,3,3,
3,3,3,3,4),(-110.907080642184,-110.448920883375,-109.453885560102,-108.458850236828,
-107.463814913554,-106.468779590281,-105.473744267007,-104.623895335004),
 .UNSPECIFIED.);
#949=B_SPLINE_CURVE_WITH_KNOTS('',3,(#73928,#73929,#73930,#73931,#73932,
#73933,#73934,#73935,#73936,#73937,#73938,#73939,#73940,#73941,#73942,#73943,
#73944,#73945,#73946,#73947,#73948,#73949),.UNSPECIFIED.,.F.,.F.,(4,3,3,
3,3,3,3,4),(101.648265323242,102.488638297186,103.48367362046,104.478708943733,
105.473744267007,106.468779590281,107.463814913554,107.931450630421),
 .UNSPECIFIED.);
#950=B_SPLINE_CURVE_WITH_KNOTS('',3,(#73954,#73955,#73956,#73957,#73958,
#73959,#73960,#73961,#73962,#73963,#73964,#73965,#73966,#73967,#73968,#73969,
#73970,#73971,#73972,#73973,#73974,#73975),.UNSPECIFIED.,.F.,.F.,(4,3,3,
3,3,3,3,4),(-117.190265949363,-116.419132823017,-115.424097499743,-114.42906217647,
-113.434026853196,-112.438991529922,-111.443956206649,-110.907080642184),
 .UNSPECIFIED.);
#951=B_SPLINE_CURVE_WITH_KNOTS('',3,(#73976,#73977,#73978,#73979,#73980,
#73981,#73982,#73983,#73984,#73985,#73986,#73987,#73988,#73989,#73990,#73991,
#73992,#73993,#73994,#73995,#73996,#73997),.UNSPECIFIED.,.F.,.F.,(4,3,3,
3,3,3,3,4),(107.931450630421,108.458850236828,109.453885560101,110.448920883375,
111.443956206649,112.438991529922,113.434026853196,114.214635937601),
 .UNSPECIFIED.);
#952=B_SPLINE_CURVE_WITH_KNOTS('',3,(#74004,#74005,#74006,#74007,#74008,
#74009,#74010,#74011,#74012,#74013,#74014,#74015,#74016,#74017,#74018,#74019,
#74020,#74021,#74022,#74023,#74024,#74025),.UNSPECIFIED.,.F.,.F.,(4,3,3,
3,3,3,3,4),(-123.384380085933,-122.389344762659,-121.394309439385,-120.399274116112,
-119.404238792838,-118.409203469564,-117.414168146291,-117.190265949363),
 .UNSPECIFIED.);
#953=B_SPLINE_CURVE_WITH_KNOTS('',3,(#74026,#74027,#74028,#74029,#74030,
#74031,#74032,#74033,#74034,#74035,#74036,#74037,#74038,#74039,#74040,#74041,
#74042,#74043,#74044,#74045,#74046,#74047,#74048,#74049,#74050),
 .UNSPECIFIED.,.F.,.F.,(4,3,3,3,3,3,3,3,4),(114.214635937601,114.42906217647,
115.424097499743,116.419132823017,117.414168146291,118.409203469564,119.404238792838,
120.399274116112,120.49782124478),.UNSPECIFIED.);
#954=B_SPLINE_CURVE_WITH_KNOTS('',3,(#74056,#74057,#74058,#74059,#74060,
#74061,#74062,#74063),.UNSPECIFIED.,.F.,.F.,(4,1,1,1,1,4),(128.805298797182,
129.029200994109,130.024236317383,131.019271640656,132.01430696393,132.930774758842),
 .UNSPECIFIED.);
#955=B_SPLINE_CURVE_WITH_KNOTS('',3,(#74066,#74067,#74068,#74069,#74070,
#74071),.UNSPECIFIED.,.F.,.F.,(4,1,1,4),(128.805298797182,129.701786991786,
130.69682231506,131.691857638334),.UNSPECIFIED.);
#956=B_SPLINE_CURVE_WITH_KNOTS('',3,(#74076,#74077,#74078,#74079,#74080,
#74081,#74082,#74083,#74084,#74085),.UNSPECIFIED.,.F.,.F.,(4,1,1,1,1,1,
1,4),(122.522113490002,123.058989054467,124.054024377741,125.049059701014,
126.044095024288,127.039130347562,128.034165670835,128.805298797182),
 .UNSPECIFIED.);
#957=B_SPLINE_CURVE_WITH_KNOTS('',3,(#74086,#74087,#74088,#74089,#74090,
#74091,#74092,#74093,#74094,#74095,#74096),.UNSPECIFIED.,.F.,.F.,(4,1,1,
1,1,1,1,1,4),(122.522113490002,122.736539728871,123.731575052144,124.726610375418,
125.721645698692,126.716681021965,127.711716345239,128.706751668513,128.805298797182),
 .UNSPECIFIED.);
#958=B_SPLINE_CURVE_WITH_KNOTS('',3,(#74101,#74102,#74103,#74104,#74105,
#74106,#74107,#74108,#74109,#74110),.UNSPECIFIED.,.F.,.F.,(4,1,1,1,1,1,
1,4),(116.238928182822,117.088777114825,118.083812438099,119.078847761372,
120.073883084646,121.06891840792,122.063953731193,122.522113490002),
 .UNSPECIFIED.);
#959=B_SPLINE_CURVE_WITH_KNOTS('',3,(#74111,#74112,#74113,#74114,#74115,
#74116,#74117,#74118,#74119,#74120),.UNSPECIFIED.,.F.,.F.,(4,1,1,1,1,1,
1,4),(116.238928182822,116.766327789229,117.761363112503,118.756398435776,
119.75143375905,120.746469082323,121.741504405597,122.522113490002),
 .UNSPECIFIED.);
#960=B_SPLINE_CURVE_WITH_KNOTS('',3,(#74125,#74126,#74127,#74128,#74129,
#74130,#74131,#74132,#74133,#74134,#74135),.UNSPECIFIED.,.F.,.F.,(4,1,1,
1,1,1,1,1,4),(109.955742875643,110.12352985191,111.118565175183,112.113600498457,
113.108635821731,114.103671145004,115.098706468278,116.093741791551,116.238928182822),
 .UNSPECIFIED.);
#961=B_SPLINE_CURVE_WITH_KNOTS('',3,(#74136,#74137,#74138,#74139,#74140,
#74141,#74142,#74143,#74144,#74145),.UNSPECIFIED.,.F.,.F.,(4,1,1,1,1,1,
1,4),(109.955742875643,110.796115849587,111.791151172861,112.786186496134,
113.781221819408,114.776257142682,115.771292465955,116.238928182822),
 .UNSPECIFIED.);
#962=B_SPLINE_CURVE_WITH_KNOTS('',3,(#74150,#74151,#74152,#74153,#74154,
#74155,#74156,#74157,#74158,#74159),.UNSPECIFIED.,.F.,.F.,(4,1,1,1,1,1,
1,4),(103.672557568463,104.153317912268,105.148353235541,106.143388558815,
107.138423882089,108.133459205362,109.128494528636,109.955742875643),
 .UNSPECIFIED.);
#963=B_SPLINE_CURVE_WITH_KNOTS('',3,(#74160,#74161,#74162,#74163,#74164,
#74165,#74166,#74167,#74168,#74169,#74170),.UNSPECIFIED.,.F.,.F.,(4,1,1,
1,1,1,1,1,4),(103.672557568463,103.830868586671,104.825903909945,105.820939233219,
106.815974556492,107.811009879766,108.80604520304,109.801080526313,109.955742875643),
 .UNSPECIFIED.);
#964=B_SPLINE_CURVE_WITH_KNOTS('',3,(#74175,#74176,#74177,#74178,#74179,
#74180,#74181,#74182,#74183,#74184),.UNSPECIFIED.,.F.,.F.,(4,1,1,1,1,1,
1,4),(97.3893722612836,98.1831059726258,99.1781412958994,100.173176619173,
101.168211942447,102.16324726572,103.158282588994,103.672557568463),
 .UNSPECIFIED.);
#965=B_SPLINE_CURVE_WITH_KNOTS('',3,(#74185,#74186,#74187,#74188,#74189,
#74190,#74191,#74192,#74193,#74194),.UNSPECIFIED.,.F.,.F.,(4,1,1,1,1,1,
1,4),(97.3893722612835,97.8606566470295,98.8556919703032,99.8507272935768,
100.84576261685,101.840797940124,102.835833263398,103.672557568463),
 .UNSPECIFIED.);
#966=B_SPLINE_CURVE_WITH_KNOTS('',3,(#74199,#74200,#74201,#74202,#74203,
#74204,#74205,#74206,#74207,#74208,#74209),.UNSPECIFIED.,.F.,.F.,(4,1,1,
1,1,1,1,1,4),(91.106186954104,91.2178587097102,92.2128940329839,93.2079293562575,
94.2029646795312,95.1980000028048,96.1930353260785,97.1880706493521,97.3893722612836),
 .UNSPECIFIED.);
#967=B_SPLINE_CURVE_WITH_KNOTS('',3,(#74210,#74211,#74212,#74213,#74214,
#74215,#74216,#74217,#74218,#74219),.UNSPECIFIED.,.F.,.F.,(4,1,1,1,1,1,
1,4),(91.1061869541039,91.8904447073876,92.8854800306613,93.8805153539349,
94.8755506772086,95.8705860004822,96.8656213237559,97.3893722612835),
 .UNSPECIFIED.);
#968=B_SPLINE_CURVE_WITH_KNOTS('',3,(#74224,#74225,#74226,#74227,#74228,
#74229,#74230,#74231,#74232,#74233),.UNSPECIFIED.,.F.,.F.,(4,1,1,1,1,1,
1,4),(84.8230016469244,85.2476467700683,86.242682093342,87.2377174166156,
88.2327527398893,89.2277880631629,90.2228233864366,91.106186954104),
 .UNSPECIFIED.);
#969=B_SPLINE_CURVE_WITH_KNOTS('',3,(#74234,#74235,#74236,#74237,#74238,
#74239,#74240,#74241,#74242,#74243,#74244),.UNSPECIFIED.,.F.,.F.,(4,1,1,
1,1,1,1,1,4),(84.8230016469244,84.9251974444721,85.9202327677457,86.9152680910194,
87.910303414293,88.9053387375667,89.9003740608403,90.895409384114,91.1061869541039),
 .UNSPECIFIED.);
#970=B_SPLINE_CURVE_WITH_KNOTS('',3,(#74249,#74250,#74251,#74252,#74253,
#74254,#74255,#74256,#74257,#74258),.UNSPECIFIED.,.F.,.F.,(4,1,1,1,1,1,
1,4),(78.5398163397448,79.2774348304264,80.2724701537001,81.2675054769737,
82.2625408002474,83.257576123521,84.2526114467947,84.8230016469244),
 .UNSPECIFIED.);
#971=B_SPLINE_CURVE_WITH_KNOTS('',3,(#74259,#74260,#74261,#74262,#74263,
#74264,#74265,#74266,#74267,#74268),.UNSPECIFIED.,.F.,.F.,(4,1,1,1,1,1,
1,4),(78.5398163397448,78.9549855048302,79.9500208281038,80.9450561513775,
81.9400914746511,82.9351267979248,83.9301621211984,84.8230016469244),
 .UNSPECIFIED.);
#972=B_SPLINE_CURVE_WITH_KNOTS('',3,(#74273,#74274,#74275,#74276,#74277,
#74278,#74279,#74280,#74281,#74282,#74283),.UNSPECIFIED.,.F.,.F.,(4,1,1,
1,1,1,1,1,4),(72.2566310325652,72.3121875675109,73.3072228907845,74.3022582140582,
75.2972935373318,76.2923288606055,77.2873641838791,78.2823995071528,78.5398163397448),
 .UNSPECIFIED.);
#973=B_SPLINE_CURVE_WITH_KNOTS('',3,(#74284,#74285,#74286,#74287,#74288,
#74289,#74290,#74291,#74292,#74293),.UNSPECIFIED.,.F.,.F.,(4,1,1,1,1,1,
1,4),(72.2566310325652,72.9847735651883,73.9798088884619,74.9748442117356,
75.9698795350092,76.9649148582829,77.9599501815565,78.5398163397448),
 .UNSPECIFIED.);
#974=B_SPLINE_CURVE_WITH_KNOTS('',3,(#74298,#74299,#74300,#74301,#74302,
#74303,#74304,#74305,#74306,#74307),.UNSPECIFIED.,.F.,.F.,(4,1,1,1,1,1,
1,4),(65.9734457253856,66.341975627869,67.3370109511426,68.3320462744163,
69.3270815976899,70.3221169209636,71.3171522442372,72.2566310325652),
 .UNSPECIFIED.);
#975=B_SPLINE_CURVE_WITH_KNOTS('',3,(#74308,#74309,#74310,#74311,#74312,
#74313,#74314,#74315,#74316,#74317,#74318),.UNSPECIFIED.,.F.,.F.,(4,1,1,
1,1,1,1,1,4),(65.9734457253856,66.0195263022727,67.0145616255464,68.00959694882,
69.0046322720937,69.9996675953673,70.994702918641,71.9897382419146,72.2566310325652),
 .UNSPECIFIED.);
#976=B_SPLINE_CURVE_WITH_KNOTS('',3,(#74323,#74324,#74325,#74326,#74327,
#74328,#74329,#74330,#74331,#74332),.UNSPECIFIED.,.F.,.F.,(4,1,1,1,1,1,
1,4),(59.690260418206,60.3717636882271,61.3667990115007,62.3618343347744,
63.356869658048,64.3519049813217,65.3469403045953,65.9734457253856),
 .UNSPECIFIED.);
#977=B_SPLINE_CURVE_WITH_KNOTS('',3,(#74333,#74334,#74335,#74336,#74337,
#74338,#74339,#74340,#74341,#74342),.UNSPECIFIED.,.F.,.F.,(4,1,1,1,1,1,
1,4),(59.690260418206,60.0493143626308,61.0443496859045,62.0393850091781,
63.0344203324518,64.0294556557254,65.0244909789991,65.9734457253856),
 .UNSPECIFIED.);
#978=B_SPLINE_CURVE_WITH_KNOTS('',3,(#74347,#74348,#74349,#74350,#74351,
#74352,#74353,#74354,#74355,#74356),.UNSPECIFIED.,.F.,.F.,(4,1,1,1,1,1,
1,4),(53.4070751110264,54.4015517485852,55.3965870718588,56.3916223951325,
57.3866577184061,58.3816930416798,59.3767283649534,59.690260418206),
 .UNSPECIFIED.);
#979=B_SPLINE_CURVE_WITH_KNOTS('',3,(#74357,#74358,#74359,#74360,#74361,
#74362,#74363,#74364,#74365,#74366),.UNSPECIFIED.,.F.,.F.,(4,1,1,1,1,1,
1,4),(53.4070751110264,54.0791024229889,55.0741377462626,56.0691730695362,
57.0642083928099,58.0592437160835,59.0542790393572,59.690260418206),
 .UNSPECIFIED.);
#980=B_SPLINE_CURVE_WITH_KNOTS('',3,(#74371,#74372,#74373,#74374,#74375,
#74376,#74377,#74378,#74379,#74380,#74381),.UNSPECIFIED.,.F.,.F.,(4,1,1,
1,1,1,1,1,4),(47.1238898038468,47.4363044856696,48.4313398089433,49.4263751322169,
50.4214104554906,51.4164457787642,52.4114811020379,53.4065164253115,53.4070751110264),
 .UNSPECIFIED.);
#981=B_SPLINE_CURVE_WITH_KNOTS('',3,(#74382,#74383,#74384,#74385,#74386,
#74387,#74388,#74389,#74390,#74391),.UNSPECIFIED.,.F.,.F.,(4,1,1,1,1,1,
1,4),(47.1238898038468,48.108890483347,49.1039258066207,50.0989611298943,
51.093996453168,52.0890317764416,53.0840670997153,53.4070751110264),
 .UNSPECIFIED.);
#982=B_SPLINE_CURVE_WITH_KNOTS('',3,(#74396,#74397,#74398,#74399,#74400,
#74401,#74402,#74403,#74404,#74405),.UNSPECIFIED.,.F.,.F.,(4,1,1,1,1,1,
1,4),(40.8407044966672,41.4660925460277,42.4611278693014,43.456163192575,
44.4511985158487,45.4462338391223,46.441269162396,47.1238898038468),
 .UNSPECIFIED.);
#983=B_SPLINE_CURVE_WITH_KNOTS('',3,(#74406,#74407,#74408,#74409,#74410,
#74411,#74412,#74413,#74414,#74415,#74416),.UNSPECIFIED.,.F.,.F.,(4,1,1,
1,1,1,1,1,4),(40.8407044966672,41.1436432204315,42.1386785437051,43.1337138669788,
44.1287491902524,45.1237845135261,46.1188198367997,47.1138551600734,47.1238898038468),
 .UNSPECIFIED.);
#984=B_SPLINE_CURVE_WITH_KNOTS('',3,(#74421,#74422,#74423,#74424,#74425,
#74426,#74427,#74428,#74429,#74430),.UNSPECIFIED.,.F.,.F.,(4,1,1,1,1,1,
1,4),(34.5575191894877,35.4958806063858,36.4909159296595,37.4859512529331,
38.4809865762068,39.4760218994804,40.4710572227541,40.8407044966672),
 .UNSPECIFIED.);
#985=B_SPLINE_CURVE_WITH_KNOTS('',3,(#74431,#74432,#74433,#74434,#74435,
#74436,#74437,#74438,#74439,#74440),.UNSPECIFIED.,.F.,.F.,(4,1,1,1,1,1,
1,4),(34.5575191894876,35.1734312807896,36.1684666040632,37.1635019273369,
38.1585372506105,39.1535725738842,40.1486078971578,40.8407044966672),
 .UNSPECIFIED.);
#986=B_SPLINE_CURVE_WITH_KNOTS('',3,(#74445,#74446,#74447,#74448,#74449,
#74450,#74451,#74452,#74453,#74454,#74455),.UNSPECIFIED.,.F.,.F.,(4,1,1,
1,1,1,1,1,4),(28.2743338823081,28.5306333434703,29.5256686667439,30.5207039900176,
31.5157393132912,32.5107746365649,33.5058099598385,34.5008452831122,34.5575191894877),
 .UNSPECIFIED.);
#987=B_SPLINE_CURVE_WITH_KNOTS('',3,(#74456,#74457,#74458,#74459,#74460,
#74461,#74462,#74463,#74464,#74465),.UNSPECIFIED.,.F.,.F.,(4,1,1,1,1,1,
1,4),(28.274333882308,29.2032193411477,30.1982546644213,31.193289987695,
32.1883253109686,33.1833606342423,34.1783959575159,34.5575191894876),
 .UNSPECIFIED.);
#988=B_SPLINE_CURVE_WITH_KNOTS('',3,(#74470,#74471,#74472,#74473,#74474,
#74475,#74476,#74477,#74478,#74479),.UNSPECIFIED.,.F.,.F.,(4,1,1,1,1,1,
1,4),(21.9911485751285,22.5604214038284,23.555456727102,24.5504920503757,
25.5455273736493,26.540562696923,27.5355980201966,28.2743338823081),
 .UNSPECIFIED.);
#989=B_SPLINE_CURVE_WITH_KNOTS('',3,(#74480,#74481,#74482,#74483,#74484,
#74485,#74486,#74487,#74488,#74489,#74490),.UNSPECIFIED.,.F.,.F.,(4,1,1,
1,1,1,1,1,4),(21.9911485751284,22.2379720782321,23.2330074015058,24.2280427247794,
25.2230780480531,26.2181133713267,27.2131486946004,28.208184017874,28.274333882308),
 .UNSPECIFIED.);
#990=B_SPLINE_CURVE_WITH_KNOTS('',3,(#74495,#74496,#74497,#74498,#74499,
#74500,#74501,#74502,#74503,#74504),.UNSPECIFIED.,.F.,.F.,(4,1,1,1,1,1,
1,4),(15.7079632679489,16.5902094641865,17.5852447874601,18.5802801107338,
19.5753154340074,20.5703507572811,21.5653860805547,21.9911485751285),
 .UNSPECIFIED.);
#991=B_SPLINE_CURVE_WITH_KNOTS('',3,(#74505,#74506,#74507,#74508,#74509,
#74510,#74511,#74512,#74513,#74514),.UNSPECIFIED.,.F.,.F.,(4,1,1,1,1,1,
1,4),(15.7079632679489,16.2677601385902,17.2627954618639,18.2578307851375,
19.2528661084112,20.2479014316848,21.2429367549585,21.9911485751284),
 .UNSPECIFIED.);
#992=B_SPLINE_CURVE_WITH_KNOTS('',3,(#74516,#74517,#74518,#74519,#74520,
#74521,#74522,#74523,#74524,#74525,#74526,#74527,#74528,#74529,#74530,#74531,
#74532,#74533,#74534,#74535,#74536,#74537,#74538,#74539,#74540,#74541,#74542,
#74543,#74544,#74545,#74546,#74547,#74548,#74549,#74550,#74551,#74552,#74553,
#74554,#74555,#74556,#74557,#74558,#74559,#74560,#74561,#74562,#74563,#74564,
#74565,#74566,#74567,#74568,#74569,#74570),.UNSPECIFIED.,.F.,.F.,(4,3,3,
3,3,3,3,3,3,3,3,3,3,3,3,3,3,3,4),(-0.555272788399296,-0.536334845639292,
-0.498799075009887,-0.480079388780021,-0.444545864814167,-0.427699608514178,
-0.413313249422015,-0.365214576623026,-0.332698016808039,-0.315863285595313,
-0.281639241746625,-0.246434336528297,-0.224130346638797,-0.211045162239551,
-0.161112023899574,-0.115330355900824,-0.101980705380743,-0.0495823722640936,
0.),.UNSPECIFIED.);
#993=B_SPLINE_CURVE_WITH_KNOTS('',3,(#74573,#74574,#74575,#74576,#74577,
#74578,#74579,#74580,#74581,#74582,#74583,#74584,#74585,#74586,#74587,#74588,
#74589,#74590,#74591,#74592,#74593,#74594,#74595,#74596,#74597,#74598,#74599,
#74600,#74601,#74602,#74603,#74604,#74605,#74606,#74607,#74608,#74609,#74610,
#74611,#74612,#74613,#74614,#74615,#74616,#74617,#74618,#74619,#74620,#74621,
#74622,#74623,#74624,#74625,#74626,#74627,#74628,#74629,#74630),
 .UNSPECIFIED.,.F.,.F.,(4,3,3,3,3,3,3,3,3,3,3,3,3,3,3,3,3,3,3,4),(-0.552745378375053,
-0.529682502351927,-0.492625929038547,-0.475852674070136,-0.459554142798526,
-0.429705175104552,-0.407584520370654,-0.3903823622905,-0.340467563061915,
-0.306542400025418,-0.292717972343459,-0.251653204733385,-0.202811158742405,
-0.189814062131831,-0.142360546598873,-0.105670766634947,-0.0926673115723117,
-0.0463336557861558,-0.00283643147681147,0.),.UNSPECIFIED.);
#994=B_SPLINE_CURVE_WITH_KNOTS('',3,(#75139,#75140,#75141,#75142),
 .UNSPECIFIED.,.F.,.F.,(4,4),(120.49782124478,121.315741911023),
 .UNSPECIFIED.);
#995=B_SPLINE_CURVE_WITH_KNOTS('',3,(#75144,#75145,#75146,#75147,#75148,
#75149,#75150,#75151,#75152,#75153,#75154,#75155,#75156,#75157,#75158,#75159,
#75160,#75161,#75162,#75163,#75164,#75165,#75166,#75167,#75168,#75169,#75170,
#75171,#75172,#75173,#75174,#75175,#75176,#75177,#75178,#75179,#75180,#75181,
#75182,#75183,#75184,#75185,#75186,#75187,#75188,#75189,#75190,#75191,#75192,
#75193,#75194,#75195,#75196,#75197,#75198),.UNSPECIFIED.,.F.,.F.,(4,3,3,
3,3,3,3,3,3,3,3,3,3,3,3,3,3,3,4),(-0.55527278839938,-0.536334845639381,
-0.498799076325247,-0.480079393209122,-0.444545051261333,-0.427702481446592,
-0.413318783858085,-0.365220196215889,-0.332701424146626,-0.315863774062079,
-0.281639241746661,-0.246434336528328,-0.22413033896029,-0.211045152097239,
-0.161112024781915,-0.115330357453797,-0.101980704464306,-0.0495823608376667,
0.),.UNSPECIFIED.);
#996=B_SPLINE_CURVE_WITH_KNOTS('',3,(#75199,#75200,#75201,#75202,#75203,
#75204,#75205,#75206,#75207),.UNSPECIFIED.,.F.,.F.,(4,1,1,1,1,1,4),(10.3761157273102,
11.292583522222,12.2876188454956,13.2826541687693,14.2776894920429,15.2727248153166,
15.7079632679489),.UNSPECIFIED.);
#997=B_SPLINE_CURVE_WITH_KNOTS('',3,(#75213,#75214,#75215,#75216,#75217,
#75218,#75219,#75220,#75221,#75222,#75223,#75224,#75225,#75226,#75227,#75228,
#75229,#75230,#75231,#75232,#75233,#75234,#75235,#75236,#75237,#75238,#75239,
#75240,#75241,#75242,#75243,#75244,#75245,#75246,#75247,#75248,#75249,#75250,
#75251,#75252,#75253,#75254,#75255,#75256,#75257,#75258,#75259,#75260,#75261,
#75262,#75263,#75264,#75265,#75266,#75267,#75268,#75269,#75270),
 .UNSPECIFIED.,.F.,.F.,(4,3,3,3,3,3,3,3,3,3,3,3,3,3,3,3,3,3,3,4),(-0.552745378375031,
-0.529682502351911,-0.492625920903535,-0.475852659500376,-0.45955413358707,
-0.42970514462757,-0.40758439098946,-0.390382317972672,-0.340467508816843,
-0.306542269974025,-0.292717807416595,-0.251653204733357,-0.202811154924846,
-0.189814058627298,-0.142360543970473,-0.10567076548842,-0.0926673119182951,
-0.0463336559591476,-0.00283647083604326,0.),.UNSPECIFIED.);
#998=B_SPLINE_CURVE_WITH_KNOTS('',3,(#75273,#75274,#75275,#75276,#75277,
#75278,#75279,#75280),.UNSPECIFIED.,.F.,.F.,(4,1,1,1,1,4),(11.6150328478182,
12.6100681710919,13.6051034943655,14.6001388176392,15.5951741409128,15.7079632679489),
 .UNSPECIFIED.);
#999=SHAPE_REPRESENTATION_RELATIONSHIP('SRR','None',#76736,#1019);
#1000=SHAPE_REPRESENTATION_RELATIONSHIP('SRR','None',#76737,#1020);
#1001=SHAPE_REPRESENTATION_RELATIONSHIP('SRR','None',#76738,#1021);
#1002=SHAPE_REPRESENTATION_RELATIONSHIP('SRR','None',#76739,#1022);
#1003=SHAPE_REPRESENTATION_RELATIONSHIP('SRR','None',#76740,#1023);
#1004=SHAPE_REPRESENTATION_RELATIONSHIP('SRR','None',#76741,#1024);
#1005=SHAPE_REPRESENTATION_RELATIONSHIP('SRR','None',#76742,#1025);
#1006=SHAPE_REPRESENTATION_RELATIONSHIP('SRR','None',#76743,#1026);
#1007=SHAPE_REPRESENTATION_RELATIONSHIP('SRR','None',#76744,#1027);
#1008=SHAPE_REPRESENTATION_RELATIONSHIP('SRR','None',#76745,#1028);
#1009=SHAPE_REPRESENTATION_RELATIONSHIP('SRR','None',#76746,#1029);
#1010=SHAPE_REPRESENTATION_RELATIONSHIP('SRR','None',#76747,#1030);
#1011=SHAPE_REPRESENTATION_RELATIONSHIP('SRR','None',#76748,#1031);
#1012=SHAPE_REPRESENTATION_RELATIONSHIP('SRR','None',#76749,#1032);
#1013=SHAPE_REPRESENTATION_RELATIONSHIP('SRR','None',#76750,#1033);
#1014=SHAPE_REPRESENTATION_RELATIONSHIP('SRR','None',#76751,#1034);
#1015=SHAPE_REPRESENTATION_RELATIONSHIP('SRR','None',#76752,#1035);
#1016=SHAPE_REPRESENTATION_RELATIONSHIP('SRR','None',#76753,#1036);
#1017=SHAPE_REPRESENTATION_RELATIONSHIP('SRR','None',#76754,#1037);
#1018=SHAPE_REPRESENTATION_RELATIONSHIP('SRR','None',#76755,#1038);
#1019=ADVANCED_BREP_SHAPE_REPRESENTATION('',(#1059),#76640);
#1020=ADVANCED_BREP_SHAPE_REPRESENTATION('',(#1060),#76641);
#1021=ADVANCED_BREP_SHAPE_REPRESENTATION('',(#1061),#76642);
#1022=ADVANCED_BREP_SHAPE_REPRESENTATION('',(#1062),#76643);
#1023=ADVANCED_BREP_SHAPE_REPRESENTATION('',(#1063),#76644);
#1024=ADVANCED_BREP_SHAPE_REPRESENTATION('',(#1064),#76645);
#1025=ADVANCED_BREP_SHAPE_REPRESENTATION('',(#1065),#76646);
#1026=ADVANCED_BREP_SHAPE_REPRESENTATION('',(#1066),#76647);
#1027=ADVANCED_BREP_SHAPE_REPRESENTATION('',(#1067),#76648);
#1028=ADVANCED_BREP_SHAPE_REPRESENTATION('',(#1068),#76649);
#1029=ADVANCED_BREP_SHAPE_REPRESENTATION('',(#1069),#76650);
#1030=ADVANCED_BREP_SHAPE_REPRESENTATION('',(#1070),#76651);
#1031=ADVANCED_BREP_SHAPE_REPRESENTATION('',(#1071),#76652);
#1032=ADVANCED_BREP_SHAPE_REPRESENTATION('',(#1072),#76653);
#1033=ADVANCED_BREP_SHAPE_REPRESENTATION('',(#1073),#76654);
#1034=ADVANCED_BREP_SHAPE_REPRESENTATION('',(#1074),#76655);
#1035=ADVANCED_BREP_SHAPE_REPRESENTATION('',(#1075),#76656);
#1036=ADVANCED_BREP_SHAPE_REPRESENTATION('',(#1076),#76657);
#1037=ADVANCED_BREP_SHAPE_REPRESENTATION('',(#1077),#76658);
#1038=ADVANCED_BREP_SHAPE_REPRESENTATION('',(#1078),#76659);
#1039=STYLED_ITEM('',(#76885),#1059);
#1040=STYLED_ITEM('',(#76892),#1060);
#1041=STYLED_ITEM('',(#76920),#1061);
#1042=STYLED_ITEM('',(#76892),#1062);
#1043=STYLED_ITEM('',(#76913),#1063);
#1044=STYLED_ITEM('',(#76913),#1064);
#1045=STYLED_ITEM('',(#76906),#1065);
#1046=STYLED_ITEM('',(#76899),#1066);
#1047=STYLED_ITEM('',(#76913),#1067);
#1048=STYLED_ITEM('',(#76906),#1068);
#1049=STYLED_ITEM('',(#76899),#1069);
#1050=STYLED_ITEM('',(#76892),#1070);
#1051=STYLED_ITEM('',(#76913),#1071);
#1052=STYLED_ITEM('',(#76906),#1072);
#1053=STYLED_ITEM('',(#76913),#1073);
#1054=STYLED_ITEM('',(#76920),#1074);
#1055=STYLED_ITEM('',(#76906),#1075);
#1056=STYLED_ITEM('',(#76913),#1076);
#1057=STYLED_ITEM('',(#76913),#1077);
#1058=STYLED_ITEM('',(#76913),#1078);
#1059=MANIFOLD_SOLID_BREP('Base',#26664);
#1060=MANIFOLD_SOLID_BREP('Casing',#26665);
#1061=MANIFOLD_SOLID_BREP('Quill',#26666);
#1062=MANIFOLD_SOLID_BREP('Dead centre',#26667);
#1063=MANIFOLD_SOLID_BREP('Feed screw',#26668);
#1064=MANIFOLD_SOLID_BREP('Bronze nut',#26669);
#1065=MANIFOLD_SOLID_BREP('Rear cap',#26670);
#1066=MANIFOLD_SOLID_BREP('Handwheel',#26671);
#1067=MANIFOLD_SOLID_BREP('Socket head screw',#26672);
#1068=MANIFOLD_SOLID_BREP('Key',#26673);
#1069=MANIFOLD_SOLID_BREP('Clamp lever',#26674);
#1070=MANIFOLD_SOLID_BREP('Clamp shoe',#26675);
#1071=MANIFOLD_SOLID_BREP('Dog point set screw',#26676);
#1072=MANIFOLD_SOLID_BREP('Key bar',#26677);
#1073=MANIFOLD_SOLID_BREP('Hex screw',#26678);
#1074=MANIFOLD_SOLID_BREP('Clamping plate',#26679);
#1075=MANIFOLD_SOLID_BREP('Bearing 51104',#26680);
#1076=MANIFOLD_SOLID_BREP('Hex screw',#26681);
#1077=MANIFOLD_SOLID_BREP('Socket head screw',#26682);
#1078=MANIFOLD_SOLID_BREP('Socket head screw',#26683);
#1079=TOROIDAL_SURFACE('',#27101,0.7,0.3);
#1080=TOROIDAL_SURFACE('',#27107,0.700000000000007,0.3);
#1081=TOROIDAL_SURFACE('',#27111,0.700000000000002,0.3);
#1082=TOROIDAL_SURFACE('',#27115,0.699999999999998,0.3);
#1083=TOROIDAL_SURFACE('',#27370,4.8,0.3);
#1084=TOROIDAL_SURFACE('',#27375,5.8,0.3);
#1085=TOROIDAL_SURFACE('',#27865,10.4,1.1);
#1086=TOROIDAL_SURFACE('',#27917,0.4183,0.025);
#1087=TOROIDAL_SURFACE('',#28689,0.5175,0.025);
#1088=TOROIDAL_SURFACE('',#29028,0.3192,0.025);
#1089=ELLIPSE('',#26967,0.654847281176891,0.605);
#1090=ELLIPSE('',#26976,0.654847281176891,0.605);
#1091=ELLIPSE('',#26995,0.654847281176891,0.605);
#1092=ELLIPSE('',#27030,0.654847281176891,0.605);
#1093=ELLIPSE('',#27339,0.378533806327918,0.3);
#1094=ELLIPSE('',#27353,28.3617829428801,19.3853883884215);
#1095=ELLIPSE('',#27356,28.3617829428803,19.3853883884215);
#1096=ELLIPSE('',#27361,0.378533806327918,0.3);
#1097=ELLIPSE('',#27367,0.424264068711929,0.3);
#1098=ELLIPSE('',#27369,0.424264068711928,0.3);
#1099=ELLIPSE('',#27852,1.41421356237309,1.);
#1100=ELLIPSE('',#27854,1.41421356237308,1.);
#1101=ELLIPSE('',#28266,4.9583738518292,0.681149454424407);
#1102=ELLIPSE('',#28268,4.9583738518292,0.681149454424407);
#1103=CYLINDRICAL_SURFACE('',#26946,0.505000000000003);
#1104=CYLINDRICAL_SURFACE('',#26950,0.505000000000003);
#1105=CYLINDRICAL_SURFACE('',#26954,0.504999999999999);
#1106=CYLINDRICAL_SURFACE('',#26958,0.504999999999999);
#1107=CYLINDRICAL_SURFACE('',#26985,1.);
#1108=CYLINDRICAL_SURFACE('',#26988,1.00000000000001);
#1109=CYLINDRICAL_SURFACE('',#26993,0.605);
#1110=CYLINDRICAL_SURFACE('',#27043,2.);
#1111=CYLINDRICAL_SURFACE('',#27046,2.);
#1112=CYLINDRICAL_SURFACE('',#27105,0.3);
#1113=CYLINDRICAL_SURFACE('',#27109,0.3);
#1114=CYLINDRICAL_SURFACE('',#27113,0.3);
#1115=CYLINDRICAL_SURFACE('',#27118,0.3);
#1116=CYLINDRICAL_SURFACE('',#27119,0.999999999999998);
#1117=CYLINDRICAL_SURFACE('',#27121,1.);
#1118=CYLINDRICAL_SURFACE('',#27130,2.);
#1119=CYLINDRICAL_SURFACE('',#27131,0.605);
#1120=CYLINDRICAL_SURFACE('',#27132,0.875);
#1121=CYLINDRICAL_SURFACE('',#27140,2.);
#1122=CYLINDRICAL_SURFACE('',#27154,1.8);
#1123=CYLINDRICAL_SURFACE('',#27168,0.305);
#1124=CYLINDRICAL_SURFACE('',#27174,0.305);
#1125=CYLINDRICAL_SURFACE('',#27193,5.5);
#1126=CYLINDRICAL_SURFACE('',#27197,0.700000000000003);
#1127=CYLINDRICAL_SURFACE('',#27228,1.);
#1128=CYLINDRICAL_SURFACE('',#27233,0.3);
#1129=CYLINDRICAL_SURFACE('',#27248,0.550000000000001);
#1130=CYLINDRICAL_SURFACE('',#27257,0.550000000000001);
#1131=CYLINDRICAL_SURFACE('',#27266,0.550000000000001);
#1132=CYLINDRICAL_SURFACE('',#27275,0.550000000000001);
#1133=CYLINDRICAL_SURFACE('',#27283,0.305);
#1134=CYLINDRICAL_SURFACE('',#27289,0.305);
#1135=CYLINDRICAL_SURFACE('',#27298,0.550000000000001);
#1136=CYLINDRICAL_SURFACE('',#27315,0.550000000000001);
#1137=CYLINDRICAL_SURFACE('',#27321,0.550000000000001);
#1138=CYLINDRICAL_SURFACE('',#27327,0.550000000000001);
#1139=CYLINDRICAL_SURFACE('',#27338,0.3);
#1140=CYLINDRICAL_SURFACE('',#27340,1.);
#1141=CYLINDRICAL_SURFACE('',#27342,1.);
#1142=CYLINDRICAL_SURFACE('',#27349,4.5);
#1143=CYLINDRICAL_SURFACE('',#27355,19.3853883884215);
#1144=CYLINDRICAL_SURFACE('',#27359,0.3);
#1145=CYLINDRICAL_SURFACE('',#27363,0.3);
#1146=CYLINDRICAL_SURFACE('',#27365,0.3);
#1147=CYLINDRICAL_SURFACE('',#27368,0.3);
#1148=CYLINDRICAL_SURFACE('',#27372,0.3);
#1149=CYLINDRICAL_SURFACE('',#27373,0.3);
#1150=CYLINDRICAL_SURFACE('',#27374,1.);
#1151=CYLINDRICAL_SURFACE('',#27386,0.405000000000001);
#1152=CYLINDRICAL_SURFACE('',#27387,1.005);
#1153=CYLINDRICAL_SURFACE('',#27391,0.605000000000004);
#1154=CYLINDRICAL_SURFACE('',#27392,3.5);
#1155=CYLINDRICAL_SURFACE('',#27552,0.3);
#1156=CYLINDRICAL_SURFACE('',#27555,0.3);
#1157=CYLINDRICAL_SURFACE('',#27558,2.);
#1158=CYLINDRICAL_SURFACE('',#27565,3.497);
#1159=CYLINDRICAL_SURFACE('',#27572,1.1);
#1160=CYLINDRICAL_SURFACE('',#27590,0.9925);
#1161=CYLINDRICAL_SURFACE('',#27592,0.9925);
#1162=CYLINDRICAL_SURFACE('',#27593,0.9925);
#1163=CYLINDRICAL_SURFACE('',#27594,0.9925);
#1164=CYLINDRICAL_SURFACE('',#27595,0.9925);
#1165=CYLINDRICAL_SURFACE('',#27596,0.9925);
#1166=CYLINDRICAL_SURFACE('',#27597,0.9925);
#1167=CYLINDRICAL_SURFACE('',#27598,0.9925);
#1168=CYLINDRICAL_SURFACE('',#27599,0.9925);
#1169=CYLINDRICAL_SURFACE('',#27600,0.9925);
#1170=CYLINDRICAL_SURFACE('',#27601,0.9925);
#1171=CYLINDRICAL_SURFACE('',#27602,0.9925);
#1172=CYLINDRICAL_SURFACE('',#27603,0.9925);
#1173=CYLINDRICAL_SURFACE('',#27604,0.9925);
#1174=CYLINDRICAL_SURFACE('',#27605,0.9925);
#1175=CYLINDRICAL_SURFACE('',#27606,0.9925);
#1176=CYLINDRICAL_SURFACE('',#27607,0.9925);
#1177=CYLINDRICAL_SURFACE('',#27608,0.9925);
#1178=CYLINDRICAL_SURFACE('',#27609,0.9925);
#1179=CYLINDRICAL_SURFACE('',#27610,0.9925);
#1180=CYLINDRICAL_SURFACE('',#27611,0.9925);
#1181=CYLINDRICAL_SURFACE('',#27612,0.9925);
#1182=CYLINDRICAL_SURFACE('',#27613,0.9925);
#1183=CYLINDRICAL_SURFACE('',#27614,0.9925);
#1184=CYLINDRICAL_SURFACE('',#27615,0.9925);
#1185=CYLINDRICAL_SURFACE('',#27616,0.9925);
#1186=CYLINDRICAL_SURFACE('',#27617,0.9925);
#1187=CYLINDRICAL_SURFACE('',#27618,0.9925);
#1188=CYLINDRICAL_SURFACE('',#27619,0.9925);
#1189=CYLINDRICAL_SURFACE('',#27620,0.9925);
#1190=CYLINDRICAL_SURFACE('',#27621,0.9925);
#1191=CYLINDRICAL_SURFACE('',#27622,0.9925);
#1192=CYLINDRICAL_SURFACE('',#27623,0.9925);
#1193=CYLINDRICAL_SURFACE('',#27624,0.9925);
#1194=CYLINDRICAL_SURFACE('',#27625,0.9925);
#1195=CYLINDRICAL_SURFACE('',#27626,0.9925);
#1196=CYLINDRICAL_SURFACE('',#27627,0.9925);
#1197=CYLINDRICAL_SURFACE('',#27628,0.9925);
#1198=CYLINDRICAL_SURFACE('',#27629,0.9925);
#1199=CYLINDRICAL_SURFACE('',#27630,0.9925);
#1200=CYLINDRICAL_SURFACE('',#27631,0.9925);
#1201=CYLINDRICAL_SURFACE('',#27632,0.9925);
#1202=CYLINDRICAL_SURFACE('',#27633,0.76435);
#1203=CYLINDRICAL_SURFACE('',#27635,0.76435);
#1204=CYLINDRICAL_SURFACE('',#27636,0.76435);
#1205=CYLINDRICAL_SURFACE('',#27637,0.76435);
#1206=CYLINDRICAL_SURFACE('',#27638,0.76435);
#1207=CYLINDRICAL_SURFACE('',#27639,0.76435);
#1208=CYLINDRICAL_SURFACE('',#27640,0.76435);
#1209=CYLINDRICAL_SURFACE('',#27641,0.76435);
#1210=CYLINDRICAL_SURFACE('',#27642,0.76435);
#1211=CYLINDRICAL_SURFACE('',#27643,0.76435);
#1212=CYLINDRICAL_SURFACE('',#27644,0.76435);
#1213=CYLINDRICAL_SURFACE('',#27645,0.76435);
#1214=CYLINDRICAL_SURFACE('',#27646,0.76435);
#1215=CYLINDRICAL_SURFACE('',#27647,0.76435);
#1216=CYLINDRICAL_SURFACE('',#27648,0.76435);
#1217=CYLINDRICAL_SURFACE('',#27649,0.76435);
#1218=CYLINDRICAL_SURFACE('',#27650,0.76435);
#1219=CYLINDRICAL_SURFACE('',#27651,0.76435);
#1220=CYLINDRICAL_SURFACE('',#27652,0.76435);
#1221=CYLINDRICAL_SURFACE('',#27653,0.76435);
#1222=CYLINDRICAL_SURFACE('',#27654,0.76435);
#1223=CYLINDRICAL_SURFACE('',#27655,0.76435);
#1224=CYLINDRICAL_SURFACE('',#27656,0.76435);
#1225=CYLINDRICAL_SURFACE('',#27657,0.76435);
#1226=CYLINDRICAL_SURFACE('',#27658,0.76435);
#1227=CYLINDRICAL_SURFACE('',#27659,0.76435);
#1228=CYLINDRICAL_SURFACE('',#27660,0.76435);
#1229=CYLINDRICAL_SURFACE('',#27661,0.76435);
#1230=CYLINDRICAL_SURFACE('',#27662,0.76435);
#1231=CYLINDRICAL_SURFACE('',#27663,0.76435);
#1232=CYLINDRICAL_SURFACE('',#27664,0.76435);
#1233=CYLINDRICAL_SURFACE('',#27665,0.76435);
#1234=CYLINDRICAL_SURFACE('',#27666,0.76435);
#1235=CYLINDRICAL_SURFACE('',#27667,0.76435);
#1236=CYLINDRICAL_SURFACE('',#27668,0.76435);
#1237=CYLINDRICAL_SURFACE('',#27669,0.76435);
#1238=CYLINDRICAL_SURFACE('',#27670,0.76435);
#1239=CYLINDRICAL_SURFACE('',#27671,0.76435);
#1240=CYLINDRICAL_SURFACE('',#27672,0.76435);
#1241=CYLINDRICAL_SURFACE('',#27673,0.76435);
#1242=CYLINDRICAL_SURFACE('',#27674,0.76435);
#1243=CYLINDRICAL_SURFACE('',#27675,0.76435);
#1244=CYLINDRICAL_SURFACE('',#27688,0.405000000000001);
#1245=CYLINDRICAL_SURFACE('',#27697,0.76435);
#1246=CYLINDRICAL_SURFACE('',#27699,0.9925);
#1247=CYLINDRICAL_SURFACE('',#27702,0.25);
#1248=CYLINDRICAL_SURFACE('',#27705,0.25);
#1249=CYLINDRICAL_SURFACE('',#27710,1.);
#1250=CYLINDRICAL_SURFACE('',#27716,1.6);
#1251=CYLINDRICAL_SURFACE('',#27734,1.005);
#1252=CYLINDRICAL_SURFACE('',#27739,1.92);
#1253=CYLINDRICAL_SURFACE('',#27743,2.);
#1254=CYLINDRICAL_SURFACE('',#27746,2.);
#1255=CYLINDRICAL_SURFACE('',#27760,1.8);
#1256=CYLINDRICAL_SURFACE('',#27778,6.25);
#1257=CYLINDRICAL_SURFACE('',#27803,2.8);
#1258=CYLINDRICAL_SURFACE('',#27811,1.8);
#1259=CYLINDRICAL_SURFACE('',#27813,0.330000000000002);
#1260=CYLINDRICAL_SURFACE('',#27814,0.330000000000002);
#1261=CYLINDRICAL_SURFACE('',#27815,0.330000000000002);
#1262=CYLINDRICAL_SURFACE('',#27816,0.330000000000002);
#1263=CYLINDRICAL_SURFACE('',#27817,3.495);
#1264=CYLINDRICAL_SURFACE('',#27822,1.05);
#1265=CYLINDRICAL_SURFACE('',#27831,2.5);
#1266=CYLINDRICAL_SURFACE('',#27859,1.);
#1267=CYLINDRICAL_SURFACE('',#27872,0.46);
#1268=CYLINDRICAL_SURFACE('',#27876,0.3933);
#1269=CYLINDRICAL_SURFACE('',#27878,0.3933);
#1270=CYLINDRICAL_SURFACE('',#27879,0.3933);
#1271=CYLINDRICAL_SURFACE('',#27880,0.3933);
#1272=CYLINDRICAL_SURFACE('',#27881,0.3933);
#1273=CYLINDRICAL_SURFACE('',#27882,0.3933);
#1274=CYLINDRICAL_SURFACE('',#27883,0.3933);
#1275=CYLINDRICAL_SURFACE('',#27884,0.3933);
#1276=CYLINDRICAL_SURFACE('',#27885,0.3933);
#1277=CYLINDRICAL_SURFACE('',#27886,0.3933);
#1278=CYLINDRICAL_SURFACE('',#27887,0.3933);
#1279=CYLINDRICAL_SURFACE('',#27888,0.3933);
#1280=CYLINDRICAL_SURFACE('',#27889,0.3933);
#1281=CYLINDRICAL_SURFACE('',#27890,0.3933);
#1282=CYLINDRICAL_SURFACE('',#27891,0.3933);
#1283=CYLINDRICAL_SURFACE('',#27892,0.3933);
#1284=CYLINDRICAL_SURFACE('',#27893,0.322275);
#1285=CYLINDRICAL_SURFACE('',#27895,0.322275);
#1286=CYLINDRICAL_SURFACE('',#27896,0.322275);
#1287=CYLINDRICAL_SURFACE('',#27897,0.322275);
#1288=CYLINDRICAL_SURFACE('',#27898,0.322275);
#1289=CYLINDRICAL_SURFACE('',#27899,0.322275);
#1290=CYLINDRICAL_SURFACE('',#27900,0.322275);
#1291=CYLINDRICAL_SURFACE('',#27901,0.322275);
#1292=CYLINDRICAL_SURFACE('',#27902,0.322275);
#1293=CYLINDRICAL_SURFACE('',#27903,0.322275);
#1294=CYLINDRICAL_SURFACE('',#27904,0.322275);
#1295=CYLINDRICAL_SURFACE('',#27905,0.322275);
#1296=CYLINDRICAL_SURFACE('',#27906,0.322275);
#1297=CYLINDRICAL_SURFACE('',#27907,0.322275);
#1298=CYLINDRICAL_SURFACE('',#27908,0.322275);
#1299=CYLINDRICAL_SURFACE('',#27916,0.322275);
#1300=CYLINDRICAL_SURFACE('',#27921,0.3933);
#1301=CYLINDRICAL_SURFACE('',#28166,0.65);
#1302=CYLINDRICAL_SURFACE('',#28215,0.25);
#1303=CYLINDRICAL_SURFACE('',#28226,0.25);
#1304=CYLINDRICAL_SURFACE('',#28230,0.591675);
#1305=CYLINDRICAL_SURFACE('',#28232,0.591675);
#1306=CYLINDRICAL_SURFACE('',#28233,0.591675);
#1307=CYLINDRICAL_SURFACE('',#28234,0.591675);
#1308=CYLINDRICAL_SURFACE('',#28235,0.591675);
#1309=CYLINDRICAL_SURFACE('',#28236,0.591675);
#1310=CYLINDRICAL_SURFACE('',#28237,0.591675);
#1311=CYLINDRICAL_SURFACE('',#28238,0.591675);
#1312=CYLINDRICAL_SURFACE('',#28239,0.591675);
#1313=CYLINDRICAL_SURFACE('',#28240,0.591675);
#1314=CYLINDRICAL_SURFACE('',#28241,0.491824999999999);
#1315=CYLINDRICAL_SURFACE('',#28243,0.491824999999999);
#1316=CYLINDRICAL_SURFACE('',#28244,0.491824999999999);
#1317=CYLINDRICAL_SURFACE('',#28245,0.491824999999999);
#1318=CYLINDRICAL_SURFACE('',#28246,0.491824999999999);
#1319=CYLINDRICAL_SURFACE('',#28247,0.491824999999999);
#1320=CYLINDRICAL_SURFACE('',#28248,0.491824999999999);
#1321=CYLINDRICAL_SURFACE('',#28249,0.491824999999999);
#1322=CYLINDRICAL_SURFACE('',#28250,0.491824999999999);
#1323=CYLINDRICAL_SURFACE('',#28261,0.491824999999999);
#1324=CYLINDRICAL_SURFACE('',#28277,0.591675);
#1325=CYLINDRICAL_SURFACE('',#28281,1.5);
#1326=CYLINDRICAL_SURFACE('',#28283,3.5);
#1327=CYLINDRICAL_SURFACE('',#28284,1.);
#1328=CYLINDRICAL_SURFACE('',#28290,0.3933);
#1329=CYLINDRICAL_SURFACE('',#28292,0.3933);
#1330=CYLINDRICAL_SURFACE('',#28293,0.3933);
#1331=CYLINDRICAL_SURFACE('',#28294,0.3933);
#1332=CYLINDRICAL_SURFACE('',#28295,0.3933);
#1333=CYLINDRICAL_SURFACE('',#28296,0.3933);
#1334=CYLINDRICAL_SURFACE('',#28297,0.3933);
#1335=CYLINDRICAL_SURFACE('',#28298,0.3933);
#1336=CYLINDRICAL_SURFACE('',#28299,0.3933);
#1337=CYLINDRICAL_SURFACE('',#28300,0.3933);
#1338=CYLINDRICAL_SURFACE('',#28301,0.3933);
#1339=CYLINDRICAL_SURFACE('',#28302,0.3933);
#1340=CYLINDRICAL_SURFACE('',#28303,0.3933);
#1341=CYLINDRICAL_SURFACE('',#28304,0.3933);
#1342=CYLINDRICAL_SURFACE('',#28305,0.322275);
#1343=CYLINDRICAL_SURFACE('',#28307,0.322275);
#1344=CYLINDRICAL_SURFACE('',#28308,0.322275);
#1345=CYLINDRICAL_SURFACE('',#28309,0.322275);
#1346=CYLINDRICAL_SURFACE('',#28310,0.322275);
#1347=CYLINDRICAL_SURFACE('',#28311,0.322275);
#1348=CYLINDRICAL_SURFACE('',#28312,0.322275);
#1349=CYLINDRICAL_SURFACE('',#28313,0.322275);
#1350=CYLINDRICAL_SURFACE('',#28314,0.322275);
#1351=CYLINDRICAL_SURFACE('',#28315,0.322275);
#1352=CYLINDRICAL_SURFACE('',#28316,0.322275);
#1353=CYLINDRICAL_SURFACE('',#28317,0.322275);
#1354=CYLINDRICAL_SURFACE('',#28318,0.322275);
#1355=CYLINDRICAL_SURFACE('',#28319,0.322275);
#1356=CYLINDRICAL_SURFACE('',#28324,0.322275);
#1357=CYLINDRICAL_SURFACE('',#28338,0.3933);
#1358=CYLINDRICAL_SURFACE('',#28339,0.275);
#1359=CYLINDRICAL_SURFACE('',#28364,0.7911);
#1360=CYLINDRICAL_SURFACE('',#28366,0.7911);
#1361=CYLINDRICAL_SURFACE('',#28367,0.7911);
#1362=CYLINDRICAL_SURFACE('',#28368,0.7911);
#1363=CYLINDRICAL_SURFACE('',#28369,0.7911);
#1364=CYLINDRICAL_SURFACE('',#28370,0.7911);
#1365=CYLINDRICAL_SURFACE('',#28371,0.7911);
#1366=CYLINDRICAL_SURFACE('',#28372,0.7911);
#1367=CYLINDRICAL_SURFACE('',#28373,0.7911);
#1368=CYLINDRICAL_SURFACE('',#28374,0.7911);
#1369=CYLINDRICAL_SURFACE('',#28375,0.7911);
#1370=CYLINDRICAL_SURFACE('',#28376,0.7911);
#1371=CYLINDRICAL_SURFACE('',#28377,0.7911);
#1372=CYLINDRICAL_SURFACE('',#28378,0.7911);
#1373=CYLINDRICAL_SURFACE('',#28379,0.7911);
#1374=CYLINDRICAL_SURFACE('',#28380,0.7911);
#1375=CYLINDRICAL_SURFACE('',#28381,0.7911);
#1376=CYLINDRICAL_SURFACE('',#28382,0.7911);
#1377=CYLINDRICAL_SURFACE('',#28383,0.7911);
#1378=CYLINDRICAL_SURFACE('',#28384,0.7911);
#1379=CYLINDRICAL_SURFACE('',#28385,0.6767);
#1380=CYLINDRICAL_SURFACE('',#28387,0.6767);
#1381=CYLINDRICAL_SURFACE('',#28389,0.6767);
#1382=CYLINDRICAL_SURFACE('',#28390,0.6767);
#1383=CYLINDRICAL_SURFACE('',#28391,0.6767);
#1384=CYLINDRICAL_SURFACE('',#28392,0.6767);
#1385=CYLINDRICAL_SURFACE('',#28393,0.6767);
#1386=CYLINDRICAL_SURFACE('',#28394,0.6767);
#1387=CYLINDRICAL_SURFACE('',#28395,0.6767);
#1388=CYLINDRICAL_SURFACE('',#28396,0.6767);
#1389=CYLINDRICAL_SURFACE('',#28397,0.6767);
#1390=CYLINDRICAL_SURFACE('',#28398,0.6767);
#1391=CYLINDRICAL_SURFACE('',#28399,0.6767);
#1392=CYLINDRICAL_SURFACE('',#28400,0.6767);
#1393=CYLINDRICAL_SURFACE('',#28401,0.6767);
#1394=CYLINDRICAL_SURFACE('',#28402,0.6767);
#1395=CYLINDRICAL_SURFACE('',#28403,0.6767);
#1396=CYLINDRICAL_SURFACE('',#28404,0.6767);
#1397=CYLINDRICAL_SURFACE('',#28405,0.6767);
#1398=CYLINDRICAL_SURFACE('',#28406,0.6767);
#1399=CYLINDRICAL_SURFACE('',#28411,0.6767);
#1400=CYLINDRICAL_SURFACE('',#28426,0.7911);
#1401=CYLINDRICAL_SURFACE('',#28430,1.125);
#1402=CYLINDRICAL_SURFACE('',#28444,0.805);
#1403=CYLINDRICAL_SURFACE('',#28474,0.800000000000004);
#1404=CYLINDRICAL_SURFACE('',#28477,0.799999999999997);
#1405=CYLINDRICAL_SURFACE('',#28521,0.799999999999998);
#1406=CYLINDRICAL_SURFACE('',#28523,0.800000000000004);
#1407=CYLINDRICAL_SURFACE('',#28531,1.56);
#1408=CYLINDRICAL_SURFACE('',#28533,1.05);
#1409=CYLINDRICAL_SURFACE('',#28540,1.75);
#1410=CYLINDRICAL_SURFACE('',#28543,1.56);
#1411=CYLINDRICAL_SURFACE('',#28547,1.72);
#1412=CYLINDRICAL_SURFACE('',#28553,1.);
#1413=CYLINDRICAL_SURFACE('',#28557,1.24);
#1414=CYLINDRICAL_SURFACE('',#28561,0.591675);
#1415=CYLINDRICAL_SURFACE('',#28563,0.591675);
#1416=CYLINDRICAL_SURFACE('',#28564,0.591675);
#1417=CYLINDRICAL_SURFACE('',#28565,0.591675);
#1418=CYLINDRICAL_SURFACE('',#28566,0.591675);
#1419=CYLINDRICAL_SURFACE('',#28567,0.591675);
#1420=CYLINDRICAL_SURFACE('',#28568,0.591675);
#1421=CYLINDRICAL_SURFACE('',#28569,0.591675);
#1422=CYLINDRICAL_SURFACE('',#28570,0.591675);
#1423=CYLINDRICAL_SURFACE('',#28571,0.591675);
#1424=CYLINDRICAL_SURFACE('',#28572,0.591675);
#1425=CYLINDRICAL_SURFACE('',#28573,0.591675);
#1426=CYLINDRICAL_SURFACE('',#28574,0.591675);
#1427=CYLINDRICAL_SURFACE('',#28575,0.591675);
#1428=CYLINDRICAL_SURFACE('',#28576,0.591675);
#1429=CYLINDRICAL_SURFACE('',#28577,0.591675);
#1430=CYLINDRICAL_SURFACE('',#28578,0.591675);
#1431=CYLINDRICAL_SURFACE('',#28579,0.591675);
#1432=CYLINDRICAL_SURFACE('',#28580,0.591675);
#1433=CYLINDRICAL_SURFACE('',#28581,0.591675);
#1434=CYLINDRICAL_SURFACE('',#28582,0.591675);
#1435=CYLINDRICAL_SURFACE('',#28583,0.591675);
#1436=CYLINDRICAL_SURFACE('',#28584,0.591675);
#1437=CYLINDRICAL_SURFACE('',#28585,0.491825);
#1438=CYLINDRICAL_SURFACE('',#28587,0.491825);
#1439=CYLINDRICAL_SURFACE('',#28588,0.491825);
#1440=CYLINDRICAL_SURFACE('',#28589,0.491825);
#1441=CYLINDRICAL_SURFACE('',#28590,0.491825);
#1442=CYLINDRICAL_SURFACE('',#28591,0.491825);
#1443=CYLINDRICAL_SURFACE('',#28592,0.491825);
#1444=CYLINDRICAL_SURFACE('',#28593,0.491825);
#1445=CYLINDRICAL_SURFACE('',#28594,0.491825);
#1446=CYLINDRICAL_SURFACE('',#28595,0.491825);
#1447=CYLINDRICAL_SURFACE('',#28596,0.491825);
#1448=CYLINDRICAL_SURFACE('',#28597,0.491825);
#1449=CYLINDRICAL_SURFACE('',#28598,0.491825);
#1450=CYLINDRICAL_SURFACE('',#28599,0.491825);
#1451=CYLINDRICAL_SURFACE('',#28600,0.491825);
#1452=CYLINDRICAL_SURFACE('',#28601,0.491825);
#1453=CYLINDRICAL_SURFACE('',#28602,0.491825);
#1454=CYLINDRICAL_SURFACE('',#28603,0.491825);
#1455=CYLINDRICAL_SURFACE('',#28604,0.491825);
#1456=CYLINDRICAL_SURFACE('',#28605,0.491825);
#1457=CYLINDRICAL_SURFACE('',#28606,0.491825);
#1458=CYLINDRICAL_SURFACE('',#28607,0.491825);
#1459=CYLINDRICAL_SURFACE('',#28612,0.491825);
#1460=CYLINDRICAL_SURFACE('',#28627,0.591675);
#1461=CYLINDRICAL_SURFACE('',#28631,0.83);
#1462=CYLINDRICAL_SURFACE('',#28633,0.4925);
#1463=CYLINDRICAL_SURFACE('',#28635,0.4925);
#1464=CYLINDRICAL_SURFACE('',#28636,0.4925);
#1465=CYLINDRICAL_SURFACE('',#28637,0.4925);
#1466=CYLINDRICAL_SURFACE('',#28638,0.4925);
#1467=CYLINDRICAL_SURFACE('',#28639,0.4925);
#1468=CYLINDRICAL_SURFACE('',#28640,0.4925);
#1469=CYLINDRICAL_SURFACE('',#28641,0.4925);
#1470=CYLINDRICAL_SURFACE('',#28642,0.4925);
#1471=CYLINDRICAL_SURFACE('',#28643,0.4925);
#1472=CYLINDRICAL_SURFACE('',#28644,0.4925);
#1473=CYLINDRICAL_SURFACE('',#28645,0.4925);
#1474=CYLINDRICAL_SURFACE('',#28646,0.4925);
#1475=CYLINDRICAL_SURFACE('',#28647,0.4925);
#1476=CYLINDRICAL_SURFACE('',#28648,0.4925);
#1477=CYLINDRICAL_SURFACE('',#28649,0.4925);
#1478=CYLINDRICAL_SURFACE('',#28650,0.4925);
#1479=CYLINDRICAL_SURFACE('',#28651,0.4925);
#1480=CYLINDRICAL_SURFACE('',#28652,0.4925);
#1481=CYLINDRICAL_SURFACE('',#28653,0.4925);
#1482=CYLINDRICAL_SURFACE('',#28654,0.4925);
#1483=CYLINDRICAL_SURFACE('',#28655,0.4925);
#1484=CYLINDRICAL_SURFACE('',#28656,0.4925);
#1485=CYLINDRICAL_SURFACE('',#28657,0.40705);
#1486=CYLINDRICAL_SURFACE('',#28659,0.40705);
#1487=CYLINDRICAL_SURFACE('',#28660,0.40705);
#1488=CYLINDRICAL_SURFACE('',#28661,0.40705);
#1489=CYLINDRICAL_SURFACE('',#28662,0.40705);
#1490=CYLINDRICAL_SURFACE('',#28663,0.40705);
#1491=CYLINDRICAL_SURFACE('',#28664,0.40705);
#1492=CYLINDRICAL_SURFACE('',#28665,0.40705);
#1493=CYLINDRICAL_SURFACE('',#28666,0.40705);
#1494=CYLINDRICAL_SURFACE('',#28667,0.40705);
#1495=CYLINDRICAL_SURFACE('',#28668,0.40705);
#1496=CYLINDRICAL_SURFACE('',#28669,0.40705);
#1497=CYLINDRICAL_SURFACE('',#28670,0.40705);
#1498=CYLINDRICAL_SURFACE('',#28671,0.40705);
#1499=CYLINDRICAL_SURFACE('',#28672,0.40705);
#1500=CYLINDRICAL_SURFACE('',#28673,0.40705);
#1501=CYLINDRICAL_SURFACE('',#28674,0.40705);
#1502=CYLINDRICAL_SURFACE('',#28675,0.40705);
#1503=CYLINDRICAL_SURFACE('',#28676,0.40705);
#1504=CYLINDRICAL_SURFACE('',#28677,0.40705);
#1505=CYLINDRICAL_SURFACE('',#28678,0.40705);
#1506=CYLINDRICAL_SURFACE('',#28679,0.40705);
#1507=CYLINDRICAL_SURFACE('',#28680,0.40705);
#1508=CYLINDRICAL_SURFACE('',#28688,0.40705);
#1509=CYLINDRICAL_SURFACE('',#28693,0.4925);
#1510=CYLINDRICAL_SURFACE('',#28938,0.8);
#1511=CYLINDRICAL_SURFACE('',#28979,0.2942);
#1512=CYLINDRICAL_SURFACE('',#28981,0.2942);
#1513=CYLINDRICAL_SURFACE('',#28982,0.2942);
#1514=CYLINDRICAL_SURFACE('',#28983,0.2942);
#1515=CYLINDRICAL_SURFACE('',#28984,0.2942);
#1516=CYLINDRICAL_SURFACE('',#28985,0.2942);
#1517=CYLINDRICAL_SURFACE('',#28986,0.2942);
#1518=CYLINDRICAL_SURFACE('',#28987,0.2942);
#1519=CYLINDRICAL_SURFACE('',#28988,0.2942);
#1520=CYLINDRICAL_SURFACE('',#28989,0.2942);
#1521=CYLINDRICAL_SURFACE('',#28990,0.2942);
#1522=CYLINDRICAL_SURFACE('',#28991,0.2942);
#1523=CYLINDRICAL_SURFACE('',#28992,0.2942);
#1524=CYLINDRICAL_SURFACE('',#28993,0.2942);
#1525=CYLINDRICAL_SURFACE('',#28994,0.2942);
#1526=CYLINDRICAL_SURFACE('',#28995,0.2942);
#1527=CYLINDRICAL_SURFACE('',#28996,0.2942);
#1528=CYLINDRICAL_SURFACE('',#28997,0.2942);
#1529=CYLINDRICAL_SURFACE('',#28998,0.2942);
#1530=CYLINDRICAL_SURFACE('',#28999,0.2942);
#1531=CYLINDRICAL_SURFACE('',#29001,0.237175);
#1532=CYLINDRICAL_SURFACE('',#29003,0.237175);
#1533=CYLINDRICAL_SURFACE('',#29004,0.237175);
#1534=CYLINDRICAL_SURFACE('',#29005,0.237175);
#1535=CYLINDRICAL_SURFACE('',#29006,0.237175);
#1536=CYLINDRICAL_SURFACE('',#29007,0.237175);
#1537=CYLINDRICAL_SURFACE('',#29008,0.237175);
#1538=CYLINDRICAL_SURFACE('',#29009,0.237175);
#1539=CYLINDRICAL_SURFACE('',#29010,0.237175);
#1540=CYLINDRICAL_SURFACE('',#29011,0.237175);
#1541=CYLINDRICAL_SURFACE('',#29012,0.237175);
#1542=CYLINDRICAL_SURFACE('',#29013,0.237175);
#1543=CYLINDRICAL_SURFACE('',#29014,0.237175);
#1544=CYLINDRICAL_SURFACE('',#29015,0.237175);
#1545=CYLINDRICAL_SURFACE('',#29016,0.237175);
#1546=CYLINDRICAL_SURFACE('',#29017,0.237175);
#1547=CYLINDRICAL_SURFACE('',#29018,0.237175);
#1548=CYLINDRICAL_SURFACE('',#29019,0.237175);
#1549=CYLINDRICAL_SURFACE('',#29020,0.237175);
#1550=CYLINDRICAL_SURFACE('',#29027,0.237175);
#1551=CYLINDRICAL_SURFACE('',#29032,0.2942);
#1552=CYLINDRICAL_SURFACE('',#29277,0.5);
#1553=FACE_BOUND('',#4089,.T.);
#1554=FACE_BOUND('',#4092,.T.);
#1555=FACE_BOUND('',#4093,.T.);
#1556=FACE_BOUND('',#4094,.T.);
#1557=FACE_BOUND('',#4095,.T.);
#1558=FACE_BOUND('',#4096,.T.);
#1559=FACE_BOUND('',#4097,.T.);
#1560=FACE_BOUND('',#4194,.T.);
#1561=FACE_BOUND('',#4233,.T.);
#1562=FACE_BOUND('',#4243,.T.);
#1563=FACE_BOUND('',#4244,.T.);
#1564=FACE_BOUND('',#4250,.T.);
#1565=FACE_BOUND('',#4253,.T.);
#1566=FACE_BOUND('',#4254,.T.);
#1567=FACE_BOUND('',#4255,.T.);
#1568=FACE_BOUND('',#4286,.T.);
#1569=FACE_BOUND('',#4292,.T.);
#1570=FACE_BOUND('',#4293,.T.);
#1571=FACE_BOUND('',#4328,.T.);
#1572=FACE_BOUND('',#4329,.T.);
#1573=FACE_BOUND('',#4330,.T.);
#1574=FACE_BOUND('',#4331,.T.);
#1575=FACE_BOUND('',#4401,.T.);
#1576=FACE_BOUND('',#4405,.T.);
#1577=FACE_BOUND('',#4408,.T.);
#1578=FACE_BOUND('',#4409,.T.);
#1579=FACE_BOUND('',#4411,.T.);
#1580=FACE_BOUND('',#4415,.T.);
#1581=FACE_BOUND('',#4528,.T.);
#1582=FACE_BOUND('',#4531,.T.);
#1583=FACE_BOUND('',#4532,.T.);
#1584=FACE_BOUND('',#4533,.T.);
#1585=FACE_BOUND('',#4534,.T.);
#1586=FACE_BOUND('',#4535,.T.);
#1587=FACE_BOUND('',#4536,.T.);
#1588=FACE_BOUND('',#4537,.T.);
#1589=FACE_BOUND('',#4538,.T.);
#1590=FACE_BOUND('',#4539,.T.);
#1591=FACE_BOUND('',#4540,.T.);
#1592=FACE_BOUND('',#4541,.T.);
#1593=FACE_BOUND('',#4542,.T.);
#1594=FACE_BOUND('',#4543,.T.);
#1595=FACE_BOUND('',#4544,.T.);
#1596=FACE_BOUND('',#4545,.T.);
#1597=FACE_BOUND('',#4546,.T.);
#1598=FACE_BOUND('',#4547,.T.);
#1599=FACE_BOUND('',#4548,.T.);
#1600=FACE_BOUND('',#4549,.T.);
#1601=FACE_BOUND('',#4550,.T.);
#1602=FACE_BOUND('',#4551,.T.);
#1603=FACE_BOUND('',#4552,.T.);
#1604=FACE_BOUND('',#4556,.T.);
#1605=FACE_BOUND('',#4559,.T.);
#1606=FACE_BOUND('',#4656,.T.);
#1607=FACE_BOUND('',#4672,.T.);
#1608=FACE_BOUND('',#4674,.T.);
#1609=FACE_BOUND('',#4679,.T.);
#1610=FACE_BOUND('',#4683,.T.);
#1611=FACE_BOUND('',#4687,.T.);
#1612=FACE_BOUND('',#4690,.T.);
#1613=FACE_BOUND('',#4696,.T.);
#1614=FACE_BOUND('',#4700,.T.);
#1615=FACE_BOUND('',#4705,.T.);
#1616=FACE_BOUND('',#4706,.T.);
#1617=FACE_BOUND('',#4707,.T.);
#1618=FACE_BOUND('',#4708,.T.);
#1619=FACE_BOUND('',#4709,.T.);
#1620=FACE_BOUND('',#4716,.T.);
#1621=FACE_BOUND('',#4717,.T.);
#1622=FACE_BOUND('',#4718,.T.);
#1623=FACE_BOUND('',#4719,.T.);
#1624=FACE_BOUND('',#4720,.T.);
#1625=FACE_BOUND('',#4726,.T.);
#1626=FACE_BOUND('',#4736,.T.);
#1627=FACE_BOUND('',#4739,.T.);
#1628=FACE_BOUND('',#4742,.T.);
#1629=FACE_BOUND('',#4743,.T.);
#1630=FACE_BOUND('',#4744,.T.);
#1631=FACE_BOUND('',#4745,.T.);
#1632=FACE_BOUND('',#4751,.T.);
#1633=FACE_BOUND('',#4754,.T.);
#1634=FACE_BOUND('',#4769,.T.);
#1635=FACE_BOUND('',#4809,.T.);
#1636=FACE_BOUND('',#4973,.T.);
#1637=FACE_BOUND('',#5021,.T.);
#1638=FACE_BOUND('',#5060,.T.);
#1639=FACE_BOUND('',#5069,.T.);
#1640=FACE_BOUND('',#5142,.T.);
#1641=FACE_BOUND('',#5151,.T.);
#1642=FACE_BOUND('',#5156,.T.);
#1643=FACE_BOUND('',#5163,.T.);
#1644=FACE_BOUND('',#5217,.T.);
#1645=FACE_BOUND('',#5221,.T.);
#1646=FACE_BOUND('',#5224,.T.);
#1647=FACE_BOUND('',#5228,.T.);
#1648=FACE_BOUND('',#5231,.T.);
#1649=FACE_BOUND('',#5234,.T.);
#1650=FACE_BOUND('',#5289,.T.);
#1651=FACE_BOUND('',#5298,.T.);
#1652=FACE_BOUND('',#5354,.T.);
#1653=FACE_BOUND('',#5518,.T.);
#1654=FACE_BOUND('',#5566,.T.);
#1655=FACE_BOUND('',#5730,.T.);
#1656=PLANE('',#26910);
#1657=PLANE('',#26914);
#1658=PLANE('',#26918);
#1659=PLANE('',#26922);
#1660=PLANE('',#26923);
#1661=PLANE('',#26926);
#1662=PLANE('',#26929);
#1663=PLANE('',#26937);
#1664=PLANE('',#26960);
#1665=PLANE('',#26961);
#1666=PLANE('',#26962);
#1667=PLANE('',#26963);
#1668=PLANE('',#26964);
#1669=PLANE('',#26965);
#1670=PLANE('',#26966);
#1671=PLANE('',#26971);
#1672=PLANE('',#26975);
#1673=PLANE('',#26979);
#1674=PLANE('',#26982);
#1675=PLANE('',#26987);
#1676=PLANE('',#26990);
#1677=PLANE('',#26997);
#1678=PLANE('',#26998);
#1679=PLANE('',#26999);
#1680=PLANE('',#27000);
#1681=PLANE('',#27001);
#1682=PLANE('',#27002);
#1683=PLANE('',#27003);
#1684=PLANE('',#27004);
#1685=PLANE('',#27005);
#1686=PLANE('',#27006);
#1687=PLANE('',#27009);
#1688=PLANE('',#27012);
#1689=PLANE('',#27015);
#1690=PLANE('',#27018);
#1691=PLANE('',#27019);
#1692=PLANE('',#27022);
#1693=PLANE('',#27025);
#1694=PLANE('',#27029);
#1695=PLANE('',#27034);
#1696=PLANE('',#27037);
#1697=PLANE('',#27040);
#1698=PLANE('',#27045);
#1699=PLANE('',#27048);
#1700=PLANE('',#27052);
#1701=PLANE('',#27055);
#1702=PLANE('',#27058);
#1703=PLANE('',#27061);
#1704=PLANE('',#27062);
#1705=PLANE('',#27063);
#1706=PLANE('',#27067);
#1707=PLANE('',#27071);
#1708=PLANE('',#27072);
#1709=PLANE('',#27073);
#1710=PLANE('',#27074);
#1711=PLANE('',#27075);
#1712=PLANE('',#27076);
#1713=PLANE('',#27077);
#1714=PLANE('',#27080);
#1715=PLANE('',#27084);
#1716=PLANE('',#27085);
#1717=PLANE('',#27086);
#1718=PLANE('',#27087);
#1719=PLANE('',#27088);
#1720=PLANE('',#27090);
#1721=PLANE('',#27091);
#1722=PLANE('',#27093);
#1723=PLANE('',#27094);
#1724=PLANE('',#27096);
#1725=PLANE('',#27097);
#1726=PLANE('',#27098);
#1727=PLANE('',#27099);
#1728=PLANE('',#27100);
#1729=PLANE('',#27120);
#1730=PLANE('',#27123);
#1731=PLANE('',#27125);
#1732=PLANE('',#27127);
#1733=PLANE('',#27129);
#1734=PLANE('',#27137);
#1735=PLANE('',#27138);
#1736=PLANE('',#27139);
#1737=PLANE('',#27149);
#1738=PLANE('',#27176);
#1739=PLANE('',#27177);
#1740=PLANE('',#27184);
#1741=PLANE('',#27185);
#1742=PLANE('',#27191);
#1743=PLANE('',#27200);
#1744=PLANE('',#27201);
#1745=PLANE('',#27205);
#1746=PLANE('',#27206);
#1747=PLANE('',#27207);
#1748=PLANE('',#27208);
#1749=PLANE('',#27209);
#1750=PLANE('',#27210);
#1751=PLANE('',#27214);
#1752=PLANE('',#27218);
#1753=PLANE('',#27219);
#1754=PLANE('',#27220);
#1755=PLANE('',#27221);
#1756=PLANE('',#27222);
#1757=PLANE('',#27227);
#1758=PLANE('',#27230);
#1759=PLANE('',#27234);
#1760=PLANE('',#27235);
#1761=PLANE('',#27236);
#1762=PLANE('',#27237);
#1763=PLANE('',#27242);
#1764=PLANE('',#27245);
#1765=PLANE('',#27250);
#1766=PLANE('',#27251);
#1767=PLANE('',#27254);
#1768=PLANE('',#27259);
#1769=PLANE('',#27260);
#1770=PLANE('',#27263);
#1771=PLANE('',#27268);
#1772=PLANE('',#27269);
#1773=PLANE('',#27272);
#1774=PLANE('',#27277);
#1775=PLANE('',#27291);
#1776=PLANE('',#27295);
#1777=PLANE('',#27299);
#1778=PLANE('',#27310);
#1779=PLANE('',#27313);
#1780=PLANE('',#27316);
#1781=PLANE('',#27319);
#1782=PLANE('',#27322);
#1783=PLANE('',#27325);
#1784=PLANE('',#27330);
#1785=PLANE('',#27333);
#1786=PLANE('',#27336);
#1787=PLANE('',#27341);
#1788=PLANE('',#27343);
#1789=PLANE('',#27344);
#1790=PLANE('',#27348);
#1791=PLANE('',#27351);
#1792=PLANE('',#27352);
#1793=PLANE('',#27354);
#1794=PLANE('',#27357);
#1795=PLANE('',#27358);
#1796=PLANE('',#27364);
#1797=PLANE('',#27376);
#1798=PLANE('',#27377);
#1799=PLANE('',#27378);
#1800=PLANE('',#27379);
#1801=PLANE('',#27384);
#1802=PLANE('',#27389);
#1803=PLANE('',#27394);
#1804=PLANE('',#27402);
#1805=PLANE('',#27404);
#1806=PLANE('',#27405);
#1807=PLANE('',#27407);
#1808=PLANE('',#27408);
#1809=PLANE('',#27410);
#1810=PLANE('',#27411);
#1811=PLANE('',#27412);
#1812=PLANE('',#27414);
#1813=PLANE('',#27415);
#1814=PLANE('',#27417);
#1815=PLANE('',#27418);
#1816=PLANE('',#27419);
#1817=PLANE('',#27421);
#1818=PLANE('',#27422);
#1819=PLANE('',#27424);
#1820=PLANE('',#27425);
#1821=PLANE('',#27426);
#1822=PLANE('',#27428);
#1823=PLANE('',#27429);
#1824=PLANE('',#27431);
#1825=PLANE('',#27432);
#1826=PLANE('',#27433);
#1827=PLANE('',#27435);
#1828=PLANE('',#27436);
#1829=PLANE('',#27438);
#1830=PLANE('',#27439);
#1831=PLANE('',#27440);
#1832=PLANE('',#27442);
#1833=PLANE('',#27443);
#1834=PLANE('',#27445);
#1835=PLANE('',#27446);
#1836=PLANE('',#27447);
#1837=PLANE('',#27449);
#1838=PLANE('',#27450);
#1839=PLANE('',#27452);
#1840=PLANE('',#27453);
#1841=PLANE('',#27454);
#1842=PLANE('',#27456);
#1843=PLANE('',#27457);
#1844=PLANE('',#27459);
#1845=PLANE('',#27460);
#1846=PLANE('',#27461);
#1847=PLANE('',#27463);
#1848=PLANE('',#27464);
#1849=PLANE('',#27466);
#1850=PLANE('',#27467);
#1851=PLANE('',#27468);
#1852=PLANE('',#27470);
#1853=PLANE('',#27471);
#1854=PLANE('',#27473);
#1855=PLANE('',#27474);
#1856=PLANE('',#27475);
#1857=PLANE('',#27477);
#1858=PLANE('',#27478);
#1859=PLANE('',#27480);
#1860=PLANE('',#27481);
#1861=PLANE('',#27482);
#1862=PLANE('',#27484);
#1863=PLANE('',#27485);
#1864=PLANE('',#27487);
#1865=PLANE('',#27488);
#1866=PLANE('',#27489);
#1867=PLANE('',#27491);
#1868=PLANE('',#27492);
#1869=PLANE('',#27494);
#1870=PLANE('',#27495);
#1871=PLANE('',#27496);
#1872=PLANE('',#27498);
#1873=PLANE('',#27499);
#1874=PLANE('',#27501);
#1875=PLANE('',#27502);
#1876=PLANE('',#27503);
#1877=PLANE('',#27505);
#1878=PLANE('',#27506);
#1879=PLANE('',#27508);
#1880=PLANE('',#27509);
#1881=PLANE('',#27510);
#1882=PLANE('',#27512);
#1883=PLANE('',#27513);
#1884=PLANE('',#27515);
#1885=PLANE('',#27516);
#1886=PLANE('',#27517);
#1887=PLANE('',#27519);
#1888=PLANE('',#27520);
#1889=PLANE('',#27522);
#1890=PLANE('',#27523);
#1891=PLANE('',#27524);
#1892=PLANE('',#27526);
#1893=PLANE('',#27527);
#1894=PLANE('',#27529);
#1895=PLANE('',#27530);
#1896=PLANE('',#27531);
#1897=PLANE('',#27533);
#1898=PLANE('',#27534);
#1899=PLANE('',#27536);
#1900=PLANE('',#27537);
#1901=PLANE('',#27538);
#1902=PLANE('',#27540);
#1903=PLANE('',#27541);
#1904=PLANE('',#27543);
#1905=PLANE('',#27544);
#1906=PLANE('',#27545);
#1907=PLANE('',#27547);
#1908=PLANE('',#27548);
#1909=PLANE('',#27550);
#1910=PLANE('',#27551);
#1911=PLANE('',#27554);
#1912=PLANE('',#27557);
#1913=PLANE('',#27561);
#1914=PLANE('',#27570);
#1915=PLANE('',#27574);
#1916=PLANE('',#27584);
#1917=PLANE('',#27684);
#1918=PLANE('',#27690);
#1919=PLANE('',#27696);
#1920=PLANE('',#27701);
#1921=PLANE('',#27704);
#1922=PLANE('',#27707);
#1923=PLANE('',#27712);
#1924=PLANE('',#27720);
#1925=PLANE('',#27729);
#1926=PLANE('',#27736);
#1927=PLANE('',#27741);
#1928=PLANE('',#27750);
#1929=PLANE('',#27758);
#1930=PLANE('',#27769);
#1931=PLANE('',#27789);
#1932=PLANE('',#27806);
#1933=PLANE('',#27820);
#1934=PLANE('',#27824);
#1935=PLANE('',#27845);
#1936=PLANE('',#27849);
#1937=PLANE('',#27851);
#1938=PLANE('',#27853);
#1939=PLANE('',#27855);
#1940=PLANE('',#27856);
#1941=PLANE('',#27857);
#1942=PLANE('',#27858);
#1943=PLANE('',#27874);
#1944=PLANE('',#27909);
#1945=PLANE('',#27912);
#1946=PLANE('',#27922);
#1947=PLANE('',#27924);
#1948=PLANE('',#27926);
#1949=PLANE('',#27928);
#1950=PLANE('',#27930);
#1951=PLANE('',#27932);
#1952=PLANE('',#27934);
#1953=PLANE('',#27937);
#1954=PLANE('',#27938);
#1955=PLANE('',#27939);
#1956=PLANE('',#27940);
#1957=PLANE('',#27941);
#1958=PLANE('',#27942);
#1959=PLANE('',#27943);
#1960=PLANE('',#27944);
#1961=PLANE('',#27946);
#1962=PLANE('',#27947);
#1963=PLANE('',#27949);
#1964=PLANE('',#27950);
#1965=PLANE('',#27952);
#1966=PLANE('',#27953);
#1967=PLANE('',#27955);
#1968=PLANE('',#27956);
#1969=PLANE('',#27958);
#1970=PLANE('',#27959);
#1971=PLANE('',#27961);
#1972=PLANE('',#27962);
#1973=PLANE('',#27964);
#1974=PLANE('',#27965);
#1975=PLANE('',#27967);
#1976=PLANE('',#27968);
#1977=PLANE('',#27970);
#1978=PLANE('',#27971);
#1979=PLANE('',#27973);
#1980=PLANE('',#27974);
#1981=PLANE('',#27976);
#1982=PLANE('',#27977);
#1983=PLANE('',#27979);
#1984=PLANE('',#27980);
#1985=PLANE('',#27982);
#1986=PLANE('',#27983);
#1987=PLANE('',#27985);
#1988=PLANE('',#27986);
#1989=PLANE('',#27988);
#1990=PLANE('',#27989);
#1991=PLANE('',#27991);
#1992=PLANE('',#27992);
#1993=PLANE('',#27995);
#1994=PLANE('',#27996);
#1995=PLANE('',#27999);
#1996=PLANE('',#28000);
#1997=PLANE('',#28002);
#1998=PLANE('',#28003);
#1999=PLANE('',#28005);
#2000=PLANE('',#28006);
#2001=PLANE('',#28008);
#2002=PLANE('',#28009);
#2003=PLANE('',#28011);
#2004=PLANE('',#28012);
#2005=PLANE('',#28014);
#2006=PLANE('',#28015);
#2007=PLANE('',#28017);
#2008=PLANE('',#28018);
#2009=PLANE('',#28020);
#2010=PLANE('',#28021);
#2011=PLANE('',#28023);
#2012=PLANE('',#28024);
#2013=PLANE('',#28026);
#2014=PLANE('',#28027);
#2015=PLANE('',#28029);
#2016=PLANE('',#28030);
#2017=PLANE('',#28032);
#2018=PLANE('',#28033);
#2019=PLANE('',#28035);
#2020=PLANE('',#28036);
#2021=PLANE('',#28038);
#2022=PLANE('',#28039);
#2023=PLANE('',#28041);
#2024=PLANE('',#28042);
#2025=PLANE('',#28044);
#2026=PLANE('',#28045);
#2027=PLANE('',#28047);
#2028=PLANE('',#28048);
#2029=PLANE('',#28050);
#2030=PLANE('',#28051);
#2031=PLANE('',#28053);
#2032=PLANE('',#28054);
#2033=PLANE('',#28056);
#2034=PLANE('',#28057);
#2035=PLANE('',#28059);
#2036=PLANE('',#28060);
#2037=PLANE('',#28062);
#2038=PLANE('',#28063);
#2039=PLANE('',#28065);
#2040=PLANE('',#28066);
#2041=PLANE('',#28068);
#2042=PLANE('',#28069);
#2043=PLANE('',#28071);
#2044=PLANE('',#28072);
#2045=PLANE('',#28074);
#2046=PLANE('',#28075);
#2047=PLANE('',#28077);
#2048=PLANE('',#28078);
#2049=PLANE('',#28080);
#2050=PLANE('',#28081);
#2051=PLANE('',#28083);
#2052=PLANE('',#28084);
#2053=PLANE('',#28086);
#2054=PLANE('',#28087);
#2055=PLANE('',#28089);
#2056=PLANE('',#28090);
#2057=PLANE('',#28092);
#2058=PLANE('',#28093);
#2059=PLANE('',#28095);
#2060=PLANE('',#28096);
#2061=PLANE('',#28098);
#2062=PLANE('',#28099);
#2063=PLANE('',#28101);
#2064=PLANE('',#28103);
#2065=PLANE('',#28104);
#2066=PLANE('',#28105);
#2067=PLANE('',#28107);
#2068=PLANE('',#28108);
#2069=PLANE('',#28110);
#2070=PLANE('',#28111);
#2071=PLANE('',#28113);
#2072=PLANE('',#28114);
#2073=PLANE('',#28116);
#2074=PLANE('',#28117);
#2075=PLANE('',#28119);
#2076=PLANE('',#28120);
#2077=PLANE('',#28122);
#2078=PLANE('',#28123);
#2079=PLANE('',#28125);
#2080=PLANE('',#28126);
#2081=PLANE('',#28128);
#2082=PLANE('',#28129);
#2083=PLANE('',#28131);
#2084=PLANE('',#28132);
#2085=PLANE('',#28134);
#2086=PLANE('',#28135);
#2087=PLANE('',#28137);
#2088=PLANE('',#28138);
#2089=PLANE('',#28140);
#2090=PLANE('',#28141);
#2091=PLANE('',#28143);
#2092=PLANE('',#28144);
#2093=PLANE('',#28146);
#2094=PLANE('',#28147);
#2095=PLANE('',#28149);
#2096=PLANE('',#28150);
#2097=PLANE('',#28152);
#2098=PLANE('',#28153);
#2099=PLANE('',#28155);
#2100=PLANE('',#28156);
#2101=PLANE('',#28158);
#2102=PLANE('',#28159);
#2103=PLANE('',#28161);
#2104=PLANE('',#28205);
#2105=PLANE('',#28207);
#2106=PLANE('',#28211);
#2107=PLANE('',#28217);
#2108=PLANE('',#28218);
#2109=PLANE('',#28219);
#2110=PLANE('',#28223);
#2111=PLANE('',#28227);
#2112=PLANE('',#28228);
#2113=PLANE('',#28257);
#2114=PLANE('',#28272);
#2115=PLANE('',#28273);
#2116=PLANE('',#28274);
#2117=PLANE('',#28279);
#2118=PLANE('',#28288);
#2119=PLANE('',#28320);
#2120=PLANE('',#28325);
#2121=PLANE('',#28328);
#2122=PLANE('',#28329);
#2123=PLANE('',#28330);
#2124=PLANE('',#28331);
#2125=PLANE('',#28332);
#2126=PLANE('',#28333);
#2127=PLANE('',#28334);
#2128=PLANE('',#28335);
#2129=PLANE('',#28343);
#2130=PLANE('',#28345);
#2131=PLANE('',#28346);
#2132=PLANE('',#28347);
#2133=PLANE('',#28348);
#2134=PLANE('',#28349);
#2135=PLANE('',#28350);
#2136=PLANE('',#28351);
#2137=PLANE('',#28352);
#2138=PLANE('',#28353);
#2139=PLANE('',#28354);
#2140=PLANE('',#28355);
#2141=PLANE('',#28356);
#2142=PLANE('',#28357);
#2143=PLANE('',#28358);
#2144=PLANE('',#28359);
#2145=PLANE('',#28360);
#2146=PLANE('',#28361);
#2147=PLANE('',#28362);
#2148=PLANE('',#28407);
#2149=PLANE('',#28414);
#2150=PLANE('',#28415);
#2151=PLANE('',#28416);
#2152=PLANE('',#28417);
#2153=PLANE('',#28419);
#2154=PLANE('',#28420);
#2155=PLANE('',#28421);
#2156=PLANE('',#28422);
#2157=PLANE('',#28423);
#2158=PLANE('',#28428);
#2159=PLANE('',#28437);
#2160=PLANE('',#28452);
#2161=PLANE('',#28460);
#2162=PLANE('',#28464);
#2163=PLANE('',#28468);
#2164=PLANE('',#28472);
#2165=PLANE('',#28473);
#2166=PLANE('',#28476);
#2167=PLANE('',#28479);
#2168=PLANE('',#28481);
#2169=PLANE('',#28483);
#2170=PLANE('',#28486);
#2171=PLANE('',#28489);
#2172=PLANE('',#28492);
#2173=PLANE('',#28497);
#2174=PLANE('',#28500);
#2175=PLANE('',#28501);
#2176=PLANE('',#28503);
#2177=PLANE('',#28505);
#2178=PLANE('',#28509);
#2179=PLANE('',#28514);
#2180=PLANE('',#28516);
#2181=PLANE('',#28517);
#2182=PLANE('',#28519);
#2183=PLANE('',#28522);
#2184=PLANE('',#28524);
#2185=PLANE('',#28536);
#2186=PLANE('',#28542);
#2187=PLANE('',#28545);
#2188=PLANE('',#28551);
#2189=PLANE('',#28555);
#2190=PLANE('',#28559);
#2191=PLANE('',#28608);
#2192=PLANE('',#28615);
#2193=PLANE('',#28616);
#2194=PLANE('',#28617);
#2195=PLANE('',#28618);
#2196=PLANE('',#28620);
#2197=PLANE('',#28621);
#2198=PLANE('',#28622);
#2199=PLANE('',#28623);
#2200=PLANE('',#28624);
#2201=PLANE('',#28629);
#2202=PLANE('',#28681);
#2203=PLANE('',#28684);
#2204=PLANE('',#28694);
#2205=PLANE('',#28696);
#2206=PLANE('',#28698);
#2207=PLANE('',#28700);
#2208=PLANE('',#28702);
#2209=PLANE('',#28704);
#2210=PLANE('',#28706);
#2211=PLANE('',#28709);
#2212=PLANE('',#28710);
#2213=PLANE('',#28711);
#2214=PLANE('',#28712);
#2215=PLANE('',#28713);
#2216=PLANE('',#28714);
#2217=PLANE('',#28715);
#2218=PLANE('',#28716);
#2219=PLANE('',#28718);
#2220=PLANE('',#28719);
#2221=PLANE('',#28721);
#2222=PLANE('',#28722);
#2223=PLANE('',#28724);
#2224=PLANE('',#28725);
#2225=PLANE('',#28727);
#2226=PLANE('',#28728);
#2227=PLANE('',#28730);
#2228=PLANE('',#28731);
#2229=PLANE('',#28733);
#2230=PLANE('',#28734);
#2231=PLANE('',#28736);
#2232=PLANE('',#28737);
#2233=PLANE('',#28739);
#2234=PLANE('',#28740);
#2235=PLANE('',#28742);
#2236=PLANE('',#28743);
#2237=PLANE('',#28745);
#2238=PLANE('',#28746);
#2239=PLANE('',#28748);
#2240=PLANE('',#28749);
#2241=PLANE('',#28751);
#2242=PLANE('',#28752);
#2243=PLANE('',#28754);
#2244=PLANE('',#28755);
#2245=PLANE('',#28757);
#2246=PLANE('',#28758);
#2247=PLANE('',#28760);
#2248=PLANE('',#28761);
#2249=PLANE('',#28763);
#2250=PLANE('',#28764);
#2251=PLANE('',#28767);
#2252=PLANE('',#28768);
#2253=PLANE('',#28771);
#2254=PLANE('',#28772);
#2255=PLANE('',#28774);
#2256=PLANE('',#28775);
#2257=PLANE('',#28777);
#2258=PLANE('',#28778);
#2259=PLANE('',#28780);
#2260=PLANE('',#28781);
#2261=PLANE('',#28783);
#2262=PLANE('',#28784);
#2263=PLANE('',#28786);
#2264=PLANE('',#28787);
#2265=PLANE('',#28789);
#2266=PLANE('',#28790);
#2267=PLANE('',#28792);
#2268=PLANE('',#28793);
#2269=PLANE('',#28795);
#2270=PLANE('',#28796);
#2271=PLANE('',#28798);
#2272=PLANE('',#28799);
#2273=PLANE('',#28801);
#2274=PLANE('',#28802);
#2275=PLANE('',#28804);
#2276=PLANE('',#28805);
#2277=PLANE('',#28807);
#2278=PLANE('',#28808);
#2279=PLANE('',#28810);
#2280=PLANE('',#28811);
#2281=PLANE('',#28813);
#2282=PLANE('',#28814);
#2283=PLANE('',#28816);
#2284=PLANE('',#28817);
#2285=PLANE('',#28819);
#2286=PLANE('',#28820);
#2287=PLANE('',#28822);
#2288=PLANE('',#28823);
#2289=PLANE('',#28825);
#2290=PLANE('',#28826);
#2291=PLANE('',#28828);
#2292=PLANE('',#28829);
#2293=PLANE('',#28831);
#2294=PLANE('',#28832);
#2295=PLANE('',#28834);
#2296=PLANE('',#28835);
#2297=PLANE('',#28837);
#2298=PLANE('',#28838);
#2299=PLANE('',#28840);
#2300=PLANE('',#28841);
#2301=PLANE('',#28843);
#2302=PLANE('',#28844);
#2303=PLANE('',#28846);
#2304=PLANE('',#28847);
#2305=PLANE('',#28849);
#2306=PLANE('',#28850);
#2307=PLANE('',#28852);
#2308=PLANE('',#28853);
#2309=PLANE('',#28855);
#2310=PLANE('',#28856);
#2311=PLANE('',#28858);
#2312=PLANE('',#28859);
#2313=PLANE('',#28861);
#2314=PLANE('',#28862);
#2315=PLANE('',#28864);
#2316=PLANE('',#28865);
#2317=PLANE('',#28867);
#2318=PLANE('',#28868);
#2319=PLANE('',#28870);
#2320=PLANE('',#28871);
#2321=PLANE('',#28873);
#2322=PLANE('',#28875);
#2323=PLANE('',#28876);
#2324=PLANE('',#28877);
#2325=PLANE('',#28879);
#2326=PLANE('',#28880);
#2327=PLANE('',#28882);
#2328=PLANE('',#28883);
#2329=PLANE('',#28885);
#2330=PLANE('',#28886);
#2331=PLANE('',#28888);
#2332=PLANE('',#28889);
#2333=PLANE('',#28891);
#2334=PLANE('',#28892);
#2335=PLANE('',#28894);
#2336=PLANE('',#28895);
#2337=PLANE('',#28897);
#2338=PLANE('',#28898);
#2339=PLANE('',#28900);
#2340=PLANE('',#28901);
#2341=PLANE('',#28903);
#2342=PLANE('',#28904);
#2343=PLANE('',#28906);
#2344=PLANE('',#28907);
#2345=PLANE('',#28909);
#2346=PLANE('',#28910);
#2347=PLANE('',#28912);
#2348=PLANE('',#28913);
#2349=PLANE('',#28915);
#2350=PLANE('',#28916);
#2351=PLANE('',#28918);
#2352=PLANE('',#28919);
#2353=PLANE('',#28921);
#2354=PLANE('',#28922);
#2355=PLANE('',#28924);
#2356=PLANE('',#28925);
#2357=PLANE('',#28927);
#2358=PLANE('',#28928);
#2359=PLANE('',#28930);
#2360=PLANE('',#28931);
#2361=PLANE('',#28933);
#2362=PLANE('',#28977);
#2363=PLANE('',#29021);
#2364=PLANE('',#29023);
#2365=PLANE('',#29033);
#2366=PLANE('',#29035);
#2367=PLANE('',#29037);
#2368=PLANE('',#29039);
#2369=PLANE('',#29041);
#2370=PLANE('',#29043);
#2371=PLANE('',#29045);
#2372=PLANE('',#29048);
#2373=PLANE('',#29049);
#2374=PLANE('',#29050);
#2375=PLANE('',#29051);
#2376=PLANE('',#29052);
#2377=PLANE('',#29053);
#2378=PLANE('',#29054);
#2379=PLANE('',#29055);
#2380=PLANE('',#29057);
#2381=PLANE('',#29058);
#2382=PLANE('',#29060);
#2383=PLANE('',#29061);
#2384=PLANE('',#29063);
#2385=PLANE('',#29064);
#2386=PLANE('',#29066);
#2387=PLANE('',#29067);
#2388=PLANE('',#29069);
#2389=PLANE('',#29070);
#2390=PLANE('',#29072);
#2391=PLANE('',#29073);
#2392=PLANE('',#29075);
#2393=PLANE('',#29076);
#2394=PLANE('',#29078);
#2395=PLANE('',#29079);
#2396=PLANE('',#29081);
#2397=PLANE('',#29082);
#2398=PLANE('',#29084);
#2399=PLANE('',#29085);
#2400=PLANE('',#29087);
#2401=PLANE('',#29088);
#2402=PLANE('',#29090);
#2403=PLANE('',#29091);
#2404=PLANE('',#29093);
#2405=PLANE('',#29094);
#2406=PLANE('',#29096);
#2407=PLANE('',#29097);
#2408=PLANE('',#29099);
#2409=PLANE('',#29100);
#2410=PLANE('',#29102);
#2411=PLANE('',#29103);
#2412=PLANE('',#29106);
#2413=PLANE('',#29107);
#2414=PLANE('',#29110);
#2415=PLANE('',#29111);
#2416=PLANE('',#29113);
#2417=PLANE('',#29114);
#2418=PLANE('',#29116);
#2419=PLANE('',#29117);
#2420=PLANE('',#29119);
#2421=PLANE('',#29120);
#2422=PLANE('',#29122);
#2423=PLANE('',#29123);
#2424=PLANE('',#29125);
#2425=PLANE('',#29126);
#2426=PLANE('',#29128);
#2427=PLANE('',#29129);
#2428=PLANE('',#29131);
#2429=PLANE('',#29132);
#2430=PLANE('',#29134);
#2431=PLANE('',#29135);
#2432=PLANE('',#29137);
#2433=PLANE('',#29138);
#2434=PLANE('',#29140);
#2435=PLANE('',#29141);
#2436=PLANE('',#29143);
#2437=PLANE('',#29144);
#2438=PLANE('',#29146);
#2439=PLANE('',#29147);
#2440=PLANE('',#29149);
#2441=PLANE('',#29150);
#2442=PLANE('',#29152);
#2443=PLANE('',#29153);
#2444=PLANE('',#29155);
#2445=PLANE('',#29156);
#2446=PLANE('',#29158);
#2447=PLANE('',#29159);
#2448=PLANE('',#29161);
#2449=PLANE('',#29162);
#2450=PLANE('',#29164);
#2451=PLANE('',#29165);
#2452=PLANE('',#29167);
#2453=PLANE('',#29168);
#2454=PLANE('',#29170);
#2455=PLANE('',#29171);
#2456=PLANE('',#29173);
#2457=PLANE('',#29174);
#2458=PLANE('',#29176);
#2459=PLANE('',#29177);
#2460=PLANE('',#29179);
#2461=PLANE('',#29180);
#2462=PLANE('',#29182);
#2463=PLANE('',#29183);
#2464=PLANE('',#29185);
#2465=PLANE('',#29186);
#2466=PLANE('',#29188);
#2467=PLANE('',#29189);
#2468=PLANE('',#29191);
#2469=PLANE('',#29192);
#2470=PLANE('',#29194);
#2471=PLANE('',#29195);
#2472=PLANE('',#29197);
#2473=PLANE('',#29198);
#2474=PLANE('',#29200);
#2475=PLANE('',#29201);
#2476=PLANE('',#29203);
#2477=PLANE('',#29204);
#2478=PLANE('',#29206);
#2479=PLANE('',#29207);
#2480=PLANE('',#29209);
#2481=PLANE('',#29210);
#2482=PLANE('',#29212);
#2483=PLANE('',#29214);
#2484=PLANE('',#29215);
#2485=PLANE('',#29216);
#2486=PLANE('',#29218);
#2487=PLANE('',#29219);
#2488=PLANE('',#29221);
#2489=PLANE('',#29222);
#2490=PLANE('',#29224);
#2491=PLANE('',#29225);
#2492=PLANE('',#29227);
#2493=PLANE('',#29228);
#2494=PLANE('',#29230);
#2495=PLANE('',#29231);
#2496=PLANE('',#29233);
#2497=PLANE('',#29234);
#2498=PLANE('',#29236);
#2499=PLANE('',#29237);
#2500=PLANE('',#29239);
#2501=PLANE('',#29240);
#2502=PLANE('',#29242);
#2503=PLANE('',#29243);
#2504=PLANE('',#29245);
#2505=PLANE('',#29246);
#2506=PLANE('',#29248);
#2507=PLANE('',#29249);
#2508=PLANE('',#29251);
#2509=PLANE('',#29252);
#2510=PLANE('',#29254);
#2511=PLANE('',#29255);
#2512=PLANE('',#29257);
#2513=PLANE('',#29258);
#2514=PLANE('',#29260);
#2515=PLANE('',#29261);
#2516=PLANE('',#29263);
#2517=PLANE('',#29264);
#2518=PLANE('',#29266);
#2519=PLANE('',#29267);
#2520=PLANE('',#29269);
#2521=PLANE('',#29270);
#2522=PLANE('',#29272);
#2523=PLANE('',#29316);
#2524=FACE_OUTER_BOUND('',#4076,.T.);
#2525=FACE_OUTER_BOUND('',#4077,.T.);
#2526=FACE_OUTER_BOUND('',#4078,.T.);
#2527=FACE_OUTER_BOUND('',#4079,.T.);
#2528=FACE_OUTER_BOUND('',#4080,.T.);
#2529=FACE_OUTER_BOUND('',#4081,.T.);
#2530=FACE_OUTER_BOUND('',#4082,.T.);
#2531=FACE_OUTER_BOUND('',#4083,.T.);
#2532=FACE_OUTER_BOUND('',#4084,.T.);
#2533=FACE_OUTER_BOUND('',#4085,.T.);
#2534=FACE_OUTER_BOUND('',#4086,.T.);
#2535=FACE_OUTER_BOUND('',#4087,.T.);
#2536=FACE_OUTER_BOUND('',#4088,.T.);
#2537=FACE_OUTER_BOUND('',#4090,.T.);
#2538=FACE_OUTER_BOUND('',#4091,.T.);
#2539=FACE_OUTER_BOUND('',#4098,.T.);
#2540=FACE_OUTER_BOUND('',#4099,.T.);
#2541=FACE_OUTER_BOUND('',#4100,.T.);
#2542=FACE_OUTER_BOUND('',#4101,.T.);
#2543=FACE_OUTER_BOUND('',#4102,.T.);
#2544=FACE_OUTER_BOUND('',#4103,.T.);
#2545=FACE_OUTER_BOUND('',#4104,.T.);
#2546=FACE_OUTER_BOUND('',#4105,.T.);
#2547=FACE_OUTER_BOUND('',#4106,.T.);
#2548=FACE_OUTER_BOUND('',#4107,.T.);
#2549=FACE_OUTER_BOUND('',#4108,.T.);
#2550=FACE_OUTER_BOUND('',#4109,.T.);
#2551=FACE_OUTER_BOUND('',#4110,.T.);
#2552=FACE_OUTER_BOUND('',#4111,.T.);
#2553=FACE_OUTER_BOUND('',#4112,.T.);
#2554=FACE_OUTER_BOUND('',#4113,.T.);
#2555=FACE_OUTER_BOUND('',#4114,.T.);
#2556=FACE_OUTER_BOUND('',#4115,.T.);
#2557=FACE_OUTER_BOUND('',#4116,.T.);
#2558=FACE_OUTER_BOUND('',#4117,.T.);
#2559=FACE_OUTER_BOUND('',#4118,.T.);
#2560=FACE_OUTER_BOUND('',#4119,.T.);
#2561=FACE_OUTER_BOUND('',#4120,.T.);
#2562=FACE_OUTER_BOUND('',#4121,.T.);
#2563=FACE_OUTER_BOUND('',#4122,.T.);
#2564=FACE_OUTER_BOUND('',#4123,.T.);
#2565=FACE_OUTER_BOUND('',#4124,.T.);
#2566=FACE_OUTER_BOUND('',#4125,.T.);
#2567=FACE_OUTER_BOUND('',#4126,.T.);
#2568=FACE_OUTER_BOUND('',#4127,.T.);
#2569=FACE_OUTER_BOUND('',#4128,.T.);
#2570=FACE_OUTER_BOUND('',#4129,.T.);
#2571=FACE_OUTER_BOUND('',#4130,.T.);
#2572=FACE_OUTER_BOUND('',#4131,.T.);
#2573=FACE_OUTER_BOUND('',#4132,.T.);
#2574=FACE_OUTER_BOUND('',#4133,.T.);
#2575=FACE_OUTER_BOUND('',#4134,.T.);
#2576=FACE_OUTER_BOUND('',#4135,.T.);
#2577=FACE_OUTER_BOUND('',#4136,.T.);
#2578=FACE_OUTER_BOUND('',#4137,.T.);
#2579=FACE_OUTER_BOUND('',#4138,.T.);
#2580=FACE_OUTER_BOUND('',#4139,.T.);
#2581=FACE_OUTER_BOUND('',#4140,.T.);
#2582=FACE_OUTER_BOUND('',#4141,.T.);
#2583=FACE_OUTER_BOUND('',#4142,.T.);
#2584=FACE_OUTER_BOUND('',#4143,.T.);
#2585=FACE_OUTER_BOUND('',#4144,.T.);
#2586=FACE_OUTER_BOUND('',#4145,.T.);
#2587=FACE_OUTER_BOUND('',#4146,.T.);
#2588=FACE_OUTER_BOUND('',#4147,.T.);
#2589=FACE_OUTER_BOUND('',#4148,.T.);
#2590=FACE_OUTER_BOUND('',#4149,.T.);
#2591=FACE_OUTER_BOUND('',#4150,.T.);
#2592=FACE_OUTER_BOUND('',#4151,.T.);
#2593=FACE_OUTER_BOUND('',#4152,.T.);
#2594=FACE_OUTER_BOUND('',#4153,.T.);
#2595=FACE_OUTER_BOUND('',#4154,.T.);
#2596=FACE_OUTER_BOUND('',#4155,.T.);
#2597=FACE_OUTER_BOUND('',#4156,.T.);
#2598=FACE_OUTER_BOUND('',#4157,.T.);
#2599=FACE_OUTER_BOUND('',#4158,.T.);
#2600=FACE_OUTER_BOUND('',#4159,.T.);
#2601=FACE_OUTER_BOUND('',#4160,.T.);
#2602=FACE_OUTER_BOUND('',#4161,.T.);
#2603=FACE_OUTER_BOUND('',#4162,.T.);
#2604=FACE_OUTER_BOUND('',#4163,.T.);
#2605=FACE_OUTER_BOUND('',#4164,.T.);
#2606=FACE_OUTER_BOUND('',#4165,.T.);
#2607=FACE_OUTER_BOUND('',#4166,.T.);
#2608=FACE_OUTER_BOUND('',#4167,.T.);
#2609=FACE_OUTER_BOUND('',#4168,.T.);
#2610=FACE_OUTER_BOUND('',#4169,.T.);
#2611=FACE_OUTER_BOUND('',#4170,.T.);
#2612=FACE_OUTER_BOUND('',#4171,.T.);
#2613=FACE_OUTER_BOUND('',#4172,.T.);
#2614=FACE_OUTER_BOUND('',#4173,.T.);
#2615=FACE_OUTER_BOUND('',#4174,.T.);
#2616=FACE_OUTER_BOUND('',#4175,.T.);
#2617=FACE_OUTER_BOUND('',#4176,.T.);
#2618=FACE_OUTER_BOUND('',#4177,.T.);
#2619=FACE_OUTER_BOUND('',#4178,.T.);
#2620=FACE_OUTER_BOUND('',#4179,.T.);
#2621=FACE_OUTER_BOUND('',#4180,.T.);
#2622=FACE_OUTER_BOUND('',#4181,.T.);
#2623=FACE_OUTER_BOUND('',#4182,.T.);
#2624=FACE_OUTER_BOUND('',#4183,.T.);
#2625=FACE_OUTER_BOUND('',#4184,.T.);
#2626=FACE_OUTER_BOUND('',#4185,.T.);
#2627=FACE_OUTER_BOUND('',#4186,.T.);
#2628=FACE_OUTER_BOUND('',#4187,.T.);
#2629=FACE_OUTER_BOUND('',#4188,.T.);
#2630=FACE_OUTER_BOUND('',#4189,.T.);
#2631=FACE_OUTER_BOUND('',#4190,.T.);
#2632=FACE_OUTER_BOUND('',#4191,.T.);
#2633=FACE_OUTER_BOUND('',#4192,.T.);
#2634=FACE_OUTER_BOUND('',#4193,.T.);
#2635=FACE_OUTER_BOUND('',#4195,.T.);
#2636=FACE_OUTER_BOUND('',#4196,.T.);
#2637=FACE_OUTER_BOUND('',#4197,.T.);
#2638=FACE_OUTER_BOUND('',#4198,.T.);
#2639=FACE_OUTER_BOUND('',#4199,.T.);
#2640=FACE_OUTER_BOUND('',#4200,.T.);
#2641=FACE_OUTER_BOUND('',#4201,.T.);
#2642=FACE_OUTER_BOUND('',#4202,.T.);
#2643=FACE_OUTER_BOUND('',#4203,.T.);
#2644=FACE_OUTER_BOUND('',#4204,.T.);
#2645=FACE_OUTER_BOUND('',#4205,.T.);
#2646=FACE_OUTER_BOUND('',#4206,.T.);
#2647=FACE_OUTER_BOUND('',#4207,.T.);
#2648=FACE_OUTER_BOUND('',#4208,.T.);
#2649=FACE_OUTER_BOUND('',#4209,.T.);
#2650=FACE_OUTER_BOUND('',#4210,.T.);
#2651=FACE_OUTER_BOUND('',#4211,.T.);
#2652=FACE_OUTER_BOUND('',#4212,.T.);
#2653=FACE_OUTER_BOUND('',#4213,.T.);
#2654=FACE_OUTER_BOUND('',#4214,.T.);
#2655=FACE_OUTER_BOUND('',#4215,.T.);
#2656=FACE_OUTER_BOUND('',#4216,.T.);
#2657=FACE_OUTER_BOUND('',#4217,.T.);
#2658=FACE_OUTER_BOUND('',#4218,.T.);
#2659=FACE_OUTER_BOUND('',#4219,.T.);
#2660=FACE_OUTER_BOUND('',#4220,.T.);
#2661=FACE_OUTER_BOUND('',#4221,.T.);
#2662=FACE_OUTER_BOUND('',#4222,.T.);
#2663=FACE_OUTER_BOUND('',#4223,.T.);
#2664=FACE_OUTER_BOUND('',#4224,.T.);
#2665=FACE_OUTER_BOUND('',#4225,.T.);
#2666=FACE_OUTER_BOUND('',#4226,.T.);
#2667=FACE_OUTER_BOUND('',#4227,.T.);
#2668=FACE_OUTER_BOUND('',#4228,.T.);
#2669=FACE_OUTER_BOUND('',#4229,.T.);
#2670=FACE_OUTER_BOUND('',#4230,.T.);
#2671=FACE_OUTER_BOUND('',#4231,.T.);
#2672=FACE_OUTER_BOUND('',#4232,.T.);
#2673=FACE_OUTER_BOUND('',#4234,.T.);
#2674=FACE_OUTER_BOUND('',#4235,.T.);
#2675=FACE_OUTER_BOUND('',#4236,.T.);
#2676=FACE_OUTER_BOUND('',#4237,.T.);
#2677=FACE_OUTER_BOUND('',#4238,.T.);
#2678=FACE_OUTER_BOUND('',#4239,.T.);
#2679=FACE_OUTER_BOUND('',#4240,.T.);
#2680=FACE_OUTER_BOUND('',#4241,.T.);
#2681=FACE_OUTER_BOUND('',#4242,.T.);
#2682=FACE_OUTER_BOUND('',#4245,.T.);
#2683=FACE_OUTER_BOUND('',#4246,.T.);
#2684=FACE_OUTER_BOUND('',#4247,.T.);
#2685=FACE_OUTER_BOUND('',#4248,.T.);
#2686=FACE_OUTER_BOUND('',#4249,.T.);
#2687=FACE_OUTER_BOUND('',#4251,.T.);
#2688=FACE_OUTER_BOUND('',#4252,.T.);
#2689=FACE_OUTER_BOUND('',#4256,.T.);
#2690=FACE_OUTER_BOUND('',#4257,.T.);
#2691=FACE_OUTER_BOUND('',#4258,.T.);
#2692=FACE_OUTER_BOUND('',#4259,.T.);
#2693=FACE_OUTER_BOUND('',#4260,.T.);
#2694=FACE_OUTER_BOUND('',#4261,.T.);
#2695=FACE_OUTER_BOUND('',#4262,.T.);
#2696=FACE_OUTER_BOUND('',#4263,.T.);
#2697=FACE_OUTER_BOUND('',#4264,.T.);
#2698=FACE_OUTER_BOUND('',#4265,.T.);
#2699=FACE_OUTER_BOUND('',#4266,.T.);
#2700=FACE_OUTER_BOUND('',#4267,.T.);
#2701=FACE_OUTER_BOUND('',#4268,.T.);
#2702=FACE_OUTER_BOUND('',#4269,.T.);
#2703=FACE_OUTER_BOUND('',#4270,.T.);
#2704=FACE_OUTER_BOUND('',#4271,.T.);
#2705=FACE_OUTER_BOUND('',#4272,.T.);
#2706=FACE_OUTER_BOUND('',#4273,.T.);
#2707=FACE_OUTER_BOUND('',#4274,.T.);
#2708=FACE_OUTER_BOUND('',#4275,.T.);
#2709=FACE_OUTER_BOUND('',#4276,.T.);
#2710=FACE_OUTER_BOUND('',#4277,.T.);
#2711=FACE_OUTER_BOUND('',#4278,.T.);
#2712=FACE_OUTER_BOUND('',#4279,.T.);
#2713=FACE_OUTER_BOUND('',#4280,.T.);
#2714=FACE_OUTER_BOUND('',#4281,.T.);
#2715=FACE_OUTER_BOUND('',#4282,.T.);
#2716=FACE_OUTER_BOUND('',#4283,.T.);
#2717=FACE_OUTER_BOUND('',#4284,.T.);
#2718=FACE_OUTER_BOUND('',#4285,.T.);
#2719=FACE_OUTER_BOUND('',#4287,.T.);
#2720=FACE_OUTER_BOUND('',#4288,.T.);
#2721=FACE_OUTER_BOUND('',#4289,.T.);
#2722=FACE_OUTER_BOUND('',#4290,.T.);
#2723=FACE_OUTER_BOUND('',#4291,.T.);
#2724=FACE_OUTER_BOUND('',#4294,.T.);
#2725=FACE_OUTER_BOUND('',#4295,.T.);
#2726=FACE_OUTER_BOUND('',#4296,.T.);
#2727=FACE_OUTER_BOUND('',#4297,.T.);
#2728=FACE_OUTER_BOUND('',#4298,.T.);
#2729=FACE_OUTER_BOUND('',#4299,.T.);
#2730=FACE_OUTER_BOUND('',#4300,.T.);
#2731=FACE_OUTER_BOUND('',#4301,.T.);
#2732=FACE_OUTER_BOUND('',#4302,.T.);
#2733=FACE_OUTER_BOUND('',#4303,.T.);
#2734=FACE_OUTER_BOUND('',#4304,.T.);
#2735=FACE_OUTER_BOUND('',#4305,.T.);
#2736=FACE_OUTER_BOUND('',#4306,.T.);
#2737=FACE_OUTER_BOUND('',#4307,.T.);
#2738=FACE_OUTER_BOUND('',#4308,.T.);
#2739=FACE_OUTER_BOUND('',#4309,.T.);
#2740=FACE_OUTER_BOUND('',#4310,.T.);
#2741=FACE_OUTER_BOUND('',#4311,.T.);
#2742=FACE_OUTER_BOUND('',#4312,.T.);
#2743=FACE_OUTER_BOUND('',#4313,.T.);
#2744=FACE_OUTER_BOUND('',#4314,.T.);
#2745=FACE_OUTER_BOUND('',#4315,.T.);
#2746=FACE_OUTER_BOUND('',#4316,.T.);
#2747=FACE_OUTER_BOUND('',#4317,.T.);
#2748=FACE_OUTER_BOUND('',#4318,.T.);
#2749=FACE_OUTER_BOUND('',#4319,.T.);
#2750=FACE_OUTER_BOUND('',#4320,.T.);
#2751=FACE_OUTER_BOUND('',#4321,.T.);
#2752=FACE_OUTER_BOUND('',#4322,.T.);
#2753=FACE_OUTER_BOUND('',#4323,.T.);
#2754=FACE_OUTER_BOUND('',#4324,.T.);
#2755=FACE_OUTER_BOUND('',#4325,.T.);
#2756=FACE_OUTER_BOUND('',#4326,.T.);
#2757=FACE_OUTER_BOUND('',#4327,.T.);
#2758=FACE_OUTER_BOUND('',#4332,.T.);
#2759=FACE_OUTER_BOUND('',#4333,.T.);
#2760=FACE_OUTER_BOUND('',#4334,.T.);
#2761=FACE_OUTER_BOUND('',#4335,.T.);
#2762=FACE_OUTER_BOUND('',#4336,.T.);
#2763=FACE_OUTER_BOUND('',#4337,.T.);
#2764=FACE_OUTER_BOUND('',#4338,.T.);
#2765=FACE_OUTER_BOUND('',#4339,.T.);
#2766=FACE_OUTER_BOUND('',#4340,.T.);
#2767=FACE_OUTER_BOUND('',#4341,.T.);
#2768=FACE_OUTER_BOUND('',#4342,.T.);
#2769=FACE_OUTER_BOUND('',#4343,.T.);
#2770=FACE_OUTER_BOUND('',#4344,.T.);
#2771=FACE_OUTER_BOUND('',#4345,.T.);
#2772=FACE_OUTER_BOUND('',#4346,.T.);
#2773=FACE_OUTER_BOUND('',#4347,.T.);
#2774=FACE_OUTER_BOUND('',#4348,.T.);
#2775=FACE_OUTER_BOUND('',#4349,.T.);
#2776=FACE_OUTER_BOUND('',#4350,.T.);
#2777=FACE_OUTER_BOUND('',#4351,.T.);
#2778=FACE_OUTER_BOUND('',#4352,.T.);
#2779=FACE_OUTER_BOUND('',#4353,.T.);
#2780=FACE_OUTER_BOUND('',#4354,.T.);
#2781=FACE_OUTER_BOUND('',#4355,.T.);
#2782=FACE_OUTER_BOUND('',#4356,.T.);
#2783=FACE_OUTER_BOUND('',#4357,.T.);
#2784=FACE_OUTER_BOUND('',#4358,.T.);
#2785=FACE_OUTER_BOUND('',#4359,.T.);
#2786=FACE_OUTER_BOUND('',#4360,.T.);
#2787=FACE_OUTER_BOUND('',#4361,.T.);
#2788=FACE_OUTER_BOUND('',#4362,.T.);
#2789=FACE_OUTER_BOUND('',#4363,.T.);
#2790=FACE_OUTER_BOUND('',#4364,.T.);
#2791=FACE_OUTER_BOUND('',#4365,.T.);
#2792=FACE_OUTER_BOUND('',#4366,.T.);
#2793=FACE_OUTER_BOUND('',#4367,.T.);
#2794=FACE_OUTER_BOUND('',#4368,.T.);
#2795=FACE_OUTER_BOUND('',#4369,.T.);
#2796=FACE_OUTER_BOUND('',#4370,.T.);
#2797=FACE_OUTER_BOUND('',#4371,.T.);
#2798=FACE_OUTER_BOUND('',#4372,.T.);
#2799=FACE_OUTER_BOUND('',#4373,.T.);
#2800=FACE_OUTER_BOUND('',#4374,.T.);
#2801=FACE_OUTER_BOUND('',#4375,.T.);
#2802=FACE_OUTER_BOUND('',#4376,.T.);
#2803=FACE_OUTER_BOUND('',#4377,.T.);
#2804=FACE_OUTER_BOUND('',#4378,.T.);
#2805=FACE_OUTER_BOUND('',#4379,.T.);
#2806=FACE_OUTER_BOUND('',#4380,.T.);
#2807=FACE_OUTER_BOUND('',#4381,.T.);
#2808=FACE_OUTER_BOUND('',#4382,.T.);
#2809=FACE_OUTER_BOUND('',#4383,.T.);
#2810=FACE_OUTER_BOUND('',#4384,.T.);
#2811=FACE_OUTER_BOUND('',#4385,.T.);
#2812=FACE_OUTER_BOUND('',#4386,.T.);
#2813=FACE_OUTER_BOUND('',#4387,.T.);
#2814=FACE_OUTER_BOUND('',#4388,.T.);
#2815=FACE_OUTER_BOUND('',#4389,.T.);
#2816=FACE_OUTER_BOUND('',#4390,.T.);
#2817=FACE_OUTER_BOUND('',#4391,.T.);
#2818=FACE_OUTER_BOUND('',#4392,.T.);
#2819=FACE_OUTER_BOUND('',#4393,.T.);
#2820=FACE_OUTER_BOUND('',#4394,.T.);
#2821=FACE_OUTER_BOUND('',#4395,.T.);
#2822=FACE_OUTER_BOUND('',#4396,.T.);
#2823=FACE_OUTER_BOUND('',#4397,.T.);
#2824=FACE_OUTER_BOUND('',#4398,.T.);
#2825=FACE_OUTER_BOUND('',#4399,.T.);
#2826=FACE_OUTER_BOUND('',#4400,.T.);
#2827=FACE_OUTER_BOUND('',#4402,.T.);
#2828=FACE_OUTER_BOUND('',#4403,.T.);
#2829=FACE_OUTER_BOUND('',#4404,.T.);
#2830=FACE_OUTER_BOUND('',#4406,.T.);
#2831=FACE_OUTER_BOUND('',#4407,.T.);
#2832=FACE_OUTER_BOUND('',#4410,.T.);
#2833=FACE_OUTER_BOUND('',#4412,.T.);
#2834=FACE_OUTER_BOUND('',#4413,.T.);
#2835=FACE_OUTER_BOUND('',#4414,.T.);
#2836=FACE_OUTER_BOUND('',#4416,.T.);
#2837=FACE_OUTER_BOUND('',#4417,.T.);
#2838=FACE_OUTER_BOUND('',#4418,.T.);
#2839=FACE_OUTER_BOUND('',#4419,.T.);
#2840=FACE_OUTER_BOUND('',#4420,.T.);
#2841=FACE_OUTER_BOUND('',#4421,.T.);
#2842=FACE_OUTER_BOUND('',#4422,.T.);
#2843=FACE_OUTER_BOUND('',#4423,.T.);
#2844=FACE_OUTER_BOUND('',#4424,.T.);
#2845=FACE_OUTER_BOUND('',#4425,.T.);
#2846=FACE_OUTER_BOUND('',#4426,.T.);
#2847=FACE_OUTER_BOUND('',#4427,.T.);
#2848=FACE_OUTER_BOUND('',#4428,.T.);
#2849=FACE_OUTER_BOUND('',#4429,.T.);
#2850=FACE_OUTER_BOUND('',#4430,.T.);
#2851=FACE_OUTER_BOUND('',#4431,.T.);
#2852=FACE_OUTER_BOUND('',#4432,.T.);
#2853=FACE_OUTER_BOUND('',#4433,.T.);
#2854=FACE_OUTER_BOUND('',#4434,.T.);
#2855=FACE_OUTER_BOUND('',#4435,.T.);
#2856=FACE_OUTER_BOUND('',#4436,.T.);
#2857=FACE_OUTER_BOUND('',#4437,.T.);
#2858=FACE_OUTER_BOUND('',#4438,.T.);
#2859=FACE_OUTER_BOUND('',#4439,.T.);
#2860=FACE_OUTER_BOUND('',#4440,.T.);
#2861=FACE_OUTER_BOUND('',#4441,.T.);
#2862=FACE_OUTER_BOUND('',#4442,.T.);
#2863=FACE_OUTER_BOUND('',#4443,.T.);
#2864=FACE_OUTER_BOUND('',#4444,.T.);
#2865=FACE_OUTER_BOUND('',#4445,.T.);
#2866=FACE_OUTER_BOUND('',#4446,.T.);
#2867=FACE_OUTER_BOUND('',#4447,.T.);
#2868=FACE_OUTER_BOUND('',#4448,.T.);
#2869=FACE_OUTER_BOUND('',#4449,.T.);
#2870=FACE_OUTER_BOUND('',#4450,.T.);
#2871=FACE_OUTER_BOUND('',#4451,.T.);
#2872=FACE_OUTER_BOUND('',#4452,.T.);
#2873=FACE_OUTER_BOUND('',#4453,.T.);
#2874=FACE_OUTER_BOUND('',#4454,.T.);
#2875=FACE_OUTER_BOUND('',#4455,.T.);
#2876=FACE_OUTER_BOUND('',#4456,.T.);
#2877=FACE_OUTER_BOUND('',#4457,.T.);
#2878=FACE_OUTER_BOUND('',#4458,.T.);
#2879=FACE_OUTER_BOUND('',#4459,.T.);
#2880=FACE_OUTER_BOUND('',#4460,.T.);
#2881=FACE_OUTER_BOUND('',#4461,.T.);
#2882=FACE_OUTER_BOUND('',#4462,.T.);
#2883=FACE_OUTER_BOUND('',#4463,.T.);
#2884=FACE_OUTER_BOUND('',#4464,.T.);
#2885=FACE_OUTER_BOUND('',#4465,.T.);
#2886=FACE_OUTER_BOUND('',#4466,.T.);
#2887=FACE_OUTER_BOUND('',#4467,.T.);
#2888=FACE_OUTER_BOUND('',#4468,.T.);
#2889=FACE_OUTER_BOUND('',#4469,.T.);
#2890=FACE_OUTER_BOUND('',#4470,.T.);
#2891=FACE_OUTER_BOUND('',#4471,.T.);
#2892=FACE_OUTER_BOUND('',#4472,.T.);
#2893=FACE_OUTER_BOUND('',#4473,.T.);
#2894=FACE_OUTER_BOUND('',#4474,.T.);
#2895=FACE_OUTER_BOUND('',#4475,.T.);
#2896=FACE_OUTER_BOUND('',#4476,.T.);
#2897=FACE_OUTER_BOUND('',#4477,.T.);
#2898=FACE_OUTER_BOUND('',#4478,.T.);
#2899=FACE_OUTER_BOUND('',#4479,.T.);
#2900=FACE_OUTER_BOUND('',#4480,.T.);
#2901=FACE_OUTER_BOUND('',#4481,.T.);
#2902=FACE_OUTER_BOUND('',#4482,.T.);
#2903=FACE_OUTER_BOUND('',#4483,.T.);
#2904=FACE_OUTER_BOUND('',#4484,.T.);
#2905=FACE_OUTER_BOUND('',#4485,.T.);
#2906=FACE_OUTER_BOUND('',#4486,.T.);
#2907=FACE_OUTER_BOUND('',#4487,.T.);
#2908=FACE_OUTER_BOUND('',#4488,.T.);
#2909=FACE_OUTER_BOUND('',#4489,.T.);
#2910=FACE_OUTER_BOUND('',#4490,.T.);
#2911=FACE_OUTER_BOUND('',#4491,.T.);
#2912=FACE_OUTER_BOUND('',#4492,.T.);
#2913=FACE_OUTER_BOUND('',#4493,.T.);
#2914=FACE_OUTER_BOUND('',#4494,.T.);
#2915=FACE_OUTER_BOUND('',#4495,.T.);
#2916=FACE_OUTER_BOUND('',#4496,.T.);
#2917=FACE_OUTER_BOUND('',#4497,.T.);
#2918=FACE_OUTER_BOUND('',#4498,.T.);
#2919=FACE_OUTER_BOUND('',#4499,.T.);
#2920=FACE_OUTER_BOUND('',#4500,.T.);
#2921=FACE_OUTER_BOUND('',#4501,.T.);
#2922=FACE_OUTER_BOUND('',#4502,.T.);
#2923=FACE_OUTER_BOUND('',#4503,.T.);
#2924=FACE_OUTER_BOUND('',#4504,.T.);
#2925=FACE_OUTER_BOUND('',#4505,.T.);
#2926=FACE_OUTER_BOUND('',#4506,.T.);
#2927=FACE_OUTER_BOUND('',#4507,.T.);
#2928=FACE_OUTER_BOUND('',#4508,.T.);
#2929=FACE_OUTER_BOUND('',#4509,.T.);
#2930=FACE_OUTER_BOUND('',#4510,.T.);
#2931=FACE_OUTER_BOUND('',#4511,.T.);
#2932=FACE_OUTER_BOUND('',#4512,.T.);
#2933=FACE_OUTER_BOUND('',#4513,.T.);
#2934=FACE_OUTER_BOUND('',#4514,.T.);
#2935=FACE_OUTER_BOUND('',#4515,.T.);
#2936=FACE_OUTER_BOUND('',#4516,.T.);
#2937=FACE_OUTER_BOUND('',#4517,.T.);
#2938=FACE_OUTER_BOUND('',#4518,.T.);
#2939=FACE_OUTER_BOUND('',#4519,.T.);
#2940=FACE_OUTER_BOUND('',#4520,.T.);
#2941=FACE_OUTER_BOUND('',#4521,.T.);
#2942=FACE_OUTER_BOUND('',#4522,.T.);
#2943=FACE_OUTER_BOUND('',#4523,.T.);
#2944=FACE_OUTER_BOUND('',#4524,.T.);
#2945=FACE_OUTER_BOUND('',#4525,.T.);
#2946=FACE_OUTER_BOUND('',#4526,.T.);
#2947=FACE_OUTER_BOUND('',#4527,.T.);
#2948=FACE_OUTER_BOUND('',#4529,.T.);
#2949=FACE_OUTER_BOUND('',#4530,.T.);
#2950=FACE_OUTER_BOUND('',#4553,.T.);
#2951=FACE_OUTER_BOUND('',#4554,.T.);
#2952=FACE_OUTER_BOUND('',#4555,.T.);
#2953=FACE_OUTER_BOUND('',#4557,.T.);
#2954=FACE_OUTER_BOUND('',#4558,.T.);
#2955=FACE_OUTER_BOUND('',#4560,.T.);
#2956=FACE_OUTER_BOUND('',#4561,.T.);
#2957=FACE_OUTER_BOUND('',#4562,.T.);
#2958=FACE_OUTER_BOUND('',#4563,.T.);
#2959=FACE_OUTER_BOUND('',#4564,.T.);
#2960=FACE_OUTER_BOUND('',#4565,.T.);
#2961=FACE_OUTER_BOUND('',#4566,.T.);
#2962=FACE_OUTER_BOUND('',#4567,.T.);
#2963=FACE_OUTER_BOUND('',#4568,.T.);
#2964=FACE_OUTER_BOUND('',#4569,.T.);
#2965=FACE_OUTER_BOUND('',#4570,.T.);
#2966=FACE_OUTER_BOUND('',#4571,.T.);
#2967=FACE_OUTER_BOUND('',#4572,.T.);
#2968=FACE_OUTER_BOUND('',#4573,.T.);
#2969=FACE_OUTER_BOUND('',#4574,.T.);
#2970=FACE_OUTER_BOUND('',#4575,.T.);
#2971=FACE_OUTER_BOUND('',#4576,.T.);
#2972=FACE_OUTER_BOUND('',#4577,.T.);
#2973=FACE_OUTER_BOUND('',#4578,.T.);
#2974=FACE_OUTER_BOUND('',#4579,.T.);
#2975=FACE_OUTER_BOUND('',#4580,.T.);
#2976=FACE_OUTER_BOUND('',#4581,.T.);
#2977=FACE_OUTER_BOUND('',#4582,.T.);
#2978=FACE_OUTER_BOUND('',#4583,.T.);
#2979=FACE_OUTER_BOUND('',#4584,.T.);
#2980=FACE_OUTER_BOUND('',#4585,.T.);
#2981=FACE_OUTER_BOUND('',#4586,.T.);
#2982=FACE_OUTER_BOUND('',#4587,.T.);
#2983=FACE_OUTER_BOUND('',#4588,.T.);
#2984=FACE_OUTER_BOUND('',#4589,.T.);
#2985=FACE_OUTER_BOUND('',#4590,.T.);
#2986=FACE_OUTER_BOUND('',#4591,.T.);
#2987=FACE_OUTER_BOUND('',#4592,.T.);
#2988=FACE_OUTER_BOUND('',#4593,.T.);
#2989=FACE_OUTER_BOUND('',#4594,.T.);
#2990=FACE_OUTER_BOUND('',#4595,.T.);
#2991=FACE_OUTER_BOUND('',#4596,.T.);
#2992=FACE_OUTER_BOUND('',#4597,.T.);
#2993=FACE_OUTER_BOUND('',#4598,.T.);
#2994=FACE_OUTER_BOUND('',#4599,.T.);
#2995=FACE_OUTER_BOUND('',#4600,.T.);
#2996=FACE_OUTER_BOUND('',#4601,.T.);
#2997=FACE_OUTER_BOUND('',#4602,.T.);
#2998=FACE_OUTER_BOUND('',#4603,.T.);
#2999=FACE_OUTER_BOUND('',#4604,.T.);
#3000=FACE_OUTER_BOUND('',#4605,.T.);
#3001=FACE_OUTER_BOUND('',#4606,.T.);
#3002=FACE_OUTER_BOUND('',#4607,.T.);
#3003=FACE_OUTER_BOUND('',#4608,.T.);
#3004=FACE_OUTER_BOUND('',#4609,.T.);
#3005=FACE_OUTER_BOUND('',#4610,.T.);
#3006=FACE_OUTER_BOUND('',#4611,.T.);
#3007=FACE_OUTER_BOUND('',#4612,.T.);
#3008=FACE_OUTER_BOUND('',#4613,.T.);
#3009=FACE_OUTER_BOUND('',#4614,.T.);
#3010=FACE_OUTER_BOUND('',#4615,.T.);
#3011=FACE_OUTER_BOUND('',#4616,.T.);
#3012=FACE_OUTER_BOUND('',#4617,.T.);
#3013=FACE_OUTER_BOUND('',#4618,.T.);
#3014=FACE_OUTER_BOUND('',#4619,.T.);
#3015=FACE_OUTER_BOUND('',#4620,.T.);
#3016=FACE_OUTER_BOUND('',#4621,.T.);
#3017=FACE_OUTER_BOUND('',#4622,.T.);
#3018=FACE_OUTER_BOUND('',#4623,.T.);
#3019=FACE_OUTER_BOUND('',#4624,.T.);
#3020=FACE_OUTER_BOUND('',#4625,.T.);
#3021=FACE_OUTER_BOUND('',#4626,.T.);
#3022=FACE_OUTER_BOUND('',#4627,.T.);
#3023=FACE_OUTER_BOUND('',#4628,.T.);
#3024=FACE_OUTER_BOUND('',#4629,.T.);
#3025=FACE_OUTER_BOUND('',#4630,.T.);
#3026=FACE_OUTER_BOUND('',#4631,.T.);
#3027=FACE_OUTER_BOUND('',#4632,.T.);
#3028=FACE_OUTER_BOUND('',#4633,.T.);
#3029=FACE_OUTER_BOUND('',#4634,.T.);
#3030=FACE_OUTER_BOUND('',#4635,.T.);
#3031=FACE_OUTER_BOUND('',#4636,.T.);
#3032=FACE_OUTER_BOUND('',#4637,.T.);
#3033=FACE_OUTER_BOUND('',#4638,.T.);
#3034=FACE_OUTER_BOUND('',#4639,.T.);
#3035=FACE_OUTER_BOUND('',#4640,.T.);
#3036=FACE_OUTER_BOUND('',#4641,.T.);
#3037=FACE_OUTER_BOUND('',#4642,.T.);
#3038=FACE_OUTER_BOUND('',#4643,.T.);
#3039=FACE_OUTER_BOUND('',#4644,.T.);
#3040=FACE_OUTER_BOUND('',#4645,.T.);
#3041=FACE_OUTER_BOUND('',#4646,.T.);
#3042=FACE_OUTER_BOUND('',#4647,.T.);
#3043=FACE_OUTER_BOUND('',#4648,.T.);
#3044=FACE_OUTER_BOUND('',#4649,.T.);
#3045=FACE_OUTER_BOUND('',#4650,.T.);
#3046=FACE_OUTER_BOUND('',#4651,.T.);
#3047=FACE_OUTER_BOUND('',#4652,.T.);
#3048=FACE_OUTER_BOUND('',#4653,.T.);
#3049=FACE_OUTER_BOUND('',#4654,.T.);
#3050=FACE_OUTER_BOUND('',#4655,.T.);
#3051=FACE_OUTER_BOUND('',#4657,.T.);
#3052=FACE_OUTER_BOUND('',#4658,.T.);
#3053=FACE_OUTER_BOUND('',#4659,.T.);
#3054=FACE_OUTER_BOUND('',#4660,.T.);
#3055=FACE_OUTER_BOUND('',#4661,.T.);
#3056=FACE_OUTER_BOUND('',#4662,.T.);
#3057=FACE_OUTER_BOUND('',#4663,.T.);
#3058=FACE_OUTER_BOUND('',#4664,.T.);
#3059=FACE_OUTER_BOUND('',#4665,.T.);
#3060=FACE_OUTER_BOUND('',#4666,.T.);
#3061=FACE_OUTER_BOUND('',#4667,.T.);
#3062=FACE_OUTER_BOUND('',#4668,.T.);
#3063=FACE_OUTER_BOUND('',#4669,.T.);
#3064=FACE_OUTER_BOUND('',#4670,.T.);
#3065=FACE_OUTER_BOUND('',#4671,.T.);
#3066=FACE_OUTER_BOUND('',#4673,.T.);
#3067=FACE_OUTER_BOUND('',#4675,.T.);
#3068=FACE_OUTER_BOUND('',#4676,.T.);
#3069=FACE_OUTER_BOUND('',#4677,.T.);
#3070=FACE_OUTER_BOUND('',#4678,.T.);
#3071=FACE_OUTER_BOUND('',#4680,.T.);
#3072=FACE_OUTER_BOUND('',#4681,.T.);
#3073=FACE_OUTER_BOUND('',#4682,.T.);
#3074=FACE_OUTER_BOUND('',#4684,.T.);
#3075=FACE_OUTER_BOUND('',#4685,.T.);
#3076=FACE_OUTER_BOUND('',#4686,.T.);
#3077=FACE_OUTER_BOUND('',#4688,.T.);
#3078=FACE_OUTER_BOUND('',#4689,.T.);
#3079=FACE_OUTER_BOUND('',#4691,.T.);
#3080=FACE_OUTER_BOUND('',#4692,.T.);
#3081=FACE_OUTER_BOUND('',#4693,.T.);
#3082=FACE_OUTER_BOUND('',#4694,.T.);
#3083=FACE_OUTER_BOUND('',#4695,.T.);
#3084=FACE_OUTER_BOUND('',#4697,.T.);
#3085=FACE_OUTER_BOUND('',#4698,.T.);
#3086=FACE_OUTER_BOUND('',#4699,.T.);
#3087=FACE_OUTER_BOUND('',#4701,.T.);
#3088=FACE_OUTER_BOUND('',#4702,.T.);
#3089=FACE_OUTER_BOUND('',#4703,.T.);
#3090=FACE_OUTER_BOUND('',#4704,.T.);
#3091=FACE_OUTER_BOUND('',#4710,.T.);
#3092=FACE_OUTER_BOUND('',#4711,.T.);
#3093=FACE_OUTER_BOUND('',#4712,.T.);
#3094=FACE_OUTER_BOUND('',#4713,.T.);
#3095=FACE_OUTER_BOUND('',#4714,.T.);
#3096=FACE_OUTER_BOUND('',#4715,.T.);
#3097=FACE_OUTER_BOUND('',#4721,.T.);
#3098=FACE_OUTER_BOUND('',#4722,.T.);
#3099=FACE_OUTER_BOUND('',#4723,.T.);
#3100=FACE_OUTER_BOUND('',#4724,.T.);
#3101=FACE_OUTER_BOUND('',#4725,.T.);
#3102=FACE_OUTER_BOUND('',#4727,.T.);
#3103=FACE_OUTER_BOUND('',#4728,.T.);
#3104=FACE_OUTER_BOUND('',#4729,.T.);
#3105=FACE_OUTER_BOUND('',#4730,.T.);
#3106=FACE_OUTER_BOUND('',#4731,.T.);
#3107=FACE_OUTER_BOUND('',#4732,.T.);
#3108=FACE_OUTER_BOUND('',#4733,.T.);
#3109=FACE_OUTER_BOUND('',#4734,.T.);
#3110=FACE_OUTER_BOUND('',#4735,.T.);
#3111=FACE_OUTER_BOUND('',#4737,.T.);
#3112=FACE_OUTER_BOUND('',#4738,.T.);
#3113=FACE_OUTER_BOUND('',#4740,.T.);
#3114=FACE_OUTER_BOUND('',#4741,.T.);
#3115=FACE_OUTER_BOUND('',#4746,.T.);
#3116=FACE_OUTER_BOUND('',#4747,.T.);
#3117=FACE_OUTER_BOUND('',#4748,.T.);
#3118=FACE_OUTER_BOUND('',#4749,.T.);
#3119=FACE_OUTER_BOUND('',#4750,.T.);
#3120=FACE_OUTER_BOUND('',#4752,.T.);
#3121=FACE_OUTER_BOUND('',#4753,.T.);
#3122=FACE_OUTER_BOUND('',#4755,.T.);
#3123=FACE_OUTER_BOUND('',#4756,.T.);
#3124=FACE_OUTER_BOUND('',#4757,.T.);
#3125=FACE_OUTER_BOUND('',#4758,.T.);
#3126=FACE_OUTER_BOUND('',#4759,.T.);
#3127=FACE_OUTER_BOUND('',#4760,.T.);
#3128=FACE_OUTER_BOUND('',#4761,.T.);
#3129=FACE_OUTER_BOUND('',#4762,.T.);
#3130=FACE_OUTER_BOUND('',#4763,.T.);
#3131=FACE_OUTER_BOUND('',#4764,.T.);
#3132=FACE_OUTER_BOUND('',#4765,.T.);
#3133=FACE_OUTER_BOUND('',#4766,.T.);
#3134=FACE_OUTER_BOUND('',#4767,.T.);
#3135=FACE_OUTER_BOUND('',#4768,.T.);
#3136=FACE_OUTER_BOUND('',#4770,.T.);
#3137=FACE_OUTER_BOUND('',#4771,.T.);
#3138=FACE_OUTER_BOUND('',#4772,.T.);
#3139=FACE_OUTER_BOUND('',#4773,.T.);
#3140=FACE_OUTER_BOUND('',#4774,.T.);
#3141=FACE_OUTER_BOUND('',#4775,.T.);
#3142=FACE_OUTER_BOUND('',#4776,.T.);
#3143=FACE_OUTER_BOUND('',#4777,.T.);
#3144=FACE_OUTER_BOUND('',#4778,.T.);
#3145=FACE_OUTER_BOUND('',#4779,.T.);
#3146=FACE_OUTER_BOUND('',#4780,.T.);
#3147=FACE_OUTER_BOUND('',#4781,.T.);
#3148=FACE_OUTER_BOUND('',#4782,.T.);
#3149=FACE_OUTER_BOUND('',#4783,.T.);
#3150=FACE_OUTER_BOUND('',#4784,.T.);
#3151=FACE_OUTER_BOUND('',#4785,.T.);
#3152=FACE_OUTER_BOUND('',#4786,.T.);
#3153=FACE_OUTER_BOUND('',#4787,.T.);
#3154=FACE_OUTER_BOUND('',#4788,.T.);
#3155=FACE_OUTER_BOUND('',#4789,.T.);
#3156=FACE_OUTER_BOUND('',#4790,.T.);
#3157=FACE_OUTER_BOUND('',#4791,.T.);
#3158=FACE_OUTER_BOUND('',#4792,.T.);
#3159=FACE_OUTER_BOUND('',#4793,.T.);
#3160=FACE_OUTER_BOUND('',#4794,.T.);
#3161=FACE_OUTER_BOUND('',#4795,.T.);
#3162=FACE_OUTER_BOUND('',#4796,.T.);
#3163=FACE_OUTER_BOUND('',#4797,.T.);
#3164=FACE_OUTER_BOUND('',#4798,.T.);
#3165=FACE_OUTER_BOUND('',#4799,.T.);
#3166=FACE_OUTER_BOUND('',#4800,.T.);
#3167=FACE_OUTER_BOUND('',#4801,.T.);
#3168=FACE_OUTER_BOUND('',#4802,.T.);
#3169=FACE_OUTER_BOUND('',#4803,.T.);
#3170=FACE_OUTER_BOUND('',#4804,.T.);
#3171=FACE_OUTER_BOUND('',#4805,.T.);
#3172=FACE_OUTER_BOUND('',#4806,.T.);
#3173=FACE_OUTER_BOUND('',#4807,.T.);
#3174=FACE_OUTER_BOUND('',#4808,.T.);
#3175=FACE_OUTER_BOUND('',#4810,.T.);
#3176=FACE_OUTER_BOUND('',#4811,.T.);
#3177=FACE_OUTER_BOUND('',#4812,.T.);
#3178=FACE_OUTER_BOUND('',#4813,.T.);
#3179=FACE_OUTER_BOUND('',#4814,.T.);
#3180=FACE_OUTER_BOUND('',#4815,.T.);
#3181=FACE_OUTER_BOUND('',#4816,.T.);
#3182=FACE_OUTER_BOUND('',#4817,.T.);
#3183=FACE_OUTER_BOUND('',#4818,.T.);
#3184=FACE_OUTER_BOUND('',#4819,.T.);
#3185=FACE_OUTER_BOUND('',#4820,.T.);
#3186=FACE_OUTER_BOUND('',#4821,.T.);
#3187=FACE_OUTER_BOUND('',#4822,.T.);
#3188=FACE_OUTER_BOUND('',#4823,.T.);
#3189=FACE_OUTER_BOUND('',#4824,.T.);
#3190=FACE_OUTER_BOUND('',#4825,.T.);
#3191=FACE_OUTER_BOUND('',#4826,.T.);
#3192=FACE_OUTER_BOUND('',#4827,.T.);
#3193=FACE_OUTER_BOUND('',#4828,.T.);
#3194=FACE_OUTER_BOUND('',#4829,.T.);
#3195=FACE_OUTER_BOUND('',#4830,.T.);
#3196=FACE_OUTER_BOUND('',#4831,.T.);
#3197=FACE_OUTER_BOUND('',#4832,.T.);
#3198=FACE_OUTER_BOUND('',#4833,.T.);
#3199=FACE_OUTER_BOUND('',#4834,.T.);
#3200=FACE_OUTER_BOUND('',#4835,.T.);
#3201=FACE_OUTER_BOUND('',#4836,.T.);
#3202=FACE_OUTER_BOUND('',#4837,.T.);
#3203=FACE_OUTER_BOUND('',#4838,.T.);
#3204=FACE_OUTER_BOUND('',#4839,.T.);
#3205=FACE_OUTER_BOUND('',#4840,.T.);
#3206=FACE_OUTER_BOUND('',#4841,.T.);
#3207=FACE_OUTER_BOUND('',#4842,.T.);
#3208=FACE_OUTER_BOUND('',#4843,.T.);
#3209=FACE_OUTER_BOUND('',#4844,.T.);
#3210=FACE_OUTER_BOUND('',#4845,.T.);
#3211=FACE_OUTER_BOUND('',#4846,.T.);
#3212=FACE_OUTER_BOUND('',#4847,.T.);
#3213=FACE_OUTER_BOUND('',#4848,.T.);
#3214=FACE_OUTER_BOUND('',#4849,.T.);
#3215=FACE_OUTER_BOUND('',#4850,.T.);
#3216=FACE_OUTER_BOUND('',#4851,.T.);
#3217=FACE_OUTER_BOUND('',#4852,.T.);
#3218=FACE_OUTER_BOUND('',#4853,.T.);
#3219=FACE_OUTER_BOUND('',#4854,.T.);
#3220=FACE_OUTER_BOUND('',#4855,.T.);
#3221=FACE_OUTER_BOUND('',#4856,.T.);
#3222=FACE_OUTER_BOUND('',#4857,.T.);
#3223=FACE_OUTER_BOUND('',#4858,.T.);
#3224=FACE_OUTER_BOUND('',#4859,.T.);
#3225=FACE_OUTER_BOUND('',#4860,.T.);
#3226=FACE_OUTER_BOUND('',#4861,.T.);
#3227=FACE_OUTER_BOUND('',#4862,.T.);
#3228=FACE_OUTER_BOUND('',#4863,.T.);
#3229=FACE_OUTER_BOUND('',#4864,.T.);
#3230=FACE_OUTER_BOUND('',#4865,.T.);
#3231=FACE_OUTER_BOUND('',#4866,.T.);
#3232=FACE_OUTER_BOUND('',#4867,.T.);
#3233=FACE_OUTER_BOUND('',#4868,.T.);
#3234=FACE_OUTER_BOUND('',#4869,.T.);
#3235=FACE_OUTER_BOUND('',#4870,.T.);
#3236=FACE_OUTER_BOUND('',#4871,.T.);
#3237=FACE_OUTER_BOUND('',#4872,.T.);
#3238=FACE_OUTER_BOUND('',#4873,.T.);
#3239=FACE_OUTER_BOUND('',#4874,.T.);
#3240=FACE_OUTER_BOUND('',#4875,.T.);
#3241=FACE_OUTER_BOUND('',#4876,.T.);
#3242=FACE_OUTER_BOUND('',#4877,.T.);
#3243=FACE_OUTER_BOUND('',#4878,.T.);
#3244=FACE_OUTER_BOUND('',#4879,.T.);
#3245=FACE_OUTER_BOUND('',#4880,.T.);
#3246=FACE_OUTER_BOUND('',#4881,.T.);
#3247=FACE_OUTER_BOUND('',#4882,.T.);
#3248=FACE_OUTER_BOUND('',#4883,.T.);
#3249=FACE_OUTER_BOUND('',#4884,.T.);
#3250=FACE_OUTER_BOUND('',#4885,.T.);
#3251=FACE_OUTER_BOUND('',#4886,.T.);
#3252=FACE_OUTER_BOUND('',#4887,.T.);
#3253=FACE_OUTER_BOUND('',#4888,.T.);
#3254=FACE_OUTER_BOUND('',#4889,.T.);
#3255=FACE_OUTER_BOUND('',#4890,.T.);
#3256=FACE_OUTER_BOUND('',#4891,.T.);
#3257=FACE_OUTER_BOUND('',#4892,.T.);
#3258=FACE_OUTER_BOUND('',#4893,.T.);
#3259=FACE_OUTER_BOUND('',#4894,.T.);
#3260=FACE_OUTER_BOUND('',#4895,.T.);
#3261=FACE_OUTER_BOUND('',#4896,.T.);
#3262=FACE_OUTER_BOUND('',#4897,.T.);
#3263=FACE_OUTER_BOUND('',#4898,.T.);
#3264=FACE_OUTER_BOUND('',#4899,.T.);
#3265=FACE_OUTER_BOUND('',#4900,.T.);
#3266=FACE_OUTER_BOUND('',#4901,.T.);
#3267=FACE_OUTER_BOUND('',#4902,.T.);
#3268=FACE_OUTER_BOUND('',#4903,.T.);
#3269=FACE_OUTER_BOUND('',#4904,.T.);
#3270=FACE_OUTER_BOUND('',#4905,.T.);
#3271=FACE_OUTER_BOUND('',#4906,.T.);
#3272=FACE_OUTER_BOUND('',#4907,.T.);
#3273=FACE_OUTER_BOUND('',#4908,.T.);
#3274=FACE_OUTER_BOUND('',#4909,.T.);
#3275=FACE_OUTER_BOUND('',#4910,.T.);
#3276=FACE_OUTER_BOUND('',#4911,.T.);
#3277=FACE_OUTER_BOUND('',#4912,.T.);
#3278=FACE_OUTER_BOUND('',#4913,.T.);
#3279=FACE_OUTER_BOUND('',#4914,.T.);
#3280=FACE_OUTER_BOUND('',#4915,.T.);
#3281=FACE_OUTER_BOUND('',#4916,.T.);
#3282=FACE_OUTER_BOUND('',#4917,.T.);
#3283=FACE_OUTER_BOUND('',#4918,.T.);
#3284=FACE_OUTER_BOUND('',#4919,.T.);
#3285=FACE_OUTER_BOUND('',#4920,.T.);
#3286=FACE_OUTER_BOUND('',#4921,.T.);
#3287=FACE_OUTER_BOUND('',#4922,.T.);
#3288=FACE_OUTER_BOUND('',#4923,.T.);
#3289=FACE_OUTER_BOUND('',#4924,.T.);
#3290=FACE_OUTER_BOUND('',#4925,.T.);
#3291=FACE_OUTER_BOUND('',#4926,.T.);
#3292=FACE_OUTER_BOUND('',#4927,.T.);
#3293=FACE_OUTER_BOUND('',#4928,.T.);
#3294=FACE_OUTER_BOUND('',#4929,.T.);
#3295=FACE_OUTER_BOUND('',#4930,.T.);
#3296=FACE_OUTER_BOUND('',#4931,.T.);
#3297=FACE_OUTER_BOUND('',#4932,.T.);
#3298=FACE_OUTER_BOUND('',#4933,.T.);
#3299=FACE_OUTER_BOUND('',#4934,.T.);
#3300=FACE_OUTER_BOUND('',#4935,.T.);
#3301=FACE_OUTER_BOUND('',#4936,.T.);
#3302=FACE_OUTER_BOUND('',#4937,.T.);
#3303=FACE_OUTER_BOUND('',#4938,.T.);
#3304=FACE_OUTER_BOUND('',#4939,.T.);
#3305=FACE_OUTER_BOUND('',#4940,.T.);
#3306=FACE_OUTER_BOUND('',#4941,.T.);
#3307=FACE_OUTER_BOUND('',#4942,.T.);
#3308=FACE_OUTER_BOUND('',#4943,.T.);
#3309=FACE_OUTER_BOUND('',#4944,.T.);
#3310=FACE_OUTER_BOUND('',#4945,.T.);
#3311=FACE_OUTER_BOUND('',#4946,.T.);
#3312=FACE_OUTER_BOUND('',#4947,.T.);
#3313=FACE_OUTER_BOUND('',#4948,.T.);
#3314=FACE_OUTER_BOUND('',#4949,.T.);
#3315=FACE_OUTER_BOUND('',#4950,.T.);
#3316=FACE_OUTER_BOUND('',#4951,.T.);
#3317=FACE_OUTER_BOUND('',#4952,.T.);
#3318=FACE_OUTER_BOUND('',#4953,.T.);
#3319=FACE_OUTER_BOUND('',#4954,.T.);
#3320=FACE_OUTER_BOUND('',#4955,.T.);
#3321=FACE_OUTER_BOUND('',#4956,.T.);
#3322=FACE_OUTER_BOUND('',#4957,.T.);
#3323=FACE_OUTER_BOUND('',#4958,.T.);
#3324=FACE_OUTER_BOUND('',#4959,.T.);
#3325=FACE_OUTER_BOUND('',#4960,.T.);
#3326=FACE_OUTER_BOUND('',#4961,.T.);
#3327=FACE_OUTER_BOUND('',#4962,.T.);
#3328=FACE_OUTER_BOUND('',#4963,.T.);
#3329=FACE_OUTER_BOUND('',#4964,.T.);
#3330=FACE_OUTER_BOUND('',#4965,.T.);
#3331=FACE_OUTER_BOUND('',#4966,.T.);
#3332=FACE_OUTER_BOUND('',#4967,.T.);
#3333=FACE_OUTER_BOUND('',#4968,.T.);
#3334=FACE_OUTER_BOUND('',#4969,.T.);
#3335=FACE_OUTER_BOUND('',#4970,.T.);
#3336=FACE_OUTER_BOUND('',#4971,.T.);
#3337=FACE_OUTER_BOUND('',#4972,.T.);
#3338=FACE_OUTER_BOUND('',#4974,.T.);
#3339=FACE_OUTER_BOUND('',#4975,.T.);
#3340=FACE_OUTER_BOUND('',#4976,.T.);
#3341=FACE_OUTER_BOUND('',#4977,.T.);
#3342=FACE_OUTER_BOUND('',#4978,.T.);
#3343=FACE_OUTER_BOUND('',#4979,.T.);
#3344=FACE_OUTER_BOUND('',#4980,.T.);
#3345=FACE_OUTER_BOUND('',#4981,.T.);
#3346=FACE_OUTER_BOUND('',#4982,.T.);
#3347=FACE_OUTER_BOUND('',#4983,.T.);
#3348=FACE_OUTER_BOUND('',#4984,.T.);
#3349=FACE_OUTER_BOUND('',#4985,.T.);
#3350=FACE_OUTER_BOUND('',#4986,.T.);
#3351=FACE_OUTER_BOUND('',#4987,.T.);
#3352=FACE_OUTER_BOUND('',#4988,.T.);
#3353=FACE_OUTER_BOUND('',#4989,.T.);
#3354=FACE_OUTER_BOUND('',#4990,.T.);
#3355=FACE_OUTER_BOUND('',#4991,.T.);
#3356=FACE_OUTER_BOUND('',#4992,.T.);
#3357=FACE_OUTER_BOUND('',#4993,.T.);
#3358=FACE_OUTER_BOUND('',#4994,.T.);
#3359=FACE_OUTER_BOUND('',#4995,.T.);
#3360=FACE_OUTER_BOUND('',#4996,.T.);
#3361=FACE_OUTER_BOUND('',#4997,.T.);
#3362=FACE_OUTER_BOUND('',#4998,.T.);
#3363=FACE_OUTER_BOUND('',#4999,.T.);
#3364=FACE_OUTER_BOUND('',#5000,.T.);
#3365=FACE_OUTER_BOUND('',#5001,.T.);
#3366=FACE_OUTER_BOUND('',#5002,.T.);
#3367=FACE_OUTER_BOUND('',#5003,.T.);
#3368=FACE_OUTER_BOUND('',#5004,.T.);
#3369=FACE_OUTER_BOUND('',#5005,.T.);
#3370=FACE_OUTER_BOUND('',#5006,.T.);
#3371=FACE_OUTER_BOUND('',#5007,.T.);
#3372=FACE_OUTER_BOUND('',#5008,.T.);
#3373=FACE_OUTER_BOUND('',#5009,.T.);
#3374=FACE_OUTER_BOUND('',#5010,.T.);
#3375=FACE_OUTER_BOUND('',#5011,.T.);
#3376=FACE_OUTER_BOUND('',#5012,.T.);
#3377=FACE_OUTER_BOUND('',#5013,.T.);
#3378=FACE_OUTER_BOUND('',#5014,.T.);
#3379=FACE_OUTER_BOUND('',#5015,.T.);
#3380=FACE_OUTER_BOUND('',#5016,.T.);
#3381=FACE_OUTER_BOUND('',#5017,.T.);
#3382=FACE_OUTER_BOUND('',#5018,.T.);
#3383=FACE_OUTER_BOUND('',#5019,.T.);
#3384=FACE_OUTER_BOUND('',#5020,.T.);
#3385=FACE_OUTER_BOUND('',#5022,.T.);
#3386=FACE_OUTER_BOUND('',#5023,.T.);
#3387=FACE_OUTER_BOUND('',#5024,.T.);
#3388=FACE_OUTER_BOUND('',#5025,.T.);
#3389=FACE_OUTER_BOUND('',#5026,.T.);
#3390=FACE_OUTER_BOUND('',#5027,.T.);
#3391=FACE_OUTER_BOUND('',#5028,.T.);
#3392=FACE_OUTER_BOUND('',#5029,.T.);
#3393=FACE_OUTER_BOUND('',#5030,.T.);
#3394=FACE_OUTER_BOUND('',#5031,.T.);
#3395=FACE_OUTER_BOUND('',#5032,.T.);
#3396=FACE_OUTER_BOUND('',#5033,.T.);
#3397=FACE_OUTER_BOUND('',#5034,.T.);
#3398=FACE_OUTER_BOUND('',#5035,.T.);
#3399=FACE_OUTER_BOUND('',#5036,.T.);
#3400=FACE_OUTER_BOUND('',#5037,.T.);
#3401=FACE_OUTER_BOUND('',#5038,.T.);
#3402=FACE_OUTER_BOUND('',#5039,.T.);
#3403=FACE_OUTER_BOUND('',#5040,.T.);
#3404=FACE_OUTER_BOUND('',#5041,.T.);
#3405=FACE_OUTER_BOUND('',#5042,.T.);
#3406=FACE_OUTER_BOUND('',#5043,.T.);
#3407=FACE_OUTER_BOUND('',#5044,.T.);
#3408=FACE_OUTER_BOUND('',#5045,.T.);
#3409=FACE_OUTER_BOUND('',#5046,.T.);
#3410=FACE_OUTER_BOUND('',#5047,.T.);
#3411=FACE_OUTER_BOUND('',#5048,.T.);
#3412=FACE_OUTER_BOUND('',#5049,.T.);
#3413=FACE_OUTER_BOUND('',#5050,.T.);
#3414=FACE_OUTER_BOUND('',#5051,.T.);
#3415=FACE_OUTER_BOUND('',#5052,.T.);
#3416=FACE_OUTER_BOUND('',#5053,.T.);
#3417=FACE_OUTER_BOUND('',#5054,.T.);
#3418=FACE_OUTER_BOUND('',#5055,.T.);
#3419=FACE_OUTER_BOUND('',#5056,.T.);
#3420=FACE_OUTER_BOUND('',#5057,.T.);
#3421=FACE_OUTER_BOUND('',#5058,.T.);
#3422=FACE_OUTER_BOUND('',#5059,.T.);
#3423=FACE_OUTER_BOUND('',#5061,.T.);
#3424=FACE_OUTER_BOUND('',#5062,.T.);
#3425=FACE_OUTER_BOUND('',#5063,.T.);
#3426=FACE_OUTER_BOUND('',#5064,.T.);
#3427=FACE_OUTER_BOUND('',#5065,.T.);
#3428=FACE_OUTER_BOUND('',#5066,.T.);
#3429=FACE_OUTER_BOUND('',#5067,.T.);
#3430=FACE_OUTER_BOUND('',#5068,.T.);
#3431=FACE_OUTER_BOUND('',#5070,.T.);
#3432=FACE_OUTER_BOUND('',#5071,.T.);
#3433=FACE_OUTER_BOUND('',#5072,.T.);
#3434=FACE_OUTER_BOUND('',#5073,.T.);
#3435=FACE_OUTER_BOUND('',#5074,.T.);
#3436=FACE_OUTER_BOUND('',#5075,.T.);
#3437=FACE_OUTER_BOUND('',#5076,.T.);
#3438=FACE_OUTER_BOUND('',#5077,.T.);
#3439=FACE_OUTER_BOUND('',#5078,.T.);
#3440=FACE_OUTER_BOUND('',#5079,.T.);
#3441=FACE_OUTER_BOUND('',#5080,.T.);
#3442=FACE_OUTER_BOUND('',#5081,.T.);
#3443=FACE_OUTER_BOUND('',#5082,.T.);
#3444=FACE_OUTER_BOUND('',#5083,.T.);
#3445=FACE_OUTER_BOUND('',#5084,.T.);
#3446=FACE_OUTER_BOUND('',#5085,.T.);
#3447=FACE_OUTER_BOUND('',#5086,.T.);
#3448=FACE_OUTER_BOUND('',#5087,.T.);
#3449=FACE_OUTER_BOUND('',#5088,.T.);
#3450=FACE_OUTER_BOUND('',#5089,.T.);
#3451=FACE_OUTER_BOUND('',#5090,.T.);
#3452=FACE_OUTER_BOUND('',#5091,.T.);
#3453=FACE_OUTER_BOUND('',#5092,.T.);
#3454=FACE_OUTER_BOUND('',#5093,.T.);
#3455=FACE_OUTER_BOUND('',#5094,.T.);
#3456=FACE_OUTER_BOUND('',#5095,.T.);
#3457=FACE_OUTER_BOUND('',#5096,.T.);
#3458=FACE_OUTER_BOUND('',#5097,.T.);
#3459=FACE_OUTER_BOUND('',#5098,.T.);
#3460=FACE_OUTER_BOUND('',#5099,.T.);
#3461=FACE_OUTER_BOUND('',#5100,.T.);
#3462=FACE_OUTER_BOUND('',#5101,.T.);
#3463=FACE_OUTER_BOUND('',#5102,.T.);
#3464=FACE_OUTER_BOUND('',#5103,.T.);
#3465=FACE_OUTER_BOUND('',#5104,.T.);
#3466=FACE_OUTER_BOUND('',#5105,.T.);
#3467=FACE_OUTER_BOUND('',#5106,.T.);
#3468=FACE_OUTER_BOUND('',#5107,.T.);
#3469=FACE_OUTER_BOUND('',#5108,.T.);
#3470=FACE_OUTER_BOUND('',#5109,.T.);
#3471=FACE_OUTER_BOUND('',#5110,.T.);
#3472=FACE_OUTER_BOUND('',#5111,.T.);
#3473=FACE_OUTER_BOUND('',#5112,.T.);
#3474=FACE_OUTER_BOUND('',#5113,.T.);
#3475=FACE_OUTER_BOUND('',#5114,.T.);
#3476=FACE_OUTER_BOUND('',#5115,.T.);
#3477=FACE_OUTER_BOUND('',#5116,.T.);
#3478=FACE_OUTER_BOUND('',#5117,.T.);
#3479=FACE_OUTER_BOUND('',#5118,.T.);
#3480=FACE_OUTER_BOUND('',#5119,.T.);
#3481=FACE_OUTER_BOUND('',#5120,.T.);
#3482=FACE_OUTER_BOUND('',#5121,.T.);
#3483=FACE_OUTER_BOUND('',#5122,.T.);
#3484=FACE_OUTER_BOUND('',#5123,.T.);
#3485=FACE_OUTER_BOUND('',#5124,.T.);
#3486=FACE_OUTER_BOUND('',#5125,.T.);
#3487=FACE_OUTER_BOUND('',#5126,.T.);
#3488=FACE_OUTER_BOUND('',#5127,.T.);
#3489=FACE_OUTER_BOUND('',#5128,.T.);
#3490=FACE_OUTER_BOUND('',#5129,.T.);
#3491=FACE_OUTER_BOUND('',#5130,.T.);
#3492=FACE_OUTER_BOUND('',#5131,.T.);
#3493=FACE_OUTER_BOUND('',#5132,.T.);
#3494=FACE_OUTER_BOUND('',#5133,.T.);
#3495=FACE_OUTER_BOUND('',#5134,.T.);
#3496=FACE_OUTER_BOUND('',#5135,.T.);
#3497=FACE_OUTER_BOUND('',#5136,.T.);
#3498=FACE_OUTER_BOUND('',#5137,.T.);
#3499=FACE_OUTER_BOUND('',#5138,.T.);
#3500=FACE_OUTER_BOUND('',#5139,.T.);
#3501=FACE_OUTER_BOUND('',#5140,.T.);
#3502=FACE_OUTER_BOUND('',#5141,.T.);
#3503=FACE_OUTER_BOUND('',#5143,.T.);
#3504=FACE_OUTER_BOUND('',#5144,.T.);
#3505=FACE_OUTER_BOUND('',#5145,.T.);
#3506=FACE_OUTER_BOUND('',#5146,.T.);
#3507=FACE_OUTER_BOUND('',#5147,.T.);
#3508=FACE_OUTER_BOUND('',#5148,.T.);
#3509=FACE_OUTER_BOUND('',#5149,.T.);
#3510=FACE_OUTER_BOUND('',#5150,.T.);
#3511=FACE_OUTER_BOUND('',#5152,.T.);
#3512=FACE_OUTER_BOUND('',#5153,.T.);
#3513=FACE_OUTER_BOUND('',#5154,.T.);
#3514=FACE_OUTER_BOUND('',#5155,.T.);
#3515=FACE_OUTER_BOUND('',#5157,.T.);
#3516=FACE_OUTER_BOUND('',#5158,.T.);
#3517=FACE_OUTER_BOUND('',#5159,.T.);
#3518=FACE_OUTER_BOUND('',#5160,.T.);
#3519=FACE_OUTER_BOUND('',#5161,.T.);
#3520=FACE_OUTER_BOUND('',#5162,.T.);
#3521=FACE_OUTER_BOUND('',#5164,.T.);
#3522=FACE_OUTER_BOUND('',#5165,.T.);
#3523=FACE_OUTER_BOUND('',#5166,.T.);
#3524=FACE_OUTER_BOUND('',#5167,.T.);
#3525=FACE_OUTER_BOUND('',#5168,.T.);
#3526=FACE_OUTER_BOUND('',#5169,.T.);
#3527=FACE_OUTER_BOUND('',#5170,.T.);
#3528=FACE_OUTER_BOUND('',#5171,.T.);
#3529=FACE_OUTER_BOUND('',#5172,.T.);
#3530=FACE_OUTER_BOUND('',#5173,.T.);
#3531=FACE_OUTER_BOUND('',#5174,.T.);
#3532=FACE_OUTER_BOUND('',#5175,.T.);
#3533=FACE_OUTER_BOUND('',#5176,.T.);
#3534=FACE_OUTER_BOUND('',#5177,.T.);
#3535=FACE_OUTER_BOUND('',#5178,.T.);
#3536=FACE_OUTER_BOUND('',#5179,.T.);
#3537=FACE_OUTER_BOUND('',#5180,.T.);
#3538=FACE_OUTER_BOUND('',#5181,.T.);
#3539=FACE_OUTER_BOUND('',#5182,.T.);
#3540=FACE_OUTER_BOUND('',#5183,.T.);
#3541=FACE_OUTER_BOUND('',#5184,.T.);
#3542=FACE_OUTER_BOUND('',#5185,.T.);
#3543=FACE_OUTER_BOUND('',#5186,.T.);
#3544=FACE_OUTER_BOUND('',#5187,.T.);
#3545=FACE_OUTER_BOUND('',#5188,.T.);
#3546=FACE_OUTER_BOUND('',#5189,.T.);
#3547=FACE_OUTER_BOUND('',#5190,.T.);
#3548=FACE_OUTER_BOUND('',#5191,.T.);
#3549=FACE_OUTER_BOUND('',#5192,.T.);
#3550=FACE_OUTER_BOUND('',#5193,.T.);
#3551=FACE_OUTER_BOUND('',#5194,.T.);
#3552=FACE_OUTER_BOUND('',#5195,.T.);
#3553=FACE_OUTER_BOUND('',#5196,.T.);
#3554=FACE_OUTER_BOUND('',#5197,.T.);
#3555=FACE_OUTER_BOUND('',#5198,.T.);
#3556=FACE_OUTER_BOUND('',#5199,.T.);
#3557=FACE_OUTER_BOUND('',#5200,.T.);
#3558=FACE_OUTER_BOUND('',#5201,.T.);
#3559=FACE_OUTER_BOUND('',#5202,.T.);
#3560=FACE_OUTER_BOUND('',#5203,.T.);
#3561=FACE_OUTER_BOUND('',#5204,.T.);
#3562=FACE_OUTER_BOUND('',#5205,.T.);
#3563=FACE_OUTER_BOUND('',#5206,.T.);
#3564=FACE_OUTER_BOUND('',#5207,.T.);
#3565=FACE_OUTER_BOUND('',#5208,.T.);
#3566=FACE_OUTER_BOUND('',#5209,.T.);
#3567=FACE_OUTER_BOUND('',#5210,.T.);
#3568=FACE_OUTER_BOUND('',#5211,.T.);
#3569=FACE_OUTER_BOUND('',#5212,.T.);
#3570=FACE_OUTER_BOUND('',#5213,.T.);
#3571=FACE_OUTER_BOUND('',#5214,.T.);
#3572=FACE_OUTER_BOUND('',#5215,.T.);
#3573=FACE_OUTER_BOUND('',#5216,.T.);
#3574=FACE_OUTER_BOUND('',#5218,.T.);
#3575=FACE_OUTER_BOUND('',#5219,.T.);
#3576=FACE_OUTER_BOUND('',#5220,.T.);
#3577=FACE_OUTER_BOUND('',#5222,.T.);
#3578=FACE_OUTER_BOUND('',#5223,.T.);
#3579=FACE_OUTER_BOUND('',#5225,.T.);
#3580=FACE_OUTER_BOUND('',#5226,.T.);
#3581=FACE_OUTER_BOUND('',#5227,.T.);
#3582=FACE_OUTER_BOUND('',#5229,.T.);
#3583=FACE_OUTER_BOUND('',#5230,.T.);
#3584=FACE_OUTER_BOUND('',#5232,.T.);
#3585=FACE_OUTER_BOUND('',#5233,.T.);
#3586=FACE_OUTER_BOUND('',#5235,.T.);
#3587=FACE_OUTER_BOUND('',#5236,.T.);
#3588=FACE_OUTER_BOUND('',#5237,.T.);
#3589=FACE_OUTER_BOUND('',#5238,.T.);
#3590=FACE_OUTER_BOUND('',#5239,.T.);
#3591=FACE_OUTER_BOUND('',#5240,.T.);
#3592=FACE_OUTER_BOUND('',#5241,.T.);
#3593=FACE_OUTER_BOUND('',#5242,.T.);
#3594=FACE_OUTER_BOUND('',#5243,.T.);
#3595=FACE_OUTER_BOUND('',#5244,.T.);
#3596=FACE_OUTER_BOUND('',#5245,.T.);
#3597=FACE_OUTER_BOUND('',#5246,.T.);
#3598=FACE_OUTER_BOUND('',#5247,.T.);
#3599=FACE_OUTER_BOUND('',#5248,.T.);
#3600=FACE_OUTER_BOUND('',#5249,.T.);
#3601=FACE_OUTER_BOUND('',#5250,.T.);
#3602=FACE_OUTER_BOUND('',#5251,.T.);
#3603=FACE_OUTER_BOUND('',#5252,.T.);
#3604=FACE_OUTER_BOUND('',#5253,.T.);
#3605=FACE_OUTER_BOUND('',#5254,.T.);
#3606=FACE_OUTER_BOUND('',#5255,.T.);
#3607=FACE_OUTER_BOUND('',#5256,.T.);
#3608=FACE_OUTER_BOUND('',#5257,.T.);
#3609=FACE_OUTER_BOUND('',#5258,.T.);
#3610=FACE_OUTER_BOUND('',#5259,.T.);
#3611=FACE_OUTER_BOUND('',#5260,.T.);
#3612=FACE_OUTER_BOUND('',#5261,.T.);
#3613=FACE_OUTER_BOUND('',#5262,.T.);
#3614=FACE_OUTER_BOUND('',#5263,.T.);
#3615=FACE_OUTER_BOUND('',#5264,.T.);
#3616=FACE_OUTER_BOUND('',#5265,.T.);
#3617=FACE_OUTER_BOUND('',#5266,.T.);
#3618=FACE_OUTER_BOUND('',#5267,.T.);
#3619=FACE_OUTER_BOUND('',#5268,.T.);
#3620=FACE_OUTER_BOUND('',#5269,.T.);
#3621=FACE_OUTER_BOUND('',#5270,.T.);
#3622=FACE_OUTER_BOUND('',#5271,.T.);
#3623=FACE_OUTER_BOUND('',#5272,.T.);
#3624=FACE_OUTER_BOUND('',#5273,.T.);
#3625=FACE_OUTER_BOUND('',#5274,.T.);
#3626=FACE_OUTER_BOUND('',#5275,.T.);
#3627=FACE_OUTER_BOUND('',#5276,.T.);
#3628=FACE_OUTER_BOUND('',#5277,.T.);
#3629=FACE_OUTER_BOUND('',#5278,.T.);
#3630=FACE_OUTER_BOUND('',#5279,.T.);
#3631=FACE_OUTER_BOUND('',#5280,.T.);
#3632=FACE_OUTER_BOUND('',#5281,.T.);
#3633=FACE_OUTER_BOUND('',#5282,.T.);
#3634=FACE_OUTER_BOUND('',#5283,.T.);
#3635=FACE_OUTER_BOUND('',#5284,.T.);
#3636=FACE_OUTER_BOUND('',#5285,.T.);
#3637=FACE_OUTER_BOUND('',#5286,.T.);
#3638=FACE_OUTER_BOUND('',#5287,.T.);
#3639=FACE_OUTER_BOUND('',#5288,.T.);
#3640=FACE_OUTER_BOUND('',#5290,.T.);
#3641=FACE_OUTER_BOUND('',#5291,.T.);
#3642=FACE_OUTER_BOUND('',#5292,.T.);
#3643=FACE_OUTER_BOUND('',#5293,.T.);
#3644=FACE_OUTER_BOUND('',#5294,.T.);
#3645=FACE_OUTER_BOUND('',#5295,.T.);
#3646=FACE_OUTER_BOUND('',#5296,.T.);
#3647=FACE_OUTER_BOUND('',#5297,.T.);
#3648=FACE_OUTER_BOUND('',#5299,.T.);
#3649=FACE_OUTER_BOUND('',#5300,.T.);
#3650=FACE_OUTER_BOUND('',#5301,.T.);
#3651=FACE_OUTER_BOUND('',#5302,.T.);
#3652=FACE_OUTER_BOUND('',#5303,.T.);
#3653=FACE_OUTER_BOUND('',#5304,.T.);
#3654=FACE_OUTER_BOUND('',#5305,.T.);
#3655=FACE_OUTER_BOUND('',#5306,.T.);
#3656=FACE_OUTER_BOUND('',#5307,.T.);
#3657=FACE_OUTER_BOUND('',#5308,.T.);
#3658=FACE_OUTER_BOUND('',#5309,.T.);
#3659=FACE_OUTER_BOUND('',#5310,.T.);
#3660=FACE_OUTER_BOUND('',#5311,.T.);
#3661=FACE_OUTER_BOUND('',#5312,.T.);
#3662=FACE_OUTER_BOUND('',#5313,.T.);
#3663=FACE_OUTER_BOUND('',#5314,.T.);
#3664=FACE_OUTER_BOUND('',#5315,.T.);
#3665=FACE_OUTER_BOUND('',#5316,.T.);
#3666=FACE_OUTER_BOUND('',#5317,.T.);
#3667=FACE_OUTER_BOUND('',#5318,.T.);
#3668=FACE_OUTER_BOUND('',#5319,.T.);
#3669=FACE_OUTER_BOUND('',#5320,.T.);
#3670=FACE_OUTER_BOUND('',#5321,.T.);
#3671=FACE_OUTER_BOUND('',#5322,.T.);
#3672=FACE_OUTER_BOUND('',#5323,.T.);
#3673=FACE_OUTER_BOUND('',#5324,.T.);
#3674=FACE_OUTER_BOUND('',#5325,.T.);
#3675=FACE_OUTER_BOUND('',#5326,.T.);
#3676=FACE_OUTER_BOUND('',#5327,.T.);
#3677=FACE_OUTER_BOUND('',#5328,.T.);
#3678=FACE_OUTER_BOUND('',#5329,.T.);
#3679=FACE_OUTER_BOUND('',#5330,.T.);
#3680=FACE_OUTER_BOUND('',#5331,.T.);
#3681=FACE_OUTER_BOUND('',#5332,.T.);
#3682=FACE_OUTER_BOUND('',#5333,.T.);
#3683=FACE_OUTER_BOUND('',#5334,.T.);
#3684=FACE_OUTER_BOUND('',#5335,.T.);
#3685=FACE_OUTER_BOUND('',#5336,.T.);
#3686=FACE_OUTER_BOUND('',#5337,.T.);
#3687=FACE_OUTER_BOUND('',#5338,.T.);
#3688=FACE_OUTER_BOUND('',#5339,.T.);
#3689=FACE_OUTER_BOUND('',#5340,.T.);
#3690=FACE_OUTER_BOUND('',#5341,.T.);
#3691=FACE_OUTER_BOUND('',#5342,.T.);
#3692=FACE_OUTER_BOUND('',#5343,.T.);
#3693=FACE_OUTER_BOUND('',#5344,.T.);
#3694=FACE_OUTER_BOUND('',#5345,.T.);
#3695=FACE_OUTER_BOUND('',#5346,.T.);
#3696=FACE_OUTER_BOUND('',#5347,.T.);
#3697=FACE_OUTER_BOUND('',#5348,.T.);
#3698=FACE_OUTER_BOUND('',#5349,.T.);
#3699=FACE_OUTER_BOUND('',#5350,.T.);
#3700=FACE_OUTER_BOUND('',#5351,.T.);
#3701=FACE_OUTER_BOUND('',#5352,.T.);
#3702=FACE_OUTER_BOUND('',#5353,.T.);
#3703=FACE_OUTER_BOUND('',#5355,.T.);
#3704=FACE_OUTER_BOUND('',#5356,.T.);
#3705=FACE_OUTER_BOUND('',#5357,.T.);
#3706=FACE_OUTER_BOUND('',#5358,.T.);
#3707=FACE_OUTER_BOUND('',#5359,.T.);
#3708=FACE_OUTER_BOUND('',#5360,.T.);
#3709=FACE_OUTER_BOUND('',#5361,.T.);
#3710=FACE_OUTER_BOUND('',#5362,.T.);
#3711=FACE_OUTER_BOUND('',#5363,.T.);
#3712=FACE_OUTER_BOUND('',#5364,.T.);
#3713=FACE_OUTER_BOUND('',#5365,.T.);
#3714=FACE_OUTER_BOUND('',#5366,.T.);
#3715=FACE_OUTER_BOUND('',#5367,.T.);
#3716=FACE_OUTER_BOUND('',#5368,.T.);
#3717=FACE_OUTER_BOUND('',#5369,.T.);
#3718=FACE_OUTER_BOUND('',#5370,.T.);
#3719=FACE_OUTER_BOUND('',#5371,.T.);
#3720=FACE_OUTER_BOUND('',#5372,.T.);
#3721=FACE_OUTER_BOUND('',#5373,.T.);
#3722=FACE_OUTER_BOUND('',#5374,.T.);
#3723=FACE_OUTER_BOUND('',#5375,.T.);
#3724=FACE_OUTER_BOUND('',#5376,.T.);
#3725=FACE_OUTER_BOUND('',#5377,.T.);
#3726=FACE_OUTER_BOUND('',#5378,.T.);
#3727=FACE_OUTER_BOUND('',#5379,.T.);
#3728=FACE_OUTER_BOUND('',#5380,.T.);
#3729=FACE_OUTER_BOUND('',#5381,.T.);
#3730=FACE_OUTER_BOUND('',#5382,.T.);
#3731=FACE_OUTER_BOUND('',#5383,.T.);
#3732=FACE_OUTER_BOUND('',#5384,.T.);
#3733=FACE_OUTER_BOUND('',#5385,.T.);
#3734=FACE_OUTER_BOUND('',#5386,.T.);
#3735=FACE_OUTER_BOUND('',#5387,.T.);
#3736=FACE_OUTER_BOUND('',#5388,.T.);
#3737=FACE_OUTER_BOUND('',#5389,.T.);
#3738=FACE_OUTER_BOUND('',#5390,.T.);
#3739=FACE_OUTER_BOUND('',#5391,.T.);
#3740=FACE_OUTER_BOUND('',#5392,.T.);
#3741=FACE_OUTER_BOUND('',#5393,.T.);
#3742=FACE_OUTER_BOUND('',#5394,.T.);
#3743=FACE_OUTER_BOUND('',#5395,.T.);
#3744=FACE_OUTER_BOUND('',#5396,.T.);
#3745=FACE_OUTER_BOUND('',#5397,.T.);
#3746=FACE_OUTER_BOUND('',#5398,.T.);
#3747=FACE_OUTER_BOUND('',#5399,.T.);
#3748=FACE_OUTER_BOUND('',#5400,.T.);
#3749=FACE_OUTER_BOUND('',#5401,.T.);
#3750=FACE_OUTER_BOUND('',#5402,.T.);
#3751=FACE_OUTER_BOUND('',#5403,.T.);
#3752=FACE_OUTER_BOUND('',#5404,.T.);
#3753=FACE_OUTER_BOUND('',#5405,.T.);
#3754=FACE_OUTER_BOUND('',#5406,.T.);
#3755=FACE_OUTER_BOUND('',#5407,.T.);
#3756=FACE_OUTER_BOUND('',#5408,.T.);
#3757=FACE_OUTER_BOUND('',#5409,.T.);
#3758=FACE_OUTER_BOUND('',#5410,.T.);
#3759=FACE_OUTER_BOUND('',#5411,.T.);
#3760=FACE_OUTER_BOUND('',#5412,.T.);
#3761=FACE_OUTER_BOUND('',#5413,.T.);
#3762=FACE_OUTER_BOUND('',#5414,.T.);
#3763=FACE_OUTER_BOUND('',#5415,.T.);
#3764=FACE_OUTER_BOUND('',#5416,.T.);
#3765=FACE_OUTER_BOUND('',#5417,.T.);
#3766=FACE_OUTER_BOUND('',#5418,.T.);
#3767=FACE_OUTER_BOUND('',#5419,.T.);
#3768=FACE_OUTER_BOUND('',#5420,.T.);
#3769=FACE_OUTER_BOUND('',#5421,.T.);
#3770=FACE_OUTER_BOUND('',#5422,.T.);
#3771=FACE_OUTER_BOUND('',#5423,.T.);
#3772=FACE_OUTER_BOUND('',#5424,.T.);
#3773=FACE_OUTER_BOUND('',#5425,.T.);
#3774=FACE_OUTER_BOUND('',#5426,.T.);
#3775=FACE_OUTER_BOUND('',#5427,.T.);
#3776=FACE_OUTER_BOUND('',#5428,.T.);
#3777=FACE_OUTER_BOUND('',#5429,.T.);
#3778=FACE_OUTER_BOUND('',#5430,.T.);
#3779=FACE_OUTER_BOUND('',#5431,.T.);
#3780=FACE_OUTER_BOUND('',#5432,.T.);
#3781=FACE_OUTER_BOUND('',#5433,.T.);
#3782=FACE_OUTER_BOUND('',#5434,.T.);
#3783=FACE_OUTER_BOUND('',#5435,.T.);
#3784=FACE_OUTER_BOUND('',#5436,.T.);
#3785=FACE_OUTER_BOUND('',#5437,.T.);
#3786=FACE_OUTER_BOUND('',#5438,.T.);
#3787=FACE_OUTER_BOUND('',#5439,.T.);
#3788=FACE_OUTER_BOUND('',#5440,.T.);
#3789=FACE_OUTER_BOUND('',#5441,.T.);
#3790=FACE_OUTER_BOUND('',#5442,.T.);
#3791=FACE_OUTER_BOUND('',#5443,.T.);
#3792=FACE_OUTER_BOUND('',#5444,.T.);
#3793=FACE_OUTER_BOUND('',#5445,.T.);
#3794=FACE_OUTER_BOUND('',#5446,.T.);
#3795=FACE_OUTER_BOUND('',#5447,.T.);
#3796=FACE_OUTER_BOUND('',#5448,.T.);
#3797=FACE_OUTER_BOUND('',#5449,.T.);
#3798=FACE_OUTER_BOUND('',#5450,.T.);
#3799=FACE_OUTER_BOUND('',#5451,.T.);
#3800=FACE_OUTER_BOUND('',#5452,.T.);
#3801=FACE_OUTER_BOUND('',#5453,.T.);
#3802=FACE_OUTER_BOUND('',#5454,.T.);
#3803=FACE_OUTER_BOUND('',#5455,.T.);
#3804=FACE_OUTER_BOUND('',#5456,.T.);
#3805=FACE_OUTER_BOUND('',#5457,.T.);
#3806=FACE_OUTER_BOUND('',#5458,.T.);
#3807=FACE_OUTER_BOUND('',#5459,.T.);
#3808=FACE_OUTER_BOUND('',#5460,.T.);
#3809=FACE_OUTER_BOUND('',#5461,.T.);
#3810=FACE_OUTER_BOUND('',#5462,.T.);
#3811=FACE_OUTER_BOUND('',#5463,.T.);
#3812=FACE_OUTER_BOUND('',#5464,.T.);
#3813=FACE_OUTER_BOUND('',#5465,.T.);
#3814=FACE_OUTER_BOUND('',#5466,.T.);
#3815=FACE_OUTER_BOUND('',#5467,.T.);
#3816=FACE_OUTER_BOUND('',#5468,.T.);
#3817=FACE_OUTER_BOUND('',#5469,.T.);
#3818=FACE_OUTER_BOUND('',#5470,.T.);
#3819=FACE_OUTER_BOUND('',#5471,.T.);
#3820=FACE_OUTER_BOUND('',#5472,.T.);
#3821=FACE_OUTER_BOUND('',#5473,.T.);
#3822=FACE_OUTER_BOUND('',#5474,.T.);
#3823=FACE_OUTER_BOUND('',#5475,.T.);
#3824=FACE_OUTER_BOUND('',#5476,.T.);
#3825=FACE_OUTER_BOUND('',#5477,.T.);
#3826=FACE_OUTER_BOUND('',#5478,.T.);
#3827=FACE_OUTER_BOUND('',#5479,.T.);
#3828=FACE_OUTER_BOUND('',#5480,.T.);
#3829=FACE_OUTER_BOUND('',#5481,.T.);
#3830=FACE_OUTER_BOUND('',#5482,.T.);
#3831=FACE_OUTER_BOUND('',#5483,.T.);
#3832=FACE_OUTER_BOUND('',#5484,.T.);
#3833=FACE_OUTER_BOUND('',#5485,.T.);
#3834=FACE_OUTER_BOUND('',#5486,.T.);
#3835=FACE_OUTER_BOUND('',#5487,.T.);
#3836=FACE_OUTER_BOUND('',#5488,.T.);
#3837=FACE_OUTER_BOUND('',#5489,.T.);
#3838=FACE_OUTER_BOUND('',#5490,.T.);
#3839=FACE_OUTER_BOUND('',#5491,.T.);
#3840=FACE_OUTER_BOUND('',#5492,.T.);
#3841=FACE_OUTER_BOUND('',#5493,.T.);
#3842=FACE_OUTER_BOUND('',#5494,.T.);
#3843=FACE_OUTER_BOUND('',#5495,.T.);
#3844=FACE_OUTER_BOUND('',#5496,.T.);
#3845=FACE_OUTER_BOUND('',#5497,.T.);
#3846=FACE_OUTER_BOUND('',#5498,.T.);
#3847=FACE_OUTER_BOUND('',#5499,.T.);
#3848=FACE_OUTER_BOUND('',#5500,.T.);
#3849=FACE_OUTER_BOUND('',#5501,.T.);
#3850=FACE_OUTER_BOUND('',#5502,.T.);
#3851=FACE_OUTER_BOUND('',#5503,.T.);
#3852=FACE_OUTER_BOUND('',#5504,.T.);
#3853=FACE_OUTER_BOUND('',#5505,.T.);
#3854=FACE_OUTER_BOUND('',#5506,.T.);
#3855=FACE_OUTER_BOUND('',#5507,.T.);
#3856=FACE_OUTER_BOUND('',#5508,.T.);
#3857=FACE_OUTER_BOUND('',#5509,.T.);
#3858=FACE_OUTER_BOUND('',#5510,.T.);
#3859=FACE_OUTER_BOUND('',#5511,.T.);
#3860=FACE_OUTER_BOUND('',#5512,.T.);
#3861=FACE_OUTER_BOUND('',#5513,.T.);
#3862=FACE_OUTER_BOUND('',#5514,.T.);
#3863=FACE_OUTER_BOUND('',#5515,.T.);
#3864=FACE_OUTER_BOUND('',#5516,.T.);
#3865=FACE_OUTER_BOUND('',#5517,.T.);
#3866=FACE_OUTER_BOUND('',#5519,.T.);
#3867=FACE_OUTER_BOUND('',#5520,.T.);
#3868=FACE_OUTER_BOUND('',#5521,.T.);
#3869=FACE_OUTER_BOUND('',#5522,.T.);
#3870=FACE_OUTER_BOUND('',#5523,.T.);
#3871=FACE_OUTER_BOUND('',#5524,.T.);
#3872=FACE_OUTER_BOUND('',#5525,.T.);
#3873=FACE_OUTER_BOUND('',#5526,.T.);
#3874=FACE_OUTER_BOUND('',#5527,.T.);
#3875=FACE_OUTER_BOUND('',#5528,.T.);
#3876=FACE_OUTER_BOUND('',#5529,.T.);
#3877=FACE_OUTER_BOUND('',#5530,.T.);
#3878=FACE_OUTER_BOUND('',#5531,.T.);
#3879=FACE_OUTER_BOUND('',#5532,.T.);
#3880=FACE_OUTER_BOUND('',#5533,.T.);
#3881=FACE_OUTER_BOUND('',#5534,.T.);
#3882=FACE_OUTER_BOUND('',#5535,.T.);
#3883=FACE_OUTER_BOUND('',#5536,.T.);
#3884=FACE_OUTER_BOUND('',#5537,.T.);
#3885=FACE_OUTER_BOUND('',#5538,.T.);
#3886=FACE_OUTER_BOUND('',#5539,.T.);
#3887=FACE_OUTER_BOUND('',#5540,.T.);
#3888=FACE_OUTER_BOUND('',#5541,.T.);
#3889=FACE_OUTER_BOUND('',#5542,.T.);
#3890=FACE_OUTER_BOUND('',#5543,.T.);
#3891=FACE_OUTER_BOUND('',#5544,.T.);
#3892=FACE_OUTER_BOUND('',#5545,.T.);
#3893=FACE_OUTER_BOUND('',#5546,.T.);
#3894=FACE_OUTER_BOUND('',#5547,.T.);
#3895=FACE_OUTER_BOUND('',#5548,.T.);
#3896=FACE_OUTER_BOUND('',#5549,.T.);
#3897=FACE_OUTER_BOUND('',#5550,.T.);
#3898=FACE_OUTER_BOUND('',#5551,.T.);
#3899=FACE_OUTER_BOUND('',#5552,.T.);
#3900=FACE_OUTER_BOUND('',#5553,.T.);
#3901=FACE_OUTER_BOUND('',#5554,.T.);
#3902=FACE_OUTER_BOUND('',#5555,.T.);
#3903=FACE_OUTER_BOUND('',#5556,.T.);
#3904=FACE_OUTER_BOUND('',#5557,.T.);
#3905=FACE_OUTER_BOUND('',#5558,.T.);
#3906=FACE_OUTER_BOUND('',#5559,.T.);
#3907=FACE_OUTER_BOUND('',#5560,.T.);
#3908=FACE_OUTER_BOUND('',#5561,.T.);
#3909=FACE_OUTER_BOUND('',#5562,.T.);
#3910=FACE_OUTER_BOUND('',#5563,.T.);
#3911=FACE_OUTER_BOUND('',#5564,.T.);
#3912=FACE_OUTER_BOUND('',#5565,.T.);
#3913=FACE_OUTER_BOUND('',#5567,.T.);
#3914=FACE_OUTER_BOUND('',#5568,.T.);
#3915=FACE_OUTER_BOUND('',#5569,.T.);
#3916=FACE_OUTER_BOUND('',#5570,.T.);
#3917=FACE_OUTER_BOUND('',#5571,.T.);
#3918=FACE_OUTER_BOUND('',#5572,.T.);
#3919=FACE_OUTER_BOUND('',#5573,.T.);
#3920=FACE_OUTER_BOUND('',#5574,.T.);
#3921=FACE_OUTER_BOUND('',#5575,.T.);
#3922=FACE_OUTER_BOUND('',#5576,.T.);
#3923=FACE_OUTER_BOUND('',#5577,.T.);
#3924=FACE_OUTER_BOUND('',#5578,.T.);
#3925=FACE_OUTER_BOUND('',#5579,.T.);
#3926=FACE_OUTER_BOUND('',#5580,.T.);
#3927=FACE_OUTER_BOUND('',#5581,.T.);
#3928=FACE_OUTER_BOUND('',#5582,.T.);
#3929=FACE_OUTER_BOUND('',#5583,.T.);
#3930=FACE_OUTER_BOUND('',#5584,.T.);
#3931=FACE_OUTER_BOUND('',#5585,.T.);
#3932=FACE_OUTER_BOUND('',#5586,.T.);
#3933=FACE_OUTER_BOUND('',#5587,.T.);
#3934=FACE_OUTER_BOUND('',#5588,.T.);
#3935=FACE_OUTER_BOUND('',#5589,.T.);
#3936=FACE_OUTER_BOUND('',#5590,.T.);
#3937=FACE_OUTER_BOUND('',#5591,.T.);
#3938=FACE_OUTER_BOUND('',#5592,.T.);
#3939=FACE_OUTER_BOUND('',#5593,.T.);
#3940=FACE_OUTER_BOUND('',#5594,.T.);
#3941=FACE_OUTER_BOUND('',#5595,.T.);
#3942=FACE_OUTER_BOUND('',#5596,.T.);
#3943=FACE_OUTER_BOUND('',#5597,.T.);
#3944=FACE_OUTER_BOUND('',#5598,.T.);
#3945=FACE_OUTER_BOUND('',#5599,.T.);
#3946=FACE_OUTER_BOUND('',#5600,.T.);
#3947=FACE_OUTER_BOUND('',#5601,.T.);
#3948=FACE_OUTER_BOUND('',#5602,.T.);
#3949=FACE_OUTER_BOUND('',#5603,.T.);
#3950=FACE_OUTER_BOUND('',#5604,.T.);
#3951=FACE_OUTER_BOUND('',#5605,.T.);
#3952=FACE_OUTER_BOUND('',#5606,.T.);
#3953=FACE_OUTER_BOUND('',#5607,.T.);
#3954=FACE_OUTER_BOUND('',#5608,.T.);
#3955=FACE_OUTER_BOUND('',#5609,.T.);
#3956=FACE_OUTER_BOUND('',#5610,.T.);
#3957=FACE_OUTER_BOUND('',#5611,.T.);
#3958=FACE_OUTER_BOUND('',#5612,.T.);
#3959=FACE_OUTER_BOUND('',#5613,.T.);
#3960=FACE_OUTER_BOUND('',#5614,.T.);
#3961=FACE_OUTER_BOUND('',#5615,.T.);
#3962=FACE_OUTER_BOUND('',#5616,.T.);
#3963=FACE_OUTER_BOUND('',#5617,.T.);
#3964=FACE_OUTER_BOUND('',#5618,.T.);
#3965=FACE_OUTER_BOUND('',#5619,.T.);
#3966=FACE_OUTER_BOUND('',#5620,.T.);
#3967=FACE_OUTER_BOUND('',#5621,.T.);
#3968=FACE_OUTER_BOUND('',#5622,.T.);
#3969=FACE_OUTER_BOUND('',#5623,.T.);
#3970=FACE_OUTER_BOUND('',#5624,.T.);
#3971=FACE_OUTER_BOUND('',#5625,.T.);
#3972=FACE_OUTER_BOUND('',#5626,.T.);
#3973=FACE_OUTER_BOUND('',#5627,.T.);
#3974=FACE_OUTER_BOUND('',#5628,.T.);
#3975=FACE_OUTER_BOUND('',#5629,.T.);
#3976=FACE_OUTER_BOUND('',#5630,.T.);
#3977=FACE_OUTER_BOUND('',#5631,.T.);
#3978=FACE_OUTER_BOUND('',#5632,.T.);
#3979=FACE_OUTER_BOUND('',#5633,.T.);
#3980=FACE_OUTER_BOUND('',#5634,.T.);
#3981=FACE_OUTER_BOUND('',#5635,.T.);
#3982=FACE_OUTER_BOUND('',#5636,.T.);
#3983=FACE_OUTER_BOUND('',#5637,.T.);
#3984=FACE_OUTER_BOUND('',#5638,.T.);
#3985=FACE_OUTER_BOUND('',#5639,.T.);
#3986=FACE_OUTER_BOUND('',#5640,.T.);
#3987=FACE_OUTER_BOUND('',#5641,.T.);
#3988=FACE_OUTER_BOUND('',#5642,.T.);
#3989=FACE_OUTER_BOUND('',#5643,.T.);
#3990=FACE_OUTER_BOUND('',#5644,.T.);
#3991=FACE_OUTER_BOUND('',#5645,.T.);
#3992=FACE_OUTER_BOUND('',#5646,.T.);
#3993=FACE_OUTER_BOUND('',#5647,.T.);
#3994=FACE_OUTER_BOUND('',#5648,.T.);
#3995=FACE_OUTER_BOUND('',#5649,.T.);
#3996=FACE_OUTER_BOUND('',#5650,.T.);
#3997=FACE_OUTER_BOUND('',#5651,.T.);
#3998=FACE_OUTER_BOUND('',#5652,.T.);
#3999=FACE_OUTER_BOUND('',#5653,.T.);
#4000=FACE_OUTER_BOUND('',#5654,.T.);
#4001=FACE_OUTER_BOUND('',#5655,.T.);
#4002=FACE_OUTER_BOUND('',#5656,.T.);
#4003=FACE_OUTER_BOUND('',#5657,.T.);
#4004=FACE_OUTER_BOUND('',#5658,.T.);
#4005=FACE_OUTER_BOUND('',#5659,.T.);
#4006=FACE_OUTER_BOUND('',#5660,.T.);
#4007=FACE_OUTER_BOUND('',#5661,.T.);
#4008=FACE_OUTER_BOUND('',#5662,.T.);
#4009=FACE_OUTER_BOUND('',#5663,.T.);
#4010=FACE_OUTER_BOUND('',#5664,.T.);
#4011=FACE_OUTER_BOUND('',#5665,.T.);
#4012=FACE_OUTER_BOUND('',#5666,.T.);
#4013=FACE_OUTER_BOUND('',#5667,.T.);
#4014=FACE_OUTER_BOUND('',#5668,.T.);
#4015=FACE_OUTER_BOUND('',#5669,.T.);
#4016=FACE_OUTER_BOUND('',#5670,.T.);
#4017=FACE_OUTER_BOUND('',#5671,.T.);
#4018=FACE_OUTER_BOUND('',#5672,.T.);
#4019=FACE_OUTER_BOUND('',#5673,.T.);
#4020=FACE_OUTER_BOUND('',#5674,.T.);
#4021=FACE_OUTER_BOUND('',#5675,.T.);
#4022=FACE_OUTER_BOUND('',#5676,.T.);
#4023=FACE_OUTER_BOUND('',#5677,.T.);
#4024=FACE_OUTER_BOUND('',#5678,.T.);
#4025=FACE_OUTER_BOUND('',#5679,.T.);
#4026=FACE_OUTER_BOUND('',#5680,.T.);
#4027=FACE_OUTER_BOUND('',#5681,.T.);
#4028=FACE_OUTER_BOUND('',#5682,.T.);
#4029=FACE_OUTER_BOUND('',#5683,.T.);
#4030=FACE_OUTER_BOUND('',#5684,.T.);
#4031=FACE_OUTER_BOUND('',#5685,.T.);
#4032=FACE_OUTER_BOUND('',#5686,.T.);
#4033=FACE_OUTER_BOUND('',#5687,.T.);
#4034=FACE_OUTER_BOUND('',#5688,.T.);
#4035=FACE_OUTER_BOUND('',#5689,.T.);
#4036=FACE_OUTER_BOUND('',#5690,.T.);
#4037=FACE_OUTER_BOUND('',#5691,.T.);
#4038=FACE_OUTER_BOUND('',#5692,.T.);
#4039=FACE_OUTER_BOUND('',#5693,.T.);
#4040=FACE_OUTER_BOUND('',#5694,.T.);
#4041=FACE_OUTER_BOUND('',#5695,.T.);
#4042=FACE_OUTER_BOUND('',#5696,.T.);
#4043=FACE_OUTER_BOUND('',#5697,.T.);
#4044=FACE_OUTER_BOUND('',#5698,.T.);
#4045=FACE_OUTER_BOUND('',#5699,.T.);
#4046=FACE_OUTER_BOUND('',#5700,.T.);
#4047=FACE_OUTER_BOUND('',#5701,.T.);
#4048=FACE_OUTER_BOUND('',#5702,.T.);
#4049=FACE_OUTER_BOUND('',#5703,.T.);
#4050=FACE_OUTER_BOUND('',#5704,.T.);
#4051=FACE_OUTER_BOUND('',#5705,.T.);
#4052=FACE_OUTER_BOUND('',#5706,.T.);
#4053=FACE_OUTER_BOUND('',#5707,.T.);
#4054=FACE_OUTER_BOUND('',#5708,.T.);
#4055=FACE_OUTER_BOUND('',#5709,.T.);
#4056=FACE_OUTER_BOUND('',#5710,.T.);
#4057=FACE_OUTER_BOUND('',#5711,.T.);
#4058=FACE_OUTER_BOUND('',#5712,.T.);
#4059=FACE_OUTER_BOUND('',#5713,.T.);
#4060=FACE_OUTER_BOUND('',#5714,.T.);
#4061=FACE_OUTER_BOUND('',#5715,.T.);
#4062=FACE_OUTER_BOUND('',#5716,.T.);
#4063=FACE_OUTER_BOUND('',#5717,.T.);
#4064=FACE_OUTER_BOUND('',#5718,.T.);
#4065=FACE_OUTER_BOUND('',#5719,.T.);
#4066=FACE_OUTER_BOUND('',#5720,.T.);
#4067=FACE_OUTER_BOUND('',#5721,.T.);
#4068=FACE_OUTER_BOUND('',#5722,.T.);
#4069=FACE_OUTER_BOUND('',#5723,.T.);
#4070=FACE_OUTER_BOUND('',#5724,.T.);
#4071=FACE_OUTER_BOUND('',#5725,.T.);
#4072=FACE_OUTER_BOUND('',#5726,.T.);
#4073=FACE_OUTER_BOUND('',#5727,.T.);
#4074=FACE_OUTER_BOUND('',#5728,.T.);
#4075=FACE_OUTER_BOUND('',#5729,.T.);
#4076=EDGE_LOOP('',(#17185,#17186,#17187,#17188));
#4077=EDGE_LOOP('',(#17189,#17190,#17191,#17192));
#4078=EDGE_LOOP('',(#17193,#17194,#17195,#17196));
#4079=EDGE_LOOP('',(#17197,#17198,#17199,#17200));
#4080=EDGE_LOOP('',(#17201,#17202,#17203,#17204));
#4081=EDGE_LOOP('',(#17205,#17206,#17207,#17208));
#4082=EDGE_LOOP('',(#17209,#17210,#17211,#17212));
#4083=EDGE_LOOP('',(#17213,#17214,#17215,#17216));
#4084=EDGE_LOOP('',(#17217,#17218,#17219,#17220));
#4085=EDGE_LOOP('',(#17221,#17222,#17223,#17224));
#4086=EDGE_LOOP('',(#17225,#17226,#17227,#17228));
#4087=EDGE_LOOP('',(#17229,#17230,#17231,#17232));
#4088=EDGE_LOOP('',(#17233,#17234,#17235,#17236,#17237,#17238,#17239,#17240));
#4089=EDGE_LOOP('',(#17241,#17242,#17243,#17244,#17245,#17246,#17247,#17248));
#4090=EDGE_LOOP('',(#17249,#17250,#17251,#17252));
#4091=EDGE_LOOP('',(#17253,#17254,#17255,#17256,#17257,#17258,#17259,#17260));
#4092=EDGE_LOOP('',(#17261));
#4093=EDGE_LOOP('',(#17262));
#4094=EDGE_LOOP('',(#17263));
#4095=EDGE_LOOP('',(#17264,#17265,#17266,#17267));
#4096=EDGE_LOOP('',(#17268));
#4097=EDGE_LOOP('',(#17269));
#4098=EDGE_LOOP('',(#17270,#17271,#17272,#17273));
#4099=EDGE_LOOP('',(#17274,#17275,#17276,#17277));
#4100=EDGE_LOOP('',(#17278,#17279,#17280,#17281));
#4101=EDGE_LOOP('',(#17282,#17283,#17284,#17285));
#4102=EDGE_LOOP('',(#17286,#17287,#17288,#17289));
#4103=EDGE_LOOP('',(#17290,#17291,#17292,#17293));
#4104=EDGE_LOOP('',(#17294,#17295,#17296,#17297));
#4105=EDGE_LOOP('',(#17298,#17299,#17300,#17301));
#4106=EDGE_LOOP('',(#17302,#17303,#17304,#17305));
#4107=EDGE_LOOP('',(#17306,#17307,#17308,#17309));
#4108=EDGE_LOOP('',(#17310,#17311,#17312,#17313));
#4109=EDGE_LOOP('',(#17314,#17315,#17316,#17317));
#4110=EDGE_LOOP('',(#17318,#17319,#17320,#17321));
#4111=EDGE_LOOP('',(#17322,#17323,#17324,#17325,#17326,#17327));
#4112=EDGE_LOOP('',(#17328,#17329,#17330,#17331));
#4113=EDGE_LOOP('',(#17332,#17333,#17334,#17335));
#4114=EDGE_LOOP('',(#17336,#17337,#17338,#17339));
#4115=EDGE_LOOP('',(#17340,#17341,#17342,#17343,#17344,#17345));
#4116=EDGE_LOOP('',(#17346,#17347,#17348,#17349));
#4117=EDGE_LOOP('',(#17350,#17351,#17352,#17353));
#4118=EDGE_LOOP('',(#17354,#17355,#17356,#17357));
#4119=EDGE_LOOP('',(#17358,#17359,#17360,#17361,#17362,#17363,#17364));
#4120=EDGE_LOOP('',(#17365,#17366,#17367,#17368));
#4121=EDGE_LOOP('',(#17369,#17370,#17371,#17372));
#4122=EDGE_LOOP('',(#17373,#17374,#17375,#17376));
#4123=EDGE_LOOP('',(#17377,#17378,#17379,#17380,#17381,#17382,#17383));
#4124=EDGE_LOOP('',(#17384,#17385,#17386,#17387,#17388,#17389,#17390,#17391));
#4125=EDGE_LOOP('',(#17392,#17393,#17394,#17395,#17396));
#4126=EDGE_LOOP('',(#17397,#17398,#17399,#17400));
#4127=EDGE_LOOP('',(#17401,#17402,#17403,#17404,#17405));
#4128=EDGE_LOOP('',(#17406,#17407,#17408,#17409,#17410,#17411,#17412,#17413));
#4129=EDGE_LOOP('',(#17414,#17415,#17416,#17417,#17418,#17419));
#4130=EDGE_LOOP('',(#17420,#17421,#17422,#17423,#17424));
#4131=EDGE_LOOP('',(#17425,#17426,#17427,#17428,#17429));
#4132=EDGE_LOOP('',(#17430,#17431,#17432,#17433));
#4133=EDGE_LOOP('',(#17434,#17435,#17436,#17437));
#4134=EDGE_LOOP('',(#17438,#17439,#17440,#17441,#17442));
#4135=EDGE_LOOP('',(#17443,#17444,#17445,#17446));
#4136=EDGE_LOOP('',(#17447,#17448,#17449,#17450));
#4137=EDGE_LOOP('',(#17451,#17452,#17453,#17454));
#4138=EDGE_LOOP('',(#17455,#17456,#17457,#17458));
#4139=EDGE_LOOP('',(#17459,#17460,#17461,#17462));
#4140=EDGE_LOOP('',(#17463,#17464,#17465,#17466));
#4141=EDGE_LOOP('',(#17467,#17468,#17469,#17470));
#4142=EDGE_LOOP('',(#17471,#17472,#17473,#17474));
#4143=EDGE_LOOP('',(#17475,#17476,#17477,#17478));
#4144=EDGE_LOOP('',(#17479,#17480,#17481,#17482));
#4145=EDGE_LOOP('',(#17483,#17484,#17485,#17486));
#4146=EDGE_LOOP('',(#17487,#17488,#17489,#17490));
#4147=EDGE_LOOP('',(#17491,#17492,#17493,#17494));
#4148=EDGE_LOOP('',(#17495,#17496,#17497,#17498));
#4149=EDGE_LOOP('',(#17499,#17500,#17501,#17502,#17503,#17504));
#4150=EDGE_LOOP('',(#17505,#17506,#17507,#17508));
#4151=EDGE_LOOP('',(#17509,#17510,#17511,#17512));
#4152=EDGE_LOOP('',(#17513,#17514,#17515,#17516));
#4153=EDGE_LOOP('',(#17517,#17518,#17519,#17520,#17521,#17522));
#4154=EDGE_LOOP('',(#17523,#17524,#17525,#17526));
#4155=EDGE_LOOP('',(#17527,#17528,#17529,#17530,#17531,#17532,#17533));
#4156=EDGE_LOOP('',(#17534,#17535,#17536,#17537));
#4157=EDGE_LOOP('',(#17538,#17539,#17540,#17541,#17542,#17543,#17544,#17545));
#4158=EDGE_LOOP('',(#17546,#17547,#17548,#17549));
#4159=EDGE_LOOP('',(#17550,#17551,#17552,#17553,#17554,#17555,#17556));
#4160=EDGE_LOOP('',(#17557,#17558,#17559,#17560));
#4161=EDGE_LOOP('',(#17561,#17562,#17563,#17564));
#4162=EDGE_LOOP('',(#17565,#17566,#17567,#17568));
#4163=EDGE_LOOP('',(#17569,#17570,#17571,#17572,#17573));
#4164=EDGE_LOOP('',(#17574,#17575,#17576,#17577));
#4165=EDGE_LOOP('',(#17578,#17579,#17580,#17581));
#4166=EDGE_LOOP('',(#17582,#17583,#17584,#17585));
#4167=EDGE_LOOP('',(#17586,#17587,#17588));
#4168=EDGE_LOOP('',(#17589,#17590,#17591));
#4169=EDGE_LOOP('',(#17592,#17593,#17594,#17595));
#4170=EDGE_LOOP('',(#17596,#17597,#17598,#17599));
#4171=EDGE_LOOP('',(#17600,#17601,#17602,#17603));
#4172=EDGE_LOOP('',(#17604,#17605,#17606,#17607));
#4173=EDGE_LOOP('',(#17608,#17609,#17610,#17611));
#4174=EDGE_LOOP('',(#17612,#17613,#17614,#17615));
#4175=EDGE_LOOP('',(#17616,#17617,#17618,#17619));
#4176=EDGE_LOOP('',(#17620,#17621,#17622,#17623));
#4177=EDGE_LOOP('',(#17624,#17625,#17626,#17627));
#4178=EDGE_LOOP('',(#17628,#17629,#17630,#17631));
#4179=EDGE_LOOP('',(#17632,#17633,#17634,#17635));
#4180=EDGE_LOOP('',(#17636,#17637,#17638,#17639));
#4181=EDGE_LOOP('',(#17640,#17641,#17642,#17643));
#4182=EDGE_LOOP('',(#17644,#17645,#17646,#17647));
#4183=EDGE_LOOP('',(#17648,#17649,#17650,#17651));
#4184=EDGE_LOOP('',(#17652,#17653,#17654,#17655));
#4185=EDGE_LOOP('',(#17656,#17657,#17658,#17659));
#4186=EDGE_LOOP('',(#17660,#17661,#17662,#17663));
#4187=EDGE_LOOP('',(#17664,#17665,#17666,#17667));
#4188=EDGE_LOOP('',(#17668,#17669,#17670,#17671));
#4189=EDGE_LOOP('',(#17672,#17673,#17674,#17675));
#4190=EDGE_LOOP('',(#17676,#17677,#17678,#17679));
#4191=EDGE_LOOP('',(#17680,#17681,#17682,#17683));
#4192=EDGE_LOOP('',(#17684,#17685,#17686,#17687));
#4193=EDGE_LOOP('',(#17688,#17689,#17690,#17691));
#4194=EDGE_LOOP('',(#17692));
#4195=EDGE_LOOP('',(#17693,#17694,#17695,#17696));
#4196=EDGE_LOOP('',(#17697,#17698,#17699,#17700,#17701,#17702));
#4197=EDGE_LOOP('',(#17703,#17704,#17705,#17706));
#4198=EDGE_LOOP('',(#17707,#17708,#17709,#17710));
#4199=EDGE_LOOP('',(#17711,#17712,#17713,#17714,#17715,#17716));
#4200=EDGE_LOOP('',(#17717,#17718,#17719,#17720));
#4201=EDGE_LOOP('',(#17721,#17722,#17723,#17724));
#4202=EDGE_LOOP('',(#17725,#17726,#17727,#17728));
#4203=EDGE_LOOP('',(#17729,#17730,#17731,#17732));
#4204=EDGE_LOOP('',(#17733,#17734,#17735,#17736));
#4205=EDGE_LOOP('',(#17737,#17738,#17739,#17740));
#4206=EDGE_LOOP('',(#17741,#17742,#17743,#17744));
#4207=EDGE_LOOP('',(#17745,#17746,#17747,#17748));
#4208=EDGE_LOOP('',(#17749,#17750,#17751,#17752));
#4209=EDGE_LOOP('',(#17753,#17754,#17755,#17756));
#4210=EDGE_LOOP('',(#17757,#17758,#17759,#17760));
#4211=EDGE_LOOP('',(#17761,#17762,#17763,#17764));
#4212=EDGE_LOOP('',(#17765,#17766,#17767,#17768));
#4213=EDGE_LOOP('',(#17769,#17770,#17771,#17772));
#4214=EDGE_LOOP('',(#17773,#17774,#17775,#17776));
#4215=EDGE_LOOP('',(#17777,#17778,#17779,#17780));
#4216=EDGE_LOOP('',(#17781,#17782,#17783,#17784));
#4217=EDGE_LOOP('',(#17785,#17786,#17787,#17788));
#4218=EDGE_LOOP('',(#17789,#17790,#17791,#17792));
#4219=EDGE_LOOP('',(#17793,#17794,#17795,#17796));
#4220=EDGE_LOOP('',(#17797,#17798,#17799,#17800,#17801,#17802,#17803,#17804));
#4221=EDGE_LOOP('',(#17805,#17806,#17807,#17808));
#4222=EDGE_LOOP('',(#17809,#17810,#17811));
#4223=EDGE_LOOP('',(#17812,#17813,#17814));
#4224=EDGE_LOOP('',(#17815,#17816,#17817));
#4225=EDGE_LOOP('',(#17818,#17819,#17820));
#4226=EDGE_LOOP('',(#17821,#17822,#17823,#17824));
#4227=EDGE_LOOP('',(#17825,#17826,#17827,#17828));
#4228=EDGE_LOOP('',(#17829,#17830,#17831,#17832));
#4229=EDGE_LOOP('',(#17833,#17834,#17835,#17836));
#4230=EDGE_LOOP('',(#17837,#17838,#17839,#17840,#17841));
#4231=EDGE_LOOP('',(#17842,#17843,#17844,#17845,#17846,#17847));
#4232=EDGE_LOOP('',(#17848));
#4233=EDGE_LOOP('',(#17849));
#4234=EDGE_LOOP('',(#17850,#17851,#17852,#17853,#17854,#17855));
#4235=EDGE_LOOP('',(#17856,#17857,#17858,#17859,#17860,#17861));
#4236=EDGE_LOOP('',(#17862,#17863,#17864,#17865,#17866,#17867,#17868));
#4237=EDGE_LOOP('',(#17869,#17870,#17871,#17872,#17873,#17874,#17875,#17876,
#17877,#17878,#17879,#17880,#17881));
#4238=EDGE_LOOP('',(#17882,#17883,#17884,#17885,#17886));
#4239=EDGE_LOOP('',(#17887,#17888,#17889,#17890,#17891,#17892));
#4240=EDGE_LOOP('',(#17893,#17894,#17895,#17896));
#4241=EDGE_LOOP('',(#17897,#17898,#17899,#17900,#17901,#17902));
#4242=EDGE_LOOP('',(#17903,#17904,#17905,#17906,#17907,#17908,#17909,#17910));
#4243=EDGE_LOOP('',(#17911,#17912,#17913,#17914));
#4244=EDGE_LOOP('',(#17915,#17916,#17917,#17918));
#4245=EDGE_LOOP('',(#17919,#17920,#17921,#17922,#17923));
#4246=EDGE_LOOP('',(#17924,#17925,#17926,#17927,#17928));
#4247=EDGE_LOOP('',(#17929,#17930,#17931,#17932));
#4248=EDGE_LOOP('',(#17933,#17934,#17935,#17936));
#4249=EDGE_LOOP('',(#17937));
#4250=EDGE_LOOP('',(#17938));
#4251=EDGE_LOOP('',(#17939,#17940,#17941,#17942,#17943));
#4252=EDGE_LOOP('',(#17944,#17945,#17946,#17947,#17948,#17949));
#4253=EDGE_LOOP('',(#17950,#17951,#17952,#17953,#17954,#17955,#17956,#17957));
#4254=EDGE_LOOP('',(#17958,#17959));
#4255=EDGE_LOOP('',(#17960));
#4256=EDGE_LOOP('',(#17961,#17962,#17963,#17964,#17965));
#4257=EDGE_LOOP('',(#17966,#17967,#17968,#17969,#17970));
#4258=EDGE_LOOP('',(#17971,#17972,#17973,#17974));
#4259=EDGE_LOOP('',(#17975,#17976,#17977,#17978));
#4260=EDGE_LOOP('',(#17979,#17980,#17981,#17982));
#4261=EDGE_LOOP('',(#17983,#17984,#17985,#17986));
#4262=EDGE_LOOP('',(#17987,#17988,#17989,#17990));
#4263=EDGE_LOOP('',(#17991,#17992,#17993,#17994));
#4264=EDGE_LOOP('',(#17995,#17996,#17997,#17998,#17999));
#4265=EDGE_LOOP('',(#18000,#18001,#18002,#18003,#18004));
#4266=EDGE_LOOP('',(#18005,#18006,#18007));
#4267=EDGE_LOOP('',(#18008,#18009,#18010,#18011));
#4268=EDGE_LOOP('',(#18012,#18013,#18014));
#4269=EDGE_LOOP('',(#18015,#18016,#18017,#18018));
#4270=EDGE_LOOP('',(#18019,#18020,#18021,#18022));
#4271=EDGE_LOOP('',(#18023,#18024,#18025,#18026));
#4272=EDGE_LOOP('',(#18027,#18028,#18029,#18030));
#4273=EDGE_LOOP('',(#18031,#18032,#18033,#18034));
#4274=EDGE_LOOP('',(#18035,#18036,#18037,#18038));
#4275=EDGE_LOOP('',(#18039,#18040,#18041,#18042));
#4276=EDGE_LOOP('',(#18043,#18044,#18045,#18046));
#4277=EDGE_LOOP('',(#18047,#18048,#18049,#18050));
#4278=EDGE_LOOP('',(#18051,#18052,#18053,#18054));
#4279=EDGE_LOOP('',(#18055,#18056,#18057,#18058));
#4280=EDGE_LOOP('',(#18059,#18060,#18061,#18062));
#4281=EDGE_LOOP('',(#18063,#18064,#18065,#18066));
#4282=EDGE_LOOP('',(#18067,#18068,#18069,#18070));
#4283=EDGE_LOOP('',(#18071,#18072,#18073,#18074,#18075,#18076,#18077,#18078));
#4284=EDGE_LOOP('',(#18079,#18080,#18081,#18082,#18083,#18084,#18085,#18086,
#18087,#18088));
#4285=EDGE_LOOP('',(#18089,#18090,#18091,#18092,#18093,#18094,#18095,#18096,
#18097,#18098,#18099,#18100));
#4286=EDGE_LOOP('',(#18101,#18102,#18103,#18104));
#4287=EDGE_LOOP('',(#18105,#18106,#18107,#18108,#18109,#18110));
#4288=EDGE_LOOP('',(#18111,#18112,#18113,#18114));
#4289=EDGE_LOOP('',(#18115,#18116,#18117,#18118));
#4290=EDGE_LOOP('',(#18119,#18120,#18121,#18122));
#4291=EDGE_LOOP('',(#18123,#18124,#18125,#18126,#18127,#18128));
#4292=EDGE_LOOP('',(#18129,#18130,#18131,#18132));
#4293=EDGE_LOOP('',(#18133,#18134,#18135,#18136));
#4294=EDGE_LOOP('',(#18137,#18138,#18139,#18140));
#4295=EDGE_LOOP('',(#18141,#18142,#18143,#18144));
#4296=EDGE_LOOP('',(#18145,#18146,#18147,#18148));
#4297=EDGE_LOOP('',(#18149,#18150,#18151,#18152));
#4298=EDGE_LOOP('',(#18153,#18154,#18155,#18156));
#4299=EDGE_LOOP('',(#18157,#18158,#18159,#18160));
#4300=EDGE_LOOP('',(#18161,#18162,#18163,#18164));
#4301=EDGE_LOOP('',(#18165,#18166,#18167,#18168));
#4302=EDGE_LOOP('',(#18169,#18170,#18171,#18172));
#4303=EDGE_LOOP('',(#18173,#18174,#18175,#18176));
#4304=EDGE_LOOP('',(#18177,#18178,#18179,#18180));
#4305=EDGE_LOOP('',(#18181,#18182,#18183,#18184));
#4306=EDGE_LOOP('',(#18185,#18186,#18187,#18188));
#4307=EDGE_LOOP('',(#18189,#18190,#18191,#18192));
#4308=EDGE_LOOP('',(#18193,#18194,#18195,#18196));
#4309=EDGE_LOOP('',(#18197,#18198,#18199,#18200));
#4310=EDGE_LOOP('',(#18201,#18202,#18203,#18204));
#4311=EDGE_LOOP('',(#18205,#18206,#18207,#18208));
#4312=EDGE_LOOP('',(#18209,#18210,#18211,#18212));
#4313=EDGE_LOOP('',(#18213,#18214,#18215,#18216));
#4314=EDGE_LOOP('',(#18217,#18218,#18219,#18220));
#4315=EDGE_LOOP('',(#18221,#18222,#18223,#18224));
#4316=EDGE_LOOP('',(#18225,#18226,#18227,#18228));
#4317=EDGE_LOOP('',(#18229,#18230,#18231,#18232));
#4318=EDGE_LOOP('',(#18233,#18234,#18235,#18236,#18237,#18238,#18239));
#4319=EDGE_LOOP('',(#18240,#18241,#18242,#18243,#18244));
#4320=EDGE_LOOP('',(#18245,#18246,#18247,#18248,#18249,#18250));
#4321=EDGE_LOOP('',(#18251,#18252,#18253,#18254));
#4322=EDGE_LOOP('',(#18255,#18256,#18257,#18258));
#4323=EDGE_LOOP('',(#18259,#18260,#18261,#18262));
#4324=EDGE_LOOP('',(#18263,#18264,#18265,#18266));
#4325=EDGE_LOOP('',(#18267,#18268,#18269,#18270));
#4326=EDGE_LOOP('',(#18271,#18272,#18273,#18274));
#4327=EDGE_LOOP('',(#18275,#18276,#18277,#18278,#18279,#18280,#18281,#18282,
#18283,#18284,#18285,#18286,#18287,#18288,#18289,#18290,#18291,#18292,#18293,
#18294,#18295,#18296));
#4328=EDGE_LOOP('',(#18297,#18298,#18299,#18300));
#4329=EDGE_LOOP('',(#18301,#18302,#18303,#18304));
#4330=EDGE_LOOP('',(#18305,#18306,#18307,#18308));
#4331=EDGE_LOOP('',(#18309,#18310,#18311,#18312));
#4332=EDGE_LOOP('',(#18313,#18314,#18315,#18316));
#4333=EDGE_LOOP('',(#18317,#18318,#18319,#18320));
#4334=EDGE_LOOP('',(#18321,#18322,#18323,#18324));
#4335=EDGE_LOOP('',(#18325,#18326,#18327,#18328));
#4336=EDGE_LOOP('',(#18329,#18330,#18331,#18332));
#4337=EDGE_LOOP('',(#18333,#18334,#18335,#18336));
#4338=EDGE_LOOP('',(#18337,#18338,#18339,#18340));
#4339=EDGE_LOOP('',(#18341,#18342,#18343,#18344));
#4340=EDGE_LOOP('',(#18345,#18346,#18347,#18348));
#4341=EDGE_LOOP('',(#18349,#18350,#18351,#18352));
#4342=EDGE_LOOP('',(#18353,#18354,#18355,#18356));
#4343=EDGE_LOOP('',(#18357,#18358,#18359,#18360));
#4344=EDGE_LOOP('',(#18361,#18362,#18363,#18364));
#4345=EDGE_LOOP('',(#18365,#18366,#18367,#18368));
#4346=EDGE_LOOP('',(#18369,#18370,#18371,#18372));
#4347=EDGE_LOOP('',(#18373,#18374,#18375,#18376));
#4348=EDGE_LOOP('',(#18377,#18378,#18379,#18380));
#4349=EDGE_LOOP('',(#18381,#18382,#18383,#18384));
#4350=EDGE_LOOP('',(#18385,#18386,#18387,#18388));
#4351=EDGE_LOOP('',(#18389,#18390,#18391,#18392));
#4352=EDGE_LOOP('',(#18393,#18394,#18395,#18396));
#4353=EDGE_LOOP('',(#18397,#18398,#18399,#18400));
#4354=EDGE_LOOP('',(#18401,#18402,#18403,#18404));
#4355=EDGE_LOOP('',(#18405,#18406,#18407,#18408));
#4356=EDGE_LOOP('',(#18409,#18410,#18411,#18412));
#4357=EDGE_LOOP('',(#18413,#18414,#18415,#18416));
#4358=EDGE_LOOP('',(#18417,#18418,#18419,#18420));
#4359=EDGE_LOOP('',(#18421,#18422,#18423,#18424));
#4360=EDGE_LOOP('',(#18425,#18426,#18427,#18428,#18429));
#4361=EDGE_LOOP('',(#18430,#18431,#18432,#18433));
#4362=EDGE_LOOP('',(#18434,#18435,#18436,#18437));
#4363=EDGE_LOOP('',(#18438,#18439,#18440,#18441));
#4364=EDGE_LOOP('',(#18442,#18443,#18444,#18445,#18446,#18447,#18448,#18449));
#4365=EDGE_LOOP('',(#18450,#18451,#18452,#18453));
#4366=EDGE_LOOP('',(#18454,#18455,#18456,#18457));
#4367=EDGE_LOOP('',(#18458,#18459,#18460,#18461));
#4368=EDGE_LOOP('',(#18462,#18463,#18464,#18465));
#4369=EDGE_LOOP('',(#18466,#18467,#18468,#18469));
#4370=EDGE_LOOP('',(#18470,#18471,#18472,#18473,#18474,#18475));
#4371=EDGE_LOOP('',(#18476,#18477,#18478,#18479));
#4372=EDGE_LOOP('',(#18480,#18481,#18482,#18483,#18484,#18485));
#4373=EDGE_LOOP('',(#18486,#18487,#18488,#18489,#18490));
#4374=EDGE_LOOP('',(#18491,#18492,#18493,#18494));
#4375=EDGE_LOOP('',(#18495,#18496,#18497,#18498));
#4376=EDGE_LOOP('',(#18499,#18500,#18501,#18502,#18503,#18504,#18505,#18506,
#18507,#18508,#18509,#18510));
#4377=EDGE_LOOP('',(#18511,#18512,#18513,#18514,#18515));
#4378=EDGE_LOOP('',(#18516,#18517,#18518,#18519));
#4379=EDGE_LOOP('',(#18520,#18521,#18522,#18523,#18524,#18525));
#4380=EDGE_LOOP('',(#18526,#18527,#18528,#18529));
#4381=EDGE_LOOP('',(#18530,#18531,#18532,#18533));
#4382=EDGE_LOOP('',(#18534,#18535,#18536,#18537));
#4383=EDGE_LOOP('',(#18538,#18539,#18540,#18541));
#4384=EDGE_LOOP('',(#18542,#18543,#18544,#18545,#18546,#18547));
#4385=EDGE_LOOP('',(#18548,#18549,#18550,#18551));
#4386=EDGE_LOOP('',(#18552,#18553,#18554,#18555));
#4387=EDGE_LOOP('',(#18556,#18557,#18558,#18559));
#4388=EDGE_LOOP('',(#18560,#18561,#18562,#18563));
#4389=EDGE_LOOP('',(#18564,#18565,#18566,#18567,#18568));
#4390=EDGE_LOOP('',(#18569,#18570,#18571,#18572,#18573,#18574,#18575,#18576,
#18577,#18578));
#4391=EDGE_LOOP('',(#18579,#18580,#18581,#18582));
#4392=EDGE_LOOP('',(#18583,#18584,#18585,#18586));
#4393=EDGE_LOOP('',(#18587,#18588,#18589,#18590));
#4394=EDGE_LOOP('',(#18591,#18592,#18593,#18594));
#4395=EDGE_LOOP('',(#18595,#18596,#18597,#18598));
#4396=EDGE_LOOP('',(#18599,#18600,#18601));
#4397=EDGE_LOOP('',(#18602,#18603,#18604));
#4398=EDGE_LOOP('',(#18605,#18606,#18607));
#4399=EDGE_LOOP('',(#18608,#18609,#18610));
#4400=EDGE_LOOP('',(#18611));
#4401=EDGE_LOOP('',(#18612));
#4402=EDGE_LOOP('',(#18613,#18614,#18615,#18616,#18617));
#4403=EDGE_LOOP('',(#18618,#18619,#18620,#18621,#18622));
#4404=EDGE_LOOP('',(#18623));
#4405=EDGE_LOOP('',(#18624));
#4406=EDGE_LOOP('',(#18625,#18626,#18627,#18628));
#4407=EDGE_LOOP('',(#18629,#18630,#18631,#18632));
#4408=EDGE_LOOP('',(#18633,#18634));
#4409=EDGE_LOOP('',(#18635,#18636));
#4410=EDGE_LOOP('',(#18637,#18638,#18639,#18640,#18641,#18642,#18643,#18644,
#18645,#18646,#18647,#18648,#18649));
#4411=EDGE_LOOP('',(#18650));
#4412=EDGE_LOOP('',(#18651,#18652,#18653,#18654,#18655));
#4413=EDGE_LOOP('',(#18656,#18657,#18658,#18659,#18660));
#4414=EDGE_LOOP('',(#18661));
#4415=EDGE_LOOP('',(#18662));
#4416=EDGE_LOOP('',(#18663,#18664,#18665,#18666));
#4417=EDGE_LOOP('',(#18667,#18668,#18669,#18670));
#4418=EDGE_LOOP('',(#18671,#18672,#18673,#18674));
#4419=EDGE_LOOP('',(#18675,#18676,#18677,#18678));
#4420=EDGE_LOOP('',(#18679,#18680,#18681,#18682));
#4421=EDGE_LOOP('',(#18683,#18684,#18685,#18686));
#4422=EDGE_LOOP('',(#18687,#18688,#18689,#18690));
#4423=EDGE_LOOP('',(#18691,#18692,#18693,#18694));
#4424=EDGE_LOOP('',(#18695,#18696,#18697,#18698));
#4425=EDGE_LOOP('',(#18699,#18700,#18701,#18702));
#4426=EDGE_LOOP('',(#18703,#18704,#18705,#18706));
#4427=EDGE_LOOP('',(#18707,#18708,#18709,#18710));
#4428=EDGE_LOOP('',(#18711,#18712,#18713,#18714));
#4429=EDGE_LOOP('',(#18715,#18716,#18717,#18718));
#4430=EDGE_LOOP('',(#18719,#18720,#18721,#18722));
#4431=EDGE_LOOP('',(#18723,#18724,#18725,#18726));
#4432=EDGE_LOOP('',(#18727,#18728,#18729,#18730));
#4433=EDGE_LOOP('',(#18731,#18732,#18733,#18734));
#4434=EDGE_LOOP('',(#18735,#18736,#18737,#18738));
#4435=EDGE_LOOP('',(#18739,#18740,#18741,#18742));
#4436=EDGE_LOOP('',(#18743,#18744,#18745,#18746));
#4437=EDGE_LOOP('',(#18747,#18748,#18749,#18750));
#4438=EDGE_LOOP('',(#18751,#18752,#18753,#18754));
#4439=EDGE_LOOP('',(#18755,#18756,#18757,#18758));
#4440=EDGE_LOOP('',(#18759,#18760,#18761,#18762));
#4441=EDGE_LOOP('',(#18763,#18764,#18765,#18766));
#4442=EDGE_LOOP('',(#18767,#18768,#18769,#18770));
#4443=EDGE_LOOP('',(#18771,#18772,#18773,#18774));
#4444=EDGE_LOOP('',(#18775,#18776,#18777,#18778));
#4445=EDGE_LOOP('',(#18779,#18780,#18781,#18782));
#4446=EDGE_LOOP('',(#18783,#18784,#18785,#18786));
#4447=EDGE_LOOP('',(#18787,#18788,#18789,#18790));
#4448=EDGE_LOOP('',(#18791,#18792,#18793,#18794));
#4449=EDGE_LOOP('',(#18795,#18796,#18797,#18798));
#4450=EDGE_LOOP('',(#18799,#18800,#18801,#18802));
#4451=EDGE_LOOP('',(#18803,#18804,#18805,#18806));
#4452=EDGE_LOOP('',(#18807,#18808,#18809,#18810));
#4453=EDGE_LOOP('',(#18811,#18812,#18813,#18814));
#4454=EDGE_LOOP('',(#18815,#18816,#18817,#18818));
#4455=EDGE_LOOP('',(#18819,#18820,#18821,#18822));
#4456=EDGE_LOOP('',(#18823,#18824,#18825,#18826));
#4457=EDGE_LOOP('',(#18827,#18828,#18829,#18830));
#4458=EDGE_LOOP('',(#18831,#18832,#18833,#18834));
#4459=EDGE_LOOP('',(#18835,#18836,#18837,#18838));
#4460=EDGE_LOOP('',(#18839,#18840,#18841,#18842));
#4461=EDGE_LOOP('',(#18843,#18844,#18845,#18846));
#4462=EDGE_LOOP('',(#18847,#18848,#18849,#18850));
#4463=EDGE_LOOP('',(#18851,#18852,#18853,#18854));
#4464=EDGE_LOOP('',(#18855,#18856,#18857,#18858));
#4465=EDGE_LOOP('',(#18859,#18860,#18861,#18862));
#4466=EDGE_LOOP('',(#18863,#18864,#18865,#18866));
#4467=EDGE_LOOP('',(#18867,#18868,#18869,#18870));
#4468=EDGE_LOOP('',(#18871,#18872,#18873,#18874));
#4469=EDGE_LOOP('',(#18875,#18876,#18877,#18878));
#4470=EDGE_LOOP('',(#18879,#18880,#18881,#18882));
#4471=EDGE_LOOP('',(#18883,#18884,#18885,#18886));
#4472=EDGE_LOOP('',(#18887,#18888,#18889,#18890));
#4473=EDGE_LOOP('',(#18891,#18892,#18893,#18894));
#4474=EDGE_LOOP('',(#18895,#18896,#18897,#18898));
#4475=EDGE_LOOP('',(#18899,#18900,#18901,#18902));
#4476=EDGE_LOOP('',(#18903,#18904,#18905,#18906));
#4477=EDGE_LOOP('',(#18907,#18908,#18909,#18910));
#4478=EDGE_LOOP('',(#18911,#18912,#18913,#18914));
#4479=EDGE_LOOP('',(#18915,#18916,#18917,#18918));
#4480=EDGE_LOOP('',(#18919,#18920,#18921,#18922));
#4481=EDGE_LOOP('',(#18923,#18924,#18925,#18926));
#4482=EDGE_LOOP('',(#18927,#18928,#18929,#18930));
#4483=EDGE_LOOP('',(#18931,#18932,#18933,#18934));
#4484=EDGE_LOOP('',(#18935,#18936,#18937,#18938));
#4485=EDGE_LOOP('',(#18939,#18940,#18941,#18942));
#4486=EDGE_LOOP('',(#18943,#18944,#18945,#18946));
#4487=EDGE_LOOP('',(#18947,#18948,#18949,#18950));
#4488=EDGE_LOOP('',(#18951,#18952,#18953,#18954));
#4489=EDGE_LOOP('',(#18955,#18956,#18957,#18958));
#4490=EDGE_LOOP('',(#18959,#18960,#18961,#18962));
#4491=EDGE_LOOP('',(#18963,#18964,#18965,#18966));
#4492=EDGE_LOOP('',(#18967,#18968,#18969,#18970));
#4493=EDGE_LOOP('',(#18971,#18972,#18973,#18974));
#4494=EDGE_LOOP('',(#18975,#18976,#18977,#18978));
#4495=EDGE_LOOP('',(#18979,#18980,#18981,#18982));
#4496=EDGE_LOOP('',(#18983,#18984,#18985,#18986));
#4497=EDGE_LOOP('',(#18987,#18988,#18989,#18990));
#4498=EDGE_LOOP('',(#18991,#18992,#18993,#18994));
#4499=EDGE_LOOP('',(#18995,#18996,#18997,#18998));
#4500=EDGE_LOOP('',(#18999,#19000,#19001,#19002));
#4501=EDGE_LOOP('',(#19003,#19004,#19005,#19006));
#4502=EDGE_LOOP('',(#19007,#19008,#19009,#19010));
#4503=EDGE_LOOP('',(#19011,#19012,#19013,#19014));
#4504=EDGE_LOOP('',(#19015,#19016,#19017,#19018));
#4505=EDGE_LOOP('',(#19019,#19020,#19021,#19022));
#4506=EDGE_LOOP('',(#19023,#19024,#19025,#19026));
#4507=EDGE_LOOP('',(#19027,#19028,#19029,#19030));
#4508=EDGE_LOOP('',(#19031,#19032,#19033,#19034));
#4509=EDGE_LOOP('',(#19035,#19036,#19037,#19038));
#4510=EDGE_LOOP('',(#19039,#19040,#19041,#19042));
#4511=EDGE_LOOP('',(#19043,#19044,#19045,#19046));
#4512=EDGE_LOOP('',(#19047,#19048,#19049,#19050));
#4513=EDGE_LOOP('',(#19051,#19052,#19053,#19054));
#4514=EDGE_LOOP('',(#19055,#19056,#19057,#19058));
#4515=EDGE_LOOP('',(#19059,#19060,#19061,#19062));
#4516=EDGE_LOOP('',(#19063,#19064,#19065,#19066));
#4517=EDGE_LOOP('',(#19067,#19068,#19069,#19070));
#4518=EDGE_LOOP('',(#19071,#19072,#19073,#19074));
#4519=EDGE_LOOP('',(#19075,#19076,#19077,#19078));
#4520=EDGE_LOOP('',(#19079,#19080,#19081,#19082));
#4521=EDGE_LOOP('',(#19083,#19084,#19085,#19086));
#4522=EDGE_LOOP('',(#19087,#19088,#19089,#19090));
#4523=EDGE_LOOP('',(#19091,#19092,#19093,#19094));
#4524=EDGE_LOOP('',(#19095,#19096,#19097,#19098));
#4525=EDGE_LOOP('',(#19099,#19100,#19101,#19102));
#4526=EDGE_LOOP('',(#19103,#19104,#19105,#19106));
#4527=EDGE_LOOP('',(#19107));
#4528=EDGE_LOOP('',(#19108));
#4529=EDGE_LOOP('',(#19109,#19110,#19111,#19112));
#4530=EDGE_LOOP('',(#19113,#19114,#19115,#19116));
#4531=EDGE_LOOP('',(#19117,#19118,#19119,#19120));
#4532=EDGE_LOOP('',(#19121,#19122,#19123,#19124));
#4533=EDGE_LOOP('',(#19125,#19126,#19127,#19128));
#4534=EDGE_LOOP('',(#19129,#19130,#19131,#19132));
#4535=EDGE_LOOP('',(#19133,#19134,#19135,#19136));
#4536=EDGE_LOOP('',(#19137,#19138,#19139,#19140));
#4537=EDGE_LOOP('',(#19141,#19142,#19143,#19144));
#4538=EDGE_LOOP('',(#19145,#19146,#19147,#19148));
#4539=EDGE_LOOP('',(#19149,#19150,#19151,#19152));
#4540=EDGE_LOOP('',(#19153,#19154,#19155,#19156));
#4541=EDGE_LOOP('',(#19157,#19158,#19159,#19160));
#4542=EDGE_LOOP('',(#19161,#19162,#19163,#19164));
#4543=EDGE_LOOP('',(#19165,#19166,#19167,#19168));
#4544=EDGE_LOOP('',(#19169,#19170,#19171,#19172));
#4545=EDGE_LOOP('',(#19173,#19174,#19175,#19176));
#4546=EDGE_LOOP('',(#19177,#19178,#19179,#19180));
#4547=EDGE_LOOP('',(#19181,#19182,#19183,#19184));
#4548=EDGE_LOOP('',(#19185,#19186,#19187,#19188));
#4549=EDGE_LOOP('',(#19189,#19190,#19191,#19192));
#4550=EDGE_LOOP('',(#19193,#19194,#19195,#19196));
#4551=EDGE_LOOP('',(#19197,#19198,#19199,#19200));
#4552=EDGE_LOOP('',(#19201,#19202,#19203,#19204));
#4553=EDGE_LOOP('',(#19205,#19206,#19207,#19208));
#4554=EDGE_LOOP('',(#19209,#19210,#19211,#19212));
#4555=EDGE_LOOP('',(#19213));
#4556=EDGE_LOOP('',(#19214));
#4557=EDGE_LOOP('',(#19215,#19216,#19217,#19218));
#4558=EDGE_LOOP('',(#19219));
#4559=EDGE_LOOP('',(#19220));
#4560=EDGE_LOOP('',(#19221,#19222,#19223,#19224,#19225,#19226));
#4561=EDGE_LOOP('',(#19227,#19228,#19229,#19230,#19231));
#4562=EDGE_LOOP('',(#19232,#19233,#19234,#19235));
#4563=EDGE_LOOP('',(#19236));
#4564=EDGE_LOOP('',(#19237,#19238,#19239,#19240));
#4565=EDGE_LOOP('',(#19241,#19242,#19243,#19244));
#4566=EDGE_LOOP('',(#19245,#19246,#19247,#19248));
#4567=EDGE_LOOP('',(#19249,#19250,#19251,#19252));
#4568=EDGE_LOOP('',(#19253,#19254,#19255,#19256));
#4569=EDGE_LOOP('',(#19257,#19258,#19259,#19260));
#4570=EDGE_LOOP('',(#19261,#19262,#19263,#19264));
#4571=EDGE_LOOP('',(#19265,#19266,#19267,#19268));
#4572=EDGE_LOOP('',(#19269,#19270,#19271,#19272));
#4573=EDGE_LOOP('',(#19273,#19274,#19275,#19276));
#4574=EDGE_LOOP('',(#19277,#19278,#19279,#19280));
#4575=EDGE_LOOP('',(#19281,#19282,#19283,#19284));
#4576=EDGE_LOOP('',(#19285,#19286,#19287,#19288));
#4577=EDGE_LOOP('',(#19289,#19290,#19291,#19292));
#4578=EDGE_LOOP('',(#19293,#19294,#19295,#19296));
#4579=EDGE_LOOP('',(#19297,#19298,#19299,#19300));
#4580=EDGE_LOOP('',(#19301,#19302,#19303,#19304));
#4581=EDGE_LOOP('',(#19305,#19306,#19307,#19308));
#4582=EDGE_LOOP('',(#19309,#19310,#19311,#19312));
#4583=EDGE_LOOP('',(#19313,#19314,#19315,#19316));
#4584=EDGE_LOOP('',(#19317,#19318,#19319,#19320));
#4585=EDGE_LOOP('',(#19321,#19322,#19323,#19324));
#4586=EDGE_LOOP('',(#19325,#19326,#19327,#19328));
#4587=EDGE_LOOP('',(#19329,#19330,#19331,#19332));
#4588=EDGE_LOOP('',(#19333,#19334,#19335,#19336));
#4589=EDGE_LOOP('',(#19337,#19338,#19339,#19340));
#4590=EDGE_LOOP('',(#19341,#19342,#19343,#19344));
#4591=EDGE_LOOP('',(#19345,#19346,#19347,#19348));
#4592=EDGE_LOOP('',(#19349,#19350,#19351,#19352));
#4593=EDGE_LOOP('',(#19353,#19354,#19355,#19356));
#4594=EDGE_LOOP('',(#19357,#19358,#19359,#19360));
#4595=EDGE_LOOP('',(#19361,#19362,#19363,#19364));
#4596=EDGE_LOOP('',(#19365,#19366,#19367,#19368));
#4597=EDGE_LOOP('',(#19369,#19370,#19371,#19372));
#4598=EDGE_LOOP('',(#19373,#19374,#19375,#19376));
#4599=EDGE_LOOP('',(#19377,#19378,#19379,#19380));
#4600=EDGE_LOOP('',(#19381,#19382,#19383,#19384));
#4601=EDGE_LOOP('',(#19385,#19386,#19387,#19388));
#4602=EDGE_LOOP('',(#19389,#19390,#19391,#19392));
#4603=EDGE_LOOP('',(#19393,#19394,#19395,#19396));
#4604=EDGE_LOOP('',(#19397,#19398,#19399,#19400));
#4605=EDGE_LOOP('',(#19401,#19402,#19403,#19404));
#4606=EDGE_LOOP('',(#19405,#19406,#19407,#19408));
#4607=EDGE_LOOP('',(#19409,#19410,#19411,#19412));
#4608=EDGE_LOOP('',(#19413,#19414,#19415,#19416));
#4609=EDGE_LOOP('',(#19417,#19418,#19419,#19420));
#4610=EDGE_LOOP('',(#19421,#19422,#19423,#19424));
#4611=EDGE_LOOP('',(#19425,#19426,#19427,#19428));
#4612=EDGE_LOOP('',(#19429,#19430,#19431,#19432));
#4613=EDGE_LOOP('',(#19433,#19434,#19435,#19436));
#4614=EDGE_LOOP('',(#19437,#19438,#19439,#19440));
#4615=EDGE_LOOP('',(#19441,#19442,#19443,#19444));
#4616=EDGE_LOOP('',(#19445,#19446,#19447,#19448));
#4617=EDGE_LOOP('',(#19449,#19450,#19451,#19452));
#4618=EDGE_LOOP('',(#19453,#19454,#19455,#19456));
#4619=EDGE_LOOP('',(#19457,#19458,#19459,#19460));
#4620=EDGE_LOOP('',(#19461,#19462,#19463,#19464));
#4621=EDGE_LOOP('',(#19465,#19466,#19467,#19468));
#4622=EDGE_LOOP('',(#19469,#19470,#19471,#19472));
#4623=EDGE_LOOP('',(#19473,#19474,#19475,#19476));
#4624=EDGE_LOOP('',(#19477,#19478,#19479,#19480));
#4625=EDGE_LOOP('',(#19481,#19482,#19483,#19484));
#4626=EDGE_LOOP('',(#19485,#19486,#19487,#19488));
#4627=EDGE_LOOP('',(#19489,#19490,#19491,#19492));
#4628=EDGE_LOOP('',(#19493,#19494,#19495,#19496));
#4629=EDGE_LOOP('',(#19497,#19498,#19499,#19500));
#4630=EDGE_LOOP('',(#19501,#19502,#19503,#19504));
#4631=EDGE_LOOP('',(#19505,#19506,#19507,#19508));
#4632=EDGE_LOOP('',(#19509,#19510,#19511,#19512));
#4633=EDGE_LOOP('',(#19513,#19514,#19515,#19516));
#4634=EDGE_LOOP('',(#19517,#19518,#19519,#19520));
#4635=EDGE_LOOP('',(#19521,#19522,#19523,#19524));
#4636=EDGE_LOOP('',(#19525,#19526,#19527,#19528));
#4637=EDGE_LOOP('',(#19529,#19530,#19531,#19532));
#4638=EDGE_LOOP('',(#19533,#19534,#19535,#19536));
#4639=EDGE_LOOP('',(#19537,#19538,#19539,#19540));
#4640=EDGE_LOOP('',(#19541,#19542,#19543,#19544));
#4641=EDGE_LOOP('',(#19545,#19546,#19547,#19548));
#4642=EDGE_LOOP('',(#19549,#19550,#19551,#19552));
#4643=EDGE_LOOP('',(#19553,#19554,#19555,#19556));
#4644=EDGE_LOOP('',(#19557,#19558,#19559,#19560));
#4645=EDGE_LOOP('',(#19561,#19562,#19563,#19564));
#4646=EDGE_LOOP('',(#19565,#19566,#19567,#19568));
#4647=EDGE_LOOP('',(#19569,#19570,#19571,#19572));
#4648=EDGE_LOOP('',(#19573,#19574,#19575,#19576));
#4649=EDGE_LOOP('',(#19577,#19578,#19579,#19580));
#4650=EDGE_LOOP('',(#19581,#19582,#19583,#19584,#19585));
#4651=EDGE_LOOP('',(#19586,#19587,#19588,#19589,#19590,#19591,#19592));
#4652=EDGE_LOOP('',(#19593));
#4653=EDGE_LOOP('',(#19594,#19595,#19596,#19597));
#4654=EDGE_LOOP('',(#19598,#19599,#19600,#19601));
#4655=EDGE_LOOP('',(#19602));
#4656=EDGE_LOOP('',(#19603));
#4657=EDGE_LOOP('',(#19604,#19605,#19606,#19607,#19608));
#4658=EDGE_LOOP('',(#19609,#19610,#19611,#19612,#19613,#19614,#19615,#19616,
#19617,#19618,#19619,#19620,#19621,#19622,#19623,#19624,#19625,#19626,#19627,
#19628,#19629,#19630,#19631,#19632,#19633,#19634,#19635,#19636,#19637,#19638,
#19639,#19640,#19641,#19642,#19643,#19644,#19645,#19646,#19647,#19648,#19649,
#19650,#19651,#19652,#19653,#19654,#19655,#19656,#19657,#19658,#19659,#19660,
#19661,#19662,#19663,#19664,#19665,#19666,#19667,#19668,#19669,#19670,#19671,
#19672,#19673,#19674,#19675,#19676,#19677,#19678,#19679,#19680,#19681,#19682,
#19683,#19684,#19685,#19686,#19687,#19688,#19689,#19690,#19691,#19692,#19693,
#19694,#19695,#19696,#19697,#19698));
#4659=EDGE_LOOP('',(#19699,#19700,#19701,#19702));
#4660=EDGE_LOOP('',(#19703,#19704,#19705,#19706));
#4661=EDGE_LOOP('',(#19707,#19708,#19709,#19710,#19711,#19712,#19713,#19714,
#19715,#19716,#19717,#19718,#19719,#19720,#19721,#19722,#19723,#19724,#19725,
#19726,#19727,#19728,#19729,#19730,#19731,#19732,#19733,#19734,#19735,#19736,
#19737,#19738,#19739,#19740,#19741,#19742,#19743,#19744,#19745,#19746,#19747,
#19748,#19749,#19750,#19751,#19752,#19753,#19754,#19755,#19756,#19757,#19758,
#19759,#19760,#19761,#19762,#19763,#19764,#19765,#19766,#19767,#19768,#19769,
#19770,#19771,#19772,#19773,#19774,#19775,#19776,#19777,#19778,#19779,#19780,
#19781,#19782,#19783,#19784,#19785,#19786,#19787,#19788,#19789,#19790,#19791,
#19792,#19793,#19794,#19795,#19796));
#4662=EDGE_LOOP('',(#19797,#19798,#19799,#19800));
#4663=EDGE_LOOP('',(#19801,#19802,#19803,#19804));
#4664=EDGE_LOOP('',(#19805,#19806,#19807));
#4665=EDGE_LOOP('',(#19808,#19809,#19810,#19811));
#4666=EDGE_LOOP('',(#19812,#19813,#19814,#19815));
#4667=EDGE_LOOP('',(#19816,#19817,#19818,#19819));
#4668=EDGE_LOOP('',(#19820,#19821,#19822,#19823));
#4669=EDGE_LOOP('',(#19824,#19825,#19826,#19827));
#4670=EDGE_LOOP('',(#19828,#19829,#19830,#19831));
#4671=EDGE_LOOP('',(#19832,#19833,#19834,#19835));
#4672=EDGE_LOOP('',(#19836,#19837,#19838,#19839));
#4673=EDGE_LOOP('',(#19840));
#4674=EDGE_LOOP('',(#19841));
#4675=EDGE_LOOP('',(#19842,#19843,#19844,#19845));
#4676=EDGE_LOOP('',(#19846,#19847,#19848,#19849));
#4677=EDGE_LOOP('',(#19850,#19851,#19852,#19853));
#4678=EDGE_LOOP('',(#19854));
#4679=EDGE_LOOP('',(#19855,#19856,#19857,#19858));
#4680=EDGE_LOOP('',(#19859,#19860,#19861,#19862,#19863));
#4681=EDGE_LOOP('',(#19864,#19865,#19866,#19867,#19868,#19869));
#4682=EDGE_LOOP('',(#19870));
#4683=EDGE_LOOP('',(#19871));
#4684=EDGE_LOOP('',(#19872,#19873,#19874,#19875,#19876,#19877));
#4685=EDGE_LOOP('',(#19878,#19879,#19880,#19881,#19882));
#4686=EDGE_LOOP('',(#19883));
#4687=EDGE_LOOP('',(#19884));
#4688=EDGE_LOOP('',(#19885,#19886,#19887,#19888));
#4689=EDGE_LOOP('',(#19889));
#4690=EDGE_LOOP('',(#19890));
#4691=EDGE_LOOP('',(#19891,#19892,#19893,#19894));
#4692=EDGE_LOOP('',(#19895,#19896,#19897,#19898));
#4693=EDGE_LOOP('',(#19899,#19900,#19901,#19902));
#4694=EDGE_LOOP('',(#19903,#19904,#19905,#19906));
#4695=EDGE_LOOP('',(#19907));
#4696=EDGE_LOOP('',(#19908));
#4697=EDGE_LOOP('',(#19909,#19910,#19911,#19912));
#4698=EDGE_LOOP('',(#19913,#19914,#19915,#19916,#19917));
#4699=EDGE_LOOP('',(#19918));
#4700=EDGE_LOOP('',(#19919));
#4701=EDGE_LOOP('',(#19920,#19921,#19922,#19923,#19924));
#4702=EDGE_LOOP('',(#19925,#19926,#19927,#19928,#19929));
#4703=EDGE_LOOP('',(#19930,#19931,#19932,#19933,#19934,#19935));
#4704=EDGE_LOOP('',(#19936));
#4705=EDGE_LOOP('',(#19937));
#4706=EDGE_LOOP('',(#19938));
#4707=EDGE_LOOP('',(#19939));
#4708=EDGE_LOOP('',(#19940));
#4709=EDGE_LOOP('',(#19941));
#4710=EDGE_LOOP('',(#19942,#19943,#19944,#19945,#19946,#19947));
#4711=EDGE_LOOP('',(#19948,#19949,#19950,#19951,#19952,#19953));
#4712=EDGE_LOOP('',(#19954,#19955,#19956,#19957,#19958,#19959));
#4713=EDGE_LOOP('',(#19960,#19961,#19962,#19963,#19964,#19965));
#4714=EDGE_LOOP('',(#19966,#19967,#19968,#19969,#19970));
#4715=EDGE_LOOP('',(#19971));
#4716=EDGE_LOOP('',(#19972));
#4717=EDGE_LOOP('',(#19973));
#4718=EDGE_LOOP('',(#19974));
#4719=EDGE_LOOP('',(#19975));
#4720=EDGE_LOOP('',(#19976));
#4721=EDGE_LOOP('',(#19977,#19978,#19979,#19980,#19981,#19982));
#4722=EDGE_LOOP('',(#19983,#19984,#19985,#19986,#19987,#19988));
#4723=EDGE_LOOP('',(#19989,#19990,#19991,#19992,#19993));
#4724=EDGE_LOOP('',(#19994,#19995,#19996,#19997,#19998));
#4725=EDGE_LOOP('',(#19999));
#4726=EDGE_LOOP('',(#20000));
#4727=EDGE_LOOP('',(#20001,#20002,#20003,#20004,#20005));
#4728=EDGE_LOOP('',(#20006,#20007,#20008,#20009,#20010));
#4729=EDGE_LOOP('',(#20011,#20012,#20013,#20014));
#4730=EDGE_LOOP('',(#20015,#20016,#20017,#20018));
#4731=EDGE_LOOP('',(#20019,#20020,#20021,#20022));
#4732=EDGE_LOOP('',(#20023,#20024,#20025,#20026));
#4733=EDGE_LOOP('',(#20027,#20028,#20029,#20030));
#4734=EDGE_LOOP('',(#20031,#20032,#20033,#20034));
#4735=EDGE_LOOP('',(#20035));
#4736=EDGE_LOOP('',(#20036));
#4737=EDGE_LOOP('',(#20037,#20038,#20039,#20040));
#4738=EDGE_LOOP('',(#20041));
#4739=EDGE_LOOP('',(#20042));
#4740=EDGE_LOOP('',(#20043,#20044,#20045,#20046,#20047,#20048));
#4741=EDGE_LOOP('',(#20049,#20050,#20051,#20052,#20053,#20054));
#4742=EDGE_LOOP('',(#20055,#20056));
#4743=EDGE_LOOP('',(#20057,#20058));
#4744=EDGE_LOOP('',(#20059,#20060));
#4745=EDGE_LOOP('',(#20061,#20062));
#4746=EDGE_LOOP('',(#20063,#20064,#20065,#20066,#20067,#20068));
#4747=EDGE_LOOP('',(#20069,#20070,#20071,#20072,#20073,#20074));
#4748=EDGE_LOOP('',(#20075,#20076,#20077,#20078,#20079,#20080));
#4749=EDGE_LOOP('',(#20081,#20082,#20083,#20084,#20085));
#4750=EDGE_LOOP('',(#20086));
#4751=EDGE_LOOP('',(#20087));
#4752=EDGE_LOOP('',(#20088,#20089,#20090,#20091,#20092));
#4753=EDGE_LOOP('',(#20093));
#4754=EDGE_LOOP('',(#20094,#20095,#20096,#20097));
#4755=EDGE_LOOP('',(#20098,#20099,#20100,#20101));
#4756=EDGE_LOOP('',(#20102,#20103,#20104,#20105));
#4757=EDGE_LOOP('',(#20106,#20107,#20108,#20109));
#4758=EDGE_LOOP('',(#20110,#20111,#20112,#20113));
#4759=EDGE_LOOP('',(#20114,#20115,#20116,#20117));
#4760=EDGE_LOOP('',(#20118,#20119,#20120,#20121));
#4761=EDGE_LOOP('',(#20122,#20123,#20124,#20125,#20126,#20127));
#4762=EDGE_LOOP('',(#20128,#20129,#20130,#20131,#20132,#20133,#20134));
#4763=EDGE_LOOP('',(#20135,#20136,#20137,#20138,#20139,#20140,#20141));
#4764=EDGE_LOOP('',(#20142,#20143,#20144,#20145,#20146,#20147,#20148));
#4765=EDGE_LOOP('',(#20149,#20150,#20151,#20152,#20153,#20154,#20155));
#4766=EDGE_LOOP('',(#20156,#20157,#20158,#20159,#20160,#20161,#20162,#20163,
#20164,#20165,#20166,#20167,#20168,#20169,#20170,#20171,#20172,#20173,#20174,
#20175,#20176,#20177,#20178,#20179));
#4767=EDGE_LOOP('',(#20180,#20181,#20182,#20183));
#4768=EDGE_LOOP('',(#20184,#20185,#20186,#20187));
#4769=EDGE_LOOP('',(#20188));
#4770=EDGE_LOOP('',(#20189,#20190,#20191,#20192));
#4771=EDGE_LOOP('',(#20193,#20194,#20195,#20196));
#4772=EDGE_LOOP('',(#20197,#20198,#20199,#20200));
#4773=EDGE_LOOP('',(#20201,#20202,#20203,#20204));
#4774=EDGE_LOOP('',(#20205,#20206,#20207,#20208));
#4775=EDGE_LOOP('',(#20209,#20210,#20211,#20212));
#4776=EDGE_LOOP('',(#20213,#20214,#20215,#20216));
#4777=EDGE_LOOP('',(#20217,#20218,#20219,#20220));
#4778=EDGE_LOOP('',(#20221,#20222,#20223,#20224));
#4779=EDGE_LOOP('',(#20225,#20226,#20227,#20228));
#4780=EDGE_LOOP('',(#20229,#20230,#20231,#20232));
#4781=EDGE_LOOP('',(#20233,#20234,#20235,#20236));
#4782=EDGE_LOOP('',(#20237,#20238,#20239,#20240));
#4783=EDGE_LOOP('',(#20241,#20242,#20243,#20244));
#4784=EDGE_LOOP('',(#20245,#20246,#20247,#20248));
#4785=EDGE_LOOP('',(#20249,#20250,#20251,#20252));
#4786=EDGE_LOOP('',(#20253,#20254,#20255,#20256));
#4787=EDGE_LOOP('',(#20257,#20258,#20259,#20260));
#4788=EDGE_LOOP('',(#20261,#20262,#20263,#20264));
#4789=EDGE_LOOP('',(#20265,#20266,#20267,#20268));
#4790=EDGE_LOOP('',(#20269,#20270,#20271,#20272));
#4791=EDGE_LOOP('',(#20273,#20274,#20275,#20276));
#4792=EDGE_LOOP('',(#20277,#20278,#20279,#20280));
#4793=EDGE_LOOP('',(#20281,#20282,#20283,#20284));
#4794=EDGE_LOOP('',(#20285,#20286,#20287,#20288));
#4795=EDGE_LOOP('',(#20289,#20290,#20291,#20292));
#4796=EDGE_LOOP('',(#20293,#20294,#20295,#20296));
#4797=EDGE_LOOP('',(#20297,#20298,#20299,#20300));
#4798=EDGE_LOOP('',(#20301,#20302,#20303,#20304));
#4799=EDGE_LOOP('',(#20305,#20306,#20307,#20308));
#4800=EDGE_LOOP('',(#20309,#20310,#20311,#20312));
#4801=EDGE_LOOP('',(#20313,#20314,#20315,#20316,#20317));
#4802=EDGE_LOOP('',(#20318,#20319,#20320,#20321,#20322,#20323,#20324,#20325,
#20326,#20327,#20328,#20329,#20330,#20331,#20332,#20333,#20334,#20335,#20336,
#20337,#20338,#20339,#20340,#20341,#20342,#20343,#20344,#20345,#20346,#20347,
#20348,#20349,#20350,#20351,#20352));
#4803=EDGE_LOOP('',(#20353,#20354,#20355,#20356,#20357));
#4804=EDGE_LOOP('',(#20358,#20359,#20360,#20361));
#4805=EDGE_LOOP('',(#20362,#20363,#20364,#20365,#20366,#20367,#20368,#20369,
#20370,#20371,#20372,#20373,#20374,#20375,#20376,#20377,#20378,#20379,#20380,
#20381,#20382,#20383,#20384,#20385,#20386,#20387,#20388,#20389,#20390,#20391,
#20392,#20393,#20394,#20395,#20396));
#4806=EDGE_LOOP('',(#20397,#20398,#20399,#20400,#20401,#20402));
#4807=EDGE_LOOP('',(#20403,#20404,#20405,#20406));
#4808=EDGE_LOOP('',(#20407));
#4809=EDGE_LOOP('',(#20408));
#4810=EDGE_LOOP('',(#20409,#20410));
#4811=EDGE_LOOP('',(#20411,#20412));
#4812=EDGE_LOOP('',(#20413,#20414));
#4813=EDGE_LOOP('',(#20415,#20416));
#4814=EDGE_LOOP('',(#20417,#20418));
#4815=EDGE_LOOP('',(#20419,#20420));
#4816=EDGE_LOOP('',(#20421,#20422,#20423,#20424,#20425,#20426,#20427,#20428));
#4817=EDGE_LOOP('',(#20429,#20430,#20431,#20432));
#4818=EDGE_LOOP('',(#20433,#20434,#20435,#20436));
#4819=EDGE_LOOP('',(#20437,#20438,#20439,#20440));
#4820=EDGE_LOOP('',(#20441,#20442,#20443,#20444));
#4821=EDGE_LOOP('',(#20445,#20446,#20447,#20448));
#4822=EDGE_LOOP('',(#20449,#20450,#20451,#20452));
#4823=EDGE_LOOP('',(#20453,#20454,#20455,#20456));
#4824=EDGE_LOOP('',(#20457,#20458,#20459));
#4825=EDGE_LOOP('',(#20460,#20461,#20462,#20463));
#4826=EDGE_LOOP('',(#20464,#20465,#20466));
#4827=EDGE_LOOP('',(#20467,#20468,#20469,#20470));
#4828=EDGE_LOOP('',(#20471,#20472,#20473));
#4829=EDGE_LOOP('',(#20474,#20475,#20476,#20477));
#4830=EDGE_LOOP('',(#20478,#20479,#20480));
#4831=EDGE_LOOP('',(#20481,#20482,#20483,#20484));
#4832=EDGE_LOOP('',(#20485,#20486,#20487));
#4833=EDGE_LOOP('',(#20488,#20489,#20490,#20491));
#4834=EDGE_LOOP('',(#20492,#20493,#20494));
#4835=EDGE_LOOP('',(#20495,#20496,#20497,#20498));
#4836=EDGE_LOOP('',(#20499,#20500,#20501));
#4837=EDGE_LOOP('',(#20502,#20503,#20504,#20505));
#4838=EDGE_LOOP('',(#20506,#20507,#20508));
#4839=EDGE_LOOP('',(#20509,#20510,#20511,#20512));
#4840=EDGE_LOOP('',(#20513,#20514,#20515));
#4841=EDGE_LOOP('',(#20516,#20517,#20518,#20519));
#4842=EDGE_LOOP('',(#20520,#20521,#20522));
#4843=EDGE_LOOP('',(#20523,#20524,#20525,#20526));
#4844=EDGE_LOOP('',(#20527,#20528,#20529));
#4845=EDGE_LOOP('',(#20530,#20531,#20532,#20533));
#4846=EDGE_LOOP('',(#20534,#20535,#20536));
#4847=EDGE_LOOP('',(#20537,#20538,#20539,#20540));
#4848=EDGE_LOOP('',(#20541,#20542,#20543));
#4849=EDGE_LOOP('',(#20544,#20545,#20546,#20547));
#4850=EDGE_LOOP('',(#20548,#20549,#20550));
#4851=EDGE_LOOP('',(#20551,#20552,#20553,#20554));
#4852=EDGE_LOOP('',(#20555,#20556,#20557));
#4853=EDGE_LOOP('',(#20558,#20559,#20560,#20561));
#4854=EDGE_LOOP('',(#20562,#20563,#20564));
#4855=EDGE_LOOP('',(#20565,#20566,#20567,#20568));
#4856=EDGE_LOOP('',(#20569,#20570,#20571,#20572));
#4857=EDGE_LOOP('',(#20573,#20574,#20575,#20576));
#4858=EDGE_LOOP('',(#20577,#20578,#20579,#20580));
#4859=EDGE_LOOP('',(#20581,#20582,#20583,#20584));
#4860=EDGE_LOOP('',(#20585,#20586,#20587));
#4861=EDGE_LOOP('',(#20588,#20589,#20590,#20591));
#4862=EDGE_LOOP('',(#20592,#20593,#20594));
#4863=EDGE_LOOP('',(#20595,#20596,#20597,#20598));
#4864=EDGE_LOOP('',(#20599,#20600,#20601));
#4865=EDGE_LOOP('',(#20602,#20603,#20604,#20605));
#4866=EDGE_LOOP('',(#20606,#20607,#20608));
#4867=EDGE_LOOP('',(#20609,#20610,#20611,#20612));
#4868=EDGE_LOOP('',(#20613,#20614,#20615));
#4869=EDGE_LOOP('',(#20616,#20617,#20618,#20619));
#4870=EDGE_LOOP('',(#20620,#20621,#20622));
#4871=EDGE_LOOP('',(#20623,#20624,#20625,#20626));
#4872=EDGE_LOOP('',(#20627,#20628,#20629));
#4873=EDGE_LOOP('',(#20630,#20631,#20632,#20633));
#4874=EDGE_LOOP('',(#20634,#20635,#20636));
#4875=EDGE_LOOP('',(#20637,#20638,#20639,#20640));
#4876=EDGE_LOOP('',(#20641,#20642,#20643));
#4877=EDGE_LOOP('',(#20644,#20645,#20646,#20647));
#4878=EDGE_LOOP('',(#20648,#20649,#20650));
#4879=EDGE_LOOP('',(#20651,#20652,#20653,#20654));
#4880=EDGE_LOOP('',(#20655,#20656,#20657));
#4881=EDGE_LOOP('',(#20658,#20659,#20660,#20661));
#4882=EDGE_LOOP('',(#20662,#20663,#20664));
#4883=EDGE_LOOP('',(#20665,#20666,#20667,#20668));
#4884=EDGE_LOOP('',(#20669,#20670,#20671));
#4885=EDGE_LOOP('',(#20672,#20673,#20674,#20675));
#4886=EDGE_LOOP('',(#20676,#20677,#20678));
#4887=EDGE_LOOP('',(#20679,#20680,#20681,#20682));
#4888=EDGE_LOOP('',(#20683,#20684,#20685));
#4889=EDGE_LOOP('',(#20686,#20687,#20688,#20689));
#4890=EDGE_LOOP('',(#20690,#20691,#20692));
#4891=EDGE_LOOP('',(#20693,#20694,#20695,#20696));
#4892=EDGE_LOOP('',(#20697,#20698,#20699));
#4893=EDGE_LOOP('',(#20700,#20701,#20702,#20703));
#4894=EDGE_LOOP('',(#20704,#20705,#20706));
#4895=EDGE_LOOP('',(#20707,#20708,#20709,#20710));
#4896=EDGE_LOOP('',(#20711,#20712,#20713));
#4897=EDGE_LOOP('',(#20714,#20715,#20716,#20717));
#4898=EDGE_LOOP('',(#20718,#20719,#20720));
#4899=EDGE_LOOP('',(#20721,#20722,#20723,#20724));
#4900=EDGE_LOOP('',(#20725,#20726,#20727));
#4901=EDGE_LOOP('',(#20728,#20729,#20730,#20731));
#4902=EDGE_LOOP('',(#20732,#20733,#20734));
#4903=EDGE_LOOP('',(#20735,#20736,#20737,#20738));
#4904=EDGE_LOOP('',(#20739,#20740,#20741));
#4905=EDGE_LOOP('',(#20742,#20743,#20744,#20745));
#4906=EDGE_LOOP('',(#20746,#20747,#20748));
#4907=EDGE_LOOP('',(#20749,#20750,#20751,#20752));
#4908=EDGE_LOOP('',(#20753,#20754,#20755));
#4909=EDGE_LOOP('',(#20756,#20757,#20758,#20759));
#4910=EDGE_LOOP('',(#20760,#20761,#20762));
#4911=EDGE_LOOP('',(#20763,#20764,#20765,#20766));
#4912=EDGE_LOOP('',(#20767,#20768,#20769));
#4913=EDGE_LOOP('',(#20770,#20771,#20772,#20773));
#4914=EDGE_LOOP('',(#20774,#20775,#20776));
#4915=EDGE_LOOP('',(#20777,#20778,#20779,#20780));
#4916=EDGE_LOOP('',(#20781,#20782,#20783));
#4917=EDGE_LOOP('',(#20784,#20785,#20786,#20787));
#4918=EDGE_LOOP('',(#20788,#20789,#20790));
#4919=EDGE_LOOP('',(#20791,#20792,#20793,#20794));
#4920=EDGE_LOOP('',(#20795,#20796,#20797));
#4921=EDGE_LOOP('',(#20798,#20799,#20800,#20801));
#4922=EDGE_LOOP('',(#20802,#20803,#20804));
#4923=EDGE_LOOP('',(#20805,#20806,#20807,#20808));
#4924=EDGE_LOOP('',(#20809,#20810,#20811));
#4925=EDGE_LOOP('',(#20812,#20813,#20814,#20815));
#4926=EDGE_LOOP('',(#20816,#20817,#20818));
#4927=EDGE_LOOP('',(#20819,#20820,#20821));
#4928=EDGE_LOOP('',(#20822,#20823,#20824,#20825));
#4929=EDGE_LOOP('',(#20826,#20827,#20828,#20829));
#4930=EDGE_LOOP('',(#20830,#20831,#20832));
#4931=EDGE_LOOP('',(#20833,#20834,#20835,#20836));
#4932=EDGE_LOOP('',(#20837,#20838,#20839));
#4933=EDGE_LOOP('',(#20840,#20841,#20842,#20843));
#4934=EDGE_LOOP('',(#20844,#20845,#20846));
#4935=EDGE_LOOP('',(#20847,#20848,#20849,#20850));
#4936=EDGE_LOOP('',(#20851,#20852,#20853));
#4937=EDGE_LOOP('',(#20854,#20855,#20856,#20857));
#4938=EDGE_LOOP('',(#20858,#20859,#20860));
#4939=EDGE_LOOP('',(#20861,#20862,#20863,#20864));
#4940=EDGE_LOOP('',(#20865,#20866,#20867));
#4941=EDGE_LOOP('',(#20868,#20869,#20870,#20871));
#4942=EDGE_LOOP('',(#20872,#20873,#20874));
#4943=EDGE_LOOP('',(#20875,#20876,#20877,#20878));
#4944=EDGE_LOOP('',(#20879,#20880,#20881));
#4945=EDGE_LOOP('',(#20882,#20883,#20884,#20885));
#4946=EDGE_LOOP('',(#20886,#20887,#20888));
#4947=EDGE_LOOP('',(#20889,#20890,#20891,#20892));
#4948=EDGE_LOOP('',(#20893,#20894,#20895));
#4949=EDGE_LOOP('',(#20896,#20897,#20898,#20899));
#4950=EDGE_LOOP('',(#20900,#20901,#20902));
#4951=EDGE_LOOP('',(#20903,#20904,#20905,#20906));
#4952=EDGE_LOOP('',(#20907,#20908,#20909));
#4953=EDGE_LOOP('',(#20910,#20911,#20912,#20913));
#4954=EDGE_LOOP('',(#20914,#20915,#20916));
#4955=EDGE_LOOP('',(#20917,#20918,#20919,#20920));
#4956=EDGE_LOOP('',(#20921,#20922,#20923));
#4957=EDGE_LOOP('',(#20924,#20925,#20926,#20927));
#4958=EDGE_LOOP('',(#20928,#20929,#20930));
#4959=EDGE_LOOP('',(#20931,#20932,#20933,#20934));
#4960=EDGE_LOOP('',(#20935,#20936,#20937));
#4961=EDGE_LOOP('',(#20938,#20939,#20940,#20941));
#4962=EDGE_LOOP('',(#20942,#20943,#20944));
#4963=EDGE_LOOP('',(#20945,#20946,#20947,#20948));
#4964=EDGE_LOOP('',(#20949,#20950,#20951));
#4965=EDGE_LOOP('',(#20952,#20953,#20954,#20955));
#4966=EDGE_LOOP('',(#20956,#20957,#20958));
#4967=EDGE_LOOP('',(#20959));
#4968=EDGE_LOOP('',(#20960,#20961,#20962,#20963,#20964,#20965));
#4969=EDGE_LOOP('',(#20966,#20967,#20968,#20969));
#4970=EDGE_LOOP('',(#20970,#20971,#20972,#20973,#20974,#20975,#20976,#20977,
#20978,#20979,#20980,#20981,#20982,#20983,#20984,#20985,#20986,#20987,#20988,
#20989,#20990,#20991,#20992,#20993,#20994,#20995,#20996,#20997,#20998,#20999,
#21000,#21001,#21002,#21003,#21004,#21005,#21006,#21007,#21008,#21009,#21010,
#21011,#21012,#21013,#21014,#21015,#21016,#21017,#21018,#21019,#21020,#21021,
#21022,#21023,#21024,#21025,#21026,#21027,#21028,#21029,#21030,#21031,#21032,
#21033,#21034,#21035,#21036,#21037,#21038,#21039,#21040,#21041,#21042,#21043,
#21044,#21045,#21046,#21047,#21048,#21049,#21050,#21051,#21052,#21053,#21054,
#21055,#21056,#21057,#21058,#21059,#21060,#21061,#21062,#21063,#21064,#21065,
#21066,#21067,#21068,#21069,#21070,#21071,#21072,#21073,#21074,#21075,#21076,
#21077,#21078,#21079,#21080,#21081,#21082,#21083,#21084,#21085,#21086,#21087,
#21088,#21089,#21090,#21091,#21092,#21093,#21094,#21095,#21096,#21097,#21098,
#21099,#21100,#21101,#21102,#21103,#21104,#21105,#21106,#21107,#21108,#21109,
#21110,#21111,#21112,#21113,#21114,#21115,#21116,#21117));
#4971=EDGE_LOOP('',(#21118,#21119,#21120,#21121,#21122,#21123,#21124,#21125,
#21126,#21127,#21128,#21129,#21130,#21131,#21132,#21133,#21134,#21135,#21136,
#21137,#21138,#21139,#21140,#21141,#21142,#21143,#21144,#21145,#21146,#21147,
#21148,#21149,#21150,#21151,#21152,#21153,#21154,#21155,#21156,#21157,#21158,
#21159,#21160,#21161,#21162,#21163,#21164,#21165,#21166,#21167,#21168,#21169,
#21170,#21171,#21172,#21173,#21174,#21175,#21176,#21177,#21178,#21179,#21180,
#21181,#21182,#21183,#21184,#21185,#21186,#21187,#21188,#21189,#21190,#21191,
#21192,#21193));
#4972=EDGE_LOOP('',(#21194));
#4973=EDGE_LOOP('',(#21195,#21196,#21197,#21198,#21199,#21200));
#4974=EDGE_LOOP('',(#21201,#21202,#21203,#21204));
#4975=EDGE_LOOP('',(#21205,#21206,#21207,#21208));
#4976=EDGE_LOOP('',(#21209,#21210,#21211,#21212));
#4977=EDGE_LOOP('',(#21213,#21214,#21215,#21216));
#4978=EDGE_LOOP('',(#21217,#21218,#21219,#21220));
#4979=EDGE_LOOP('',(#21221,#21222,#21223,#21224));
#4980=EDGE_LOOP('',(#21225,#21226,#21227,#21228));
#4981=EDGE_LOOP('',(#21229,#21230,#21231,#21232));
#4982=EDGE_LOOP('',(#21233,#21234,#21235,#21236));
#4983=EDGE_LOOP('',(#21237,#21238,#21239,#21240));
#4984=EDGE_LOOP('',(#21241,#21242,#21243,#21244));
#4985=EDGE_LOOP('',(#21245,#21246,#21247,#21248));
#4986=EDGE_LOOP('',(#21249,#21250,#21251,#21252));
#4987=EDGE_LOOP('',(#21253,#21254,#21255,#21256));
#4988=EDGE_LOOP('',(#21257,#21258,#21259,#21260));
#4989=EDGE_LOOP('',(#21261,#21262,#21263,#21264));
#4990=EDGE_LOOP('',(#21265,#21266,#21267,#21268));
#4991=EDGE_LOOP('',(#21269,#21270,#21271,#21272));
#4992=EDGE_LOOP('',(#21273,#21274,#21275,#21276));
#4993=EDGE_LOOP('',(#21277,#21278,#21279,#21280));
#4994=EDGE_LOOP('',(#21281,#21282,#21283,#21284));
#4995=EDGE_LOOP('',(#21285,#21286,#21287,#21288));
#4996=EDGE_LOOP('',(#21289,#21290,#21291,#21292));
#4997=EDGE_LOOP('',(#21293,#21294,#21295,#21296));
#4998=EDGE_LOOP('',(#21297,#21298,#21299,#21300));
#4999=EDGE_LOOP('',(#21301,#21302,#21303,#21304));
#5000=EDGE_LOOP('',(#21305,#21306,#21307,#21308));
#5001=EDGE_LOOP('',(#21309,#21310,#21311,#21312));
#5002=EDGE_LOOP('',(#21313,#21314,#21315,#21316));
#5003=EDGE_LOOP('',(#21317,#21318,#21319,#21320));
#5004=EDGE_LOOP('',(#21321,#21322,#21323,#21324));
#5005=EDGE_LOOP('',(#21325,#21326,#21327,#21328));
#5006=EDGE_LOOP('',(#21329,#21330,#21331,#21332));
#5007=EDGE_LOOP('',(#21333,#21334,#21335,#21336));
#5008=EDGE_LOOP('',(#21337,#21338,#21339,#21340,#21341));
#5009=EDGE_LOOP('',(#21342,#21343,#21344,#21345,#21346,#21347,#21348,#21349,
#21350,#21351,#21352,#21353,#21354,#21355,#21356,#21357,#21358,#21359,#21360,
#21361,#21362,#21363,#21364));
#5010=EDGE_LOOP('',(#21365,#21366,#21367,#21368,#21369));
#5011=EDGE_LOOP('',(#21370,#21371,#21372,#21373));
#5012=EDGE_LOOP('',(#21374,#21375,#21376,#21377,#21378,#21379,#21380,#21381,
#21382,#21383,#21384,#21385,#21386,#21387,#21388,#21389,#21390,#21391,#21392,
#21393,#21394,#21395,#21396));
#5013=EDGE_LOOP('',(#21397,#21398,#21399,#21400,#21401,#21402,#21403,#21404,
#21405,#21406,#21407,#21408,#21409,#21410));
#5014=EDGE_LOOP('',(#21411,#21412,#21413,#21414,#21415,#21416,#21417));
#5015=EDGE_LOOP('',(#21418,#21419));
#5016=EDGE_LOOP('',(#21420,#21421,#21422,#21423));
#5017=EDGE_LOOP('',(#21424));
#5018=EDGE_LOOP('',(#21425,#21426,#21427,#21428,#21429,#21430));
#5019=EDGE_LOOP('',(#21431,#21432,#21433,#21434));
#5020=EDGE_LOOP('',(#21435));
#5021=EDGE_LOOP('',(#21436,#21437,#21438,#21439));
#5022=EDGE_LOOP('',(#21440,#21441,#21442,#21443,#21444,#21445,#21446));
#5023=EDGE_LOOP('',(#21447,#21448));
#5024=EDGE_LOOP('',(#21449,#21450,#21451,#21452,#21453));
#5025=EDGE_LOOP('',(#21454,#21455,#21456,#21457));
#5026=EDGE_LOOP('',(#21458));
#5027=EDGE_LOOP('',(#21459,#21460,#21461,#21462));
#5028=EDGE_LOOP('',(#21463,#21464,#21465,#21466));
#5029=EDGE_LOOP('',(#21467,#21468,#21469,#21470));
#5030=EDGE_LOOP('',(#21471,#21472,#21473,#21474));
#5031=EDGE_LOOP('',(#21475,#21476,#21477,#21478));
#5032=EDGE_LOOP('',(#21479,#21480,#21481,#21482));
#5033=EDGE_LOOP('',(#21483,#21484,#21485,#21486));
#5034=EDGE_LOOP('',(#21487,#21488,#21489,#21490));
#5035=EDGE_LOOP('',(#21491,#21492,#21493,#21494));
#5036=EDGE_LOOP('',(#21495,#21496,#21497,#21498));
#5037=EDGE_LOOP('',(#21499,#21500,#21501,#21502));
#5038=EDGE_LOOP('',(#21503,#21504,#21505,#21506));
#5039=EDGE_LOOP('',(#21507,#21508,#21509,#21510));
#5040=EDGE_LOOP('',(#21511,#21512,#21513,#21514));
#5041=EDGE_LOOP('',(#21515,#21516,#21517,#21518));
#5042=EDGE_LOOP('',(#21519,#21520,#21521,#21522));
#5043=EDGE_LOOP('',(#21523,#21524,#21525,#21526));
#5044=EDGE_LOOP('',(#21527,#21528,#21529,#21530));
#5045=EDGE_LOOP('',(#21531,#21532,#21533,#21534));
#5046=EDGE_LOOP('',(#21535,#21536,#21537,#21538));
#5047=EDGE_LOOP('',(#21539,#21540,#21541,#21542));
#5048=EDGE_LOOP('',(#21543,#21544,#21545,#21546));
#5049=EDGE_LOOP('',(#21547,#21548,#21549,#21550));
#5050=EDGE_LOOP('',(#21551,#21552,#21553,#21554));
#5051=EDGE_LOOP('',(#21555,#21556,#21557,#21558));
#5052=EDGE_LOOP('',(#21559,#21560,#21561,#21562));
#5053=EDGE_LOOP('',(#21563,#21564,#21565,#21566));
#5054=EDGE_LOOP('',(#21567,#21568,#21569,#21570));
#5055=EDGE_LOOP('',(#21571,#21572,#21573,#21574,#21575,#21576,#21577,#21578,
#21579,#21580,#21581,#21582,#21583,#21584,#21585,#21586,#21587,#21588,#21589,
#21590,#21591,#21592,#21593,#21594,#21595,#21596,#21597,#21598,#21599,#21600,
#21601,#21602));
#5056=EDGE_LOOP('',(#21603,#21604,#21605,#21606,#21607));
#5057=EDGE_LOOP('',(#21608,#21609,#21610,#21611));
#5058=EDGE_LOOP('',(#21612,#21613,#21614,#21615,#21616,#21617,#21618,#21619,
#21620,#21621,#21622,#21623,#21624,#21625,#21626,#21627,#21628,#21629,#21630,
#21631,#21632,#21633,#21634,#21635,#21636,#21637,#21638,#21639,#21640,#21641,
#21642,#21643));
#5059=EDGE_LOOP('',(#21644,#21645,#21646,#21647));
#5060=EDGE_LOOP('',(#21648));
#5061=EDGE_LOOP('',(#21649,#21650,#21651,#21652));
#5062=EDGE_LOOP('',(#21653,#21654,#21655,#21656));
#5063=EDGE_LOOP('',(#21657,#21658,#21659,#21660));
#5064=EDGE_LOOP('',(#21661,#21662,#21663,#21664));
#5065=EDGE_LOOP('',(#21665,#21666,#21667,#21668));
#5066=EDGE_LOOP('',(#21669,#21670,#21671,#21672));
#5067=EDGE_LOOP('',(#21673,#21674,#21675,#21676,#21677,#21678));
#5068=EDGE_LOOP('',(#21679));
#5069=EDGE_LOOP('',(#21680,#21681,#21682,#21683,#21684,#21685));
#5070=EDGE_LOOP('',(#21686,#21687,#21688,#21689,#21690,#21691));
#5071=EDGE_LOOP('',(#21692,#21693,#21694,#21695));
#5072=EDGE_LOOP('',(#21696,#21697,#21698,#21699));
#5073=EDGE_LOOP('',(#21700,#21701,#21702,#21703));
#5074=EDGE_LOOP('',(#21704));
#5075=EDGE_LOOP('',(#21705,#21706,#21707,#21708,#21709,#21710));
#5076=EDGE_LOOP('',(#21711,#21712,#21713,#21714));
#5077=EDGE_LOOP('',(#21715,#21716,#21717,#21718,#21719,#21720));
#5078=EDGE_LOOP('',(#21721,#21722,#21723,#21724,#21725,#21726));
#5079=EDGE_LOOP('',(#21727,#21728,#21729,#21730,#21731,#21732));
#5080=EDGE_LOOP('',(#21733,#21734,#21735,#21736,#21737,#21738));
#5081=EDGE_LOOP('',(#21739,#21740,#21741,#21742));
#5082=EDGE_LOOP('',(#21743,#21744,#21745,#21746,#21747,#21748));
#5083=EDGE_LOOP('',(#21749,#21750,#21751,#21752,#21753,#21754));
#5084=EDGE_LOOP('',(#21755,#21756,#21757,#21758));
#5085=EDGE_LOOP('',(#21759,#21760,#21761,#21762,#21763,#21764));
#5086=EDGE_LOOP('',(#21765,#21766,#21767,#21768,#21769,#21770));
#5087=EDGE_LOOP('',(#21771,#21772,#21773,#21774,#21775,#21776));
#5088=EDGE_LOOP('',(#21777,#21778,#21779,#21780,#21781,#21782));
#5089=EDGE_LOOP('',(#21783,#21784,#21785,#21786));
#5090=EDGE_LOOP('',(#21787,#21788,#21789,#21790,#21791,#21792));
#5091=EDGE_LOOP('',(#21793,#21794,#21795,#21796));
#5092=EDGE_LOOP('',(#21797,#21798,#21799,#21800));
#5093=EDGE_LOOP('',(#21801,#21802,#21803,#21804));
#5094=EDGE_LOOP('',(#21805,#21806,#21807,#21808));
#5095=EDGE_LOOP('',(#21809,#21810,#21811,#21812));
#5096=EDGE_LOOP('',(#21813,#21814,#21815,#21816));
#5097=EDGE_LOOP('',(#21817,#21818,#21819,#21820));
#5098=EDGE_LOOP('',(#21821,#21822,#21823,#21824));
#5099=EDGE_LOOP('',(#21825,#21826,#21827,#21828));
#5100=EDGE_LOOP('',(#21829,#21830,#21831,#21832));
#5101=EDGE_LOOP('',(#21833,#21834,#21835,#21836));
#5102=EDGE_LOOP('',(#21837,#21838,#21839,#21840));
#5103=EDGE_LOOP('',(#21841,#21842,#21843,#21844));
#5104=EDGE_LOOP('',(#21845,#21846,#21847,#21848));
#5105=EDGE_LOOP('',(#21849,#21850,#21851,#21852));
#5106=EDGE_LOOP('',(#21853,#21854,#21855,#21856));
#5107=EDGE_LOOP('',(#21857,#21858,#21859,#21860));
#5108=EDGE_LOOP('',(#21861,#21862,#21863,#21864));
#5109=EDGE_LOOP('',(#21865,#21866,#21867,#21868));
#5110=EDGE_LOOP('',(#21869,#21870,#21871,#21872));
#5111=EDGE_LOOP('',(#21873,#21874,#21875,#21876));
#5112=EDGE_LOOP('',(#21877,#21878,#21879,#21880));
#5113=EDGE_LOOP('',(#21881,#21882,#21883));
#5114=EDGE_LOOP('',(#21884,#21885,#21886,#21887,#21888));
#5115=EDGE_LOOP('',(#21889,#21890,#21891,#21892));
#5116=EDGE_LOOP('',(#21893,#21894,#21895,#21896));
#5117=EDGE_LOOP('',(#21897,#21898,#21899,#21900));
#5118=EDGE_LOOP('',(#21901,#21902,#21903,#21904));
#5119=EDGE_LOOP('',(#21905,#21906,#21907,#21908));
#5120=EDGE_LOOP('',(#21909,#21910,#21911,#21912));
#5121=EDGE_LOOP('',(#21913,#21914,#21915,#21916));
#5122=EDGE_LOOP('',(#21917,#21918,#21919,#21920));
#5123=EDGE_LOOP('',(#21921,#21922,#21923,#21924));
#5124=EDGE_LOOP('',(#21925,#21926,#21927,#21928));
#5125=EDGE_LOOP('',(#21929,#21930,#21931,#21932));
#5126=EDGE_LOOP('',(#21933,#21934,#21935,#21936));
#5127=EDGE_LOOP('',(#21937,#21938,#21939,#21940));
#5128=EDGE_LOOP('',(#21941,#21942,#21943,#21944));
#5129=EDGE_LOOP('',(#21945,#21946,#21947,#21948));
#5130=EDGE_LOOP('',(#21949,#21950,#21951,#21952));
#5131=EDGE_LOOP('',(#21953,#21954,#21955,#21956));
#5132=EDGE_LOOP('',(#21957,#21958,#21959,#21960));
#5133=EDGE_LOOP('',(#21961,#21962,#21963,#21964,#21965,#21966,#21967,#21968,
#21969,#21970,#21971,#21972,#21973,#21974,#21975,#21976,#21977,#21978,#21979,
#21980,#21981,#21982,#21983,#21984,#21985,#21986,#21987,#21988,#21989,#21990,
#21991,#21992,#21993,#21994,#21995,#21996,#21997,#21998,#21999,#22000,#22001,
#22002,#22003));
#5134=EDGE_LOOP('',(#22004,#22005,#22006,#22007,#22008));
#5135=EDGE_LOOP('',(#22009,#22010,#22011,#22012));
#5136=EDGE_LOOP('',(#22013,#22014,#22015,#22016,#22017,#22018,#22019,#22020,
#22021,#22022,#22023,#22024,#22025,#22026,#22027,#22028,#22029,#22030,#22031,
#22032,#22033,#22034,#22035,#22036,#22037,#22038,#22039,#22040,#22041,#22042,
#22043,#22044,#22045,#22046,#22047,#22048,#22049,#22050,#22051,#22052,#22053,
#22054,#22055,#22056));
#5137=EDGE_LOOP('',(#22057,#22058,#22059,#22060,#22061,#22062,#22063,#22064,
#22065,#22066));
#5138=EDGE_LOOP('',(#22067,#22068,#22069,#22070));
#5139=EDGE_LOOP('',(#22071,#22072,#22073,#22074));
#5140=EDGE_LOOP('',(#22075,#22076,#22077,#22078));
#5141=EDGE_LOOP('',(#22079,#22080,#22081,#22082,#22083,#22084));
#5142=EDGE_LOOP('',(#22085));
#5143=EDGE_LOOP('',(#22086,#22087,#22088,#22089));
#5144=EDGE_LOOP('',(#22090,#22091,#22092,#22093));
#5145=EDGE_LOOP('',(#22094,#22095,#22096,#22097,#22098));
#5146=EDGE_LOOP('',(#22099));
#5147=EDGE_LOOP('',(#22100));
#5148=EDGE_LOOP('',(#22101,#22102,#22103,#22104,#22105,#22106));
#5149=EDGE_LOOP('',(#22107,#22108,#22109,#22110));
#5150=EDGE_LOOP('',(#22111));
#5151=EDGE_LOOP('',(#22112,#22113,#22114,#22115,#22116));
#5152=EDGE_LOOP('',(#22117,#22118,#22119,#22120));
#5153=EDGE_LOOP('',(#22121,#22122,#22123,#22124));
#5154=EDGE_LOOP('',(#22125,#22126,#22127,#22128));
#5155=EDGE_LOOP('',(#22129,#22130,#22131,#22132,#22133,#22134,#22135,#22136));
#5156=EDGE_LOOP('',(#22137));
#5157=EDGE_LOOP('',(#22138,#22139,#22140,#22141));
#5158=EDGE_LOOP('',(#22142,#22143,#22144,#22145));
#5159=EDGE_LOOP('',(#22146,#22147,#22148,#22149));
#5160=EDGE_LOOP('',(#22150,#22151,#22152,#22153));
#5161=EDGE_LOOP('',(#22154,#22155,#22156,#22157));
#5162=EDGE_LOOP('',(#22158,#22159,#22160,#22161,#22162,#22163,#22164,#22165));
#5163=EDGE_LOOP('',(#22166));
#5164=EDGE_LOOP('',(#22167,#22168,#22169,#22170));
#5165=EDGE_LOOP('',(#22171,#22172,#22173,#22174));
#5166=EDGE_LOOP('',(#22175,#22176,#22177,#22178));
#5167=EDGE_LOOP('',(#22179,#22180,#22181,#22182));
#5168=EDGE_LOOP('',(#22183,#22184,#22185,#22186));
#5169=EDGE_LOOP('',(#22187,#22188,#22189,#22190));
#5170=EDGE_LOOP('',(#22191,#22192,#22193,#22194));
#5171=EDGE_LOOP('',(#22195,#22196,#22197,#22198));
#5172=EDGE_LOOP('',(#22199,#22200,#22201,#22202));
#5173=EDGE_LOOP('',(#22203,#22204,#22205,#22206));
#5174=EDGE_LOOP('',(#22207,#22208,#22209,#22210));
#5175=EDGE_LOOP('',(#22211,#22212,#22213,#22214));
#5176=EDGE_LOOP('',(#22215,#22216,#22217,#22218));
#5177=EDGE_LOOP('',(#22219,#22220,#22221,#22222));
#5178=EDGE_LOOP('',(#22223,#22224,#22225,#22226));
#5179=EDGE_LOOP('',(#22227,#22228,#22229,#22230));
#5180=EDGE_LOOP('',(#22231,#22232,#22233,#22234));
#5181=EDGE_LOOP('',(#22235,#22236,#22237,#22238));
#5182=EDGE_LOOP('',(#22239,#22240,#22241,#22242));
#5183=EDGE_LOOP('',(#22243,#22244,#22245,#22246));
#5184=EDGE_LOOP('',(#22247,#22248,#22249,#22250));
#5185=EDGE_LOOP('',(#22251,#22252,#22253,#22254));
#5186=EDGE_LOOP('',(#22255,#22256,#22257,#22258));
#5187=EDGE_LOOP('',(#22259,#22260,#22261,#22262));
#5188=EDGE_LOOP('',(#22263,#22264,#22265,#22266));
#5189=EDGE_LOOP('',(#22267,#22268,#22269,#22270));
#5190=EDGE_LOOP('',(#22271,#22272,#22273,#22274));
#5191=EDGE_LOOP('',(#22275,#22276,#22277,#22278));
#5192=EDGE_LOOP('',(#22279,#22280,#22281,#22282));
#5193=EDGE_LOOP('',(#22283,#22284,#22285,#22286));
#5194=EDGE_LOOP('',(#22287,#22288,#22289,#22290));
#5195=EDGE_LOOP('',(#22291,#22292,#22293,#22294));
#5196=EDGE_LOOP('',(#22295,#22296,#22297,#22298));
#5197=EDGE_LOOP('',(#22299,#22300,#22301,#22302));
#5198=EDGE_LOOP('',(#22303,#22304,#22305,#22306));
#5199=EDGE_LOOP('',(#22307,#22308,#22309,#22310));
#5200=EDGE_LOOP('',(#22311,#22312,#22313,#22314));
#5201=EDGE_LOOP('',(#22315,#22316,#22317,#22318));
#5202=EDGE_LOOP('',(#22319,#22320,#22321,#22322));
#5203=EDGE_LOOP('',(#22323,#22324,#22325,#22326));
#5204=EDGE_LOOP('',(#22327,#22328,#22329,#22330));
#5205=EDGE_LOOP('',(#22331,#22332,#22333,#22334));
#5206=EDGE_LOOP('',(#22335,#22336,#22337,#22338));
#5207=EDGE_LOOP('',(#22339,#22340,#22341,#22342));
#5208=EDGE_LOOP('',(#22343,#22344,#22345,#22346));
#5209=EDGE_LOOP('',(#22347,#22348,#22349,#22350));
#5210=EDGE_LOOP('',(#22351,#22352,#22353,#22354));
#5211=EDGE_LOOP('',(#22355,#22356,#22357,#22358));
#5212=EDGE_LOOP('',(#22359,#22360,#22361,#22362));
#5213=EDGE_LOOP('',(#22363,#22364,#22365,#22366));
#5214=EDGE_LOOP('',(#22367,#22368,#22369,#22370));
#5215=EDGE_LOOP('',(#22371,#22372,#22373,#22374));
#5216=EDGE_LOOP('',(#22375));
#5217=EDGE_LOOP('',(#22376));
#5218=EDGE_LOOP('',(#22377,#22378,#22379,#22380));
#5219=EDGE_LOOP('',(#22381,#22382,#22383,#22384));
#5220=EDGE_LOOP('',(#22385));
#5221=EDGE_LOOP('',(#22386));
#5222=EDGE_LOOP('',(#22387,#22388,#22389,#22390));
#5223=EDGE_LOOP('',(#22391));
#5224=EDGE_LOOP('',(#22392));
#5225=EDGE_LOOP('',(#22393,#22394,#22395,#22396));
#5226=EDGE_LOOP('',(#22397,#22398,#22399,#22400));
#5227=EDGE_LOOP('',(#22401));
#5228=EDGE_LOOP('',(#22402));
#5229=EDGE_LOOP('',(#22403,#22404,#22405,#22406));
#5230=EDGE_LOOP('',(#22407));
#5231=EDGE_LOOP('',(#22408));
#5232=EDGE_LOOP('',(#22409,#22410,#22411,#22412));
#5233=EDGE_LOOP('',(#22413));
#5234=EDGE_LOOP('',(#22414));
#5235=EDGE_LOOP('',(#22415,#22416,#22417,#22418));
#5236=EDGE_LOOP('',(#22419,#22420,#22421,#22422));
#5237=EDGE_LOOP('',(#22423,#22424,#22425,#22426));
#5238=EDGE_LOOP('',(#22427,#22428,#22429,#22430));
#5239=EDGE_LOOP('',(#22431,#22432,#22433,#22434));
#5240=EDGE_LOOP('',(#22435,#22436,#22437,#22438));
#5241=EDGE_LOOP('',(#22439,#22440,#22441,#22442));
#5242=EDGE_LOOP('',(#22443,#22444,#22445,#22446));
#5243=EDGE_LOOP('',(#22447,#22448,#22449,#22450));
#5244=EDGE_LOOP('',(#22451,#22452,#22453,#22454));
#5245=EDGE_LOOP('',(#22455,#22456,#22457,#22458));
#5246=EDGE_LOOP('',(#22459,#22460,#22461,#22462));
#5247=EDGE_LOOP('',(#22463,#22464,#22465,#22466));
#5248=EDGE_LOOP('',(#22467,#22468,#22469,#22470));
#5249=EDGE_LOOP('',(#22471,#22472,#22473,#22474));
#5250=EDGE_LOOP('',(#22475,#22476,#22477,#22478));
#5251=EDGE_LOOP('',(#22479,#22480,#22481,#22482));
#5252=EDGE_LOOP('',(#22483,#22484,#22485,#22486));
#5253=EDGE_LOOP('',(#22487,#22488,#22489,#22490));
#5254=EDGE_LOOP('',(#22491,#22492,#22493,#22494));
#5255=EDGE_LOOP('',(#22495,#22496,#22497,#22498));
#5256=EDGE_LOOP('',(#22499,#22500,#22501,#22502));
#5257=EDGE_LOOP('',(#22503,#22504,#22505,#22506));
#5258=EDGE_LOOP('',(#22507,#22508,#22509,#22510));
#5259=EDGE_LOOP('',(#22511,#22512,#22513,#22514));
#5260=EDGE_LOOP('',(#22515,#22516,#22517,#22518));
#5261=EDGE_LOOP('',(#22519,#22520,#22521,#22522));
#5262=EDGE_LOOP('',(#22523,#22524,#22525,#22526));
#5263=EDGE_LOOP('',(#22527,#22528,#22529,#22530));
#5264=EDGE_LOOP('',(#22531,#22532,#22533,#22534));
#5265=EDGE_LOOP('',(#22535,#22536,#22537,#22538));
#5266=EDGE_LOOP('',(#22539,#22540,#22541,#22542));
#5267=EDGE_LOOP('',(#22543,#22544,#22545,#22546));
#5268=EDGE_LOOP('',(#22547,#22548,#22549,#22550));
#5269=EDGE_LOOP('',(#22551,#22552,#22553,#22554));
#5270=EDGE_LOOP('',(#22555,#22556,#22557,#22558));
#5271=EDGE_LOOP('',(#22559,#22560,#22561,#22562));
#5272=EDGE_LOOP('',(#22563,#22564,#22565,#22566));
#5273=EDGE_LOOP('',(#22567,#22568,#22569,#22570));
#5274=EDGE_LOOP('',(#22571,#22572,#22573,#22574));
#5275=EDGE_LOOP('',(#22575,#22576,#22577,#22578));
#5276=EDGE_LOOP('',(#22579,#22580,#22581,#22582));
#5277=EDGE_LOOP('',(#22583,#22584,#22585,#22586));
#5278=EDGE_LOOP('',(#22587,#22588,#22589,#22590));
#5279=EDGE_LOOP('',(#22591,#22592,#22593,#22594));
#5280=EDGE_LOOP('',(#22595,#22596,#22597,#22598,#22599,#22600,#22601,#22602,
#22603,#22604,#22605,#22606,#22607,#22608,#22609,#22610,#22611,#22612,#22613,
#22614,#22615,#22616,#22617,#22618,#22619,#22620,#22621,#22622,#22623,#22624,
#22625,#22626,#22627,#22628,#22629,#22630,#22631,#22632,#22633,#22634,#22635,
#22636,#22637,#22638,#22639,#22640,#22641,#22642,#22643));
#5281=EDGE_LOOP('',(#22644,#22645,#22646,#22647,#22648));
#5282=EDGE_LOOP('',(#22649,#22650,#22651,#22652));
#5283=EDGE_LOOP('',(#22653,#22654,#22655,#22656,#22657,#22658,#22659,#22660,
#22661,#22662,#22663,#22664,#22665,#22666,#22667,#22668,#22669,#22670,#22671,
#22672,#22673,#22674,#22675,#22676,#22677,#22678,#22679,#22680,#22681,#22682,
#22683,#22684,#22685,#22686,#22687,#22688,#22689,#22690,#22691,#22692,#22693,
#22694,#22695,#22696,#22697,#22698,#22699,#22700,#22701));
#5284=EDGE_LOOP('',(#22702,#22703,#22704,#22705,#22706,#22707,#22708,#22709,
#22710,#22711));
#5285=EDGE_LOOP('',(#22712,#22713,#22714,#22715));
#5286=EDGE_LOOP('',(#22716,#22717,#22718,#22719));
#5287=EDGE_LOOP('',(#22720,#22721,#22722,#22723));
#5288=EDGE_LOOP('',(#22724,#22725,#22726,#22727,#22728,#22729));
#5289=EDGE_LOOP('',(#22730));
#5290=EDGE_LOOP('',(#22731,#22732,#22733,#22734));
#5291=EDGE_LOOP('',(#22735,#22736,#22737,#22738));
#5292=EDGE_LOOP('',(#22739,#22740,#22741,#22742,#22743));
#5293=EDGE_LOOP('',(#22744));
#5294=EDGE_LOOP('',(#22745));
#5295=EDGE_LOOP('',(#22746,#22747,#22748,#22749,#22750,#22751));
#5296=EDGE_LOOP('',(#22752,#22753,#22754,#22755));
#5297=EDGE_LOOP('',(#22756));
#5298=EDGE_LOOP('',(#22757,#22758,#22759,#22760));
#5299=EDGE_LOOP('',(#22761,#22762,#22763,#22764));
#5300=EDGE_LOOP('',(#22765,#22766,#22767,#22768));
#5301=EDGE_LOOP('',(#22769,#22770,#22771,#22772));
#5302=EDGE_LOOP('',(#22773,#22774,#22775,#22776));
#5303=EDGE_LOOP('',(#22777,#22778,#22779,#22780));
#5304=EDGE_LOOP('',(#22781,#22782,#22783,#22784));
#5305=EDGE_LOOP('',(#22785,#22786,#22787,#22788));
#5306=EDGE_LOOP('',(#22789,#22790,#22791,#22792));
#5307=EDGE_LOOP('',(#22793,#22794,#22795,#22796));
#5308=EDGE_LOOP('',(#22797,#22798,#22799,#22800));
#5309=EDGE_LOOP('',(#22801,#22802,#22803,#22804));
#5310=EDGE_LOOP('',(#22805,#22806,#22807,#22808));
#5311=EDGE_LOOP('',(#22809,#22810,#22811,#22812));
#5312=EDGE_LOOP('',(#22813,#22814,#22815,#22816));
#5313=EDGE_LOOP('',(#22817,#22818,#22819,#22820));
#5314=EDGE_LOOP('',(#22821,#22822,#22823,#22824));
#5315=EDGE_LOOP('',(#22825,#22826,#22827,#22828));
#5316=EDGE_LOOP('',(#22829,#22830,#22831,#22832));
#5317=EDGE_LOOP('',(#22833,#22834,#22835,#22836));
#5318=EDGE_LOOP('',(#22837,#22838,#22839,#22840));
#5319=EDGE_LOOP('',(#22841,#22842,#22843,#22844));
#5320=EDGE_LOOP('',(#22845,#22846,#22847,#22848));
#5321=EDGE_LOOP('',(#22849,#22850,#22851,#22852));
#5322=EDGE_LOOP('',(#22853,#22854,#22855,#22856));
#5323=EDGE_LOOP('',(#22857,#22858,#22859,#22860));
#5324=EDGE_LOOP('',(#22861,#22862,#22863,#22864));
#5325=EDGE_LOOP('',(#22865,#22866,#22867,#22868));
#5326=EDGE_LOOP('',(#22869,#22870,#22871,#22872));
#5327=EDGE_LOOP('',(#22873,#22874,#22875,#22876));
#5328=EDGE_LOOP('',(#22877,#22878,#22879,#22880));
#5329=EDGE_LOOP('',(#22881,#22882,#22883,#22884));
#5330=EDGE_LOOP('',(#22885,#22886,#22887,#22888));
#5331=EDGE_LOOP('',(#22889,#22890,#22891,#22892));
#5332=EDGE_LOOP('',(#22893,#22894,#22895,#22896));
#5333=EDGE_LOOP('',(#22897,#22898,#22899,#22900));
#5334=EDGE_LOOP('',(#22901,#22902,#22903,#22904));
#5335=EDGE_LOOP('',(#22905,#22906,#22907,#22908));
#5336=EDGE_LOOP('',(#22909,#22910,#22911,#22912));
#5337=EDGE_LOOP('',(#22913,#22914,#22915,#22916));
#5338=EDGE_LOOP('',(#22917,#22918,#22919,#22920));
#5339=EDGE_LOOP('',(#22921,#22922,#22923,#22924));
#5340=EDGE_LOOP('',(#22925,#22926,#22927,#22928));
#5341=EDGE_LOOP('',(#22929,#22930,#22931,#22932));
#5342=EDGE_LOOP('',(#22933,#22934,#22935,#22936));
#5343=EDGE_LOOP('',(#22937,#22938,#22939,#22940));
#5344=EDGE_LOOP('',(#22941,#22942,#22943,#22944));
#5345=EDGE_LOOP('',(#22945,#22946,#22947,#22948));
#5346=EDGE_LOOP('',(#22949,#22950,#22951,#22952,#22953));
#5347=EDGE_LOOP('',(#22954,#22955,#22956,#22957,#22958,#22959,#22960,#22961,
#22962,#22963,#22964,#22965,#22966,#22967,#22968,#22969,#22970,#22971,#22972,
#22973,#22974,#22975,#22976,#22977,#22978,#22979,#22980,#22981,#22982,#22983,
#22984,#22985,#22986,#22987,#22988,#22989,#22990,#22991,#22992,#22993,#22994,
#22995,#22996,#22997,#22998,#22999,#23000,#23001,#23002,#23003));
#5348=EDGE_LOOP('',(#23004,#23005,#23006,#23007,#23008));
#5349=EDGE_LOOP('',(#23009,#23010,#23011,#23012));
#5350=EDGE_LOOP('',(#23013,#23014,#23015,#23016,#23017,#23018,#23019,#23020,
#23021,#23022,#23023,#23024,#23025,#23026,#23027,#23028,#23029,#23030,#23031,
#23032,#23033,#23034,#23035,#23036,#23037,#23038,#23039,#23040,#23041,#23042,
#23043,#23044,#23045,#23046,#23047,#23048,#23049,#23050,#23051,#23052,#23053,
#23054,#23055,#23056,#23057,#23058,#23059,#23060,#23061,#23062));
#5351=EDGE_LOOP('',(#23063,#23064,#23065,#23066,#23067,#23068));
#5352=EDGE_LOOP('',(#23069,#23070,#23071,#23072));
#5353=EDGE_LOOP('',(#23073));
#5354=EDGE_LOOP('',(#23074));
#5355=EDGE_LOOP('',(#23075,#23076));
#5356=EDGE_LOOP('',(#23077,#23078));
#5357=EDGE_LOOP('',(#23079,#23080));
#5358=EDGE_LOOP('',(#23081,#23082));
#5359=EDGE_LOOP('',(#23083,#23084));
#5360=EDGE_LOOP('',(#23085,#23086));
#5361=EDGE_LOOP('',(#23087,#23088,#23089,#23090,#23091,#23092,#23093,#23094));
#5362=EDGE_LOOP('',(#23095,#23096,#23097,#23098));
#5363=EDGE_LOOP('',(#23099,#23100,#23101,#23102));
#5364=EDGE_LOOP('',(#23103,#23104,#23105,#23106));
#5365=EDGE_LOOP('',(#23107,#23108,#23109,#23110));
#5366=EDGE_LOOP('',(#23111,#23112,#23113,#23114));
#5367=EDGE_LOOP('',(#23115,#23116,#23117,#23118));
#5368=EDGE_LOOP('',(#23119,#23120,#23121,#23122));
#5369=EDGE_LOOP('',(#23123,#23124,#23125));
#5370=EDGE_LOOP('',(#23126,#23127,#23128,#23129));
#5371=EDGE_LOOP('',(#23130,#23131,#23132));
#5372=EDGE_LOOP('',(#23133,#23134,#23135,#23136));
#5373=EDGE_LOOP('',(#23137,#23138,#23139));
#5374=EDGE_LOOP('',(#23140,#23141,#23142,#23143));
#5375=EDGE_LOOP('',(#23144,#23145,#23146));
#5376=EDGE_LOOP('',(#23147,#23148,#23149,#23150));
#5377=EDGE_LOOP('',(#23151,#23152,#23153));
#5378=EDGE_LOOP('',(#23154,#23155,#23156,#23157));
#5379=EDGE_LOOP('',(#23158,#23159,#23160));
#5380=EDGE_LOOP('',(#23161,#23162,#23163,#23164));
#5381=EDGE_LOOP('',(#23165,#23166,#23167));
#5382=EDGE_LOOP('',(#23168,#23169,#23170,#23171));
#5383=EDGE_LOOP('',(#23172,#23173,#23174));
#5384=EDGE_LOOP('',(#23175,#23176,#23177,#23178));
#5385=EDGE_LOOP('',(#23179,#23180,#23181));
#5386=EDGE_LOOP('',(#23182,#23183,#23184,#23185));
#5387=EDGE_LOOP('',(#23186,#23187,#23188));
#5388=EDGE_LOOP('',(#23189,#23190,#23191,#23192));
#5389=EDGE_LOOP('',(#23193,#23194,#23195));
#5390=EDGE_LOOP('',(#23196,#23197,#23198,#23199));
#5391=EDGE_LOOP('',(#23200,#23201,#23202));
#5392=EDGE_LOOP('',(#23203,#23204,#23205,#23206));
#5393=EDGE_LOOP('',(#23207,#23208,#23209));
#5394=EDGE_LOOP('',(#23210,#23211,#23212,#23213));
#5395=EDGE_LOOP('',(#23214,#23215,#23216));
#5396=EDGE_LOOP('',(#23217,#23218,#23219,#23220));
#5397=EDGE_LOOP('',(#23221,#23222,#23223));
#5398=EDGE_LOOP('',(#23224,#23225,#23226,#23227));
#5399=EDGE_LOOP('',(#23228,#23229,#23230));
#5400=EDGE_LOOP('',(#23231,#23232,#23233,#23234));
#5401=EDGE_LOOP('',(#23235,#23236,#23237,#23238));
#5402=EDGE_LOOP('',(#23239,#23240,#23241,#23242));
#5403=EDGE_LOOP('',(#23243,#23244,#23245,#23246));
#5404=EDGE_LOOP('',(#23247,#23248,#23249,#23250));
#5405=EDGE_LOOP('',(#23251,#23252,#23253));
#5406=EDGE_LOOP('',(#23254,#23255,#23256,#23257));
#5407=EDGE_LOOP('',(#23258,#23259,#23260));
#5408=EDGE_LOOP('',(#23261,#23262,#23263,#23264));
#5409=EDGE_LOOP('',(#23265,#23266,#23267));
#5410=EDGE_LOOP('',(#23268,#23269,#23270,#23271));
#5411=EDGE_LOOP('',(#23272,#23273,#23274));
#5412=EDGE_LOOP('',(#23275,#23276,#23277,#23278));
#5413=EDGE_LOOP('',(#23279,#23280,#23281));
#5414=EDGE_LOOP('',(#23282,#23283,#23284,#23285));
#5415=EDGE_LOOP('',(#23286,#23287,#23288));
#5416=EDGE_LOOP('',(#23289,#23290,#23291,#23292));
#5417=EDGE_LOOP('',(#23293,#23294,#23295));
#5418=EDGE_LOOP('',(#23296,#23297,#23298,#23299));
#5419=EDGE_LOOP('',(#23300,#23301,#23302));
#5420=EDGE_LOOP('',(#23303,#23304,#23305,#23306));
#5421=EDGE_LOOP('',(#23307,#23308,#23309));
#5422=EDGE_LOOP('',(#23310,#23311,#23312,#23313));
#5423=EDGE_LOOP('',(#23314,#23315,#23316));
#5424=EDGE_LOOP('',(#23317,#23318,#23319,#23320));
#5425=EDGE_LOOP('',(#23321,#23322,#23323));
#5426=EDGE_LOOP('',(#23324,#23325,#23326,#23327));
#5427=EDGE_LOOP('',(#23328,#23329,#23330));
#5428=EDGE_LOOP('',(#23331,#23332,#23333,#23334));
#5429=EDGE_LOOP('',(#23335,#23336,#23337));
#5430=EDGE_LOOP('',(#23338,#23339,#23340,#23341));
#5431=EDGE_LOOP('',(#23342,#23343,#23344));
#5432=EDGE_LOOP('',(#23345,#23346,#23347,#23348));
#5433=EDGE_LOOP('',(#23349,#23350,#23351));
#5434=EDGE_LOOP('',(#23352,#23353,#23354,#23355));
#5435=EDGE_LOOP('',(#23356,#23357,#23358));
#5436=EDGE_LOOP('',(#23359,#23360,#23361,#23362));
#5437=EDGE_LOOP('',(#23363,#23364,#23365));
#5438=EDGE_LOOP('',(#23366,#23367,#23368,#23369));
#5439=EDGE_LOOP('',(#23370,#23371,#23372));
#5440=EDGE_LOOP('',(#23373,#23374,#23375,#23376));
#5441=EDGE_LOOP('',(#23377,#23378,#23379));
#5442=EDGE_LOOP('',(#23380,#23381,#23382,#23383));
#5443=EDGE_LOOP('',(#23384,#23385,#23386));
#5444=EDGE_LOOP('',(#23387,#23388,#23389,#23390));
#5445=EDGE_LOOP('',(#23391,#23392,#23393));
#5446=EDGE_LOOP('',(#23394,#23395,#23396,#23397));
#5447=EDGE_LOOP('',(#23398,#23399,#23400));
#5448=EDGE_LOOP('',(#23401,#23402,#23403,#23404));
#5449=EDGE_LOOP('',(#23405,#23406,#23407));
#5450=EDGE_LOOP('',(#23408,#23409,#23410,#23411));
#5451=EDGE_LOOP('',(#23412,#23413,#23414));
#5452=EDGE_LOOP('',(#23415,#23416,#23417,#23418));
#5453=EDGE_LOOP('',(#23419,#23420,#23421));
#5454=EDGE_LOOP('',(#23422,#23423,#23424,#23425));
#5455=EDGE_LOOP('',(#23426,#23427,#23428));
#5456=EDGE_LOOP('',(#23429,#23430,#23431,#23432));
#5457=EDGE_LOOP('',(#23433,#23434,#23435));
#5458=EDGE_LOOP('',(#23436,#23437,#23438,#23439));
#5459=EDGE_LOOP('',(#23440,#23441,#23442));
#5460=EDGE_LOOP('',(#23443,#23444,#23445,#23446));
#5461=EDGE_LOOP('',(#23447,#23448,#23449));
#5462=EDGE_LOOP('',(#23450,#23451,#23452,#23453));
#5463=EDGE_LOOP('',(#23454,#23455,#23456));
#5464=EDGE_LOOP('',(#23457,#23458,#23459,#23460));
#5465=EDGE_LOOP('',(#23461,#23462,#23463));
#5466=EDGE_LOOP('',(#23464,#23465,#23466,#23467));
#5467=EDGE_LOOP('',(#23468,#23469,#23470));
#5468=EDGE_LOOP('',(#23471,#23472,#23473,#23474));
#5469=EDGE_LOOP('',(#23475,#23476,#23477));
#5470=EDGE_LOOP('',(#23478,#23479,#23480,#23481));
#5471=EDGE_LOOP('',(#23482,#23483,#23484));
#5472=EDGE_LOOP('',(#23485,#23486,#23487));
#5473=EDGE_LOOP('',(#23488,#23489,#23490,#23491));
#5474=EDGE_LOOP('',(#23492,#23493,#23494,#23495));
#5475=EDGE_LOOP('',(#23496,#23497,#23498));
#5476=EDGE_LOOP('',(#23499,#23500,#23501,#23502));
#5477=EDGE_LOOP('',(#23503,#23504,#23505));
#5478=EDGE_LOOP('',(#23506,#23507,#23508,#23509));
#5479=EDGE_LOOP('',(#23510,#23511,#23512));
#5480=EDGE_LOOP('',(#23513,#23514,#23515,#23516));
#5481=EDGE_LOOP('',(#23517,#23518,#23519));
#5482=EDGE_LOOP('',(#23520,#23521,#23522,#23523));
#5483=EDGE_LOOP('',(#23524,#23525,#23526));
#5484=EDGE_LOOP('',(#23527,#23528,#23529,#23530));
#5485=EDGE_LOOP('',(#23531,#23532,#23533));
#5486=EDGE_LOOP('',(#23534,#23535,#23536,#23537));
#5487=EDGE_LOOP('',(#23538,#23539,#23540));
#5488=EDGE_LOOP('',(#23541,#23542,#23543,#23544));
#5489=EDGE_LOOP('',(#23545,#23546,#23547));
#5490=EDGE_LOOP('',(#23548,#23549,#23550,#23551));
#5491=EDGE_LOOP('',(#23552,#23553,#23554));
#5492=EDGE_LOOP('',(#23555,#23556,#23557,#23558));
#5493=EDGE_LOOP('',(#23559,#23560,#23561));
#5494=EDGE_LOOP('',(#23562,#23563,#23564,#23565));
#5495=EDGE_LOOP('',(#23566,#23567,#23568));
#5496=EDGE_LOOP('',(#23569,#23570,#23571,#23572));
#5497=EDGE_LOOP('',(#23573,#23574,#23575));
#5498=EDGE_LOOP('',(#23576,#23577,#23578,#23579));
#5499=EDGE_LOOP('',(#23580,#23581,#23582));
#5500=EDGE_LOOP('',(#23583,#23584,#23585,#23586));
#5501=EDGE_LOOP('',(#23587,#23588,#23589));
#5502=EDGE_LOOP('',(#23590,#23591,#23592,#23593));
#5503=EDGE_LOOP('',(#23594,#23595,#23596));
#5504=EDGE_LOOP('',(#23597,#23598,#23599,#23600));
#5505=EDGE_LOOP('',(#23601,#23602,#23603));
#5506=EDGE_LOOP('',(#23604,#23605,#23606,#23607));
#5507=EDGE_LOOP('',(#23608,#23609,#23610));
#5508=EDGE_LOOP('',(#23611,#23612,#23613,#23614));
#5509=EDGE_LOOP('',(#23615,#23616,#23617));
#5510=EDGE_LOOP('',(#23618,#23619,#23620,#23621));
#5511=EDGE_LOOP('',(#23622,#23623,#23624));
#5512=EDGE_LOOP('',(#23625));
#5513=EDGE_LOOP('',(#23626,#23627,#23628,#23629,#23630,#23631));
#5514=EDGE_LOOP('',(#23632,#23633,#23634,#23635));
#5515=EDGE_LOOP('',(#23636,#23637,#23638,#23639,#23640,#23641,#23642,#23643,
#23644,#23645,#23646,#23647,#23648,#23649,#23650,#23651,#23652,#23653,#23654,
#23655,#23656,#23657,#23658,#23659,#23660,#23661,#23662,#23663,#23664,#23665,
#23666,#23667,#23668,#23669,#23670,#23671,#23672,#23673,#23674,#23675,#23676,
#23677,#23678,#23679,#23680,#23681,#23682,#23683,#23684,#23685,#23686,#23687,
#23688,#23689,#23690,#23691,#23692,#23693,#23694,#23695,#23696,#23697,#23698,
#23699,#23700,#23701,#23702,#23703,#23704,#23705,#23706,#23707,#23708,#23709,
#23710,#23711,#23712,#23713,#23714,#23715,#23716,#23717,#23718,#23719,#23720,
#23721,#23722,#23723,#23724,#23725,#23726,#23727,#23728,#23729,#23730,#23731,
#23732,#23733,#23734,#23735,#23736,#23737,#23738,#23739,#23740,#23741,#23742,
#23743,#23744,#23745,#23746,#23747,#23748,#23749,#23750,#23751,#23752,#23753,
#23754,#23755,#23756,#23757,#23758,#23759,#23760,#23761,#23762,#23763,#23764,
#23765,#23766,#23767,#23768,#23769,#23770,#23771,#23772,#23773,#23774,#23775,
#23776,#23777,#23778,#23779,#23780,#23781,#23782,#23783));
#5516=EDGE_LOOP('',(#23784,#23785,#23786,#23787,#23788,#23789,#23790,#23791,
#23792,#23793,#23794,#23795,#23796,#23797,#23798,#23799,#23800,#23801,#23802,
#23803,#23804,#23805,#23806,#23807,#23808,#23809,#23810,#23811,#23812,#23813,
#23814,#23815,#23816,#23817,#23818,#23819,#23820,#23821,#23822,#23823,#23824,
#23825,#23826,#23827,#23828,#23829,#23830,#23831,#23832,#23833,#23834,#23835,
#23836,#23837,#23838,#23839,#23840,#23841,#23842,#23843,#23844,#23845,#23846,
#23847,#23848,#23849,#23850,#23851,#23852,#23853,#23854,#23855,#23856,#23857,
#23858,#23859));
#5517=EDGE_LOOP('',(#23860));
#5518=EDGE_LOOP('',(#23861,#23862,#23863,#23864,#23865,#23866));
#5519=EDGE_LOOP('',(#23867,#23868,#23869,#23870));
#5520=EDGE_LOOP('',(#23871,#23872,#23873,#23874));
#5521=EDGE_LOOP('',(#23875,#23876,#23877,#23878));
#5522=EDGE_LOOP('',(#23879,#23880,#23881,#23882));
#5523=EDGE_LOOP('',(#23883,#23884,#23885,#23886));
#5524=EDGE_LOOP('',(#23887,#23888,#23889,#23890));
#5525=EDGE_LOOP('',(#23891,#23892,#23893,#23894));
#5526=EDGE_LOOP('',(#23895,#23896,#23897,#23898));
#5527=EDGE_LOOP('',(#23899,#23900,#23901,#23902));
#5528=EDGE_LOOP('',(#23903,#23904,#23905,#23906));
#5529=EDGE_LOOP('',(#23907,#23908,#23909,#23910));
#5530=EDGE_LOOP('',(#23911,#23912,#23913,#23914));
#5531=EDGE_LOOP('',(#23915,#23916,#23917,#23918));
#5532=EDGE_LOOP('',(#23919,#23920,#23921,#23922));
#5533=EDGE_LOOP('',(#23923,#23924,#23925,#23926));
#5534=EDGE_LOOP('',(#23927,#23928,#23929,#23930));
#5535=EDGE_LOOP('',(#23931,#23932,#23933,#23934));
#5536=EDGE_LOOP('',(#23935,#23936,#23937,#23938));
#5537=EDGE_LOOP('',(#23939,#23940,#23941,#23942));
#5538=EDGE_LOOP('',(#23943,#23944,#23945,#23946,#23947));
#5539=EDGE_LOOP('',(#23948,#23949,#23950,#23951));
#5540=EDGE_LOOP('',(#23952,#23953,#23954,#23955));
#5541=EDGE_LOOP('',(#23956,#23957,#23958,#23959));
#5542=EDGE_LOOP('',(#23960,#23961,#23962,#23963));
#5543=EDGE_LOOP('',(#23964,#23965,#23966,#23967));
#5544=EDGE_LOOP('',(#23968,#23969,#23970,#23971));
#5545=EDGE_LOOP('',(#23972,#23973,#23974,#23975));
#5546=EDGE_LOOP('',(#23976,#23977,#23978,#23979));
#5547=EDGE_LOOP('',(#23980,#23981,#23982,#23983));
#5548=EDGE_LOOP('',(#23984,#23985,#23986,#23987));
#5549=EDGE_LOOP('',(#23988,#23989,#23990,#23991));
#5550=EDGE_LOOP('',(#23992,#23993,#23994,#23995));
#5551=EDGE_LOOP('',(#23996,#23997,#23998,#23999));
#5552=EDGE_LOOP('',(#24000,#24001,#24002,#24003));
#5553=EDGE_LOOP('',(#24004,#24005,#24006,#24007));
#5554=EDGE_LOOP('',(#24008,#24009,#24010,#24011));
#5555=EDGE_LOOP('',(#24012,#24013,#24014,#24015));
#5556=EDGE_LOOP('',(#24016,#24017,#24018,#24019));
#5557=EDGE_LOOP('',(#24020,#24021,#24022,#24023));
#5558=EDGE_LOOP('',(#24024,#24025,#24026,#24027));
#5559=EDGE_LOOP('',(#24028,#24029,#24030,#24031,#24032,#24033,#24034,#24035,
#24036,#24037,#24038,#24039,#24040,#24041,#24042,#24043,#24044,#24045,#24046,
#24047,#24048,#24049,#24050,#24051,#24052,#24053,#24054,#24055,#24056,#24057,
#24058,#24059,#24060,#24061,#24062,#24063,#24064,#24065,#24066,#24067,#24068,
#24069,#24070));
#5560=EDGE_LOOP('',(#24071,#24072,#24073,#24074,#24075));
#5561=EDGE_LOOP('',(#24076,#24077,#24078,#24079));
#5562=EDGE_LOOP('',(#24080,#24081,#24082,#24083,#24084,#24085,#24086,#24087,
#24088,#24089,#24090,#24091,#24092,#24093,#24094,#24095,#24096,#24097,#24098,
#24099,#24100,#24101,#24102,#24103,#24104,#24105,#24106,#24107,#24108,#24109,
#24110,#24111,#24112,#24113,#24114,#24115,#24116,#24117,#24118,#24119,#24120,
#24121));
#5563=EDGE_LOOP('',(#24122,#24123,#24124,#24125,#24126,#24127));
#5564=EDGE_LOOP('',(#24128,#24129,#24130));
#5565=EDGE_LOOP('',(#24131));
#5566=EDGE_LOOP('',(#24132));
#5567=EDGE_LOOP('',(#24133,#24134));
#5568=EDGE_LOOP('',(#24135,#24136));
#5569=EDGE_LOOP('',(#24137,#24138));
#5570=EDGE_LOOP('',(#24139,#24140));
#5571=EDGE_LOOP('',(#24141,#24142));
#5572=EDGE_LOOP('',(#24143,#24144));
#5573=EDGE_LOOP('',(#24145,#24146,#24147,#24148,#24149,#24150,#24151,#24152));
#5574=EDGE_LOOP('',(#24153,#24154,#24155,#24156));
#5575=EDGE_LOOP('',(#24157,#24158,#24159,#24160));
#5576=EDGE_LOOP('',(#24161,#24162,#24163,#24164));
#5577=EDGE_LOOP('',(#24165,#24166,#24167,#24168));
#5578=EDGE_LOOP('',(#24169,#24170,#24171,#24172));
#5579=EDGE_LOOP('',(#24173,#24174,#24175,#24176));
#5580=EDGE_LOOP('',(#24177,#24178,#24179,#24180));
#5581=EDGE_LOOP('',(#24181,#24182,#24183));
#5582=EDGE_LOOP('',(#24184,#24185,#24186,#24187));
#5583=EDGE_LOOP('',(#24188,#24189,#24190));
#5584=EDGE_LOOP('',(#24191,#24192,#24193,#24194));
#5585=EDGE_LOOP('',(#24195,#24196,#24197));
#5586=EDGE_LOOP('',(#24198,#24199,#24200,#24201));
#5587=EDGE_LOOP('',(#24202,#24203,#24204));
#5588=EDGE_LOOP('',(#24205,#24206,#24207,#24208));
#5589=EDGE_LOOP('',(#24209,#24210,#24211));
#5590=EDGE_LOOP('',(#24212,#24213,#24214,#24215));
#5591=EDGE_LOOP('',(#24216,#24217,#24218));
#5592=EDGE_LOOP('',(#24219,#24220,#24221,#24222));
#5593=EDGE_LOOP('',(#24223,#24224,#24225));
#5594=EDGE_LOOP('',(#24226,#24227,#24228,#24229));
#5595=EDGE_LOOP('',(#24230,#24231,#24232));
#5596=EDGE_LOOP('',(#24233,#24234,#24235,#24236));
#5597=EDGE_LOOP('',(#24237,#24238,#24239));
#5598=EDGE_LOOP('',(#24240,#24241,#24242,#24243));
#5599=EDGE_LOOP('',(#24244,#24245,#24246));
#5600=EDGE_LOOP('',(#24247,#24248,#24249,#24250));
#5601=EDGE_LOOP('',(#24251,#24252,#24253));
#5602=EDGE_LOOP('',(#24254,#24255,#24256,#24257));
#5603=EDGE_LOOP('',(#24258,#24259,#24260));
#5604=EDGE_LOOP('',(#24261,#24262,#24263,#24264));
#5605=EDGE_LOOP('',(#24265,#24266,#24267));
#5606=EDGE_LOOP('',(#24268,#24269,#24270,#24271));
#5607=EDGE_LOOP('',(#24272,#24273,#24274));
#5608=EDGE_LOOP('',(#24275,#24276,#24277,#24278));
#5609=EDGE_LOOP('',(#24279,#24280,#24281));
#5610=EDGE_LOOP('',(#24282,#24283,#24284,#24285));
#5611=EDGE_LOOP('',(#24286,#24287,#24288));
#5612=EDGE_LOOP('',(#24289,#24290,#24291,#24292));
#5613=EDGE_LOOP('',(#24293,#24294,#24295,#24296));
#5614=EDGE_LOOP('',(#24297,#24298,#24299,#24300));
#5615=EDGE_LOOP('',(#24301,#24302,#24303,#24304));
#5616=EDGE_LOOP('',(#24305,#24306,#24307,#24308));
#5617=EDGE_LOOP('',(#24309,#24310,#24311));
#5618=EDGE_LOOP('',(#24312,#24313,#24314,#24315));
#5619=EDGE_LOOP('',(#24316,#24317,#24318));
#5620=EDGE_LOOP('',(#24319,#24320,#24321,#24322));
#5621=EDGE_LOOP('',(#24323,#24324,#24325));
#5622=EDGE_LOOP('',(#24326,#24327,#24328,#24329));
#5623=EDGE_LOOP('',(#24330,#24331,#24332));
#5624=EDGE_LOOP('',(#24333,#24334,#24335,#24336));
#5625=EDGE_LOOP('',(#24337,#24338,#24339));
#5626=EDGE_LOOP('',(#24340,#24341,#24342,#24343));
#5627=EDGE_LOOP('',(#24344,#24345,#24346));
#5628=EDGE_LOOP('',(#24347,#24348,#24349,#24350));
#5629=EDGE_LOOP('',(#24351,#24352,#24353));
#5630=EDGE_LOOP('',(#24354,#24355,#24356,#24357));
#5631=EDGE_LOOP('',(#24358,#24359,#24360));
#5632=EDGE_LOOP('',(#24361,#24362,#24363,#24364));
#5633=EDGE_LOOP('',(#24365,#24366,#24367));
#5634=EDGE_LOOP('',(#24368,#24369,#24370,#24371));
#5635=EDGE_LOOP('',(#24372,#24373,#24374));
#5636=EDGE_LOOP('',(#24375,#24376,#24377,#24378));
#5637=EDGE_LOOP('',(#24379,#24380,#24381));
#5638=EDGE_LOOP('',(#24382,#24383,#24384,#24385));
#5639=EDGE_LOOP('',(#24386,#24387,#24388));
#5640=EDGE_LOOP('',(#24389,#24390,#24391,#24392));
#5641=EDGE_LOOP('',(#24393,#24394,#24395));
#5642=EDGE_LOOP('',(#24396,#24397,#24398,#24399));
#5643=EDGE_LOOP('',(#24400,#24401,#24402));
#5644=EDGE_LOOP('',(#24403,#24404,#24405,#24406));
#5645=EDGE_LOOP('',(#24407,#24408,#24409));
#5646=EDGE_LOOP('',(#24410,#24411,#24412,#24413));
#5647=EDGE_LOOP('',(#24414,#24415,#24416));
#5648=EDGE_LOOP('',(#24417,#24418,#24419,#24420));
#5649=EDGE_LOOP('',(#24421,#24422,#24423));
#5650=EDGE_LOOP('',(#24424,#24425,#24426,#24427));
#5651=EDGE_LOOP('',(#24428,#24429,#24430));
#5652=EDGE_LOOP('',(#24431,#24432,#24433,#24434));
#5653=EDGE_LOOP('',(#24435,#24436,#24437));
#5654=EDGE_LOOP('',(#24438,#24439,#24440,#24441));
#5655=EDGE_LOOP('',(#24442,#24443,#24444));
#5656=EDGE_LOOP('',(#24445,#24446,#24447,#24448));
#5657=EDGE_LOOP('',(#24449,#24450,#24451));
#5658=EDGE_LOOP('',(#24452,#24453,#24454,#24455));
#5659=EDGE_LOOP('',(#24456,#24457,#24458));
#5660=EDGE_LOOP('',(#24459,#24460,#24461,#24462));
#5661=EDGE_LOOP('',(#24463,#24464,#24465));
#5662=EDGE_LOOP('',(#24466,#24467,#24468,#24469));
#5663=EDGE_LOOP('',(#24470,#24471,#24472));
#5664=EDGE_LOOP('',(#24473,#24474,#24475,#24476));
#5665=EDGE_LOOP('',(#24477,#24478,#24479));
#5666=EDGE_LOOP('',(#24480,#24481,#24482,#24483));
#5667=EDGE_LOOP('',(#24484,#24485,#24486));
#5668=EDGE_LOOP('',(#24487,#24488,#24489,#24490));
#5669=EDGE_LOOP('',(#24491,#24492,#24493));
#5670=EDGE_LOOP('',(#24494,#24495,#24496,#24497));
#5671=EDGE_LOOP('',(#24498,#24499,#24500));
#5672=EDGE_LOOP('',(#24501,#24502,#24503,#24504));
#5673=EDGE_LOOP('',(#24505,#24506,#24507));
#5674=EDGE_LOOP('',(#24508,#24509,#24510,#24511));
#5675=EDGE_LOOP('',(#24512,#24513,#24514));
#5676=EDGE_LOOP('',(#24515,#24516,#24517,#24518));
#5677=EDGE_LOOP('',(#24519,#24520,#24521));
#5678=EDGE_LOOP('',(#24522,#24523,#24524,#24525));
#5679=EDGE_LOOP('',(#24526,#24527,#24528));
#5680=EDGE_LOOP('',(#24529,#24530,#24531,#24532));
#5681=EDGE_LOOP('',(#24533,#24534,#24535));
#5682=EDGE_LOOP('',(#24536,#24537,#24538,#24539));
#5683=EDGE_LOOP('',(#24540,#24541,#24542));
#5684=EDGE_LOOP('',(#24543,#24544,#24545));
#5685=EDGE_LOOP('',(#24546,#24547,#24548,#24549));
#5686=EDGE_LOOP('',(#24550,#24551,#24552,#24553));
#5687=EDGE_LOOP('',(#24554,#24555,#24556));
#5688=EDGE_LOOP('',(#24557,#24558,#24559,#24560));
#5689=EDGE_LOOP('',(#24561,#24562,#24563));
#5690=EDGE_LOOP('',(#24564,#24565,#24566,#24567));
#5691=EDGE_LOOP('',(#24568,#24569,#24570));
#5692=EDGE_LOOP('',(#24571,#24572,#24573,#24574));
#5693=EDGE_LOOP('',(#24575,#24576,#24577));
#5694=EDGE_LOOP('',(#24578,#24579,#24580,#24581));
#5695=EDGE_LOOP('',(#24582,#24583,#24584));
#5696=EDGE_LOOP('',(#24585,#24586,#24587,#24588));
#5697=EDGE_LOOP('',(#24589,#24590,#24591));
#5698=EDGE_LOOP('',(#24592,#24593,#24594,#24595));
#5699=EDGE_LOOP('',(#24596,#24597,#24598));
#5700=EDGE_LOOP('',(#24599,#24600,#24601,#24602));
#5701=EDGE_LOOP('',(#24603,#24604,#24605));
#5702=EDGE_LOOP('',(#24606,#24607,#24608,#24609));
#5703=EDGE_LOOP('',(#24610,#24611,#24612));
#5704=EDGE_LOOP('',(#24613,#24614,#24615,#24616));
#5705=EDGE_LOOP('',(#24617,#24618,#24619));
#5706=EDGE_LOOP('',(#24620,#24621,#24622,#24623));
#5707=EDGE_LOOP('',(#24624,#24625,#24626));
#5708=EDGE_LOOP('',(#24627,#24628,#24629,#24630));
#5709=EDGE_LOOP('',(#24631,#24632,#24633));
#5710=EDGE_LOOP('',(#24634,#24635,#24636,#24637));
#5711=EDGE_LOOP('',(#24638,#24639,#24640));
#5712=EDGE_LOOP('',(#24641,#24642,#24643,#24644));
#5713=EDGE_LOOP('',(#24645,#24646,#24647));
#5714=EDGE_LOOP('',(#24648,#24649,#24650,#24651));
#5715=EDGE_LOOP('',(#24652,#24653,#24654));
#5716=EDGE_LOOP('',(#24655,#24656,#24657,#24658));
#5717=EDGE_LOOP('',(#24659,#24660,#24661));
#5718=EDGE_LOOP('',(#24662,#24663,#24664,#24665));
#5719=EDGE_LOOP('',(#24666,#24667,#24668));
#5720=EDGE_LOOP('',(#24669,#24670,#24671,#24672));
#5721=EDGE_LOOP('',(#24673,#24674,#24675));
#5722=EDGE_LOOP('',(#24676,#24677,#24678,#24679));
#5723=EDGE_LOOP('',(#24680,#24681,#24682));
#5724=EDGE_LOOP('',(#24683));
#5725=EDGE_LOOP('',(#24684,#24685,#24686,#24687,#24688,#24689));
#5726=EDGE_LOOP('',(#24690,#24691,#24692,#24693));
#5727=EDGE_LOOP('',(#24694,#24695,#24696,#24697,#24698,#24699,#24700,#24701,
#24702,#24703,#24704,#24705,#24706,#24707,#24708,#24709,#24710,#24711,#24712,
#24713,#24714,#24715,#24716,#24717,#24718,#24719,#24720,#24721,#24722,#24723,
#24724,#24725,#24726,#24727,#24728,#24729,#24730,#24731,#24732,#24733,#24734,
#24735,#24736,#24737,#24738,#24739,#24740,#24741,#24742,#24743,#24744,#24745,
#24746,#24747,#24748,#24749,#24750,#24751,#24752,#24753,#24754,#24755,#24756,
#24757,#24758,#24759,#24760,#24761,#24762,#24763,#24764,#24765,#24766,#24767,
#24768,#24769,#24770,#24771,#24772,#24773,#24774,#24775,#24776,#24777,#24778,
#24779,#24780,#24781,#24782,#24783,#24784,#24785,#24786,#24787,#24788,#24789,
#24790,#24791,#24792,#24793,#24794,#24795,#24796,#24797,#24798,#24799,#24800,
#24801,#24802,#24803,#24804,#24805,#24806,#24807,#24808,#24809,#24810,#24811,
#24812,#24813,#24814,#24815,#24816,#24817,#24818,#24819,#24820,#24821,#24822,
#24823,#24824,#24825,#24826,#24827,#24828,#24829,#24830,#24831,#24832,#24833,
#24834,#24835,#24836,#24837,#24838,#24839,#24840,#24841));
#5728=EDGE_LOOP('',(#24842,#24843,#24844,#24845,#24846,#24847,#24848,#24849,
#24850,#24851,#24852,#24853,#24854,#24855,#24856,#24857,#24858,#24859,#24860,
#24861,#24862,#24863,#24864,#24865,#24866,#24867,#24868,#24869,#24870,#24871,
#24872,#24873,#24874,#24875,#24876,#24877,#24878,#24879,#24880,#24881,#24882,
#24883,#24884,#24885,#24886,#24887,#24888,#24889,#24890,#24891,#24892,#24893,
#24894,#24895,#24896,#24897,#24898,#24899,#24900,#24901,#24902,#24903,#24904,
#24905,#24906,#24907,#24908,#24909,#24910,#24911,#24912,#24913,#24914,#24915,
#24916,#24917));
#5729=EDGE_LOOP('',(#24918));
#5730=EDGE_LOOP('',(#24919,#24920,#24921,#24922,#24923,#24924));
#5731=CIRCLE('',#26908,1.11464466094068);
#5732=CIRCLE('',#26909,1.2);
#5733=CIRCLE('',#26912,1.11464466094067);
#5734=CIRCLE('',#26913,1.2);
#5735=CIRCLE('',#26916,1.11464466094067);
#5736=CIRCLE('',#26917,1.2);
#5737=CIRCLE('',#26920,1.11464466094067);
#5738=CIRCLE('',#26921,1.2);
#5739=CIRCLE('',#26925,1.03535533905933);
#5740=CIRCLE('',#26928,1.03535533905933);
#5741=CIRCLE('',#26930,1.8);
#5742=CIRCLE('',#26931,1.8);
#5743=CIRCLE('',#26932,1.8);
#5744=CIRCLE('',#26933,1.80000000000001);
#5745=CIRCLE('',#26935,0.555000000000003);
#5746=CIRCLE('',#26936,0.505000000000003);
#5747=CIRCLE('',#26938,0.7);
#5748=CIRCLE('',#26939,0.699999999999998);
#5749=CIRCLE('',#26940,0.700000000000002);
#5750=CIRCLE('',#26941,0.700000000000007);
#5751=CIRCLE('',#26942,0.555000000000003);
#5752=CIRCLE('',#26943,0.555);
#5753=CIRCLE('',#26944,0.875);
#5754=CIRCLE('',#26945,0.555);
#5755=CIRCLE('',#26947,0.505000000000003);
#5756=CIRCLE('',#26949,0.505000000000003);
#5757=CIRCLE('',#26951,0.505000000000003);
#5758=CIRCLE('',#26953,0.504999999999999);
#5759=CIRCLE('',#26955,0.504999999999999);
#5760=CIRCLE('',#26957,0.504999999999999);
#5761=CIRCLE('',#26959,0.504999999999999);
#5762=CIRCLE('',#26969,1.03535533905933);
#5763=CIRCLE('',#26970,0.999999999999998);
#5764=CIRCLE('',#26973,1.03535533905933);
#5765=CIRCLE('',#26974,1.);
#5766=CIRCLE('',#26978,1.00000000000001);
#5767=CIRCLE('',#26981,1.);
#5768=CIRCLE('',#26983,0.605);
#5769=CIRCLE('',#26984,0.605);
#5770=CIRCLE('',#26986,1.);
#5771=CIRCLE('',#26989,1.00000000000001);
#5772=CIRCLE('',#26991,0.605);
#5773=CIRCLE('',#26992,0.605);
#5774=CIRCLE('',#26994,0.605);
#5775=CIRCLE('',#26996,0.605);
#5776=CIRCLE('',#27008,1.88535533905933);
#5777=CIRCLE('',#27011,1.88535533905933);
#5778=CIRCLE('',#27014,1.88535533905933);
#5779=CIRCLE('',#27017,1.88535533905933);
#5780=CIRCLE('',#27021,1.96464466094067);
#5781=CIRCLE('',#27024,1.96464466094067);
#5782=CIRCLE('',#27027,1.96464466094067);
#5783=CIRCLE('',#27028,2.);
#5784=CIRCLE('',#27032,1.96464466094068);
#5785=CIRCLE('',#27033,2.);
#5786=CIRCLE('',#27036,2.);
#5787=CIRCLE('',#27039,2.);
#5788=CIRCLE('',#27041,0.605);
#5789=CIRCLE('',#27042,0.605);
#5790=CIRCLE('',#27044,2.);
#5791=CIRCLE('',#27047,2.);
#5792=CIRCLE('',#27050,1.96464466094068);
#5793=CIRCLE('',#27051,2.);
#5794=CIRCLE('',#27054,1.96464466094067);
#5795=CIRCLE('',#27057,1.9);
#5796=CIRCLE('',#27060,1.9);
#5797=CIRCLE('',#27065,1.93535533905932);
#5798=CIRCLE('',#27066,1.85);
#5799=CIRCLE('',#27069,1.93535533905933);
#5800=CIRCLE('',#27070,1.85);
#5801=CIRCLE('',#27079,1.96464466094067);
#5802=CIRCLE('',#27082,1.96464466094067);
#5803=CIRCLE('',#27083,2.);
#5804=CIRCLE('',#27095,0.875);
#5805=CIRCLE('',#27102,0.299999999999997);
#5806=CIRCLE('',#27103,0.3);
#5807=CIRCLE('',#27104,1.);
#5808=CIRCLE('',#27106,0.3);
#5809=CIRCLE('',#27108,0.3);
#5810=CIRCLE('',#27110,0.3);
#5811=CIRCLE('',#27112,0.3);
#5812=CIRCLE('',#27114,0.3);
#5813=CIRCLE('',#27116,0.3);
#5814=CIRCLE('',#27117,0.999999999999998);
#5815=CIRCLE('',#27143,1.65000000000001);
#5816=CIRCLE('',#27144,1.73535533905934);
#5817=CIRCLE('',#27145,1.73535533905934);
#5818=CIRCLE('',#27147,1.76464466094067);
#5819=CIRCLE('',#27148,1.76464466094067);
#5820=CIRCLE('',#27150,0.605000000000004);
#5821=CIRCLE('',#27152,1.8);
#5822=CIRCLE('',#27153,1.8);
#5823=CIRCLE('',#27156,0.355000000000002);
#5824=CIRCLE('',#27157,0.305);
#5825=CIRCLE('',#27158,0.305);
#5826=CIRCLE('',#27159,0.355000000000002);
#5827=CIRCLE('',#27161,5.5);
#5828=CIRCLE('',#27162,5.5);
#5829=CIRCLE('',#27163,5.3);
#5830=CIRCLE('',#27164,5.3);
#5831=CIRCLE('',#27165,5.3);
#5832=CIRCLE('',#27166,5.3);
#5833=CIRCLE('',#27167,5.3);
#5834=CIRCLE('',#27169,0.305);
#5835=CIRCLE('',#27171,0.354999999999998);
#5836=CIRCLE('',#27172,0.305);
#5837=CIRCLE('',#27173,0.354999999999998);
#5838=CIRCLE('',#27175,0.305);
#5839=CIRCLE('',#27178,0.95);
#5840=CIRCLE('',#27179,0.950000000000001);
#5841=CIRCLE('',#27180,0.600000000000001);
#5842=CIRCLE('',#27181,0.600000000000001);
#5843=CIRCLE('',#27182,0.600000000000001);
#5844=CIRCLE('',#27183,0.600000000000001);
#5845=CIRCLE('',#27187,5.33535533905933);
#5846=CIRCLE('',#27188,5.25);
#5847=CIRCLE('',#27190,5.46464466094067);
#5848=CIRCLE('',#27192,3.5);
#5849=CIRCLE('',#27194,5.5);
#5850=CIRCLE('',#27195,5.5);
#5851=CIRCLE('',#27196,5.5);
#5852=CIRCLE('',#27198,0.700000000000003);
#5853=CIRCLE('',#27203,19.3353883884215);
#5854=CIRCLE('',#27204,19.3853883884215);
#5855=CIRCLE('',#27212,1.);
#5856=CIRCLE('',#27213,0.95);
#5857=CIRCLE('',#27216,1.);
#5858=CIRCLE('',#27217,0.95);
#5859=CIRCLE('',#27224,1.);
#5860=CIRCLE('',#27226,1.);
#5861=CIRCLE('',#27229,1.);
#5862=CIRCLE('',#27231,5.8);
#5863=CIRCLE('',#27232,4.8);
#5864=CIRCLE('',#27238,0.600000000000001);
#5865=CIRCLE('',#27239,0.600000000000001);
#5866=CIRCLE('',#27240,0.600000000000001);
#5867=CIRCLE('',#27241,0.600000000000001);
#5868=CIRCLE('',#27244,0.550000000000001);
#5869=CIRCLE('',#27247,0.550000000000001);
#5870=CIRCLE('',#27249,0.550000000000001);
#5871=CIRCLE('',#27253,0.550000000000001);
#5872=CIRCLE('',#27256,0.550000000000001);
#5873=CIRCLE('',#27258,0.550000000000001);
#5874=CIRCLE('',#27262,0.550000000000001);
#5875=CIRCLE('',#27265,0.550000000000001);
#5876=CIRCLE('',#27267,0.550000000000001);
#5877=CIRCLE('',#27271,0.550000000000001);
#5878=CIRCLE('',#27274,0.550000000000001);
#5879=CIRCLE('',#27276,0.550000000000001);
#5880=CIRCLE('',#27279,0.355000000000002);
#5881=CIRCLE('',#27280,0.305);
#5882=CIRCLE('',#27281,0.305);
#5883=CIRCLE('',#27282,0.355000000000002);
#5884=CIRCLE('',#27284,0.305);
#5885=CIRCLE('',#27286,0.355000000000001);
#5886=CIRCLE('',#27287,0.305);
#5887=CIRCLE('',#27288,0.355000000000001);
#5888=CIRCLE('',#27290,0.305);
#5889=CIRCLE('',#27293,0.600000000000001);
#5890=CIRCLE('',#27294,0.550000000000001);
#5891=CIRCLE('',#27297,0.600000000000001);
#5892=CIRCLE('',#27300,0.95);
#5893=CIRCLE('',#27301,0.95);
#5894=CIRCLE('',#27302,0.95);
#5895=CIRCLE('',#27303,0.950000000000001);
#5896=CIRCLE('',#27304,0.600000000000001);
#5897=CIRCLE('',#27305,0.600000000000001);
#5898=CIRCLE('',#27306,0.600000000000001);
#5899=CIRCLE('',#27307,0.600000000000001);
#5900=CIRCLE('',#27308,0.600000000000001);
#5901=CIRCLE('',#27309,0.600000000000001);
#5902=CIRCLE('',#27312,0.550000000000001);
#5903=CIRCLE('',#27318,0.550000000000001);
#5904=CIRCLE('',#27324,0.550000000000001);
#5905=CIRCLE('',#27329,1.);
#5906=CIRCLE('',#27332,1.);
#5907=CIRCLE('',#27335,1.);
#5908=CIRCLE('',#27346,19.3853883884215);
#5909=CIRCLE('',#27347,19.3353883884215);
#5910=CIRCLE('',#27350,4.5);
#5911=CIRCLE('',#27360,0.299999999999999);
#5912=CIRCLE('',#27362,0.3);
#5913=CIRCLE('',#27366,0.3);
#5914=CIRCLE('',#27371,0.3);
#5915=CIRCLE('',#27385,0.405000000000001);
#5916=CIRCLE('',#27388,1.005);
#5917=CIRCLE('',#27390,0.605000000000004);
#5918=CIRCLE('',#27393,3.5);
#5919=CIRCLE('',#27397,3.05);
#5920=CIRCLE('',#27398,3.11844928601987);
#5921=CIRCLE('',#27399,3.11844928601987);
#5922=CIRCLE('',#27401,3.497);
#5923=CIRCLE('',#27403,1.64335);
#5924=CIRCLE('',#27406,3.497);
#5925=CIRCLE('',#27409,3.497);
#5926=CIRCLE('',#27413,3.497);
#5927=CIRCLE('',#27416,3.497);
#5928=CIRCLE('',#27420,3.497);
#5929=CIRCLE('',#27423,3.497);
#5930=CIRCLE('',#27427,3.497);
#5931=CIRCLE('',#27430,3.497);
#5932=CIRCLE('',#27434,3.497);
#5933=CIRCLE('',#27437,3.497);
#5934=CIRCLE('',#27441,3.497);
#5935=CIRCLE('',#27444,3.497);
#5936=CIRCLE('',#27448,3.497);
#5937=CIRCLE('',#27451,3.497);
#5938=CIRCLE('',#27455,3.497);
#5939=CIRCLE('',#27458,3.497);
#5940=CIRCLE('',#27462,3.497);
#5941=CIRCLE('',#27465,3.497);
#5942=CIRCLE('',#27469,3.497);
#5943=CIRCLE('',#27472,3.497);
#5944=CIRCLE('',#27476,3.497);
#5945=CIRCLE('',#27479,3.497);
#5946=CIRCLE('',#27483,3.497);
#5947=CIRCLE('',#27486,3.497);
#5948=CIRCLE('',#27490,3.497);
#5949=CIRCLE('',#27493,3.497);
#5950=CIRCLE('',#27497,3.497);
#5951=CIRCLE('',#27500,3.497);
#5952=CIRCLE('',#27504,3.497);
#5953=CIRCLE('',#27507,3.497);
#5954=CIRCLE('',#27511,3.497);
#5955=CIRCLE('',#27514,3.497);
#5956=CIRCLE('',#27518,3.497);
#5957=CIRCLE('',#27521,3.497);
#5958=CIRCLE('',#27525,3.497);
#5959=CIRCLE('',#27528,3.497);
#5960=CIRCLE('',#27532,3.497);
#5961=CIRCLE('',#27535,3.497);
#5962=CIRCLE('',#27539,3.497);
#5963=CIRCLE('',#27542,3.497);
#5964=CIRCLE('',#27546,3.497);
#5965=CIRCLE('',#27549,3.497);
#5966=CIRCLE('',#27553,0.3);
#5967=CIRCLE('',#27556,0.3);
#5968=CIRCLE('',#27559,2.);
#5969=CIRCLE('',#27560,2.);
#5970=CIRCLE('',#27562,3.397);
#5971=CIRCLE('',#27564,3.497);
#5972=CIRCLE('',#27567,1.5612724);
#5973=CIRCLE('',#27569,1.256904);
#5974=CIRCLE('',#27571,1.1);
#5975=CIRCLE('',#27573,1.1);
#5976=CIRCLE('',#27577,1.62016810220205);
#5977=CIRCLE('',#27578,1.62016810220205);
#5978=CIRCLE('',#27579,1.64385418552926);
#5979=CIRCLE('',#27580,1.64385418552926);
#5980=CIRCLE('',#27582,1.56235);
#5981=CIRCLE('',#27585,1.1792801);
#5982=CIRCLE('',#27587,1.2592801);
#5983=CIRCLE('',#27591,0.9925);
#5984=CIRCLE('',#27634,0.76435);
#5985=CIRCLE('',#27677,0.85);
#5986=CIRCLE('',#27678,0.935355339059328);
#5987=CIRCLE('',#27679,0.935355339059328);
#5988=CIRCLE('',#27681,0.957144660940674);
#5989=CIRCLE('',#27682,0.95714466094067);
#5990=CIRCLE('',#27683,0.957144660940674);
#5991=CIRCLE('',#27686,0.455000000000002);
#5992=CIRCLE('',#27687,0.405000000000001);
#5993=CIRCLE('',#27689,0.405000000000001);
#5994=CIRCLE('',#27691,0.95);
#5995=CIRCLE('',#27693,0.9925);
#5996=CIRCLE('',#27695,0.942499999999996);
#5997=CIRCLE('',#27698,0.76435);
#5998=CIRCLE('',#27703,0.25);
#5999=CIRCLE('',#27706,0.25);
#6000=CIRCLE('',#27709,1.);
#6001=CIRCLE('',#27711,1.);
#6002=CIRCLE('',#27713,1.55);
#6003=CIRCLE('',#27715,1.6);
#6004=CIRCLE('',#27717,1.6);
#6005=CIRCLE('',#27719,1.55);
#6006=CIRCLE('',#27723,1.155);
#6007=CIRCLE('',#27724,1.06964466094067);
#6008=CIRCLE('',#27725,1.06964466094067);
#6009=CIRCLE('',#27727,1.04035533905933);
#6010=CIRCLE('',#27728,1.04035533905933);
#6011=CIRCLE('',#27730,1.95);
#6012=CIRCLE('',#27732,1.005);
#6013=CIRCLE('',#27733,1.005);
#6014=CIRCLE('',#27735,1.005);
#6015=CIRCLE('',#27737,2.);
#6016=CIRCLE('',#27738,1.92);
#6017=CIRCLE('',#27740,1.92);
#6018=CIRCLE('',#27742,2.);
#6019=CIRCLE('',#27744,2.);
#6020=CIRCLE('',#27747,2.);
#6021=CIRCLE('',#27749,1.95);
#6022=CIRCLE('',#27751,1.105);
#6023=CIRCLE('',#27755,1.8);
#6024=CIRCLE('',#27756,1.8);
#6025=CIRCLE('',#27757,1.85);
#6026=CIRCLE('',#27759,3.445);
#6027=CIRCLE('',#27761,1.8);
#6028=CIRCLE('',#27763,6.1);
#6029=CIRCLE('',#27764,6.18535533905933);
#6030=CIRCLE('',#27765,6.18535533905933);
#6031=CIRCLE('',#27767,6.21464466094067);
#6032=CIRCLE('',#27768,6.21464466094067);
#6033=CIRCLE('',#27770,3.495);
#6034=CIRCLE('',#27771,0.330000000000002);
#6035=CIRCLE('',#27772,0.330000000000002);
#6036=CIRCLE('',#27773,0.330000000000002);
#6037=CIRCLE('',#27774,0.330000000000002);
#6038=CIRCLE('',#27776,6.25);
#6039=CIRCLE('',#27777,6.25);
#6040=CIRCLE('',#27779,6.25);
#6041=CIRCLE('',#27780,6.25);
#6042=CIRCLE('',#27782,6.21464466094067);
#6043=CIRCLE('',#27783,6.21464466094067);
#6044=CIRCLE('',#27785,6.18535533905933);
#6045=CIRCLE('',#27786,6.18535533905933);
#6046=CIRCLE('',#27788,6.1);
#6047=CIRCLE('',#27790,2.8);
#6048=CIRCLE('',#27791,0.330000000000002);
#6049=CIRCLE('',#27792,0.330000000000002);
#6050=CIRCLE('',#27793,0.330000000000002);
#6051=CIRCLE('',#27794,0.330000000000002);
#6052=CIRCLE('',#27796,2.8);
#6053=CIRCLE('',#27797,2.8);
#6054=CIRCLE('',#27798,2.76464466094067);
#6055=CIRCLE('',#27799,2.76464466094067);
#6056=CIRCLE('',#27801,2.73535533905933);
#6057=CIRCLE('',#27802,2.73535533905933);
#6058=CIRCLE('',#27805,2.65);
#6059=CIRCLE('',#27807,1.85);
#6060=CIRCLE('',#27809,1.8);
#6061=CIRCLE('',#27810,1.8);
#6062=CIRCLE('',#27812,1.8);
#6063=CIRCLE('',#27818,3.495);
#6064=CIRCLE('',#27821,1.05);
#6065=CIRCLE('',#27823,1.05);
#6066=CIRCLE('',#27827,2.46464466094067);
#6067=CIRCLE('',#27828,2.46464466094067);
#6068=CIRCLE('',#27829,2.5);
#6069=CIRCLE('',#27830,2.5);
#6070=CIRCLE('',#27832,2.5);
#6071=CIRCLE('',#27833,2.5);
#6072=CIRCLE('',#27835,2.43535533905933);
#6073=CIRCLE('',#27836,2.43535533905933);
#6074=CIRCLE('',#27838,2.46464466094067);
#6075=CIRCLE('',#27839,2.46464466094067);
#6076=CIRCLE('',#27841,2.43535533905933);
#6077=CIRCLE('',#27842,2.43535533905933);
#6078=CIRCLE('',#27844,2.35);
#6079=CIRCLE('',#27846,0.46);
#6080=CIRCLE('',#27848,2.35);
#6081=CIRCLE('',#27850,1.);
#6082=CIRCLE('',#27860,1.);
#6083=CIRCLE('',#27866,1.1);
#6084=CIRCLE('',#27867,9.3);
#6085=CIRCLE('',#27868,9.3);
#6086=CIRCLE('',#27869,9.3);
#6087=CIRCLE('',#27870,9.3);
#6088=CIRCLE('',#27871,9.3);
#6089=CIRCLE('',#27873,0.46);
#6090=CIRCLE('',#27877,0.3933);
#6091=CIRCLE('',#27894,0.322275);
#6092=CIRCLE('',#27910,0.3933);
#6093=CIRCLE('',#27911,0.3933);
#6094=CIRCLE('',#27913,0.3933);
#6095=CIRCLE('',#27914,0.3933);
#6096=CIRCLE('',#27915,0.322275);
#6097=CIRCLE('',#27918,0.025);
#6098=CIRCLE('',#27919,0.4183);
#6099=CIRCLE('',#27920,0.3933);
#6100=CIRCLE('',#27923,0.62);
#6101=CIRCLE('',#27925,0.346410161513775);
#6102=CIRCLE('',#27927,0.346410161513775);
#6103=CIRCLE('',#27929,0.346410161513775);
#6104=CIRCLE('',#27931,0.346410161513775);
#6105=CIRCLE('',#27933,0.346410161513775);
#6106=CIRCLE('',#27935,0.346410161513775);
#6107=CIRCLE('',#27945,0.65);
#6108=CIRCLE('',#27948,0.65);
#6109=CIRCLE('',#27951,0.65);
#6110=CIRCLE('',#27954,0.65);
#6111=CIRCLE('',#27957,0.65);
#6112=CIRCLE('',#27960,0.65);
#6113=CIRCLE('',#27963,0.65);
#6114=CIRCLE('',#27966,0.65);
#6115=CIRCLE('',#27969,0.65);
#6116=CIRCLE('',#27972,0.65);
#6117=CIRCLE('',#27975,0.65);
#6118=CIRCLE('',#27978,0.65);
#6119=CIRCLE('',#27981,0.65);
#6120=CIRCLE('',#27984,0.65);
#6121=CIRCLE('',#27987,0.65);
#6122=CIRCLE('',#27990,0.65);
#6123=CIRCLE('',#27993,0.65);
#6124=CIRCLE('',#27994,0.65);
#6125=CIRCLE('',#27997,0.65);
#6126=CIRCLE('',#27998,0.65);
#6127=CIRCLE('',#28001,0.65);
#6128=CIRCLE('',#28004,0.65);
#6129=CIRCLE('',#28007,0.65);
#6130=CIRCLE('',#28010,0.65);
#6131=CIRCLE('',#28013,0.65);
#6132=CIRCLE('',#28016,0.65);
#6133=CIRCLE('',#28019,0.65);
#6134=CIRCLE('',#28022,0.65);
#6135=CIRCLE('',#28025,0.65);
#6136=CIRCLE('',#28028,0.65);
#6137=CIRCLE('',#28031,0.65);
#6138=CIRCLE('',#28034,0.65);
#6139=CIRCLE('',#28037,0.65);
#6140=CIRCLE('',#28040,0.65);
#6141=CIRCLE('',#28043,0.65);
#6142=CIRCLE('',#28046,0.65);
#6143=CIRCLE('',#28049,0.65);
#6144=CIRCLE('',#28052,0.65);
#6145=CIRCLE('',#28055,0.65);
#6146=CIRCLE('',#28058,0.65);
#6147=CIRCLE('',#28061,0.65);
#6148=CIRCLE('',#28064,0.65);
#6149=CIRCLE('',#28067,0.65);
#6150=CIRCLE('',#28070,0.65);
#6151=CIRCLE('',#28073,0.65);
#6152=CIRCLE('',#28076,0.65);
#6153=CIRCLE('',#28079,0.65);
#6154=CIRCLE('',#28082,0.65);
#6155=CIRCLE('',#28085,0.65);
#6156=CIRCLE('',#28088,0.65);
#6157=CIRCLE('',#28091,0.65);
#6158=CIRCLE('',#28094,0.65);
#6159=CIRCLE('',#28097,0.65);
#6160=CIRCLE('',#28100,0.65);
#6161=CIRCLE('',#28102,0.65);
#6162=CIRCLE('',#28106,0.65);
#6163=CIRCLE('',#28109,0.65);
#6164=CIRCLE('',#28112,0.65);
#6165=CIRCLE('',#28115,0.65);
#6166=CIRCLE('',#28118,0.65);
#6167=CIRCLE('',#28121,0.65);
#6168=CIRCLE('',#28124,0.65);
#6169=CIRCLE('',#28127,0.65);
#6170=CIRCLE('',#28130,0.65);
#6171=CIRCLE('',#28133,0.65);
#6172=CIRCLE('',#28136,0.65);
#6173=CIRCLE('',#28139,0.65);
#6174=CIRCLE('',#28142,0.65);
#6175=CIRCLE('',#28145,0.65);
#6176=CIRCLE('',#28148,0.65);
#6177=CIRCLE('',#28151,0.65);
#6178=CIRCLE('',#28154,0.65);
#6179=CIRCLE('',#28157,0.65);
#6180=CIRCLE('',#28160,0.65);
#6181=CIRCLE('',#28162,0.35);
#6182=CIRCLE('',#28165,0.65);
#6183=CIRCLE('',#28167,0.65);
#6184=CIRCLE('',#28168,0.65);
#6185=CIRCLE('',#28169,0.65);
#6186=CIRCLE('',#28170,0.65);
#6187=CIRCLE('',#28171,0.65);
#6188=CIRCLE('',#28172,0.65);
#6189=CIRCLE('',#28173,0.65);
#6190=CIRCLE('',#28174,0.65);
#6191=CIRCLE('',#28175,0.65);
#6192=CIRCLE('',#28176,0.65);
#6193=CIRCLE('',#28177,0.65);
#6194=CIRCLE('',#28178,0.65);
#6195=CIRCLE('',#28179,0.65);
#6196=CIRCLE('',#28180,0.65);
#6197=CIRCLE('',#28181,0.65);
#6198=CIRCLE('',#28182,0.65);
#6199=CIRCLE('',#28183,0.65);
#6200=CIRCLE('',#28184,0.65);
#6201=CIRCLE('',#28185,0.65);
#6202=CIRCLE('',#28186,0.65);
#6203=CIRCLE('',#28187,0.65);
#6204=CIRCLE('',#28188,0.65);
#6205=CIRCLE('',#28189,0.65);
#6206=CIRCLE('',#28190,0.65);
#6207=CIRCLE('',#28191,0.65);
#6208=CIRCLE('',#28192,0.65);
#6209=CIRCLE('',#28193,0.65);
#6210=CIRCLE('',#28194,0.65);
#6211=CIRCLE('',#28195,0.65);
#6212=CIRCLE('',#28196,0.65);
#6213=CIRCLE('',#28197,0.65);
#6214=CIRCLE('',#28198,0.65);
#6215=CIRCLE('',#28199,0.65);
#6216=CIRCLE('',#28200,0.65);
#6217=CIRCLE('',#28201,0.65);
#6218=CIRCLE('',#28202,0.65);
#6219=CIRCLE('',#28204,0.6);
#6220=CIRCLE('',#28209,0.25);
#6221=CIRCLE('',#28210,0.23);
#6222=CIRCLE('',#28213,0.25);
#6223=CIRCLE('',#28214,0.23);
#6224=CIRCLE('',#28216,0.25);
#6225=CIRCLE('',#28221,0.225);
#6226=CIRCLE('',#28222,0.25);
#6227=CIRCLE('',#28225,0.225);
#6228=CIRCLE('',#28231,0.591675);
#6229=CIRCLE('',#28242,0.491824999999999);
#6230=CIRCLE('',#28252,1.38);
#6231=CIRCLE('',#28253,1.3);
#6232=CIRCLE('',#28255,1.5);
#6233=CIRCLE('',#28256,1.5);
#6234=CIRCLE('',#28258,0.591675);
#6235=CIRCLE('',#28259,0.591675);
#6236=CIRCLE('',#28260,0.491824999999999);
#6237=CIRCLE('',#28263,0.599999999999992);
#6238=CIRCLE('',#28264,0.599999999999992);
#6239=CIRCLE('',#28265,0.599999999999992);
#6240=CIRCLE('',#28267,0.8);
#6241=CIRCLE('',#28270,1.1);
#6242=CIRCLE('',#28271,1.1);
#6243=CIRCLE('',#28275,0.549999999999997);
#6244=CIRCLE('',#28278,0.591675);
#6245=CIRCLE('',#28280,1.5);
#6246=CIRCLE('',#28285,1.);
#6247=CIRCLE('',#28287,0.950000000000003);
#6248=CIRCLE('',#28291,0.3933);
#6249=CIRCLE('',#28306,0.322275);
#6250=CIRCLE('',#28321,0.3933);
#6251=CIRCLE('',#28322,0.3933);
#6252=CIRCLE('',#28323,0.322275);
#6253=CIRCLE('',#28326,0.3933);
#6254=CIRCLE('',#28327,0.275);
#6255=CIRCLE('',#28336,0.34);
#6256=CIRCLE('',#28340,0.275);
#6257=CIRCLE('',#28342,0.245);
#6258=CIRCLE('',#28365,0.7911);
#6259=CIRCLE('',#28386,0.6767);
#6260=CIRCLE('',#28388,0.6767);
#6261=CIRCLE('',#28408,0.7911);
#6262=CIRCLE('',#28409,0.7911);
#6263=CIRCLE('',#28410,0.6767);
#6264=CIRCLE('',#28413,1.14);
#6265=CIRCLE('',#28418,1.125);
#6266=CIRCLE('',#28424,0.74);
#6267=CIRCLE('',#28427,0.7911);
#6268=CIRCLE('',#28429,1.125);
#6269=CIRCLE('',#28433,0.869644660940672);
#6270=CIRCLE('',#28434,0.955000000000001);
#6271=CIRCLE('',#28436,0.840355339059329);
#6272=CIRCLE('',#28438,0.700000000000004);
#6273=CIRCLE('',#28439,0.699999999999995);
#6274=CIRCLE('',#28440,0.699999999999994);
#6275=CIRCLE('',#28441,0.700000000000004);
#6276=CIRCLE('',#28443,0.805);
#6277=CIRCLE('',#28445,0.805);
#6278=CIRCLE('',#28447,0.840355339059329);
#6279=CIRCLE('',#28449,0.869644660940672);
#6280=CIRCLE('',#28451,0.955000000000001);
#6281=CIRCLE('',#28453,0.649999999999999);
#6282=CIRCLE('',#28454,0.649999999999992);
#6283=CIRCLE('',#28455,0.649999999999993);
#6284=CIRCLE('',#28456,0.650000000000003);
#6285=CIRCLE('',#28458,0.764644660940668);
#6286=CIRCLE('',#28459,0.799999999999997);
#6287=CIRCLE('',#28462,0.764644660940679);
#6288=CIRCLE('',#28463,0.800000000000004);
#6289=CIRCLE('',#28466,0.764644660940679);
#6290=CIRCLE('',#28467,0.800000000000004);
#6291=CIRCLE('',#28470,0.764644660940672);
#6292=CIRCLE('',#28471,0.799999999999998);
#6293=CIRCLE('',#28475,0.800000000000004);
#6294=CIRCLE('',#28478,0.799999999999997);
#6295=CIRCLE('',#28485,0.735355339059332);
#6296=CIRCLE('',#28488,0.735355339059321);
#6297=CIRCLE('',#28491,0.735355339059318);
#6298=CIRCLE('',#28494,0.73535533905933);
#6299=CIRCLE('',#28496,0.764644660940668);
#6300=CIRCLE('',#28499,0.764644660940678);
#6301=CIRCLE('',#28507,0.764644660940672);
#6302=CIRCLE('',#28508,0.799999999999998);
#6303=CIRCLE('',#28511,0.764644660940679);
#6304=CIRCLE('',#28512,0.800000000000004);
#6305=CIRCLE('',#28527,1.49);
#6306=CIRCLE('',#28528,1.56);
#6307=CIRCLE('',#28530,1.56);
#6308=CIRCLE('',#28532,1.56);
#6309=CIRCLE('',#28534,1.05);
#6310=CIRCLE('',#28535,1.05);
#6311=CIRCLE('',#28537,1.7);
#6312=CIRCLE('',#28539,1.75);
#6313=CIRCLE('',#28541,1.75);
#6314=CIRCLE('',#28544,1.56);
#6315=CIRCLE('',#28546,1.72);
#6316=CIRCLE('',#28548,1.72);
#6317=CIRCLE('',#28550,1.67);
#6318=CIRCLE('',#28552,1.);
#6319=CIRCLE('',#28554,1.);
#6320=CIRCLE('',#28556,1.24);
#6321=CIRCLE('',#28558,1.24);
#6322=CIRCLE('',#28562,0.591675);
#6323=CIRCLE('',#28586,0.491825);
#6324=CIRCLE('',#28609,0.591675);
#6325=CIRCLE('',#28610,0.591675);
#6326=CIRCLE('',#28611,0.491825);
#6327=CIRCLE('',#28614,0.855);
#6328=CIRCLE('',#28619,0.83);
#6329=CIRCLE('',#28625,0.54);
#6330=CIRCLE('',#28628,0.591675);
#6331=CIRCLE('',#28630,0.83);
#6332=CIRCLE('',#28634,0.4925);
#6333=CIRCLE('',#28658,0.40705);
#6334=CIRCLE('',#28682,0.4925);
#6335=CIRCLE('',#28683,0.4925);
#6336=CIRCLE('',#28685,0.4925);
#6337=CIRCLE('',#28686,0.4925);
#6338=CIRCLE('',#28687,0.40705);
#6339=CIRCLE('',#28690,0.025);
#6340=CIRCLE('',#28691,0.5175);
#6341=CIRCLE('',#28692,0.4925);
#6342=CIRCLE('',#28695,0.77);
#6343=CIRCLE('',#28697,0.461880215351701);
#6344=CIRCLE('',#28699,0.461880215351701);
#6345=CIRCLE('',#28701,0.461880215351701);
#6346=CIRCLE('',#28703,0.461880215351701);
#6347=CIRCLE('',#28705,0.461880215351701);
#6348=CIRCLE('',#28707,0.461880215351701);
#6349=CIRCLE('',#28717,0.8);
#6350=CIRCLE('',#28720,0.8);
#6351=CIRCLE('',#28723,0.8);
#6352=CIRCLE('',#28726,0.8);
#6353=CIRCLE('',#28729,0.8);
#6354=CIRCLE('',#28732,0.8);
#6355=CIRCLE('',#28735,0.8);
#6356=CIRCLE('',#28738,0.8);
#6357=CIRCLE('',#28741,0.8);
#6358=CIRCLE('',#28744,0.8);
#6359=CIRCLE('',#28747,0.8);
#6360=CIRCLE('',#28750,0.8);
#6361=CIRCLE('',#28753,0.8);
#6362=CIRCLE('',#28756,0.8);
#6363=CIRCLE('',#28759,0.8);
#6364=CIRCLE('',#28762,0.8);
#6365=CIRCLE('',#28765,0.8);
#6366=CIRCLE('',#28766,0.8);
#6367=CIRCLE('',#28769,0.8);
#6368=CIRCLE('',#28770,0.8);
#6369=CIRCLE('',#28773,0.8);
#6370=CIRCLE('',#28776,0.8);
#6371=CIRCLE('',#28779,0.8);
#6372=CIRCLE('',#28782,0.8);
#6373=CIRCLE('',#28785,0.8);
#6374=CIRCLE('',#28788,0.8);
#6375=CIRCLE('',#28791,0.8);
#6376=CIRCLE('',#28794,0.8);
#6377=CIRCLE('',#28797,0.8);
#6378=CIRCLE('',#28800,0.8);
#6379=CIRCLE('',#28803,0.8);
#6380=CIRCLE('',#28806,0.8);
#6381=CIRCLE('',#28809,0.8);
#6382=CIRCLE('',#28812,0.8);
#6383=CIRCLE('',#28815,0.8);
#6384=CIRCLE('',#28818,0.8);
#6385=CIRCLE('',#28821,0.8);
#6386=CIRCLE('',#28824,0.8);
#6387=CIRCLE('',#28827,0.8);
#6388=CIRCLE('',#28830,0.8);
#6389=CIRCLE('',#28833,0.8);
#6390=CIRCLE('',#28836,0.8);
#6391=CIRCLE('',#28839,0.8);
#6392=CIRCLE('',#28842,0.8);
#6393=CIRCLE('',#28845,0.8);
#6394=CIRCLE('',#28848,0.8);
#6395=CIRCLE('',#28851,0.8);
#6396=CIRCLE('',#28854,0.8);
#6397=CIRCLE('',#28857,0.8);
#6398=CIRCLE('',#28860,0.8);
#6399=CIRCLE('',#28863,0.8);
#6400=CIRCLE('',#28866,0.8);
#6401=CIRCLE('',#28869,0.8);
#6402=CIRCLE('',#28872,0.8);
#6403=CIRCLE('',#28874,0.8);
#6404=CIRCLE('',#28878,0.8);
#6405=CIRCLE('',#28881,0.8);
#6406=CIRCLE('',#28884,0.8);
#6407=CIRCLE('',#28887,0.8);
#6408=CIRCLE('',#28890,0.8);
#6409=CIRCLE('',#28893,0.8);
#6410=CIRCLE('',#28896,0.8);
#6411=CIRCLE('',#28899,0.8);
#6412=CIRCLE('',#28902,0.8);
#6413=CIRCLE('',#28905,0.8);
#6414=CIRCLE('',#28908,0.8);
#6415=CIRCLE('',#28911,0.8);
#6416=CIRCLE('',#28914,0.8);
#6417=CIRCLE('',#28917,0.8);
#6418=CIRCLE('',#28920,0.8);
#6419=CIRCLE('',#28923,0.8);
#6420=CIRCLE('',#28926,0.8);
#6421=CIRCLE('',#28929,0.8);
#6422=CIRCLE('',#28932,0.8);
#6423=CIRCLE('',#28934,0.45);
#6424=CIRCLE('',#28937,0.8);
#6425=CIRCLE('',#28939,0.8);
#6426=CIRCLE('',#28940,0.8);
#6427=CIRCLE('',#28941,0.8);
#6428=CIRCLE('',#28942,0.8);
#6429=CIRCLE('',#28943,0.8);
#6430=CIRCLE('',#28944,0.8);
#6431=CIRCLE('',#28945,0.8);
#6432=CIRCLE('',#28946,0.8);
#6433=CIRCLE('',#28947,0.8);
#6434=CIRCLE('',#28948,0.8);
#6435=CIRCLE('',#28949,0.8);
#6436=CIRCLE('',#28950,0.8);
#6437=CIRCLE('',#28951,0.8);
#6438=CIRCLE('',#28952,0.8);
#6439=CIRCLE('',#28953,0.8);
#6440=CIRCLE('',#28954,0.8);
#6441=CIRCLE('',#28955,0.8);
#6442=CIRCLE('',#28956,0.8);
#6443=CIRCLE('',#28957,0.8);
#6444=CIRCLE('',#28958,0.8);
#6445=CIRCLE('',#28959,0.8);
#6446=CIRCLE('',#28960,0.8);
#6447=CIRCLE('',#28961,0.8);
#6448=CIRCLE('',#28962,0.8);
#6449=CIRCLE('',#28963,0.8);
#6450=CIRCLE('',#28964,0.8);
#6451=CIRCLE('',#28965,0.8);
#6452=CIRCLE('',#28966,0.8);
#6453=CIRCLE('',#28967,0.8);
#6454=CIRCLE('',#28968,0.8);
#6455=CIRCLE('',#28969,0.8);
#6456=CIRCLE('',#28970,0.8);
#6457=CIRCLE('',#28971,0.8);
#6458=CIRCLE('',#28972,0.8);
#6459=CIRCLE('',#28973,0.8);
#6460=CIRCLE('',#28974,0.8);
#6461=CIRCLE('',#28976,0.75);
#6462=CIRCLE('',#28980,0.2942);
#6463=CIRCLE('',#29000,0.2942);
#6464=CIRCLE('',#29002,0.237175);
#6465=CIRCLE('',#29022,0.2942);
#6466=CIRCLE('',#29024,0.2942);
#6467=CIRCLE('',#29025,0.2942);
#6468=CIRCLE('',#29026,0.237175);
#6469=CIRCLE('',#29029,0.025);
#6470=CIRCLE('',#29030,0.3192);
#6471=CIRCLE('',#29031,0.2942);
#6472=CIRCLE('',#29034,0.47);
#6473=CIRCLE('',#29036,0.288675134594813);
#6474=CIRCLE('',#29038,0.288675134594813);
#6475=CIRCLE('',#29040,0.288675134594813);
#6476=CIRCLE('',#29042,0.288675134594813);
#6477=CIRCLE('',#29044,0.288675134594813);
#6478=CIRCLE('',#29046,0.288675134594813);
#6479=CIRCLE('',#29056,0.5);
#6480=CIRCLE('',#29059,0.5);
#6481=CIRCLE('',#29062,0.5);
#6482=CIRCLE('',#29065,0.5);
#6483=CIRCLE('',#29068,0.5);
#6484=CIRCLE('',#29071,0.5);
#6485=CIRCLE('',#29074,0.5);
#6486=CIRCLE('',#29077,0.5);
#6487=CIRCLE('',#29080,0.5);
#6488=CIRCLE('',#29083,0.5);
#6489=CIRCLE('',#29086,0.5);
#6490=CIRCLE('',#29089,0.5);
#6491=CIRCLE('',#29092,0.5);
#6492=CIRCLE('',#29095,0.5);
#6493=CIRCLE('',#29098,0.5);
#6494=CIRCLE('',#29101,0.5);
#6495=CIRCLE('',#29104,0.5);
#6496=CIRCLE('',#29105,0.5);
#6497=CIRCLE('',#29108,0.5);
#6498=CIRCLE('',#29109,0.5);
#6499=CIRCLE('',#29112,0.5);
#6500=CIRCLE('',#29115,0.5);
#6501=CIRCLE('',#29118,0.5);
#6502=CIRCLE('',#29121,0.5);
#6503=CIRCLE('',#29124,0.5);
#6504=CIRCLE('',#29127,0.5);
#6505=CIRCLE('',#29130,0.5);
#6506=CIRCLE('',#29133,0.5);
#6507=CIRCLE('',#29136,0.5);
#6508=CIRCLE('',#29139,0.5);
#6509=CIRCLE('',#29142,0.5);
#6510=CIRCLE('',#29145,0.5);
#6511=CIRCLE('',#29148,0.5);
#6512=CIRCLE('',#29151,0.5);
#6513=CIRCLE('',#29154,0.5);
#6514=CIRCLE('',#29157,0.5);
#6515=CIRCLE('',#29160,0.5);
#6516=CIRCLE('',#29163,0.5);
#6517=CIRCLE('',#29166,0.5);
#6518=CIRCLE('',#29169,0.5);
#6519=CIRCLE('',#29172,0.5);
#6520=CIRCLE('',#29175,0.5);
#6521=CIRCLE('',#29178,0.5);
#6522=CIRCLE('',#29181,0.5);
#6523=CIRCLE('',#29184,0.5);
#6524=CIRCLE('',#29187,0.5);
#6525=CIRCLE('',#29190,0.5);
#6526=CIRCLE('',#29193,0.5);
#6527=CIRCLE('',#29196,0.5);
#6528=CIRCLE('',#29199,0.5);
#6529=CIRCLE('',#29202,0.5);
#6530=CIRCLE('',#29205,0.5);
#6531=CIRCLE('',#29208,0.5);
#6532=CIRCLE('',#29211,0.5);
#6533=CIRCLE('',#29213,0.5);
#6534=CIRCLE('',#29217,0.5);
#6535=CIRCLE('',#29220,0.5);
#6536=CIRCLE('',#29223,0.5);
#6537=CIRCLE('',#29226,0.5);
#6538=CIRCLE('',#29229,0.5);
#6539=CIRCLE('',#29232,0.5);
#6540=CIRCLE('',#29235,0.5);
#6541=CIRCLE('',#29238,0.5);
#6542=CIRCLE('',#29241,0.5);
#6543=CIRCLE('',#29244,0.5);
#6544=CIRCLE('',#29247,0.5);
#6545=CIRCLE('',#29250,0.5);
#6546=CIRCLE('',#29253,0.5);
#6547=CIRCLE('',#29256,0.5);
#6548=CIRCLE('',#29259,0.5);
#6549=CIRCLE('',#29262,0.5);
#6550=CIRCLE('',#29265,0.5);
#6551=CIRCLE('',#29268,0.5);
#6552=CIRCLE('',#29271,0.5);
#6553=CIRCLE('',#29273,0.25);
#6554=CIRCLE('',#29276,0.5);
#6555=CIRCLE('',#29278,0.5);
#6556=CIRCLE('',#29279,0.5);
#6557=CIRCLE('',#29280,0.5);
#6558=CIRCLE('',#29281,0.5);
#6559=CIRCLE('',#29282,0.5);
#6560=CIRCLE('',#29283,0.5);
#6561=CIRCLE('',#29284,0.5);
#6562=CIRCLE('',#29285,0.5);
#6563=CIRCLE('',#29286,0.5);
#6564=CIRCLE('',#29287,0.5);
#6565=CIRCLE('',#29288,0.5);
#6566=CIRCLE('',#29289,0.5);
#6567=CIRCLE('',#29290,0.5);
#6568=CIRCLE('',#29291,0.5);
#6569=CIRCLE('',#29292,0.5);
#6570=CIRCLE('',#29293,0.5);
#6571=CIRCLE('',#29294,0.5);
#6572=CIRCLE('',#29295,0.5);
#6573=CIRCLE('',#29296,0.5);
#6574=CIRCLE('',#29297,0.5);
#6575=CIRCLE('',#29298,0.5);
#6576=CIRCLE('',#29299,0.5);
#6577=CIRCLE('',#29300,0.5);
#6578=CIRCLE('',#29301,0.5);
#6579=CIRCLE('',#29302,0.5);
#6580=CIRCLE('',#29303,0.5);
#6581=CIRCLE('',#29304,0.5);
#6582=CIRCLE('',#29305,0.5);
#6583=CIRCLE('',#29306,0.5);
#6584=CIRCLE('',#29307,0.5);
#6585=CIRCLE('',#29308,0.5);
#6586=CIRCLE('',#29309,0.5);
#6587=CIRCLE('',#29310,0.5);
#6588=CIRCLE('',#29311,0.5);
#6589=CIRCLE('',#29312,0.5);
#6590=CIRCLE('',#29313,0.5);
#6591=CIRCLE('',#29315,0.45);
#6592=LINE('',#36386,#8748);
#6593=LINE('',#36390,#8749);
#6594=LINE('',#36395,#8750);
#6595=LINE('',#36396,#8751);
#6596=LINE('',#36397,#8752);
#6597=LINE('',#36401,#8753);
#6598=LINE('',#36407,#8754);
#6599=LINE('',#36408,#8755);
#6600=LINE('',#36409,#8756);
#6601=LINE('',#36413,#8757);
#6602=LINE('',#36419,#8758);
#6603=LINE('',#36420,#8759);
#6604=LINE('',#36421,#8760);
#6605=LINE('',#36425,#8761);
#6606=LINE('',#36429,#8762);
#6607=LINE('',#36430,#8763);
#6608=LINE('',#36433,#8764);
#6609=LINE('',#36435,#8765);
#6610=LINE('',#36436,#8766);
#6611=LINE('',#36439,#8767);
#6612=LINE('',#36443,#8768);
#6613=LINE('',#36444,#8769);
#6614=LINE('',#36447,#8770);
#6615=LINE('',#36454,#8771);
#6616=LINE('',#36458,#8772);
#6617=LINE('',#36462,#8773);
#6618=LINE('',#36465,#8774);
#6619=LINE('',#36470,#8775);
#6620=LINE('',#36477,#8776);
#6621=LINE('',#36481,#8777);
#6622=LINE('',#36485,#8778);
#6623=LINE('',#36488,#8779);
#6624=LINE('',#36497,#8780);
#6625=LINE('',#36499,#8781);
#6626=LINE('',#36501,#8782);
#6627=LINE('',#36502,#8783);
#6628=LINE('',#36508,#8784);
#6629=LINE('',#36511,#8785);
#6630=LINE('',#36516,#8786);
#6631=LINE('',#36519,#8787);
#6632=LINE('',#36524,#8788);
#6633=LINE('',#36527,#8789);
#6634=LINE('',#36532,#8790);
#6635=LINE('',#36535,#8791);
#6636=LINE('',#36537,#8792);
#6637=LINE('',#36538,#8793);
#6638=LINE('',#36541,#8794);
#6639=LINE('',#36543,#8795);
#6640=LINE('',#36544,#8796);
#6641=LINE('',#36546,#8797);
#6642=LINE('',#36548,#8798);
#6643=LINE('',#36551,#8799);
#6644=LINE('',#36553,#8800);
#6645=LINE('',#36554,#8801);
#6646=LINE('',#36557,#8802);
#6647=LINE('',#36558,#8803);
#6648=LINE('',#36564,#8804);
#6649=LINE('',#36565,#8805);
#6650=LINE('',#36567,#8806);
#6651=LINE('',#36568,#8807);
#6652=LINE('',#36572,#8808);
#6653=LINE('',#36578,#8809);
#6654=LINE('',#36579,#8810);
#6655=LINE('',#36580,#8811);
#6656=LINE('',#36584,#8812);
#6657=LINE('',#36592,#8813);
#6658=LINE('',#36593,#8814);
#6659=LINE('',#36594,#8815);
#6660=LINE('',#36595,#8816);
#6661=LINE('',#36598,#8817);
#6662=LINE('',#36602,#8818);
#6663=LINE('',#36603,#8819);
#6664=LINE('',#36608,#8820);
#6665=LINE('',#36610,#8821);
#6666=LINE('',#36611,#8822);
#6667=LINE('',#36617,#8823);
#6668=LINE('',#36621,#8824);
#6669=LINE('',#36622,#8825);
#6670=LINE('',#36625,#8826);
#6671=LINE('',#36632,#8827);
#6672=LINE('',#36633,#8828);
#6673=LINE('',#36636,#8829);
#6674=LINE('',#36645,#8830);
#6675=LINE('',#36647,#8831);
#6676=LINE('',#36649,#8832);
#6677=LINE('',#36651,#8833);
#6678=LINE('',#36652,#8834);
#6679=LINE('',#36655,#8835);
#6680=LINE('',#36657,#8836);
#6681=LINE('',#36658,#8837);
#6682=LINE('',#36661,#8838);
#6683=LINE('',#36663,#8839);
#6684=LINE('',#36665,#8840);
#6685=LINE('',#36666,#8841);
#6686=LINE('',#36669,#8842);
#6687=LINE('',#36671,#8843);
#6688=LINE('',#36673,#8844);
#6689=LINE('',#36675,#8845);
#6690=LINE('',#36676,#8846);
#6691=LINE('',#36679,#8847);
#6692=LINE('',#36681,#8848);
#6693=LINE('',#36683,#8849);
#6694=LINE('',#36684,#8850);
#6695=LINE('',#36687,#8851);
#6696=LINE('',#36689,#8852);
#6697=LINE('',#36691,#8853);
#6698=LINE('',#36692,#8854);
#6699=LINE('',#36695,#8855);
#6700=LINE('',#36697,#8856);
#6701=LINE('',#36698,#8857);
#6702=LINE('',#36701,#8858);
#6703=LINE('',#36703,#8859);
#6704=LINE('',#36704,#8860);
#6705=LINE('',#36707,#8861);
#6706=LINE('',#36709,#8862);
#6707=LINE('',#36710,#8863);
#6708=LINE('',#36713,#8864);
#6709=LINE('',#36714,#8865);
#6710=LINE('',#36717,#8866);
#6711=LINE('',#36720,#8867);
#6712=LINE('',#36723,#8868);
#6713=LINE('',#36724,#8869);
#6714=LINE('',#36727,#8870);
#6715=LINE('',#36731,#8871);
#6716=LINE('',#36732,#8872);
#6717=LINE('',#36735,#8873);
#6718=LINE('',#36739,#8874);
#6719=LINE('',#36740,#8875);
#6720=LINE('',#36743,#8876);
#6721=LINE('',#36746,#8877);
#6722=LINE('',#36749,#8878);
#6723=LINE('',#36751,#8879);
#6724=LINE('',#36752,#8880);
#6725=LINE('',#36755,#8881);
#6726=LINE('',#36759,#8882);
#6727=LINE('',#36760,#8883);
#6728=LINE('',#36763,#8884);
#6729=LINE('',#36767,#8885);
#6730=LINE('',#36769,#8886);
#6731=LINE('',#36770,#8887);
#6732=LINE('',#36774,#8888);
#6733=LINE('',#36782,#8889);
#6734=LINE('',#36784,#8890);
#6735=LINE('',#36785,#8891);
#6736=LINE('',#36786,#8892);
#6737=LINE('',#36789,#8893);
#6738=LINE('',#36793,#8894);
#6739=LINE('',#36794,#8895);
#6740=LINE('',#36797,#8896);
#6741=LINE('',#36801,#8897);
#6742=LINE('',#36802,#8898);
#6743=LINE('',#36803,#8899);
#6744=LINE('',#36808,#8900);
#6745=LINE('',#36810,#8901);
#6746=LINE('',#36811,#8902);
#6747=LINE('',#36816,#8903);
#6748=LINE('',#36820,#8904);
#6749=LINE('',#36822,#8905);
#6750=LINE('',#36824,#8906);
#6751=LINE('',#36825,#8907);
#6752=LINE('',#36828,#8908);
#6753=LINE('',#36832,#8909);
#6754=LINE('',#36833,#8910);
#6755=LINE('',#36836,#8911);
#6756=LINE('',#36841,#8912);
#6757=LINE('',#36842,#8913);
#6758=LINE('',#36847,#8914);
#6759=LINE('',#36848,#8915);
#6760=LINE('',#36851,#8916);
#6761=LINE('',#36855,#8917);
#6762=LINE('',#36856,#8918);
#6763=LINE('',#36862,#8919);
#6764=LINE('',#36864,#8920);
#6765=LINE('',#36865,#8921);
#6766=LINE('',#36869,#8922);
#6767=LINE('',#36871,#8923);
#6768=LINE('',#36872,#8924);
#6769=LINE('',#36876,#8925);
#6770=LINE('',#36877,#8926);
#6771=LINE('',#36878,#8927);
#6772=LINE('',#36882,#8928);
#6773=LINE('',#36888,#8929);
#6774=LINE('',#36889,#8930);
#6775=LINE('',#36890,#8931);
#6776=LINE('',#36894,#8932);
#6777=LINE('',#36898,#8933);
#6778=LINE('',#36899,#8934);
#6779=LINE('',#36901,#8935);
#6780=LINE('',#36902,#8936);
#6781=LINE('',#36906,#8937);
#6782=LINE('',#36907,#8938);
#6783=LINE('',#36909,#8939);
#6784=LINE('',#36910,#8940);
#6785=LINE('',#36914,#8941);
#6786=LINE('',#36915,#8942);
#6787=LINE('',#36917,#8943);
#6788=LINE('',#36918,#8944);
#6789=LINE('',#36921,#8945);
#6790=LINE('',#36922,#8946);
#6791=LINE('',#36924,#8947);
#6792=LINE('',#36927,#8948);
#6793=LINE('',#36928,#8949);
#6794=LINE('',#36931,#8950);
#6795=LINE('',#36935,#8951);
#6796=LINE('',#36936,#8952);
#6797=LINE('',#36939,#8953);
#6798=LINE('',#36943,#8954);
#6799=LINE('',#36945,#8955);
#6800=LINE('',#36946,#8956);
#6801=LINE('',#36948,#8957);
#6802=LINE('',#36949,#8958);
#6803=LINE('',#36951,#8959);
#6804=LINE('',#36953,#8960);
#6805=LINE('',#36954,#8961);
#6806=LINE('',#36956,#8962);
#6807=LINE('',#36957,#8963);
#6808=LINE('',#36959,#8964);
#6809=LINE('',#36961,#8965);
#6810=LINE('',#36964,#8966);
#6811=LINE('',#36966,#8967);
#6812=LINE('',#36994,#8968);
#6813=LINE('',#36996,#8969);
#6814=LINE('',#36998,#8970);
#6815=LINE('',#37001,#8971);
#6816=LINE('',#37003,#8972);
#6817=LINE('',#37005,#8973);
#6818=LINE('',#37008,#8974);
#6819=LINE('',#37010,#8975);
#6820=LINE('',#37012,#8976);
#6821=LINE('',#37016,#8977);
#6822=LINE('',#37018,#8978);
#6823=LINE('',#37021,#8979);
#6824=LINE('',#37024,#8980);
#6825=LINE('',#37027,#8981);
#6826=LINE('',#37030,#8982);
#6827=LINE('',#37033,#8983);
#6828=LINE('',#37034,#8984);
#6829=LINE('',#37036,#8985);
#6830=LINE('',#37044,#8986);
#6831=LINE('',#37050,#8987);
#6832=LINE('',#37059,#8988);
#6833=LINE('',#37065,#8989);
#6834=LINE('',#37147,#8990);
#6835=LINE('',#37158,#8991);
#6836=LINE('',#37191,#8992);
#6837=LINE('',#37196,#8993);
#6838=LINE('',#37202,#8994);
#6839=LINE('',#37206,#8995);
#6840=LINE('',#37208,#8996);
#6841=LINE('',#37210,#8997);
#6842=LINE('',#37212,#8998);
#6843=LINE('',#37214,#8999);
#6844=LINE('',#37215,#9000);
#6845=LINE('',#37218,#9001);
#6846=LINE('',#37227,#9002);
#6847=LINE('',#37235,#9003);
#6848=LINE('',#37238,#9004);
#6849=LINE('',#37242,#9005);
#6850=LINE('',#37246,#9006);
#6851=LINE('',#37250,#9007);
#6852=LINE('',#37254,#9008);
#6853=LINE('',#37256,#9009);
#6854=LINE('',#37257,#9010);
#6855=LINE('',#37260,#9011);
#6856=LINE('',#37262,#9012);
#6857=LINE('',#37263,#9013);
#6858=LINE('',#37268,#9014);
#6859=LINE('',#37272,#9015);
#6860=LINE('',#37471,#9016);
#6861=LINE('',#37578,#9017);
#6862=LINE('',#37581,#9018);
#6863=LINE('',#37627,#9019);
#6864=LINE('',#37653,#9020);
#6865=LINE('',#37656,#9021);
#6866=LINE('',#37660,#9022);
#6867=LINE('',#37662,#9023);
#6868=LINE('',#37664,#9024);
#6869=LINE('',#37665,#9025);
#6870=LINE('',#37668,#9026);
#6871=LINE('',#37670,#9027);
#6872=LINE('',#37671,#9028);
#6873=LINE('',#37676,#9029);
#6874=LINE('',#37810,#9030);
#6875=LINE('',#37943,#9031);
#6876=LINE('',#37970,#9032);
#6877=LINE('',#37978,#9033);
#6878=LINE('',#37980,#9034);
#6879=LINE('',#37981,#9035);
#6880=LINE('',#37984,#9036);
#6881=LINE('',#37986,#9037);
#6882=LINE('',#37987,#9038);
#6883=LINE('',#37991,#9039);
#6884=LINE('',#37993,#9040);
#6885=LINE('',#37994,#9041);
#6886=LINE('',#37997,#9042);
#6887=LINE('',#37999,#9043);
#6888=LINE('',#38000,#9044);
#6889=LINE('',#38004,#9045);
#6890=LINE('',#38006,#9046);
#6891=LINE('',#38007,#9047);
#6892=LINE('',#38011,#9048);
#6893=LINE('',#38012,#9049);
#6894=LINE('',#38013,#9050);
#6895=LINE('',#38017,#9051);
#6896=LINE('',#38023,#9052);
#6897=LINE('',#38024,#9053);
#6898=LINE('',#38025,#9054);
#6899=LINE('',#38029,#9055);
#6900=LINE('',#38033,#9056);
#6901=LINE('',#38034,#9057);
#6902=LINE('',#38037,#9058);
#6903=LINE('',#38039,#9059);
#6904=LINE('',#38040,#9060);
#6905=LINE('',#38042,#9061);
#6906=LINE('',#38043,#9062);
#6907=LINE('',#38045,#9063);
#6908=LINE('',#38046,#9064);
#6909=LINE('',#38048,#9065);
#6910=LINE('',#38049,#9066);
#6911=LINE('',#38053,#9067);
#6912=LINE('',#38056,#9068);
#6913=LINE('',#38104,#9069);
#6914=LINE('',#38132,#9070);
#6915=LINE('',#38134,#9071);
#6916=LINE('',#38135,#9072);
#6917=LINE('',#38138,#9073);
#6918=LINE('',#38198,#9074);
#6919=LINE('',#38200,#9075);
#6920=LINE('',#38202,#9076);
#6921=LINE('',#38204,#9077);
#6922=LINE('',#38206,#9078);
#6923=LINE('',#38210,#9079);
#6924=LINE('',#38212,#9080);
#6925=LINE('',#38213,#9081);
#6926=LINE('',#38216,#9082);
#6927=LINE('',#38220,#9083);
#6928=LINE('',#38221,#9084);
#6929=LINE('',#38224,#9085);
#6930=LINE('',#38226,#9086);
#6931=LINE('',#38231,#9087);
#6932=LINE('',#38235,#9088);
#6933=LINE('',#38239,#9089);
#6934=LINE('',#38243,#9090);
#6935=LINE('',#38247,#9091);
#6936=LINE('',#38249,#9092);
#6937=LINE('',#38250,#9093);
#6938=LINE('',#38253,#9094);
#6939=LINE('',#38257,#9095);
#6940=LINE('',#38258,#9096);
#6941=LINE('',#38263,#9097);
#6942=LINE('',#38266,#9098);
#6943=LINE('',#38269,#9099);
#6944=LINE('',#38270,#9100);
#6945=LINE('',#38273,#9101);
#6946=LINE('',#38275,#9102);
#6947=LINE('',#38276,#9103);
#6948=LINE('',#38279,#9104);
#6949=LINE('',#38283,#9105);
#6950=LINE('',#38284,#9106);
#6951=LINE('',#38289,#9107);
#6952=LINE('',#38292,#9108);
#6953=LINE('',#38295,#9109);
#6954=LINE('',#38296,#9110);
#6955=LINE('',#38299,#9111);
#6956=LINE('',#38301,#9112);
#6957=LINE('',#38302,#9113);
#6958=LINE('',#38305,#9114);
#6959=LINE('',#38309,#9115);
#6960=LINE('',#38310,#9116);
#6961=LINE('',#38315,#9117);
#6962=LINE('',#38318,#9118);
#6963=LINE('',#38321,#9119);
#6964=LINE('',#38322,#9120);
#6965=LINE('',#38325,#9121);
#6966=LINE('',#38327,#9122);
#6967=LINE('',#38328,#9123);
#6968=LINE('',#38331,#9124);
#6969=LINE('',#38335,#9125);
#6970=LINE('',#38336,#9126);
#6971=LINE('',#38341,#9127);
#6972=LINE('',#38344,#9128);
#6973=LINE('',#38347,#9129);
#6974=LINE('',#38348,#9130);
#6975=LINE('',#38353,#9131);
#6976=LINE('',#38361,#9132);
#6977=LINE('',#38366,#9133);
#6978=LINE('',#38372,#9134);
#6979=LINE('',#38375,#9135);
#6980=LINE('',#38377,#9136);
#6981=LINE('',#38378,#9137);
#6982=LINE('',#38382,#9138);
#6983=LINE('',#38387,#9139);
#6984=LINE('',#38388,#9140);
#6985=LINE('',#38389,#9141);
#6986=LINE('',#38393,#9142);
#6987=LINE('',#38402,#9143);
#6988=LINE('',#38404,#9144);
#6989=LINE('',#38406,#9145);
#6990=LINE('',#38408,#9146);
#6991=LINE('',#38410,#9147);
#6992=LINE('',#38412,#9148);
#6993=LINE('',#38414,#9149);
#6994=LINE('',#38415,#9150);
#6995=LINE('',#38417,#9151);
#6996=LINE('',#38419,#9152);
#6997=LINE('',#38421,#9153);
#6998=LINE('',#38430,#9154);
#6999=LINE('',#38434,#9155);
#7000=LINE('',#38438,#9156);
#7001=LINE('',#38442,#9157);
#7002=LINE('',#38446,#9158);
#7003=LINE('',#38450,#9159);
#7004=LINE('',#38454,#9160);
#7005=LINE('',#38458,#9161);
#7006=LINE('',#38462,#9162);
#7007=LINE('',#38465,#9163);
#7008=LINE('',#38466,#9164);
#7009=LINE('',#38469,#9165);
#7010=LINE('',#38472,#9166);
#7011=LINE('',#38473,#9167);
#7012=LINE('',#38476,#9168);
#7013=LINE('',#38478,#9169);
#7014=LINE('',#38479,#9170);
#7015=LINE('',#38482,#9171);
#7016=LINE('',#38485,#9172);
#7017=LINE('',#38486,#9173);
#7018=LINE('',#38489,#9174);
#7019=LINE('',#38491,#9175);
#7020=LINE('',#38492,#9176);
#7021=LINE('',#38495,#9177);
#7022=LINE('',#38498,#9178);
#7023=LINE('',#38499,#9179);
#7024=LINE('',#38502,#9180);
#7025=LINE('',#38758,#9181);
#7026=LINE('',#38768,#9182);
#7027=LINE('',#38770,#9183);
#7028=LINE('',#38774,#9184);
#7029=LINE('',#38775,#9185);
#7030=LINE('',#38778,#9186);
#7031=LINE('',#38782,#9187);
#7032=LINE('',#38783,#9188);
#7033=LINE('',#38785,#9189);
#7034=LINE('',#38788,#9190);
#7035=LINE('',#38790,#9191);
#7036=LINE('',#38861,#9192);
#7037=LINE('',#38881,#9193);
#7038=LINE('',#38883,#9194);
#7039=LINE('',#38885,#9195);
#7040=LINE('',#38887,#9196);
#7041=LINE('',#38890,#9197);
#7042=LINE('',#38892,#9198);
#7043=LINE('',#38901,#9199);
#7044=LINE('',#38985,#9200);
#7045=LINE('',#39008,#9201);
#7046=LINE('',#39079,#9202);
#7047=LINE('',#39080,#9203);
#7048=LINE('',#39083,#9204);
#7049=LINE('',#39086,#9205);
#7050=LINE('',#39089,#9206);
#7051=LINE('',#39091,#9207);
#7052=LINE('',#39144,#9208);
#7053=LINE('',#39157,#9209);
#7054=LINE('',#39207,#9210);
#7055=LINE('',#39312,#9211);
#7056=LINE('',#39331,#9212);
#7057=LINE('',#39334,#9213);
#7058=LINE('',#39337,#9214);
#7059=LINE('',#39340,#9215);
#7060=LINE('',#39346,#9216);
#7061=LINE('',#39424,#9217);
#7062=LINE('',#39430,#9218);
#7063=LINE('',#39434,#9219);
#7064=LINE('',#39441,#9220);
#7065=LINE('',#39447,#9221);
#7066=LINE('',#39455,#9222);
#7067=LINE('',#39457,#9223);
#7068=LINE('',#39459,#9224);
#7069=LINE('',#39460,#9225);
#7070=LINE('',#39465,#9226);
#7071=LINE('',#39466,#9227);
#7072=LINE('',#39469,#9228);
#7073=LINE('',#39471,#9229);
#7074=LINE('',#39472,#9230);
#7075=LINE('',#39475,#9231);
#7076=LINE('',#39480,#9232);
#7077=LINE('',#39482,#9233);
#7078=LINE('',#39484,#9234);
#7079=LINE('',#39485,#9235);
#7080=LINE('',#39490,#9236);
#7081=LINE('',#39491,#9237);
#7082=LINE('',#39494,#9238);
#7083=LINE('',#39496,#9239);
#7084=LINE('',#39497,#9240);
#7085=LINE('',#39500,#9241);
#7086=LINE('',#39505,#9242);
#7087=LINE('',#39507,#9243);
#7088=LINE('',#39509,#9244);
#7089=LINE('',#39510,#9245);
#7090=LINE('',#39515,#9246);
#7091=LINE('',#39516,#9247);
#7092=LINE('',#39519,#9248);
#7093=LINE('',#39521,#9249);
#7094=LINE('',#39522,#9250);
#7095=LINE('',#39525,#9251);
#7096=LINE('',#39530,#9252);
#7097=LINE('',#39532,#9253);
#7098=LINE('',#39534,#9254);
#7099=LINE('',#39535,#9255);
#7100=LINE('',#39540,#9256);
#7101=LINE('',#39541,#9257);
#7102=LINE('',#39544,#9258);
#7103=LINE('',#39546,#9259);
#7104=LINE('',#39547,#9260);
#7105=LINE('',#39550,#9261);
#7106=LINE('',#39555,#9262);
#7107=LINE('',#39557,#9263);
#7108=LINE('',#39559,#9264);
#7109=LINE('',#39560,#9265);
#7110=LINE('',#39565,#9266);
#7111=LINE('',#39566,#9267);
#7112=LINE('',#39569,#9268);
#7113=LINE('',#39571,#9269);
#7114=LINE('',#39572,#9270);
#7115=LINE('',#39575,#9271);
#7116=LINE('',#39580,#9272);
#7117=LINE('',#39582,#9273);
#7118=LINE('',#39584,#9274);
#7119=LINE('',#39585,#9275);
#7120=LINE('',#39590,#9276);
#7121=LINE('',#39591,#9277);
#7122=LINE('',#39594,#9278);
#7123=LINE('',#39596,#9279);
#7124=LINE('',#39597,#9280);
#7125=LINE('',#39600,#9281);
#7126=LINE('',#39605,#9282);
#7127=LINE('',#39607,#9283);
#7128=LINE('',#39609,#9284);
#7129=LINE('',#39610,#9285);
#7130=LINE('',#39615,#9286);
#7131=LINE('',#39616,#9287);
#7132=LINE('',#39619,#9288);
#7133=LINE('',#39621,#9289);
#7134=LINE('',#39622,#9290);
#7135=LINE('',#39625,#9291);
#7136=LINE('',#39630,#9292);
#7137=LINE('',#39632,#9293);
#7138=LINE('',#39634,#9294);
#7139=LINE('',#39635,#9295);
#7140=LINE('',#39640,#9296);
#7141=LINE('',#39641,#9297);
#7142=LINE('',#39644,#9298);
#7143=LINE('',#39646,#9299);
#7144=LINE('',#39647,#9300);
#7145=LINE('',#39650,#9301);
#7146=LINE('',#39655,#9302);
#7147=LINE('',#39657,#9303);
#7148=LINE('',#39659,#9304);
#7149=LINE('',#39660,#9305);
#7150=LINE('',#39665,#9306);
#7151=LINE('',#39666,#9307);
#7152=LINE('',#39669,#9308);
#7153=LINE('',#39671,#9309);
#7154=LINE('',#39672,#9310);
#7155=LINE('',#39675,#9311);
#7156=LINE('',#39680,#9312);
#7157=LINE('',#39682,#9313);
#7158=LINE('',#39684,#9314);
#7159=LINE('',#39685,#9315);
#7160=LINE('',#39690,#9316);
#7161=LINE('',#39691,#9317);
#7162=LINE('',#39694,#9318);
#7163=LINE('',#39696,#9319);
#7164=LINE('',#39697,#9320);
#7165=LINE('',#39700,#9321);
#7166=LINE('',#39705,#9322);
#7167=LINE('',#39707,#9323);
#7168=LINE('',#39709,#9324);
#7169=LINE('',#39710,#9325);
#7170=LINE('',#39715,#9326);
#7171=LINE('',#39716,#9327);
#7172=LINE('',#39719,#9328);
#7173=LINE('',#39721,#9329);
#7174=LINE('',#39722,#9330);
#7175=LINE('',#39725,#9331);
#7176=LINE('',#39730,#9332);
#7177=LINE('',#39732,#9333);
#7178=LINE('',#39734,#9334);
#7179=LINE('',#39735,#9335);
#7180=LINE('',#39740,#9336);
#7181=LINE('',#39741,#9337);
#7182=LINE('',#39744,#9338);
#7183=LINE('',#39746,#9339);
#7184=LINE('',#39747,#9340);
#7185=LINE('',#39750,#9341);
#7186=LINE('',#39755,#9342);
#7187=LINE('',#39757,#9343);
#7188=LINE('',#39759,#9344);
#7189=LINE('',#39760,#9345);
#7190=LINE('',#39765,#9346);
#7191=LINE('',#39766,#9347);
#7192=LINE('',#39769,#9348);
#7193=LINE('',#39771,#9349);
#7194=LINE('',#39772,#9350);
#7195=LINE('',#39775,#9351);
#7196=LINE('',#39780,#9352);
#7197=LINE('',#39782,#9353);
#7198=LINE('',#39784,#9354);
#7199=LINE('',#39785,#9355);
#7200=LINE('',#39790,#9356);
#7201=LINE('',#39791,#9357);
#7202=LINE('',#39794,#9358);
#7203=LINE('',#39796,#9359);
#7204=LINE('',#39797,#9360);
#7205=LINE('',#39800,#9361);
#7206=LINE('',#39805,#9362);
#7207=LINE('',#39807,#9363);
#7208=LINE('',#39809,#9364);
#7209=LINE('',#39810,#9365);
#7210=LINE('',#39815,#9366);
#7211=LINE('',#39816,#9367);
#7212=LINE('',#39819,#9368);
#7213=LINE('',#39821,#9369);
#7214=LINE('',#39822,#9370);
#7215=LINE('',#39825,#9371);
#7216=LINE('',#39830,#9372);
#7217=LINE('',#39832,#9373);
#7218=LINE('',#39834,#9374);
#7219=LINE('',#39835,#9375);
#7220=LINE('',#39840,#9376);
#7221=LINE('',#39841,#9377);
#7222=LINE('',#39844,#9378);
#7223=LINE('',#39846,#9379);
#7224=LINE('',#39847,#9380);
#7225=LINE('',#39850,#9381);
#7226=LINE('',#39855,#9382);
#7227=LINE('',#39857,#9383);
#7228=LINE('',#39859,#9384);
#7229=LINE('',#39860,#9385);
#7230=LINE('',#39865,#9386);
#7231=LINE('',#39866,#9387);
#7232=LINE('',#39869,#9388);
#7233=LINE('',#39871,#9389);
#7234=LINE('',#39872,#9390);
#7235=LINE('',#39875,#9391);
#7236=LINE('',#39880,#9392);
#7237=LINE('',#39882,#9393);
#7238=LINE('',#39884,#9394);
#7239=LINE('',#39885,#9395);
#7240=LINE('',#39890,#9396);
#7241=LINE('',#39891,#9397);
#7242=LINE('',#39894,#9398);
#7243=LINE('',#39896,#9399);
#7244=LINE('',#39897,#9400);
#7245=LINE('',#39900,#9401);
#7246=LINE('',#39905,#9402);
#7247=LINE('',#39907,#9403);
#7248=LINE('',#39909,#9404);
#7249=LINE('',#39910,#9405);
#7250=LINE('',#39915,#9406);
#7251=LINE('',#39916,#9407);
#7252=LINE('',#39919,#9408);
#7253=LINE('',#39921,#9409);
#7254=LINE('',#39922,#9410);
#7255=LINE('',#39925,#9411);
#7256=LINE('',#39930,#9412);
#7257=LINE('',#39932,#9413);
#7258=LINE('',#39934,#9414);
#7259=LINE('',#39935,#9415);
#7260=LINE('',#39940,#9416);
#7261=LINE('',#39941,#9417);
#7262=LINE('',#39944,#9418);
#7263=LINE('',#39946,#9419);
#7264=LINE('',#39947,#9420);
#7265=LINE('',#39950,#9421);
#7266=LINE('',#39955,#9422);
#7267=LINE('',#39957,#9423);
#7268=LINE('',#39959,#9424);
#7269=LINE('',#39960,#9425);
#7270=LINE('',#39965,#9426);
#7271=LINE('',#39966,#9427);
#7272=LINE('',#39969,#9428);
#7273=LINE('',#39971,#9429);
#7274=LINE('',#39972,#9430);
#7275=LINE('',#39975,#9431);
#7276=LINE('',#39980,#9432);
#7277=LINE('',#39982,#9433);
#7278=LINE('',#39984,#9434);
#7279=LINE('',#39985,#9435);
#7280=LINE('',#40008,#9436);
#7281=LINE('',#40011,#9437);
#7282=LINE('',#40013,#9438);
#7283=LINE('',#40014,#9439);
#7284=LINE('',#40040,#9440);
#7285=LINE('',#40048,#9441);
#7286=LINE('',#40050,#9442);
#7287=LINE('',#40053,#9443);
#7288=LINE('',#40057,#9444);
#7289=LINE('',#40064,#9445);
#7290=LINE('',#40074,#9446);
#7291=LINE('',#40080,#9447);
#7292=LINE('',#40084,#9448);
#7293=LINE('',#40091,#9449);
#7294=LINE('',#40093,#9450);
#7295=LINE('',#40098,#9451);
#7296=LINE('',#40131,#9452);
#7297=LINE('',#40215,#9453);
#7298=LINE('',#40302,#9454);
#7299=LINE('',#40386,#9455);
#7300=LINE('',#40458,#9456);
#7301=LINE('',#40527,#9457);
#7302=LINE('',#40611,#9458);
#7303=LINE('',#40695,#9459);
#7304=LINE('',#40782,#9460);
#7305=LINE('',#40866,#9461);
#7306=LINE('',#40953,#9462);
#7307=LINE('',#41037,#9463);
#7308=LINE('',#41121,#9464);
#7309=LINE('',#41208,#9465);
#7310=LINE('',#41277,#9466);
#7311=LINE('',#41349,#9467);
#7312=LINE('',#41430,#9468);
#7313=LINE('',#41517,#9469);
#7314=LINE('',#41604,#9470);
#7315=LINE('',#41688,#9471);
#7316=LINE('',#41775,#9472);
#7317=LINE('',#41847,#9473);
#7318=LINE('',#41937,#9474);
#7319=LINE('',#42021,#9475);
#7320=LINE('',#42105,#9476);
#7321=LINE('',#42192,#9477);
#7322=LINE('',#42273,#9478);
#7323=LINE('',#42345,#9479);
#7324=LINE('',#42414,#9480);
#7325=LINE('',#42498,#9481);
#7326=LINE('',#42582,#9482);
#7327=LINE('',#42666,#9483);
#7328=LINE('',#42756,#9484);
#7329=LINE('',#42840,#9485);
#7330=LINE('',#42924,#9486);
#7331=LINE('',#43008,#9487);
#7332=LINE('',#43092,#9488);
#7333=LINE('',#43161,#9489);
#7334=LINE('',#43245,#9490);
#7335=LINE('',#43332,#9491);
#7336=LINE('',#43416,#9492);
#7337=LINE('',#43500,#9493);
#7338=LINE('',#43522,#9494);
#7339=LINE('',#43557,#9495);
#7340=LINE('',#43594,#9496);
#7341=LINE('',#43630,#9497);
#7342=LINE('',#43666,#9498);
#7343=LINE('',#43712,#9499);
#7344=LINE('',#43747,#9500);
#7345=LINE('',#43784,#9501);
#7346=LINE('',#43819,#9502);
#7347=LINE('',#43856,#9503);
#7348=LINE('',#43893,#9504);
#7349=LINE('',#43929,#9505);
#7350=LINE('',#43966,#9506);
#7351=LINE('',#44001,#9507);
#7352=LINE('',#44038,#9508);
#7353=LINE('',#44083,#9509);
#7354=LINE('',#44119,#9510);
#7355=LINE('',#44155,#9511);
#7356=LINE('',#44191,#9512);
#7357=LINE('',#44228,#9513);
#7358=LINE('',#44265,#9514);
#7359=LINE('',#44300,#9515);
#7360=LINE('',#44334,#9516);
#7361=LINE('',#44371,#9517);
#7362=LINE('',#44407,#9518);
#7363=LINE('',#44444,#9519);
#7364=LINE('',#44480,#9520);
#7365=LINE('',#44516,#9521);
#7366=LINE('',#44552,#9522);
#7367=LINE('',#44588,#9523);
#7368=LINE('',#44625,#9524);
#7369=LINE('',#44660,#9525);
#7370=LINE('',#44697,#9526);
#7371=LINE('',#44734,#9527);
#7372=LINE('',#44770,#9528);
#7373=LINE('',#44807,#9529);
#7374=LINE('',#44842,#9530);
#7375=LINE('',#44879,#9531);
#7376=LINE('',#44914,#9532);
#7377=LINE('',#44951,#9533);
#7378=LINE('',#44987,#9534);
#7379=LINE('',#45024,#9535);
#7380=LINE('',#45030,#9536);
#7381=LINE('',#45041,#9537);
#7382=LINE('',#45046,#9538);
#7383=LINE('',#49545,#9539);
#7384=LINE('',#49549,#9540);
#7385=LINE('',#49551,#9541);
#7386=LINE('',#49553,#9542);
#7387=LINE('',#49554,#9543);
#7388=LINE('',#49577,#9544);
#7389=LINE('',#49580,#9545);
#7390=LINE('',#49582,#9546);
#7391=LINE('',#49583,#9547);
#7392=LINE('',#49608,#9548);
#7393=LINE('',#49612,#9549);
#7394=LINE('',#49619,#9550);
#7395=LINE('',#49623,#9551);
#7396=LINE('',#49627,#9552);
#7397=LINE('',#49634,#9553);
#7398=LINE('',#49643,#9554);
#7399=LINE('',#49649,#9555);
#7400=LINE('',#49656,#9556);
#7401=LINE('',#49665,#9557);
#7402=LINE('',#49671,#9558);
#7403=LINE('',#49674,#9559);
#7404=LINE('',#49678,#9560);
#7405=LINE('',#49682,#9561);
#7406=LINE('',#49687,#9562);
#7407=LINE('',#49695,#9563);
#7408=LINE('',#49702,#9564);
#7409=LINE('',#49708,#9565);
#7410=LINE('',#49714,#9566);
#7411=LINE('',#49731,#9567);
#7412=LINE('',#49737,#9568);
#7413=LINE('',#49743,#9569);
#7414=LINE('',#49749,#9570);
#7415=LINE('',#49755,#9571);
#7416=LINE('',#49774,#9572);
#7417=LINE('',#49780,#9573);
#7418=LINE('',#49785,#9574);
#7419=LINE('',#49788,#9575);
#7420=LINE('',#49795,#9576);
#7421=LINE('',#49802,#9577);
#7422=LINE('',#49804,#9578);
#7423=LINE('',#49806,#9579);
#7424=LINE('',#49808,#9580);
#7425=LINE('',#49810,#9581);
#7426=LINE('',#49814,#9582);
#7427=LINE('',#49816,#9583);
#7428=LINE('',#49822,#9584);
#7429=LINE('',#49832,#9585);
#7430=LINE('',#49838,#9586);
#7431=LINE('',#49999,#9587);
#7432=LINE('',#50002,#9588);
#7433=LINE('',#50008,#9589);
#7434=LINE('',#50014,#9590);
#7435=LINE('',#50022,#9591);
#7436=LINE('',#50026,#9592);
#7437=LINE('',#50030,#9593);
#7438=LINE('',#50031,#9594);
#7439=LINE('',#50035,#9595);
#7440=LINE('',#50037,#9596);
#7441=LINE('',#50042,#9597);
#7442=LINE('',#50043,#9598);
#7443=LINE('',#50045,#9599);
#7444=LINE('',#50048,#9600);
#7445=LINE('',#50050,#9601);
#7446=LINE('',#50051,#9602);
#7447=LINE('',#50054,#9603);
#7448=LINE('',#50055,#9604);
#7449=LINE('',#50058,#9605);
#7450=LINE('',#50059,#9606);
#7451=LINE('',#50120,#9607);
#7452=LINE('',#50179,#9608);
#7453=LINE('',#50238,#9609);
#7454=LINE('',#50297,#9610);
#7455=LINE('',#50309,#9611);
#7456=LINE('',#50315,#9612);
#7457=LINE('',#50339,#9613);
#7458=LINE('',#50387,#9614);
#7459=LINE('',#50435,#9615);
#7460=LINE('',#50489,#9616);
#7461=LINE('',#50537,#9617);
#7462=LINE('',#50585,#9618);
#7463=LINE('',#50639,#9619);
#7464=LINE('',#50687,#9620);
#7465=LINE('',#50735,#9621);
#7466=LINE('',#50789,#9622);
#7467=LINE('',#50837,#9623);
#7468=LINE('',#50885,#9624);
#7469=LINE('',#50939,#9625);
#7470=LINE('',#50987,#9626);
#7471=LINE('',#51035,#9627);
#7472=LINE('',#51089,#9628);
#7473=LINE('',#51112,#9629);
#7474=LINE('',#51137,#9630);
#7475=LINE('',#51161,#9631);
#7476=LINE('',#51186,#9632);
#7477=LINE('',#51211,#9633);
#7478=LINE('',#51235,#9634);
#7479=LINE('',#51260,#9635);
#7480=LINE('',#51285,#9636);
#7481=LINE('',#51309,#9637);
#7482=LINE('',#51334,#9638);
#7483=LINE('',#51359,#9639);
#7484=LINE('',#51383,#9640);
#7485=LINE('',#51408,#9641);
#7486=LINE('',#51433,#9642);
#7487=LINE('',#52576,#9643);
#7488=LINE('',#52580,#9644);
#7489=LINE('',#52584,#9645);
#7490=LINE('',#52588,#9646);
#7491=LINE('',#52592,#9647);
#7492=LINE('',#52595,#9648);
#7493=LINE('',#52599,#9649);
#7494=LINE('',#52603,#9650);
#7495=LINE('',#52604,#9651);
#7496=LINE('',#52605,#9652);
#7497=LINE('',#52608,#9653);
#7498=LINE('',#52609,#9654);
#7499=LINE('',#52612,#9655);
#7500=LINE('',#52613,#9656);
#7501=LINE('',#52616,#9657);
#7502=LINE('',#52617,#9658);
#7503=LINE('',#52620,#9659);
#7504=LINE('',#52621,#9660);
#7505=LINE('',#52623,#9661);
#7506=LINE('',#52627,#9662);
#7507=LINE('',#52629,#9663);
#7508=LINE('',#52631,#9664);
#7509=LINE('',#52632,#9665);
#7510=LINE('',#52636,#9666);
#7511=LINE('',#52639,#9667);
#7512=LINE('',#52640,#9668);
#7513=LINE('',#52646,#9669);
#7514=LINE('',#52648,#9670);
#7515=LINE('',#52650,#9671);
#7516=LINE('',#52651,#9672);
#7517=LINE('',#52655,#9673);
#7518=LINE('',#52658,#9674);
#7519=LINE('',#52659,#9675);
#7520=LINE('',#52665,#9676);
#7521=LINE('',#52667,#9677);
#7522=LINE('',#52669,#9678);
#7523=LINE('',#52670,#9679);
#7524=LINE('',#52674,#9680);
#7525=LINE('',#52677,#9681);
#7526=LINE('',#52678,#9682);
#7527=LINE('',#52684,#9683);
#7528=LINE('',#52686,#9684);
#7529=LINE('',#52688,#9685);
#7530=LINE('',#52689,#9686);
#7531=LINE('',#52693,#9687);
#7532=LINE('',#52696,#9688);
#7533=LINE('',#52697,#9689);
#7534=LINE('',#52703,#9690);
#7535=LINE('',#52705,#9691);
#7536=LINE('',#52707,#9692);
#7537=LINE('',#52708,#9693);
#7538=LINE('',#52712,#9694);
#7539=LINE('',#52715,#9695);
#7540=LINE('',#52716,#9696);
#7541=LINE('',#52722,#9697);
#7542=LINE('',#52724,#9698);
#7543=LINE('',#52726,#9699);
#7544=LINE('',#52727,#9700);
#7545=LINE('',#52731,#9701);
#7546=LINE('',#52734,#9702);
#7547=LINE('',#52735,#9703);
#7548=LINE('',#52741,#9704);
#7549=LINE('',#52743,#9705);
#7550=LINE('',#52745,#9706);
#7551=LINE('',#52746,#9707);
#7552=LINE('',#52750,#9708);
#7553=LINE('',#52753,#9709);
#7554=LINE('',#52754,#9710);
#7555=LINE('',#52760,#9711);
#7556=LINE('',#52762,#9712);
#7557=LINE('',#52764,#9713);
#7558=LINE('',#52765,#9714);
#7559=LINE('',#52769,#9715);
#7560=LINE('',#52772,#9716);
#7561=LINE('',#52773,#9717);
#7562=LINE('',#52779,#9718);
#7563=LINE('',#52781,#9719);
#7564=LINE('',#52783,#9720);
#7565=LINE('',#52784,#9721);
#7566=LINE('',#52789,#9722);
#7567=LINE('',#52793,#9723);
#7568=LINE('',#52794,#9724);
#7569=LINE('',#52802,#9725);
#7570=LINE('',#52804,#9726);
#7571=LINE('',#52806,#9727);
#7572=LINE('',#52807,#9728);
#7573=LINE('',#52811,#9729);
#7574=LINE('',#52814,#9730);
#7575=LINE('',#52815,#9731);
#7576=LINE('',#52821,#9732);
#7577=LINE('',#52823,#9733);
#7578=LINE('',#52825,#9734);
#7579=LINE('',#52826,#9735);
#7580=LINE('',#52830,#9736);
#7581=LINE('',#52833,#9737);
#7582=LINE('',#52834,#9738);
#7583=LINE('',#52840,#9739);
#7584=LINE('',#52842,#9740);
#7585=LINE('',#52844,#9741);
#7586=LINE('',#52845,#9742);
#7587=LINE('',#52849,#9743);
#7588=LINE('',#52852,#9744);
#7589=LINE('',#52853,#9745);
#7590=LINE('',#52859,#9746);
#7591=LINE('',#52861,#9747);
#7592=LINE('',#52863,#9748);
#7593=LINE('',#52864,#9749);
#7594=LINE('',#52868,#9750);
#7595=LINE('',#52871,#9751);
#7596=LINE('',#52872,#9752);
#7597=LINE('',#52878,#9753);
#7598=LINE('',#52880,#9754);
#7599=LINE('',#52882,#9755);
#7600=LINE('',#52883,#9756);
#7601=LINE('',#52887,#9757);
#7602=LINE('',#52890,#9758);
#7603=LINE('',#52891,#9759);
#7604=LINE('',#52897,#9760);
#7605=LINE('',#52899,#9761);
#7606=LINE('',#52901,#9762);
#7607=LINE('',#52902,#9763);
#7608=LINE('',#52906,#9764);
#7609=LINE('',#52909,#9765);
#7610=LINE('',#52910,#9766);
#7611=LINE('',#52916,#9767);
#7612=LINE('',#52918,#9768);
#7613=LINE('',#52920,#9769);
#7614=LINE('',#52921,#9770);
#7615=LINE('',#52925,#9771);
#7616=LINE('',#52928,#9772);
#7617=LINE('',#52929,#9773);
#7618=LINE('',#52935,#9774);
#7619=LINE('',#52937,#9775);
#7620=LINE('',#52939,#9776);
#7621=LINE('',#52940,#9777);
#7622=LINE('',#52944,#9778);
#7623=LINE('',#52947,#9779);
#7624=LINE('',#52948,#9780);
#7625=LINE('',#52954,#9781);
#7626=LINE('',#52956,#9782);
#7627=LINE('',#52958,#9783);
#7628=LINE('',#52959,#9784);
#7629=LINE('',#52963,#9785);
#7630=LINE('',#52966,#9786);
#7631=LINE('',#52967,#9787);
#7632=LINE('',#52973,#9788);
#7633=LINE('',#52975,#9789);
#7634=LINE('',#52977,#9790);
#7635=LINE('',#52978,#9791);
#7636=LINE('',#52982,#9792);
#7637=LINE('',#52985,#9793);
#7638=LINE('',#52986,#9794);
#7639=LINE('',#52992,#9795);
#7640=LINE('',#52994,#9796);
#7641=LINE('',#52996,#9797);
#7642=LINE('',#52997,#9798);
#7643=LINE('',#53001,#9799);
#7644=LINE('',#53004,#9800);
#7645=LINE('',#53005,#9801);
#7646=LINE('',#53011,#9802);
#7647=LINE('',#53013,#9803);
#7648=LINE('',#53015,#9804);
#7649=LINE('',#53016,#9805);
#7650=LINE('',#53020,#9806);
#7651=LINE('',#53023,#9807);
#7652=LINE('',#53024,#9808);
#7653=LINE('',#53030,#9809);
#7654=LINE('',#53032,#9810);
#7655=LINE('',#53034,#9811);
#7656=LINE('',#53035,#9812);
#7657=LINE('',#53039,#9813);
#7658=LINE('',#53042,#9814);
#7659=LINE('',#53043,#9815);
#7660=LINE('',#53049,#9816);
#7661=LINE('',#53051,#9817);
#7662=LINE('',#53053,#9818);
#7663=LINE('',#53054,#9819);
#7664=LINE('',#53058,#9820);
#7665=LINE('',#53061,#9821);
#7666=LINE('',#53062,#9822);
#7667=LINE('',#53068,#9823);
#7668=LINE('',#53070,#9824);
#7669=LINE('',#53072,#9825);
#7670=LINE('',#53073,#9826);
#7671=LINE('',#53077,#9827);
#7672=LINE('',#53080,#9828);
#7673=LINE('',#53081,#9829);
#7674=LINE('',#53087,#9830);
#7675=LINE('',#53089,#9831);
#7676=LINE('',#53091,#9832);
#7677=LINE('',#53092,#9833);
#7678=LINE('',#53096,#9834);
#7679=LINE('',#53099,#9835);
#7680=LINE('',#53100,#9836);
#7681=LINE('',#53106,#9837);
#7682=LINE('',#53108,#9838);
#7683=LINE('',#53110,#9839);
#7684=LINE('',#53111,#9840);
#7685=LINE('',#53115,#9841);
#7686=LINE('',#53118,#9842);
#7687=LINE('',#53119,#9843);
#7688=LINE('',#53127,#9844);
#7689=LINE('',#53128,#9845);
#7690=LINE('',#53131,#9846);
#7691=LINE('',#53133,#9847);
#7692=LINE('',#53134,#9848);
#7693=LINE('',#53137,#9849);
#7694=LINE('',#53138,#9850);
#7695=LINE('',#53144,#9851);
#7696=LINE('',#53146,#9852);
#7697=LINE('',#53148,#9853);
#7698=LINE('',#53149,#9854);
#7699=LINE('',#53153,#9855);
#7700=LINE('',#53156,#9856);
#7701=LINE('',#53157,#9857);
#7702=LINE('',#53163,#9858);
#7703=LINE('',#53165,#9859);
#7704=LINE('',#53167,#9860);
#7705=LINE('',#53168,#9861);
#7706=LINE('',#53172,#9862);
#7707=LINE('',#53175,#9863);
#7708=LINE('',#53176,#9864);
#7709=LINE('',#53182,#9865);
#7710=LINE('',#53184,#9866);
#7711=LINE('',#53186,#9867);
#7712=LINE('',#53187,#9868);
#7713=LINE('',#53191,#9869);
#7714=LINE('',#53194,#9870);
#7715=LINE('',#53195,#9871);
#7716=LINE('',#53201,#9872);
#7717=LINE('',#53203,#9873);
#7718=LINE('',#53205,#9874);
#7719=LINE('',#53206,#9875);
#7720=LINE('',#53210,#9876);
#7721=LINE('',#53213,#9877);
#7722=LINE('',#53214,#9878);
#7723=LINE('',#53220,#9879);
#7724=LINE('',#53222,#9880);
#7725=LINE('',#53224,#9881);
#7726=LINE('',#53225,#9882);
#7727=LINE('',#53229,#9883);
#7728=LINE('',#53232,#9884);
#7729=LINE('',#53233,#9885);
#7730=LINE('',#53239,#9886);
#7731=LINE('',#53241,#9887);
#7732=LINE('',#53243,#9888);
#7733=LINE('',#53244,#9889);
#7734=LINE('',#53248,#9890);
#7735=LINE('',#53251,#9891);
#7736=LINE('',#53252,#9892);
#7737=LINE('',#53258,#9893);
#7738=LINE('',#53260,#9894);
#7739=LINE('',#53262,#9895);
#7740=LINE('',#53263,#9896);
#7741=LINE('',#53267,#9897);
#7742=LINE('',#53270,#9898);
#7743=LINE('',#53271,#9899);
#7744=LINE('',#53277,#9900);
#7745=LINE('',#53279,#9901);
#7746=LINE('',#53281,#9902);
#7747=LINE('',#53282,#9903);
#7748=LINE('',#53286,#9904);
#7749=LINE('',#53289,#9905);
#7750=LINE('',#53290,#9906);
#7751=LINE('',#53296,#9907);
#7752=LINE('',#53298,#9908);
#7753=LINE('',#53300,#9909);
#7754=LINE('',#53301,#9910);
#7755=LINE('',#53305,#9911);
#7756=LINE('',#53308,#9912);
#7757=LINE('',#53309,#9913);
#7758=LINE('',#53316,#9914);
#7759=LINE('',#53320,#9915);
#7760=LINE('',#53338,#9916);
#7761=LINE('',#53362,#9917);
#7762=LINE('',#53368,#9918);
#7763=LINE('',#53370,#9919);
#7764=LINE('',#53372,#9920);
#7765=LINE('',#53373,#9921);
#7766=LINE('',#53377,#9922);
#7767=LINE('',#53383,#9923);
#7768=LINE('',#53384,#9924);
#7769=LINE('',#53385,#9925);
#7770=LINE('',#53391,#9926);
#7771=LINE('',#53394,#9927);
#7772=LINE('',#53397,#9928);
#7773=LINE('',#53398,#9929);
#7774=LINE('',#53402,#9930);
#7775=LINE('',#53404,#9931);
#7776=LINE('',#53405,#9932);
#7777=LINE('',#53409,#9933);
#7778=LINE('',#53414,#9934);
#7779=LINE('',#53415,#9935);
#7780=LINE('',#53416,#9936);
#7781=LINE('',#53420,#9937);
#7782=LINE('',#53427,#9938);
#7783=LINE('',#53460,#9939);
#7784=LINE('',#53544,#9940);
#7785=LINE('',#53634,#9941);
#7786=LINE('',#53724,#9942);
#7787=LINE('',#53808,#9943);
#7788=LINE('',#53898,#9944);
#7789=LINE('',#53988,#9945);
#7790=LINE('',#54072,#9946);
#7791=LINE('',#54162,#9947);
#7792=LINE('',#54252,#9948);
#7793=LINE('',#54284,#9949);
#7794=LINE('',#54322,#9950);
#7795=LINE('',#54359,#9951);
#7796=LINE('',#54396,#9952);
#7797=LINE('',#54434,#9953);
#7798=LINE('',#54471,#9954);
#7799=LINE('',#54508,#9955);
#7800=LINE('',#54546,#9956);
#7801=LINE('',#55993,#9957);
#7802=LINE('',#56024,#9958);
#7803=LINE('',#56030,#9959);
#7804=LINE('',#56037,#9960);
#7805=LINE('',#56081,#9961);
#7806=LINE('',#56085,#9962);
#7807=LINE('',#56091,#9963);
#7808=LINE('',#56115,#9964);
#7809=LINE('',#56163,#9965);
#7810=LINE('',#56211,#9966);
#7811=LINE('',#56259,#9967);
#7812=LINE('',#56313,#9968);
#7813=LINE('',#56361,#9969);
#7814=LINE('',#56409,#9970);
#7815=LINE('',#56463,#9971);
#7816=LINE('',#56511,#9972);
#7817=LINE('',#56559,#9973);
#7818=LINE('',#56613,#9974);
#7819=LINE('',#56661,#9975);
#7820=LINE('',#56709,#9976);
#7821=LINE('',#56757,#9977);
#7822=LINE('',#56774,#9978);
#7823=LINE('',#56799,#9979);
#7824=LINE('',#56823,#9980);
#7825=LINE('',#56847,#9981);
#7826=LINE('',#56872,#9982);
#7827=LINE('',#56897,#9983);
#7828=LINE('',#56921,#9984);
#7829=LINE('',#56946,#9985);
#7830=LINE('',#56971,#9986);
#7831=LINE('',#56995,#9987);
#7832=LINE('',#57020,#9988);
#7833=LINE('',#57045,#9989);
#7834=LINE('',#57069,#9990);
#7835=LINE('',#58162,#9991);
#7836=LINE('',#58164,#9992);
#7837=LINE('',#58166,#9993);
#7838=LINE('',#58167,#9994);
#7839=LINE('',#58170,#9995);
#7840=LINE('',#58172,#9996);
#7841=LINE('',#58173,#9997);
#7842=LINE('',#58176,#9998);
#7843=LINE('',#58178,#9999);
#7844=LINE('',#58179,#10000);
#7845=LINE('',#58182,#10001);
#7846=LINE('',#58184,#10002);
#7847=LINE('',#58185,#10003);
#7848=LINE('',#58188,#10004);
#7849=LINE('',#58190,#10005);
#7850=LINE('',#58191,#10006);
#7851=LINE('',#58193,#10007);
#7852=LINE('',#58194,#10008);
#7853=LINE('',#58200,#10009);
#7854=LINE('',#58205,#10010);
#7855=LINE('',#58209,#10011);
#7856=LINE('',#58215,#10012);
#7857=LINE('',#58217,#10013);
#7858=LINE('',#58219,#10014);
#7859=LINE('',#58221,#10015);
#7860=LINE('',#58223,#10016);
#7861=LINE('',#58224,#10017);
#7862=LINE('',#58227,#10018);
#7863=LINE('',#58229,#10019);
#7864=LINE('',#58230,#10020);
#7865=LINE('',#58233,#10021);
#7866=LINE('',#58235,#10022);
#7867=LINE('',#58237,#10023);
#7868=LINE('',#58238,#10024);
#7869=LINE('',#58241,#10025);
#7870=LINE('',#58243,#10026);
#7871=LINE('',#58245,#10027);
#7872=LINE('',#58246,#10028);
#7873=LINE('',#58249,#10029);
#7874=LINE('',#58251,#10030);
#7875=LINE('',#58253,#10031);
#7876=LINE('',#58254,#10032);
#7877=LINE('',#58257,#10033);
#7878=LINE('',#58259,#10034);
#7879=LINE('',#58261,#10035);
#7880=LINE('',#58263,#10036);
#7881=LINE('',#58264,#10037);
#7882=LINE('',#58267,#10038);
#7883=LINE('',#58268,#10039);
#7884=LINE('',#58271,#10040);
#7885=LINE('',#58273,#10041);
#7886=LINE('',#58274,#10042);
#7887=LINE('',#58277,#10043);
#7888=LINE('',#58279,#10044);
#7889=LINE('',#58281,#10045);
#7890=LINE('',#58283,#10046);
#7891=LINE('',#58284,#10047);
#7892=LINE('',#58287,#10048);
#7893=LINE('',#58289,#10049);
#7894=LINE('',#58290,#10050);
#7895=LINE('',#58293,#10051);
#7896=LINE('',#58294,#10052);
#7897=LINE('',#58295,#10053);
#7898=LINE('',#58298,#10054);
#7899=LINE('',#58299,#10055);
#7900=LINE('',#58300,#10056);
#7901=LINE('',#58302,#10057);
#7902=LINE('',#58304,#10058);
#7903=LINE('',#58307,#10059);
#7904=LINE('',#58314,#10060);
#7905=LINE('',#58347,#10061);
#7906=LINE('',#58431,#10062);
#7907=LINE('',#58521,#10063);
#7908=LINE('',#58611,#10064);
#7909=LINE('',#58695,#10065);
#7910=LINE('',#58785,#10066);
#7911=LINE('',#58875,#10067);
#7912=LINE('',#58959,#10068);
#7913=LINE('',#59049,#10069);
#7914=LINE('',#59139,#10070);
#7915=LINE('',#59223,#10071);
#7916=LINE('',#59313,#10072);
#7917=LINE('',#59403,#10073);
#7918=LINE('',#59487,#10074);
#7919=LINE('',#59577,#10075);
#7920=LINE('',#59667,#10076);
#7921=LINE('',#59751,#10077);
#7922=LINE('',#59841,#10078);
#7923=LINE('',#59928,#10079);
#7924=LINE('',#60015,#10080);
#7925=LINE('',#60026,#10081);
#7926=LINE('',#60064,#10082);
#7927=LINE('',#60100,#10083);
#7928=LINE('',#60138,#10084);
#7929=LINE('',#60175,#10085);
#7930=LINE('',#60212,#10086);
#7931=LINE('',#60250,#10087);
#7932=LINE('',#60287,#10088);
#7933=LINE('',#60324,#10089);
#7934=LINE('',#60362,#10090);
#7935=LINE('',#60399,#10091);
#7936=LINE('',#60436,#10092);
#7937=LINE('',#60474,#10093);
#7938=LINE('',#60511,#10094);
#7939=LINE('',#60548,#10095);
#7940=LINE('',#60586,#10096);
#7941=LINE('',#60623,#10097);
#7942=LINE('',#60660,#10098);
#7943=LINE('',#60698,#10099);
#7944=LINE('',#63189,#10100);
#7945=LINE('',#63200,#10101);
#7946=LINE('',#63202,#10102);
#7947=LINE('',#63203,#10103);
#7948=LINE('',#63206,#10104);
#7949=LINE('',#63207,#10105);
#7950=LINE('',#63210,#10106);
#7951=LINE('',#63211,#10107);
#7952=LINE('',#63214,#10108);
#7953=LINE('',#63216,#10109);
#7954=LINE('',#63217,#10110);
#7955=LINE('',#63221,#10111);
#7956=LINE('',#63223,#10112);
#7957=LINE('',#63230,#10113);
#7958=LINE('',#63237,#10114);
#7959=LINE('',#63243,#10115);
#7960=LINE('',#63247,#10116);
#7961=LINE('',#63252,#10117);
#7962=LINE('',#63256,#10118);
#7963=LINE('',#63260,#10119);
#7964=LINE('',#63264,#10120);
#7965=LINE('',#63268,#10121);
#7966=LINE('',#63273,#10122);
#7967=LINE('',#63277,#10123);
#7968=LINE('',#63281,#10124);
#7969=LINE('',#63284,#10125);
#7970=LINE('',#63289,#10126);
#7971=LINE('',#63293,#10127);
#7972=LINE('',#63297,#10128);
#7973=LINE('',#63301,#10129);
#7974=LINE('',#63306,#10130);
#7975=LINE('',#63310,#10131);
#7976=LINE('',#63315,#10132);
#7977=LINE('',#63316,#10133);
#7978=LINE('',#63317,#10134);
#7979=LINE('',#63321,#10135);
#7980=LINE('',#63327,#10136);
#7981=LINE('',#63328,#10137);
#7982=LINE('',#63329,#10138);
#7983=LINE('',#63333,#10139);
#7984=LINE('',#63339,#10140);
#7985=LINE('',#63340,#10141);
#7986=LINE('',#63341,#10142);
#7987=LINE('',#63345,#10143);
#7988=LINE('',#63349,#10144);
#7989=LINE('',#63350,#10145);
#7990=LINE('',#63353,#10146);
#7991=LINE('',#63355,#10147);
#7992=LINE('',#63356,#10148);
#7993=LINE('',#63359,#10149);
#7994=LINE('',#63363,#10150);
#7995=LINE('',#63364,#10151);
#7996=LINE('',#63367,#10152);
#7997=LINE('',#63370,#10153);
#7998=LINE('',#63371,#10154);
#7999=LINE('',#63373,#10155);
#8000=LINE('',#63375,#10156);
#8001=LINE('',#63377,#10157);
#8002=LINE('',#63380,#10158);
#8003=LINE('',#63382,#10159);
#8004=LINE('',#63383,#10160);
#8005=LINE('',#63386,#10161);
#8006=LINE('',#63390,#10162);
#8007=LINE('',#63391,#10163);
#8008=LINE('',#63394,#10164);
#8009=LINE('',#63398,#10165);
#8010=LINE('',#63399,#10166);
#8011=LINE('',#63402,#10167);
#8012=LINE('',#63406,#10168);
#8013=LINE('',#63407,#10169);
#8014=LINE('',#63412,#10170);
#8015=LINE('',#63415,#10171);
#8016=LINE('',#63418,#10172);
#8017=LINE('',#63419,#10173);
#8018=LINE('',#63422,#10174);
#8019=LINE('',#63426,#10175);
#8020=LINE('',#63427,#10176);
#8021=LINE('',#63429,#10177);
#8022=LINE('',#63430,#10178);
#8023=LINE('',#63432,#10179);
#8024=LINE('',#63434,#10180);
#8025=LINE('',#63436,#10181);
#8026=LINE('',#63440,#10182);
#8027=LINE('',#63441,#10183);
#8028=LINE('',#63442,#10184);
#8029=LINE('',#63446,#10185);
#8030=LINE('',#63452,#10186);
#8031=LINE('',#63453,#10187);
#8032=LINE('',#63454,#10188);
#8033=LINE('',#63459,#10189);
#8034=LINE('',#63460,#10190);
#8035=LINE('',#63462,#10191);
#8036=LINE('',#63466,#10192);
#8037=LINE('',#63467,#10193);
#8038=LINE('',#63470,#10194);
#8039=LINE('',#63473,#10195);
#8040=LINE('',#63474,#10196);
#8041=LINE('',#63476,#10197);
#8042=LINE('',#63484,#10198);
#8043=LINE('',#63489,#10199);
#8044=LINE('',#63492,#10200);
#8045=LINE('',#63498,#10201);
#8046=LINE('',#63506,#10202);
#8047=LINE('',#63510,#10203);
#8048=LINE('',#63515,#10204);
#8049=LINE('',#63522,#10205);
#8050=LINE('',#63526,#10206);
#8051=LINE('',#63532,#10207);
#8052=LINE('',#63539,#10208);
#8053=LINE('',#63546,#10209);
#8054=LINE('',#63579,#10210);
#8055=LINE('',#63663,#10211);
#8056=LINE('',#63753,#10212);
#8057=LINE('',#63837,#10213);
#8058=LINE('',#63927,#10214);
#8059=LINE('',#64017,#10215);
#8060=LINE('',#64101,#10216);
#8061=LINE('',#64191,#10217);
#8062=LINE('',#64275,#10218);
#8063=LINE('',#64365,#10219);
#8064=LINE('',#64455,#10220);
#8065=LINE('',#64539,#10221);
#8066=LINE('',#64629,#10222);
#8067=LINE('',#64713,#10223);
#8068=LINE('',#64803,#10224);
#8069=LINE('',#64887,#10225);
#8070=LINE('',#64977,#10226);
#8071=LINE('',#65067,#10227);
#8072=LINE('',#65151,#10228);
#8073=LINE('',#65241,#10229);
#8074=LINE('',#65325,#10230);
#8075=LINE('',#65415,#10231);
#8076=LINE('',#65502,#10232);
#8077=LINE('',#65536,#10233);
#8078=LINE('',#65574,#10234);
#8079=LINE('',#65611,#10235);
#8080=LINE('',#65648,#10236);
#8081=LINE('',#65685,#10237);
#8082=LINE('',#65722,#10238);
#8083=LINE('',#65760,#10239);
#8084=LINE('',#65797,#10240);
#8085=LINE('',#65834,#10241);
#8086=LINE('',#65871,#10242);
#8087=LINE('',#65908,#10243);
#8088=LINE('',#65945,#10244);
#8089=LINE('',#65982,#10245);
#8090=LINE('',#66020,#10246);
#8091=LINE('',#66057,#10247);
#8092=LINE('',#66094,#10248);
#8093=LINE('',#66131,#10249);
#8094=LINE('',#66168,#10250);
#8095=LINE('',#66206,#10251);
#8096=LINE('',#66243,#10252);
#8097=LINE('',#66280,#10253);
#8098=LINE('',#69016,#10254);
#8099=LINE('',#69027,#10255);
#8100=LINE('',#69029,#10256);
#8101=LINE('',#69030,#10257);
#8102=LINE('',#69033,#10258);
#8103=LINE('',#69034,#10259);
#8104=LINE('',#69037,#10260);
#8105=LINE('',#69038,#10261);
#8106=LINE('',#69041,#10262);
#8107=LINE('',#69043,#10263);
#8108=LINE('',#69044,#10264);
#8109=LINE('',#69048,#10265);
#8110=LINE('',#69050,#10266);
#8111=LINE('',#69057,#10267);
#8112=LINE('',#69064,#10268);
#8113=LINE('',#69069,#10269);
#8114=LINE('',#69096,#10270);
#8115=LINE('',#69144,#10271);
#8116=LINE('',#69192,#10272);
#8117=LINE('',#69240,#10273);
#8118=LINE('',#69294,#10274);
#8119=LINE('',#69342,#10275);
#8120=LINE('',#69390,#10276);
#8121=LINE('',#69444,#10277);
#8122=LINE('',#69492,#10278);
#8123=LINE('',#69540,#10279);
#8124=LINE('',#69591,#10280);
#8125=LINE('',#69642,#10281);
#8126=LINE('',#69690,#10282);
#8127=LINE('',#69738,#10283);
#8128=LINE('',#69792,#10284);
#8129=LINE('',#69840,#10285);
#8130=LINE('',#69888,#10286);
#8131=LINE('',#69942,#10287);
#8132=LINE('',#69990,#10288);
#8133=LINE('',#70038,#10289);
#8134=LINE('',#70086,#10290);
#8135=LINE('',#70140,#10291);
#8136=LINE('',#70188,#10292);
#8137=LINE('',#70204,#10293);
#8138=LINE('',#70229,#10294);
#8139=LINE('',#70254,#10295);
#8140=LINE('',#70279,#10296);
#8141=LINE('',#70303,#10297);
#8142=LINE('',#70327,#10298);
#8143=LINE('',#70352,#10299);
#8144=LINE('',#70377,#10300);
#8145=LINE('',#70401,#10301);
#8146=LINE('',#70426,#10302);
#8147=LINE('',#70451,#10303);
#8148=LINE('',#70475,#10304);
#8149=LINE('',#70500,#10305);
#8150=LINE('',#70524,#10306);
#8151=LINE('',#70549,#10307);
#8152=LINE('',#70573,#10308);
#8153=LINE('',#70598,#10309);
#8154=LINE('',#70623,#10310);
#8155=LINE('',#70647,#10311);
#8156=LINE('',#70672,#10312);
#8157=LINE('',#70697,#10313);
#8158=LINE('',#70721,#10314);
#8159=LINE('',#72294,#10315);
#8160=LINE('',#72298,#10316);
#8161=LINE('',#72302,#10317);
#8162=LINE('',#72306,#10318);
#8163=LINE('',#72310,#10319);
#8164=LINE('',#72313,#10320);
#8165=LINE('',#72317,#10321);
#8166=LINE('',#72321,#10322);
#8167=LINE('',#72322,#10323);
#8168=LINE('',#72323,#10324);
#8169=LINE('',#72326,#10325);
#8170=LINE('',#72327,#10326);
#8171=LINE('',#72330,#10327);
#8172=LINE('',#72331,#10328);
#8173=LINE('',#72334,#10329);
#8174=LINE('',#72335,#10330);
#8175=LINE('',#72338,#10331);
#8176=LINE('',#72339,#10332);
#8177=LINE('',#72341,#10333);
#8178=LINE('',#72345,#10334);
#8179=LINE('',#72347,#10335);
#8180=LINE('',#72349,#10336);
#8181=LINE('',#72350,#10337);
#8182=LINE('',#72354,#10338);
#8183=LINE('',#72357,#10339);
#8184=LINE('',#72358,#10340);
#8185=LINE('',#72364,#10341);
#8186=LINE('',#72366,#10342);
#8187=LINE('',#72368,#10343);
#8188=LINE('',#72369,#10344);
#8189=LINE('',#72373,#10345);
#8190=LINE('',#72376,#10346);
#8191=LINE('',#72377,#10347);
#8192=LINE('',#72383,#10348);
#8193=LINE('',#72385,#10349);
#8194=LINE('',#72387,#10350);
#8195=LINE('',#72388,#10351);
#8196=LINE('',#72392,#10352);
#8197=LINE('',#72395,#10353);
#8198=LINE('',#72396,#10354);
#8199=LINE('',#72402,#10355);
#8200=LINE('',#72404,#10356);
#8201=LINE('',#72406,#10357);
#8202=LINE('',#72407,#10358);
#8203=LINE('',#72411,#10359);
#8204=LINE('',#72414,#10360);
#8205=LINE('',#72415,#10361);
#8206=LINE('',#72421,#10362);
#8207=LINE('',#72423,#10363);
#8208=LINE('',#72425,#10364);
#8209=LINE('',#72426,#10365);
#8210=LINE('',#72430,#10366);
#8211=LINE('',#72433,#10367);
#8212=LINE('',#72434,#10368);
#8213=LINE('',#72440,#10369);
#8214=LINE('',#72442,#10370);
#8215=LINE('',#72444,#10371);
#8216=LINE('',#72445,#10372);
#8217=LINE('',#72449,#10373);
#8218=LINE('',#72452,#10374);
#8219=LINE('',#72453,#10375);
#8220=LINE('',#72459,#10376);
#8221=LINE('',#72461,#10377);
#8222=LINE('',#72463,#10378);
#8223=LINE('',#72464,#10379);
#8224=LINE('',#72468,#10380);
#8225=LINE('',#72471,#10381);
#8226=LINE('',#72472,#10382);
#8227=LINE('',#72478,#10383);
#8228=LINE('',#72480,#10384);
#8229=LINE('',#72482,#10385);
#8230=LINE('',#72483,#10386);
#8231=LINE('',#72487,#10387);
#8232=LINE('',#72490,#10388);
#8233=LINE('',#72491,#10389);
#8234=LINE('',#72497,#10390);
#8235=LINE('',#72499,#10391);
#8236=LINE('',#72501,#10392);
#8237=LINE('',#72502,#10393);
#8238=LINE('',#72507,#10394);
#8239=LINE('',#72511,#10395);
#8240=LINE('',#72512,#10396);
#8241=LINE('',#72520,#10397);
#8242=LINE('',#72522,#10398);
#8243=LINE('',#72524,#10399);
#8244=LINE('',#72525,#10400);
#8245=LINE('',#72529,#10401);
#8246=LINE('',#72532,#10402);
#8247=LINE('',#72533,#10403);
#8248=LINE('',#72539,#10404);
#8249=LINE('',#72541,#10405);
#8250=LINE('',#72543,#10406);
#8251=LINE('',#72544,#10407);
#8252=LINE('',#72548,#10408);
#8253=LINE('',#72551,#10409);
#8254=LINE('',#72552,#10410);
#8255=LINE('',#72558,#10411);
#8256=LINE('',#72560,#10412);
#8257=LINE('',#72562,#10413);
#8258=LINE('',#72563,#10414);
#8259=LINE('',#72567,#10415);
#8260=LINE('',#72570,#10416);
#8261=LINE('',#72571,#10417);
#8262=LINE('',#72577,#10418);
#8263=LINE('',#72579,#10419);
#8264=LINE('',#72581,#10420);
#8265=LINE('',#72582,#10421);
#8266=LINE('',#72586,#10422);
#8267=LINE('',#72589,#10423);
#8268=LINE('',#72590,#10424);
#8269=LINE('',#72596,#10425);
#8270=LINE('',#72598,#10426);
#8271=LINE('',#72600,#10427);
#8272=LINE('',#72601,#10428);
#8273=LINE('',#72605,#10429);
#8274=LINE('',#72608,#10430);
#8275=LINE('',#72609,#10431);
#8276=LINE('',#72615,#10432);
#8277=LINE('',#72617,#10433);
#8278=LINE('',#72619,#10434);
#8279=LINE('',#72620,#10435);
#8280=LINE('',#72624,#10436);
#8281=LINE('',#72627,#10437);
#8282=LINE('',#72628,#10438);
#8283=LINE('',#72634,#10439);
#8284=LINE('',#72636,#10440);
#8285=LINE('',#72638,#10441);
#8286=LINE('',#72639,#10442);
#8287=LINE('',#72643,#10443);
#8288=LINE('',#72646,#10444);
#8289=LINE('',#72647,#10445);
#8290=LINE('',#72653,#10446);
#8291=LINE('',#72655,#10447);
#8292=LINE('',#72657,#10448);
#8293=LINE('',#72658,#10449);
#8294=LINE('',#72662,#10450);
#8295=LINE('',#72665,#10451);
#8296=LINE('',#72666,#10452);
#8297=LINE('',#72672,#10453);
#8298=LINE('',#72674,#10454);
#8299=LINE('',#72676,#10455);
#8300=LINE('',#72677,#10456);
#8301=LINE('',#72681,#10457);
#8302=LINE('',#72684,#10458);
#8303=LINE('',#72685,#10459);
#8304=LINE('',#72691,#10460);
#8305=LINE('',#72693,#10461);
#8306=LINE('',#72695,#10462);
#8307=LINE('',#72696,#10463);
#8308=LINE('',#72700,#10464);
#8309=LINE('',#72703,#10465);
#8310=LINE('',#72704,#10466);
#8311=LINE('',#72710,#10467);
#8312=LINE('',#72712,#10468);
#8313=LINE('',#72714,#10469);
#8314=LINE('',#72715,#10470);
#8315=LINE('',#72719,#10471);
#8316=LINE('',#72722,#10472);
#8317=LINE('',#72723,#10473);
#8318=LINE('',#72729,#10474);
#8319=LINE('',#72731,#10475);
#8320=LINE('',#72733,#10476);
#8321=LINE('',#72734,#10477);
#8322=LINE('',#72738,#10478);
#8323=LINE('',#72741,#10479);
#8324=LINE('',#72742,#10480);
#8325=LINE('',#72748,#10481);
#8326=LINE('',#72750,#10482);
#8327=LINE('',#72752,#10483);
#8328=LINE('',#72753,#10484);
#8329=LINE('',#72757,#10485);
#8330=LINE('',#72760,#10486);
#8331=LINE('',#72761,#10487);
#8332=LINE('',#72767,#10488);
#8333=LINE('',#72769,#10489);
#8334=LINE('',#72771,#10490);
#8335=LINE('',#72772,#10491);
#8336=LINE('',#72776,#10492);
#8337=LINE('',#72779,#10493);
#8338=LINE('',#72780,#10494);
#8339=LINE('',#72786,#10495);
#8340=LINE('',#72788,#10496);
#8341=LINE('',#72790,#10497);
#8342=LINE('',#72791,#10498);
#8343=LINE('',#72795,#10499);
#8344=LINE('',#72798,#10500);
#8345=LINE('',#72799,#10501);
#8346=LINE('',#72805,#10502);
#8347=LINE('',#72807,#10503);
#8348=LINE('',#72809,#10504);
#8349=LINE('',#72810,#10505);
#8350=LINE('',#72814,#10506);
#8351=LINE('',#72817,#10507);
#8352=LINE('',#72818,#10508);
#8353=LINE('',#72824,#10509);
#8354=LINE('',#72826,#10510);
#8355=LINE('',#72828,#10511);
#8356=LINE('',#72829,#10512);
#8357=LINE('',#72833,#10513);
#8358=LINE('',#72836,#10514);
#8359=LINE('',#72837,#10515);
#8360=LINE('',#72845,#10516);
#8361=LINE('',#72846,#10517);
#8362=LINE('',#72849,#10518);
#8363=LINE('',#72851,#10519);
#8364=LINE('',#72852,#10520);
#8365=LINE('',#72855,#10521);
#8366=LINE('',#72856,#10522);
#8367=LINE('',#72862,#10523);
#8368=LINE('',#72864,#10524);
#8369=LINE('',#72866,#10525);
#8370=LINE('',#72867,#10526);
#8371=LINE('',#72871,#10527);
#8372=LINE('',#72874,#10528);
#8373=LINE('',#72875,#10529);
#8374=LINE('',#72881,#10530);
#8375=LINE('',#72883,#10531);
#8376=LINE('',#72885,#10532);
#8377=LINE('',#72886,#10533);
#8378=LINE('',#72890,#10534);
#8379=LINE('',#72893,#10535);
#8380=LINE('',#72894,#10536);
#8381=LINE('',#72900,#10537);
#8382=LINE('',#72902,#10538);
#8383=LINE('',#72904,#10539);
#8384=LINE('',#72905,#10540);
#8385=LINE('',#72909,#10541);
#8386=LINE('',#72912,#10542);
#8387=LINE('',#72913,#10543);
#8388=LINE('',#72919,#10544);
#8389=LINE('',#72921,#10545);
#8390=LINE('',#72923,#10546);
#8391=LINE('',#72924,#10547);
#8392=LINE('',#72928,#10548);
#8393=LINE('',#72931,#10549);
#8394=LINE('',#72932,#10550);
#8395=LINE('',#72938,#10551);
#8396=LINE('',#72940,#10552);
#8397=LINE('',#72942,#10553);
#8398=LINE('',#72943,#10554);
#8399=LINE('',#72947,#10555);
#8400=LINE('',#72950,#10556);
#8401=LINE('',#72951,#10557);
#8402=LINE('',#72957,#10558);
#8403=LINE('',#72959,#10559);
#8404=LINE('',#72961,#10560);
#8405=LINE('',#72962,#10561);
#8406=LINE('',#72966,#10562);
#8407=LINE('',#72969,#10563);
#8408=LINE('',#72970,#10564);
#8409=LINE('',#72976,#10565);
#8410=LINE('',#72978,#10566);
#8411=LINE('',#72980,#10567);
#8412=LINE('',#72981,#10568);
#8413=LINE('',#72985,#10569);
#8414=LINE('',#72988,#10570);
#8415=LINE('',#72989,#10571);
#8416=LINE('',#72995,#10572);
#8417=LINE('',#72997,#10573);
#8418=LINE('',#72999,#10574);
#8419=LINE('',#73000,#10575);
#8420=LINE('',#73004,#10576);
#8421=LINE('',#73007,#10577);
#8422=LINE('',#73008,#10578);
#8423=LINE('',#73014,#10579);
#8424=LINE('',#73016,#10580);
#8425=LINE('',#73018,#10581);
#8426=LINE('',#73019,#10582);
#8427=LINE('',#73023,#10583);
#8428=LINE('',#73026,#10584);
#8429=LINE('',#73027,#10585);
#8430=LINE('',#73034,#10586);
#8431=LINE('',#73038,#10587);
#8432=LINE('',#73056,#10588);
#8433=LINE('',#73080,#10589);
#8434=LINE('',#73086,#10590);
#8435=LINE('',#73110,#10591);
#8436=LINE('',#73158,#10592);
#8437=LINE('',#73206,#10593);
#8438=LINE('',#73260,#10594);
#8439=LINE('',#73308,#10595);
#8440=LINE('',#73356,#10596);
#8441=LINE('',#73407,#10597);
#8442=LINE('',#73455,#10598);
#8443=LINE('',#73503,#10599);
#8444=LINE('',#73551,#10600);
#8445=LINE('',#73605,#10601);
#8446=LINE('',#73653,#10602);
#8447=LINE('',#73701,#10603);
#8448=LINE('',#73755,#10604);
#8449=LINE('',#73803,#10605);
#8450=LINE('',#73851,#10606);
#8451=LINE('',#73905,#10607);
#8452=LINE('',#73953,#10608);
#8453=LINE('',#74001,#10609);
#8454=LINE('',#74054,#10610);
#8455=LINE('',#74075,#10611);
#8456=LINE('',#74100,#10612);
#8457=LINE('',#74124,#10613);
#8458=LINE('',#74149,#10614);
#8459=LINE('',#74174,#10615);
#8460=LINE('',#74198,#10616);
#8461=LINE('',#74223,#10617);
#8462=LINE('',#74248,#10618);
#8463=LINE('',#74272,#10619);
#8464=LINE('',#74297,#10620);
#8465=LINE('',#74322,#10621);
#8466=LINE('',#74346,#10622);
#8467=LINE('',#74370,#10623);
#8468=LINE('',#74395,#10624);
#8469=LINE('',#74420,#10625);
#8470=LINE('',#74444,#10626);
#8471=LINE('',#74469,#10627);
#8472=LINE('',#74494,#10628);
#8473=LINE('',#75801,#10629);
#8474=LINE('',#75805,#10630);
#8475=LINE('',#75809,#10631);
#8476=LINE('',#75813,#10632);
#8477=LINE('',#75817,#10633);
#8478=LINE('',#75820,#10634);
#8479=LINE('',#75824,#10635);
#8480=LINE('',#75828,#10636);
#8481=LINE('',#75829,#10637);
#8482=LINE('',#75830,#10638);
#8483=LINE('',#75833,#10639);
#8484=LINE('',#75834,#10640);
#8485=LINE('',#75837,#10641);
#8486=LINE('',#75838,#10642);
#8487=LINE('',#75841,#10643);
#8488=LINE('',#75842,#10644);
#8489=LINE('',#75845,#10645);
#8490=LINE('',#75846,#10646);
#8491=LINE('',#75848,#10647);
#8492=LINE('',#75852,#10648);
#8493=LINE('',#75854,#10649);
#8494=LINE('',#75856,#10650);
#8495=LINE('',#75857,#10651);
#8496=LINE('',#75861,#10652);
#8497=LINE('',#75864,#10653);
#8498=LINE('',#75865,#10654);
#8499=LINE('',#75871,#10655);
#8500=LINE('',#75873,#10656);
#8501=LINE('',#75875,#10657);
#8502=LINE('',#75876,#10658);
#8503=LINE('',#75880,#10659);
#8504=LINE('',#75883,#10660);
#8505=LINE('',#75884,#10661);
#8506=LINE('',#75890,#10662);
#8507=LINE('',#75892,#10663);
#8508=LINE('',#75894,#10664);
#8509=LINE('',#75895,#10665);
#8510=LINE('',#75899,#10666);
#8511=LINE('',#75902,#10667);
#8512=LINE('',#75903,#10668);
#8513=LINE('',#75909,#10669);
#8514=LINE('',#75911,#10670);
#8515=LINE('',#75913,#10671);
#8516=LINE('',#75914,#10672);
#8517=LINE('',#75918,#10673);
#8518=LINE('',#75921,#10674);
#8519=LINE('',#75922,#10675);
#8520=LINE('',#75928,#10676);
#8521=LINE('',#75930,#10677);
#8522=LINE('',#75932,#10678);
#8523=LINE('',#75933,#10679);
#8524=LINE('',#75937,#10680);
#8525=LINE('',#75940,#10681);
#8526=LINE('',#75941,#10682);
#8527=LINE('',#75947,#10683);
#8528=LINE('',#75949,#10684);
#8529=LINE('',#75951,#10685);
#8530=LINE('',#75952,#10686);
#8531=LINE('',#75956,#10687);
#8532=LINE('',#75959,#10688);
#8533=LINE('',#75960,#10689);
#8534=LINE('',#75966,#10690);
#8535=LINE('',#75968,#10691);
#8536=LINE('',#75970,#10692);
#8537=LINE('',#75971,#10693);
#8538=LINE('',#75975,#10694);
#8539=LINE('',#75978,#10695);
#8540=LINE('',#75979,#10696);
#8541=LINE('',#75985,#10697);
#8542=LINE('',#75987,#10698);
#8543=LINE('',#75989,#10699);
#8544=LINE('',#75990,#10700);
#8545=LINE('',#75994,#10701);
#8546=LINE('',#75997,#10702);
#8547=LINE('',#75998,#10703);
#8548=LINE('',#76004,#10704);
#8549=LINE('',#76006,#10705);
#8550=LINE('',#76008,#10706);
#8551=LINE('',#76009,#10707);
#8552=LINE('',#76014,#10708);
#8553=LINE('',#76018,#10709);
#8554=LINE('',#76019,#10710);
#8555=LINE('',#76027,#10711);
#8556=LINE('',#76029,#10712);
#8557=LINE('',#76031,#10713);
#8558=LINE('',#76032,#10714);
#8559=LINE('',#76036,#10715);
#8560=LINE('',#76039,#10716);
#8561=LINE('',#76040,#10717);
#8562=LINE('',#76046,#10718);
#8563=LINE('',#76048,#10719);
#8564=LINE('',#76050,#10720);
#8565=LINE('',#76051,#10721);
#8566=LINE('',#76055,#10722);
#8567=LINE('',#76058,#10723);
#8568=LINE('',#76059,#10724);
#8569=LINE('',#76065,#10725);
#8570=LINE('',#76067,#10726);
#8571=LINE('',#76069,#10727);
#8572=LINE('',#76070,#10728);
#8573=LINE('',#76074,#10729);
#8574=LINE('',#76077,#10730);
#8575=LINE('',#76078,#10731);
#8576=LINE('',#76084,#10732);
#8577=LINE('',#76086,#10733);
#8578=LINE('',#76088,#10734);
#8579=LINE('',#76089,#10735);
#8580=LINE('',#76093,#10736);
#8581=LINE('',#76096,#10737);
#8582=LINE('',#76097,#10738);
#8583=LINE('',#76103,#10739);
#8584=LINE('',#76105,#10740);
#8585=LINE('',#76107,#10741);
#8586=LINE('',#76108,#10742);
#8587=LINE('',#76112,#10743);
#8588=LINE('',#76115,#10744);
#8589=LINE('',#76116,#10745);
#8590=LINE('',#76122,#10746);
#8591=LINE('',#76124,#10747);
#8592=LINE('',#76126,#10748);
#8593=LINE('',#76127,#10749);
#8594=LINE('',#76131,#10750);
#8595=LINE('',#76134,#10751);
#8596=LINE('',#76135,#10752);
#8597=LINE('',#76141,#10753);
#8598=LINE('',#76143,#10754);
#8599=LINE('',#76145,#10755);
#8600=LINE('',#76146,#10756);
#8601=LINE('',#76150,#10757);
#8602=LINE('',#76153,#10758);
#8603=LINE('',#76154,#10759);
#8604=LINE('',#76160,#10760);
#8605=LINE('',#76162,#10761);
#8606=LINE('',#76164,#10762);
#8607=LINE('',#76165,#10763);
#8608=LINE('',#76169,#10764);
#8609=LINE('',#76172,#10765);
#8610=LINE('',#76173,#10766);
#8611=LINE('',#76179,#10767);
#8612=LINE('',#76181,#10768);
#8613=LINE('',#76183,#10769);
#8614=LINE('',#76184,#10770);
#8615=LINE('',#76188,#10771);
#8616=LINE('',#76191,#10772);
#8617=LINE('',#76192,#10773);
#8618=LINE('',#76198,#10774);
#8619=LINE('',#76200,#10775);
#8620=LINE('',#76202,#10776);
#8621=LINE('',#76203,#10777);
#8622=LINE('',#76207,#10778);
#8623=LINE('',#76210,#10779);
#8624=LINE('',#76211,#10780);
#8625=LINE('',#76217,#10781);
#8626=LINE('',#76219,#10782);
#8627=LINE('',#76221,#10783);
#8628=LINE('',#76222,#10784);
#8629=LINE('',#76226,#10785);
#8630=LINE('',#76229,#10786);
#8631=LINE('',#76230,#10787);
#8632=LINE('',#76236,#10788);
#8633=LINE('',#76238,#10789);
#8634=LINE('',#76240,#10790);
#8635=LINE('',#76241,#10791);
#8636=LINE('',#76245,#10792);
#8637=LINE('',#76248,#10793);
#8638=LINE('',#76249,#10794);
#8639=LINE('',#76255,#10795);
#8640=LINE('',#76257,#10796);
#8641=LINE('',#76259,#10797);
#8642=LINE('',#76260,#10798);
#8643=LINE('',#76264,#10799);
#8644=LINE('',#76267,#10800);
#8645=LINE('',#76268,#10801);
#8646=LINE('',#76274,#10802);
#8647=LINE('',#76276,#10803);
#8648=LINE('',#76278,#10804);
#8649=LINE('',#76279,#10805);
#8650=LINE('',#76283,#10806);
#8651=LINE('',#76286,#10807);
#8652=LINE('',#76287,#10808);
#8653=LINE('',#76293,#10809);
#8654=LINE('',#76295,#10810);
#8655=LINE('',#76297,#10811);
#8656=LINE('',#76298,#10812);
#8657=LINE('',#76302,#10813);
#8658=LINE('',#76305,#10814);
#8659=LINE('',#76306,#10815);
#8660=LINE('',#76312,#10816);
#8661=LINE('',#76314,#10817);
#8662=LINE('',#76316,#10818);
#8663=LINE('',#76317,#10819);
#8664=LINE('',#76321,#10820);
#8665=LINE('',#76324,#10821);
#8666=LINE('',#76325,#10822);
#8667=LINE('',#76331,#10823);
#8668=LINE('',#76333,#10824);
#8669=LINE('',#76335,#10825);
#8670=LINE('',#76336,#10826);
#8671=LINE('',#76340,#10827);
#8672=LINE('',#76343,#10828);
#8673=LINE('',#76344,#10829);
#8674=LINE('',#76352,#10830);
#8675=LINE('',#76353,#10831);
#8676=LINE('',#76356,#10832);
#8677=LINE('',#76358,#10833);
#8678=LINE('',#76359,#10834);
#8679=LINE('',#76362,#10835);
#8680=LINE('',#76363,#10836);
#8681=LINE('',#76369,#10837);
#8682=LINE('',#76371,#10838);
#8683=LINE('',#76373,#10839);
#8684=LINE('',#76374,#10840);
#8685=LINE('',#76378,#10841);
#8686=LINE('',#76381,#10842);
#8687=LINE('',#76382,#10843);
#8688=LINE('',#76388,#10844);
#8689=LINE('',#76390,#10845);
#8690=LINE('',#76392,#10846);
#8691=LINE('',#76393,#10847);
#8692=LINE('',#76397,#10848);
#8693=LINE('',#76400,#10849);
#8694=LINE('',#76401,#10850);
#8695=LINE('',#76407,#10851);
#8696=LINE('',#76409,#10852);
#8697=LINE('',#76411,#10853);
#8698=LINE('',#76412,#10854);
#8699=LINE('',#76416,#10855);
#8700=LINE('',#76419,#10856);
#8701=LINE('',#76420,#10857);
#8702=LINE('',#76426,#10858);
#8703=LINE('',#76428,#10859);
#8704=LINE('',#76430,#10860);
#8705=LINE('',#76431,#10861);
#8706=LINE('',#76435,#10862);
#8707=LINE('',#76438,#10863);
#8708=LINE('',#76439,#10864);
#8709=LINE('',#76445,#10865);
#8710=LINE('',#76447,#10866);
#8711=LINE('',#76449,#10867);
#8712=LINE('',#76450,#10868);
#8713=LINE('',#76454,#10869);
#8714=LINE('',#76457,#10870);
#8715=LINE('',#76458,#10871);
#8716=LINE('',#76464,#10872);
#8717=LINE('',#76466,#10873);
#8718=LINE('',#76468,#10874);
#8719=LINE('',#76469,#10875);
#8720=LINE('',#76473,#10876);
#8721=LINE('',#76476,#10877);
#8722=LINE('',#76477,#10878);
#8723=LINE('',#76483,#10879);
#8724=LINE('',#76485,#10880);
#8725=LINE('',#76487,#10881);
#8726=LINE('',#76488,#10882);
#8727=LINE('',#76492,#10883);
#8728=LINE('',#76495,#10884);
#8729=LINE('',#76496,#10885);
#8730=LINE('',#76502,#10886);
#8731=LINE('',#76504,#10887);
#8732=LINE('',#76506,#10888);
#8733=LINE('',#76507,#10889);
#8734=LINE('',#76511,#10890);
#8735=LINE('',#76514,#10891);
#8736=LINE('',#76515,#10892);
#8737=LINE('',#76521,#10893);
#8738=LINE('',#76523,#10894);
#8739=LINE('',#76525,#10895);
#8740=LINE('',#76526,#10896);
#8741=LINE('',#76530,#10897);
#8742=LINE('',#76533,#10898);
#8743=LINE('',#76534,#10899);
#8744=LINE('',#76541,#10900);
#8745=LINE('',#76545,#10901);
#8746=LINE('',#76563,#10902);
#8747=LINE('',#76587,#10903);
#8748=VECTOR('',#29351,1.);
#8749=VECTOR('',#29354,1.);
#8750=VECTOR('',#29359,1.);
#8751=VECTOR('',#29360,1.);
#8752=VECTOR('',#29361,1.);
#8753=VECTOR('',#29364,1.);
#8754=VECTOR('',#29371,1.);
#8755=VECTOR('',#29372,1.);
#8756=VECTOR('',#29373,1.);
#8757=VECTOR('',#29376,1.);
#8758=VECTOR('',#29383,1.);
#8759=VECTOR('',#29384,1.);
#8760=VECTOR('',#29385,1.);
#8761=VECTOR('',#29388,1.);
#8762=VECTOR('',#29395,1.);
#8763=VECTOR('',#29396,1.);
#8764=VECTOR('',#29399,1.);
#8765=VECTOR('',#29400,1.);
#8766=VECTOR('',#29401,1.);
#8767=VECTOR('',#29404,1.);
#8768=VECTOR('',#29409,1.);
#8769=VECTOR('',#29410,1.);
#8770=VECTOR('',#29413,1.);
#8771=VECTOR('',#29420,1.);
#8772=VECTOR('',#29423,1.);
#8773=VECTOR('',#29426,1.);
#8774=VECTOR('',#29429,1.);
#8775=VECTOR('',#29434,0.530000000000003);
#8776=VECTOR('',#29441,1.);
#8777=VECTOR('',#29444,1.);
#8778=VECTOR('',#29447,1.);
#8779=VECTOR('',#29450,1.);
#8780=VECTOR('',#29457,1.);
#8781=VECTOR('',#29458,1.);
#8782=VECTOR('',#29459,1.);
#8783=VECTOR('',#29460,1.);
#8784=VECTOR('',#29467,0.505000000000003);
#8785=VECTOR('',#29470,0.530000000000003);
#8786=VECTOR('',#29477,0.505000000000003);
#8787=VECTOR('',#29480,0.529999999999999);
#8788=VECTOR('',#29487,0.504999999999999);
#8789=VECTOR('',#29490,0.529999999999999);
#8790=VECTOR('',#29497,0.504999999999999);
#8791=VECTOR('',#29500,1.);
#8792=VECTOR('',#29501,1.);
#8793=VECTOR('',#29502,1.);
#8794=VECTOR('',#29505,1.);
#8795=VECTOR('',#29506,1.);
#8796=VECTOR('',#29507,1.);
#8797=VECTOR('',#29510,1.);
#8798=VECTOR('',#29513,1.);
#8799=VECTOR('',#29516,1.);
#8800=VECTOR('',#29517,1.);
#8801=VECTOR('',#29518,1.);
#8802=VECTOR('',#29521,1.);
#8803=VECTOR('',#29522,1.);
#8804=VECTOR('',#29527,1.);
#8805=VECTOR('',#29528,1.);
#8806=VECTOR('',#29529,1.);
#8807=VECTOR('',#29530,1.);
#8808=VECTOR('',#29533,1.);
#8809=VECTOR('',#29540,1.);
#8810=VECTOR('',#29541,1.);
#8811=VECTOR('',#29542,1.);
#8812=VECTOR('',#29545,1.);
#8813=VECTOR('',#29554,1.);
#8814=VECTOR('',#29555,1.);
#8815=VECTOR('',#29556,1.);
#8816=VECTOR('',#29557,1.);
#8817=VECTOR('',#29560,1.);
#8818=VECTOR('',#29565,1.);
#8819=VECTOR('',#29566,1.);
#8820=VECTOR('',#29573,1.);
#8821=VECTOR('',#29574,1.);
#8822=VECTOR('',#29575,1.);
#8823=VECTOR('',#29582,1.);
#8824=VECTOR('',#29587,1.);
#8825=VECTOR('',#29588,1.);
#8826=VECTOR('',#29591,1.);
#8827=VECTOR('',#29600,1.);
#8828=VECTOR('',#29601,1.);
#8829=VECTOR('',#29604,0.605);
#8830=VECTOR('',#29613,1.);
#8831=VECTOR('',#29614,1.);
#8832=VECTOR('',#29615,1.);
#8833=VECTOR('',#29616,1.);
#8834=VECTOR('',#29617,1.);
#8835=VECTOR('',#29620,1.);
#8836=VECTOR('',#29621,1.);
#8837=VECTOR('',#29622,1.);
#8838=VECTOR('',#29625,1.);
#8839=VECTOR('',#29626,1.);
#8840=VECTOR('',#29627,1.);
#8841=VECTOR('',#29628,1.);
#8842=VECTOR('',#29631,1.);
#8843=VECTOR('',#29632,1.);
#8844=VECTOR('',#29633,1.);
#8845=VECTOR('',#29634,1.);
#8846=VECTOR('',#29635,1.);
#8847=VECTOR('',#29638,1.);
#8848=VECTOR('',#29639,1.);
#8849=VECTOR('',#29640,1.);
#8850=VECTOR('',#29641,1.);
#8851=VECTOR('',#29644,1.);
#8852=VECTOR('',#29645,1.);
#8853=VECTOR('',#29646,1.);
#8854=VECTOR('',#29647,1.);
#8855=VECTOR('',#29650,1.);
#8856=VECTOR('',#29651,1.);
#8857=VECTOR('',#29652,1.);
#8858=VECTOR('',#29655,1.);
#8859=VECTOR('',#29656,1.);
#8860=VECTOR('',#29657,1.);
#8861=VECTOR('',#29660,1.);
#8862=VECTOR('',#29661,1.);
#8863=VECTOR('',#29662,1.);
#8864=VECTOR('',#29665,1.);
#8865=VECTOR('',#29666,1.);
#8866=VECTOR('',#29669,1.);
#8867=VECTOR('',#29672,1.);
#8868=VECTOR('',#29675,1.);
#8869=VECTOR('',#29676,1.);
#8870=VECTOR('',#29679,1.);
#8871=VECTOR('',#29684,1.);
#8872=VECTOR('',#29685,1.);
#8873=VECTOR('',#29688,1.);
#8874=VECTOR('',#29693,1.);
#8875=VECTOR('',#29694,1.);
#8876=VECTOR('',#29697,1.);
#8877=VECTOR('',#29702,1.);
#8878=VECTOR('',#29705,1.);
#8879=VECTOR('',#29706,1.);
#8880=VECTOR('',#29707,1.);
#8881=VECTOR('',#29710,1.);
#8882=VECTOR('',#29715,1.);
#8883=VECTOR('',#29716,1.);
#8884=VECTOR('',#29719,1.);
#8885=VECTOR('',#29724,1.);
#8886=VECTOR('',#29725,1.);
#8887=VECTOR('',#29726,1.);
#8888=VECTOR('',#29729,1.);
#8889=VECTOR('',#29738,1.);
#8890=VECTOR('',#29739,1.);
#8891=VECTOR('',#29740,1.);
#8892=VECTOR('',#29741,1.);
#8893=VECTOR('',#29744,1.);
#8894=VECTOR('',#29751,1.);
#8895=VECTOR('',#29752,1.);
#8896=VECTOR('',#29755,1.);
#8897=VECTOR('',#29760,1.);
#8898=VECTOR('',#29761,1.);
#8899=VECTOR('',#29762,1.);
#8900=VECTOR('',#29769,1.);
#8901=VECTOR('',#29770,1.);
#8902=VECTOR('',#29771,1.);
#8903=VECTOR('',#29778,1.);
#8904=VECTOR('',#29783,1.);
#8905=VECTOR('',#29784,1.);
#8906=VECTOR('',#29785,1.);
#8907=VECTOR('',#29786,1.);
#8908=VECTOR('',#29789,1.);
#8909=VECTOR('',#29794,1.);
#8910=VECTOR('',#29795,1.);
#8911=VECTOR('',#29798,1.);
#8912=VECTOR('',#29805,1.);
#8913=VECTOR('',#29806,1.);
#8914=VECTOR('',#29813,1.);
#8915=VECTOR('',#29814,1.);
#8916=VECTOR('',#29817,1.);
#8917=VECTOR('',#29822,1.);
#8918=VECTOR('',#29823,1.);
#8919=VECTOR('',#29830,1.);
#8920=VECTOR('',#29831,1.);
#8921=VECTOR('',#29832,1.);
#8922=VECTOR('',#29835,1.);
#8923=VECTOR('',#29836,1.);
#8924=VECTOR('',#29837,1.);
#8925=VECTOR('',#29840,1.);
#8926=VECTOR('',#29841,1.);
#8927=VECTOR('',#29842,1.);
#8928=VECTOR('',#29845,1.);
#8929=VECTOR('',#29852,1.);
#8930=VECTOR('',#29853,1.);
#8931=VECTOR('',#29854,1.);
#8932=VECTOR('',#29857,1.);
#8933=VECTOR('',#29864,1.);
#8934=VECTOR('',#29865,1.);
#8935=VECTOR('',#29868,1.);
#8936=VECTOR('',#29869,1.);
#8937=VECTOR('',#29872,1.);
#8938=VECTOR('',#29873,1.);
#8939=VECTOR('',#29874,1.);
#8940=VECTOR('',#29875,1.);
#8941=VECTOR('',#29878,1.);
#8942=VECTOR('',#29879,1.);
#8943=VECTOR('',#29880,1.);
#8944=VECTOR('',#29881,1.);
#8945=VECTOR('',#29884,1.);
#8946=VECTOR('',#29885,1.);
#8947=VECTOR('',#29888,1.);
#8948=VECTOR('',#29891,1.);
#8949=VECTOR('',#29892,1.);
#8950=VECTOR('',#29895,1.);
#8951=VECTOR('',#29900,1.);
#8952=VECTOR('',#29901,1.);
#8953=VECTOR('',#29904,1.);
#8954=VECTOR('',#29911,1.);
#8955=VECTOR('',#29914,1.);
#8956=VECTOR('',#29915,1.);
#8957=VECTOR('',#29918,1.);
#8958=VECTOR('',#29919,1.);
#8959=VECTOR('',#29922,1.);
#8960=VECTOR('',#29925,1.);
#8961=VECTOR('',#29926,1.);
#8962=VECTOR('',#29929,1.);
#8963=VECTOR('',#29930,1.);
#8964=VECTOR('',#29933,1.);
#8965=VECTOR('',#29936,1.);
#8966=VECTOR('',#29941,1.);
#8967=VECTOR('',#29944,1.);
#8968=VECTOR('',#29993,1.);
#8969=VECTOR('',#29996,1.);
#8970=VECTOR('',#29999,1.);
#8971=VECTOR('',#30004,1.);
#8972=VECTOR('',#30007,1.);
#8973=VECTOR('',#30010,1.);
#8974=VECTOR('',#30015,1.);
#8975=VECTOR('',#30018,1.);
#8976=VECTOR('',#30021,1.);
#8977=VECTOR('',#30028,0.605);
#8978=VECTOR('',#30031,0.875);
#8979=VECTOR('',#30034,0.252500000000001);
#8980=VECTOR('',#30037,0.252500000000001);
#8981=VECTOR('',#30040,0.2525);
#8982=VECTOR('',#30043,0.2525);
#8983=VECTOR('',#30046,1.);
#8984=VECTOR('',#30047,1.);
#8985=VECTOR('',#30050,1.);
#8986=VECTOR('',#30061,1.69267766952967);
#8987=VECTOR('',#30068,1.75);
#8988=VECTOR('',#30079,1.78232233047033);
#8989=VECTOR('',#30086,1.8);
#8990=VECTOR('',#30091,0.330000000000001);
#8991=VECTOR('',#30104,5.4);
#8992=VECTOR('',#30119,0.305);
#8993=VECTOR('',#30124,0.329999999999999);
#8994=VECTOR('',#30133,0.305);
#8995=VECTOR('',#30136,1.);
#8996=VECTOR('',#30137,1.);
#8997=VECTOR('',#30138,1.);
#8998=VECTOR('',#30139,1.);
#8999=VECTOR('',#30140,1.);
#9000=VECTOR('',#30141,1.);
#9001=VECTOR('',#30144,1.);
#9002=VECTOR('',#30147,1.);
#9003=VECTOR('',#30150,1.);
#9004=VECTOR('',#30151,1.);
#9005=VECTOR('',#30154,1.);
#9006=VECTOR('',#30157,1.);
#9007=VECTOR('',#30160,1.);
#9008=VECTOR('',#30165,1.);
#9009=VECTOR('',#30166,1.);
#9010=VECTOR('',#30167,1.);
#9011=VECTOR('',#30170,1.);
#9012=VECTOR('',#30171,1.);
#9013=VECTOR('',#30172,1.);
#9014=VECTOR('',#30177,5.29267766952966);
#9015=VECTOR('',#30182,5.4);
#9016=VECTOR('',#30189,1.);
#9017=VECTOR('',#30196,5.5);
#9018=VECTOR('',#30197,1.);
#9019=VECTOR('',#30198,1.);
#9020=VECTOR('',#30203,0.700000000000003);
#9021=VECTOR('',#30208,5.48232233047034);
#9022=VECTOR('',#30211,1.);
#9023=VECTOR('',#30212,1.);
#9024=VECTOR('',#30213,1.);
#9025=VECTOR('',#30214,1.);
#9026=VECTOR('',#30217,1.);
#9027=VECTOR('',#30218,1.);
#9028=VECTOR('',#30219,1.);
#9029=VECTOR('',#30224,1.);
#9030=VECTOR('',#30227,1.);
#9031=VECTOR('',#30228,1.);
#9032=VECTOR('',#30229,1.);
#9033=VECTOR('',#30232,1.);
#9034=VECTOR('',#30233,1.);
#9035=VECTOR('',#30234,1.);
#9036=VECTOR('',#30237,1.);
#9037=VECTOR('',#30238,1.);
#9038=VECTOR('',#30239,1.);
#9039=VECTOR('',#30242,1.);
#9040=VECTOR('',#30243,1.);
#9041=VECTOR('',#30244,1.);
#9042=VECTOR('',#30247,1.);
#9043=VECTOR('',#30248,1.);
#9044=VECTOR('',#30249,1.);
#9045=VECTOR('',#30252,1.);
#9046=VECTOR('',#30253,1.);
#9047=VECTOR('',#30254,1.);
#9048=VECTOR('',#30257,1.);
#9049=VECTOR('',#30258,1.);
#9050=VECTOR('',#30259,1.);
#9051=VECTOR('',#30262,1.);
#9052=VECTOR('',#30269,1.);
#9053=VECTOR('',#30270,1.);
#9054=VECTOR('',#30271,1.);
#9055=VECTOR('',#30274,1.);
#9056=VECTOR('',#30281,1.);
#9057=VECTOR('',#30282,1.);
#9058=VECTOR('',#30285,1.);
#9059=VECTOR('',#30286,1.);
#9060=VECTOR('',#30287,1.);
#9061=VECTOR('',#30290,1.);
#9062=VECTOR('',#30291,1.);
#9063=VECTOR('',#30294,1.);
#9064=VECTOR('',#30295,1.);
#9065=VECTOR('',#30298,1.);
#9066=VECTOR('',#30299,1.);
#9067=VECTOR('',#30304,1.);
#9068=VECTOR('',#30307,1.);
#9069=VECTOR('',#30310,1.);
#9070=VECTOR('',#30313,1.);
#9071=VECTOR('',#30314,1.);
#9072=VECTOR('',#30315,1.);
#9073=VECTOR('',#30318,1.);
#9074=VECTOR('',#30323,1.);
#9075=VECTOR('',#30324,1.);
#9076=VECTOR('',#30325,1.);
#9077=VECTOR('',#30326,1.);
#9078=VECTOR('',#30327,1.);
#9079=VECTOR('',#30330,1.);
#9080=VECTOR('',#30331,1.);
#9081=VECTOR('',#30332,1.);
#9082=VECTOR('',#30333,1.);
#9083=VECTOR('',#30336,1.);
#9084=VECTOR('',#30337,1.);
#9085=VECTOR('',#30342,1.);
#9086=VECTOR('',#30345,1.);
#9087=VECTOR('',#30350,1.);
#9088=VECTOR('',#30353,1.);
#9089=VECTOR('',#30356,1.);
#9090=VECTOR('',#30359,1.);
#9091=VECTOR('',#30364,1.);
#9092=VECTOR('',#30365,1.);
#9093=VECTOR('',#30366,1.);
#9094=VECTOR('',#30369,1.);
#9095=VECTOR('',#30374,1.);
#9096=VECTOR('',#30375,1.);
#9097=VECTOR('',#30382,1.);
#9098=VECTOR('',#30385,1.);
#9099=VECTOR('',#30388,1.);
#9100=VECTOR('',#30389,1.);
#9101=VECTOR('',#30392,1.);
#9102=VECTOR('',#30393,1.);
#9103=VECTOR('',#30394,1.);
#9104=VECTOR('',#30397,1.);
#9105=VECTOR('',#30402,1.);
#9106=VECTOR('',#30403,1.);
#9107=VECTOR('',#30410,1.);
#9108=VECTOR('',#30413,1.);
#9109=VECTOR('',#30416,1.);
#9110=VECTOR('',#30417,1.);
#9111=VECTOR('',#30420,1.);
#9112=VECTOR('',#30421,1.);
#9113=VECTOR('',#30422,1.);
#9114=VECTOR('',#30425,1.);
#9115=VECTOR('',#30430,1.);
#9116=VECTOR('',#30431,1.);
#9117=VECTOR('',#30438,1.);
#9118=VECTOR('',#30441,1.);
#9119=VECTOR('',#30444,1.);
#9120=VECTOR('',#30445,1.);
#9121=VECTOR('',#30448,1.);
#9122=VECTOR('',#30449,1.);
#9123=VECTOR('',#30450,1.);
#9124=VECTOR('',#30453,1.);
#9125=VECTOR('',#30458,1.);
#9126=VECTOR('',#30459,1.);
#9127=VECTOR('',#30466,1.);
#9128=VECTOR('',#30469,1.);
#9129=VECTOR('',#30472,1.);
#9130=VECTOR('',#30473,1.);
#9131=VECTOR('',#30478,0.330000000000001);
#9132=VECTOR('',#30489,0.305);
#9133=VECTOR('',#30494,0.33);
#9134=VECTOR('',#30503,0.305);
#9135=VECTOR('',#30506,1.);
#9136=VECTOR('',#30507,1.);
#9137=VECTOR('',#30508,1.);
#9138=VECTOR('',#30511,1.);
#9139=VECTOR('',#30518,1.);
#9140=VECTOR('',#30519,1.);
#9141=VECTOR('',#30520,1.);
#9142=VECTOR('',#30527,1.);
#9143=VECTOR('',#30530,1.);
#9144=VECTOR('',#30531,1.);
#9145=VECTOR('',#30532,1.);
#9146=VECTOR('',#30533,1.);
#9147=VECTOR('',#30534,1.);
#9148=VECTOR('',#30535,1.);
#9149=VECTOR('',#30536,1.);
#9150=VECTOR('',#30537,1.);
#9151=VECTOR('',#30538,1.);
#9152=VECTOR('',#30539,1.);
#9153=VECTOR('',#30540,1.);
#9154=VECTOR('',#30543,1.);
#9155=VECTOR('',#30546,1.);
#9156=VECTOR('',#30549,1.);
#9157=VECTOR('',#30552,1.);
#9158=VECTOR('',#30555,1.);
#9159=VECTOR('',#30558,1.);
#9160=VECTOR('',#30561,1.);
#9161=VECTOR('',#30564,1.);
#9162=VECTOR('',#30567,1.);
#9163=VECTOR('',#30572,1.);
#9164=VECTOR('',#30573,1.);
#9165=VECTOR('',#30576,1.);
#9166=VECTOR('',#30581,1.);
#9167=VECTOR('',#30582,1.);
#9168=VECTOR('',#30587,1.);
#9169=VECTOR('',#30590,1.);
#9170=VECTOR('',#30591,1.);
#9171=VECTOR('',#30594,1.);
#9172=VECTOR('',#30599,1.);
#9173=VECTOR('',#30600,1.);
#9174=VECTOR('',#30605,1.);
#9175=VECTOR('',#30608,1.);
#9176=VECTOR('',#30609,1.);
#9177=VECTOR('',#30612,1.);
#9178=VECTOR('',#30617,1.);
#9179=VECTOR('',#30618,1.);
#9180=VECTOR('',#30623,1.);
#9181=VECTOR('',#30624,1.);
#9182=VECTOR('',#30627,1.);
#9183=VECTOR('',#30628,1.);
#9184=VECTOR('',#30633,1.);
#9185=VECTOR('',#30634,1.);
#9186=VECTOR('',#30637,1.);
#9187=VECTOR('',#30642,1.);
#9188=VECTOR('',#30643,1.);
#9189=VECTOR('',#30646,1.);
#9190=VECTOR('',#30651,1.);
#9191=VECTOR('',#30654,1.);
#9192=VECTOR('',#30655,1.);
#9193=VECTOR('',#30662,1.);
#9194=VECTOR('',#30665,1.);
#9195=VECTOR('',#30668,1.);
#9196=VECTOR('',#30671,1.);
#9197=VECTOR('',#30674,1.);
#9198=VECTOR('',#30675,1.);
#9199=VECTOR('',#30680,1.);
#9200=VECTOR('',#30683,1.);
#9201=VECTOR('',#30684,1.);
#9202=VECTOR('',#30687,1.);
#9203=VECTOR('',#30688,1.);
#9204=VECTOR('',#30691,1.);
#9205=VECTOR('',#30696,1.);
#9206=VECTOR('',#30699,1.);
#9207=VECTOR('',#30700,1.);
#9208=VECTOR('',#30705,1.);
#9209=VECTOR('',#30712,1.);
#9210=VECTOR('',#30715,1.);
#9211=VECTOR('',#30726,1.);
#9212=VECTOR('',#30761,0.1525);
#9213=VECTOR('',#30764,0.1525);
#9214=VECTOR('',#30767,0.1525);
#9215=VECTOR('',#30770,0.1525);
#9216=VECTOR('',#30777,0.405000000000001);
#9217=VECTOR('',#30780,1.005);
#9218=VECTOR('',#30789,0.605000000000004);
#9219=VECTOR('',#30794,3.5);
#9220=VECTOR('',#30803,3.08422464300993);
#9221=VECTOR('',#30810,3.2985);
#9222=VECTOR('',#30819,1.);
#9223=VECTOR('',#30820,1.);
#9224=VECTOR('',#30821,1.);
#9225=VECTOR('',#30822,1.);
#9226=VECTOR('',#30827,1.);
#9227=VECTOR('',#30828,1.);
#9228=VECTOR('',#30831,1.);
#9229=VECTOR('',#30832,1.);
#9230=VECTOR('',#30833,1.);
#9231=VECTOR('',#30838,1.);
#9232=VECTOR('',#30843,1.);
#9233=VECTOR('',#30844,1.);
#9234=VECTOR('',#30845,1.);
#9235=VECTOR('',#30846,1.);
#9236=VECTOR('',#30851,1.);
#9237=VECTOR('',#30852,1.);
#9238=VECTOR('',#30855,1.);
#9239=VECTOR('',#30856,1.);
#9240=VECTOR('',#30857,1.);
#9241=VECTOR('',#30862,1.);
#9242=VECTOR('',#30867,1.);
#9243=VECTOR('',#30868,1.);
#9244=VECTOR('',#30869,1.);
#9245=VECTOR('',#30870,1.);
#9246=VECTOR('',#30875,1.);
#9247=VECTOR('',#30876,1.);
#9248=VECTOR('',#30879,1.);
#9249=VECTOR('',#30880,1.);
#9250=VECTOR('',#30881,1.);
#9251=VECTOR('',#30886,1.);
#9252=VECTOR('',#30891,1.);
#9253=VECTOR('',#30892,1.);
#9254=VECTOR('',#30893,1.);
#9255=VECTOR('',#30894,1.);
#9256=VECTOR('',#30899,1.);
#9257=VECTOR('',#30900,1.);
#9258=VECTOR('',#30903,1.);
#9259=VECTOR('',#30904,1.);
#9260=VECTOR('',#30905,1.);
#9261=VECTOR('',#30910,1.);
#9262=VECTOR('',#30915,1.);
#9263=VECTOR('',#30916,1.);
#9264=VECTOR('',#30917,1.);
#9265=VECTOR('',#30918,1.);
#9266=VECTOR('',#30923,1.);
#9267=VECTOR('',#30924,1.);
#9268=VECTOR('',#30927,1.);
#9269=VECTOR('',#30928,1.);
#9270=VECTOR('',#30929,1.);
#9271=VECTOR('',#30934,1.);
#9272=VECTOR('',#30939,1.);
#9273=VECTOR('',#30940,1.);
#9274=VECTOR('',#30941,1.);
#9275=VECTOR('',#30942,1.);
#9276=VECTOR('',#30947,1.);
#9277=VECTOR('',#30948,1.);
#9278=VECTOR('',#30951,1.);
#9279=VECTOR('',#30952,1.);
#9280=VECTOR('',#30953,1.);
#9281=VECTOR('',#30958,1.);
#9282=VECTOR('',#30963,1.);
#9283=VECTOR('',#30964,1.);
#9284=VECTOR('',#30965,1.);
#9285=VECTOR('',#30966,1.);
#9286=VECTOR('',#30971,1.);
#9287=VECTOR('',#30972,1.);
#9288=VECTOR('',#30975,1.);
#9289=VECTOR('',#30976,1.);
#9290=VECTOR('',#30977,1.);
#9291=VECTOR('',#30982,1.);
#9292=VECTOR('',#30987,1.);
#9293=VECTOR('',#30988,1.);
#9294=VECTOR('',#30989,1.);
#9295=VECTOR('',#30990,1.);
#9296=VECTOR('',#30995,1.);
#9297=VECTOR('',#30996,1.);
#9298=VECTOR('',#30999,1.);
#9299=VECTOR('',#31000,1.);
#9300=VECTOR('',#31001,1.);
#9301=VECTOR('',#31006,1.);
#9302=VECTOR('',#31011,1.);
#9303=VECTOR('',#31012,1.);
#9304=VECTOR('',#31013,1.);
#9305=VECTOR('',#31014,1.);
#9306=VECTOR('',#31019,1.);
#9307=VECTOR('',#31020,1.);
#9308=VECTOR('',#31023,1.);
#9309=VECTOR('',#31024,1.);
#9310=VECTOR('',#31025,1.);
#9311=VECTOR('',#31030,1.);
#9312=VECTOR('',#31035,1.);
#9313=VECTOR('',#31036,1.);
#9314=VECTOR('',#31037,1.);
#9315=VECTOR('',#31038,1.);
#9316=VECTOR('',#31043,1.);
#9317=VECTOR('',#31044,1.);
#9318=VECTOR('',#31047,1.);
#9319=VECTOR('',#31048,1.);
#9320=VECTOR('',#31049,1.);
#9321=VECTOR('',#31054,1.);
#9322=VECTOR('',#31059,1.);
#9323=VECTOR('',#31060,1.);
#9324=VECTOR('',#31061,1.);
#9325=VECTOR('',#31062,1.);
#9326=VECTOR('',#31067,1.);
#9327=VECTOR('',#31068,1.);
#9328=VECTOR('',#31071,1.);
#9329=VECTOR('',#31072,1.);
#9330=VECTOR('',#31073,1.);
#9331=VECTOR('',#31078,1.);
#9332=VECTOR('',#31083,1.);
#9333=VECTOR('',#31084,1.);
#9334=VECTOR('',#31085,1.);
#9335=VECTOR('',#31086,1.);
#9336=VECTOR('',#31091,1.);
#9337=VECTOR('',#31092,1.);
#9338=VECTOR('',#31095,1.);
#9339=VECTOR('',#31096,1.);
#9340=VECTOR('',#31097,1.);
#9341=VECTOR('',#31102,1.);
#9342=VECTOR('',#31107,1.);
#9343=VECTOR('',#31108,1.);
#9344=VECTOR('',#31109,1.);
#9345=VECTOR('',#31110,1.);
#9346=VECTOR('',#31115,1.);
#9347=VECTOR('',#31116,1.);
#9348=VECTOR('',#31119,1.);
#9349=VECTOR('',#31120,1.);
#9350=VECTOR('',#31121,1.);
#9351=VECTOR('',#31126,1.);
#9352=VECTOR('',#31131,1.);
#9353=VECTOR('',#31132,1.);
#9354=VECTOR('',#31133,1.);
#9355=VECTOR('',#31134,1.);
#9356=VECTOR('',#31139,1.);
#9357=VECTOR('',#31140,1.);
#9358=VECTOR('',#31143,1.);
#9359=VECTOR('',#31144,1.);
#9360=VECTOR('',#31145,1.);
#9361=VECTOR('',#31150,1.);
#9362=VECTOR('',#31155,1.);
#9363=VECTOR('',#31156,1.);
#9364=VECTOR('',#31157,1.);
#9365=VECTOR('',#31158,1.);
#9366=VECTOR('',#31163,1.);
#9367=VECTOR('',#31164,1.);
#9368=VECTOR('',#31167,1.);
#9369=VECTOR('',#31168,1.);
#9370=VECTOR('',#31169,1.);
#9371=VECTOR('',#31174,1.);
#9372=VECTOR('',#31179,1.);
#9373=VECTOR('',#31180,1.);
#9374=VECTOR('',#31181,1.);
#9375=VECTOR('',#31182,1.);
#9376=VECTOR('',#31187,1.);
#9377=VECTOR('',#31188,1.);
#9378=VECTOR('',#31191,1.);
#9379=VECTOR('',#31192,1.);
#9380=VECTOR('',#31193,1.);
#9381=VECTOR('',#31198,1.);
#9382=VECTOR('',#31203,1.);
#9383=VECTOR('',#31204,1.);
#9384=VECTOR('',#31205,1.);
#9385=VECTOR('',#31206,1.);
#9386=VECTOR('',#31211,1.);
#9387=VECTOR('',#31212,1.);
#9388=VECTOR('',#31215,1.);
#9389=VECTOR('',#31216,1.);
#9390=VECTOR('',#31217,1.);
#9391=VECTOR('',#31222,1.);
#9392=VECTOR('',#31227,1.);
#9393=VECTOR('',#31228,1.);
#9394=VECTOR('',#31229,1.);
#9395=VECTOR('',#31230,1.);
#9396=VECTOR('',#31235,1.);
#9397=VECTOR('',#31236,1.);
#9398=VECTOR('',#31239,1.);
#9399=VECTOR('',#31240,1.);
#9400=VECTOR('',#31241,1.);
#9401=VECTOR('',#31246,1.);
#9402=VECTOR('',#31251,1.);
#9403=VECTOR('',#31252,1.);
#9404=VECTOR('',#31253,1.);
#9405=VECTOR('',#31254,1.);
#9406=VECTOR('',#31259,1.);
#9407=VECTOR('',#31260,1.);
#9408=VECTOR('',#31263,1.);
#9409=VECTOR('',#31264,1.);
#9410=VECTOR('',#31265,1.);
#9411=VECTOR('',#31270,1.);
#9412=VECTOR('',#31275,1.);
#9413=VECTOR('',#31276,1.);
#9414=VECTOR('',#31277,1.);
#9415=VECTOR('',#31278,1.);
#9416=VECTOR('',#31283,1.);
#9417=VECTOR('',#31284,1.);
#9418=VECTOR('',#31287,1.);
#9419=VECTOR('',#31288,1.);
#9420=VECTOR('',#31289,1.);
#9421=VECTOR('',#31294,1.);
#9422=VECTOR('',#31299,1.);
#9423=VECTOR('',#31300,1.);
#9424=VECTOR('',#31301,1.);
#9425=VECTOR('',#31302,1.);
#9426=VECTOR('',#31307,1.);
#9427=VECTOR('',#31308,1.);
#9428=VECTOR('',#31311,1.);
#9429=VECTOR('',#31312,1.);
#9430=VECTOR('',#31313,1.);
#9431=VECTOR('',#31318,1.);
#9432=VECTOR('',#31323,1.);
#9433=VECTOR('',#31324,1.);
#9434=VECTOR('',#31325,1.);
#9435=VECTOR('',#31326,1.);
#9436=VECTOR('',#31331,1.);
#9437=VECTOR('',#31334,1.);
#9438=VECTOR('',#31335,1.);
#9439=VECTOR('',#31336,1.);
#9440=VECTOR('',#31347,2.);
#9441=VECTOR('',#31358,3.447);
#9442=VECTOR('',#31361,3.497);
#9443=VECTOR('',#31364,1.6023112);
#9444=VECTOR('',#31369,1.4090882);
#9445=VECTOR('',#31378,1.1);
#9446=VECTOR('',#31391,1.63201114386566);
#9447=VECTOR('',#31398,1.60375905110103);
#9448=VECTOR('',#31403,1.64516810220205);
#9449=VECTOR('',#31412,1.2192801);
#9450=VECTOR('',#31415,1.41081505);
#9451=VECTOR('',#31420,1.);
#9452=VECTOR('',#31425,1.);
#9453=VECTOR('',#31428,1.);
#9454=VECTOR('',#31431,1.);
#9455=VECTOR('',#31434,1.);
#9456=VECTOR('',#31437,1.);
#9457=VECTOR('',#31440,1.);
#9458=VECTOR('',#31443,1.);
#9459=VECTOR('',#31446,1.);
#9460=VECTOR('',#31449,1.);
#9461=VECTOR('',#31452,1.);
#9462=VECTOR('',#31455,1.);
#9463=VECTOR('',#31458,1.);
#9464=VECTOR('',#31461,1.);
#9465=VECTOR('',#31464,1.);
#9466=VECTOR('',#31467,1.);
#9467=VECTOR('',#31470,1.);
#9468=VECTOR('',#31473,1.);
#9469=VECTOR('',#31476,1.);
#9470=VECTOR('',#31479,1.);
#9471=VECTOR('',#31482,1.);
#9472=VECTOR('',#31485,1.);
#9473=VECTOR('',#31488,1.);
#9474=VECTOR('',#31491,1.);
#9475=VECTOR('',#31494,1.);
#9476=VECTOR('',#31497,1.);
#9477=VECTOR('',#31500,1.);
#9478=VECTOR('',#31503,1.);
#9479=VECTOR('',#31506,1.);
#9480=VECTOR('',#31509,1.);
#9481=VECTOR('',#31512,1.);
#9482=VECTOR('',#31515,1.);
#9483=VECTOR('',#31518,1.);
#9484=VECTOR('',#31521,1.);
#9485=VECTOR('',#31524,1.);
#9486=VECTOR('',#31527,1.);
#9487=VECTOR('',#31530,1.);
#9488=VECTOR('',#31533,1.);
#9489=VECTOR('',#31536,1.);
#9490=VECTOR('',#31539,1.);
#9491=VECTOR('',#31542,1.);
#9492=VECTOR('',#31545,1.);
#9493=VECTOR('',#31548,0.76435);
#9494=VECTOR('',#31553,0.76435);
#9495=VECTOR('',#31556,0.76435);
#9496=VECTOR('',#31559,0.76435);
#9497=VECTOR('',#31562,0.76435);
#9498=VECTOR('',#31565,0.76435);
#9499=VECTOR('',#31568,0.76435);
#9500=VECTOR('',#31571,0.76435);
#9501=VECTOR('',#31574,0.76435);
#9502=VECTOR('',#31577,0.76435);
#9503=VECTOR('',#31580,0.76435);
#9504=VECTOR('',#31583,0.76435);
#9505=VECTOR('',#31586,0.76435);
#9506=VECTOR('',#31589,0.76435);
#9507=VECTOR('',#31592,0.76435);
#9508=VECTOR('',#31595,0.76435);
#9509=VECTOR('',#31598,0.76435);
#9510=VECTOR('',#31601,0.76435);
#9511=VECTOR('',#31604,0.76435);
#9512=VECTOR('',#31607,0.76435);
#9513=VECTOR('',#31610,0.76435);
#9514=VECTOR('',#31613,0.76435);
#9515=VECTOR('',#31616,0.76435);
#9516=VECTOR('',#31619,0.76435);
#9517=VECTOR('',#31622,0.76435);
#9518=VECTOR('',#31625,0.76435);
#9519=VECTOR('',#31628,0.76435);
#9520=VECTOR('',#31631,0.76435);
#9521=VECTOR('',#31634,0.76435);
#9522=VECTOR('',#31637,0.76435);
#9523=VECTOR('',#31640,0.76435);
#9524=VECTOR('',#31643,0.76435);
#9525=VECTOR('',#31646,0.76435);
#9526=VECTOR('',#31649,0.76435);
#9527=VECTOR('',#31652,0.76435);
#9528=VECTOR('',#31655,0.76435);
#9529=VECTOR('',#31658,0.76435);
#9530=VECTOR('',#31661,0.76435);
#9531=VECTOR('',#31664,0.76435);
#9532=VECTOR('',#31667,0.76435);
#9533=VECTOR('',#31670,0.76435);
#9534=VECTOR('',#31673,0.76435);
#9535=VECTOR('',#31678,0.892677669529664);
#9536=VECTOR('',#31685,0.95);
#9537=VECTOR('',#31698,0.430000000000001);
#9538=VECTOR('',#31705,0.405000000000001);
#9539=VECTOR('',#31728,0.202500000000001);
#9540=VECTOR('',#31731,1.);
#9541=VECTOR('',#31732,1.);
#9542=VECTOR('',#31733,1.);
#9543=VECTOR('',#31734,1.);
#9544=VECTOR('',#31739,1.);
#9545=VECTOR('',#31742,1.);
#9546=VECTOR('',#31743,1.);
#9547=VECTOR('',#31744,1.);
#9548=VECTOR('',#31755,0.975);
#9549=VECTOR('',#31760,1.);
#9550=VECTOR('',#31769,1.575);
#9551=VECTOR('',#31774,1.6);
#9552=VECTOR('',#31779,1.575);
#9553=VECTOR('',#31788,1.11232233047034);
#9554=VECTOR('',#31799,1.055);
#9555=VECTOR('',#31806,1.02267766952966);
#9556=VECTOR('',#31815,1.005);
#9557=VECTOR('',#31826,1.92);
#9558=VECTOR('',#31833,2.);
#9559=VECTOR('',#31838,1.975);
#9560=VECTOR('',#31843,2.);
#9561=VECTOR('',#31848,1.975);
#9562=VECTOR('',#31855,1.055);
#9563=VECTOR('',#31864,1.825);
#9564=VECTOR('',#31873,1.8);
#9565=VECTOR('',#31880,6.14267766952966);
#9566=VECTOR('',#31887,6.2);
#9567=VECTOR('',#31906,6.23232233047034);
#9568=VECTOR('',#31913,6.25);
#9569=VECTOR('',#31920,6.23232233047034);
#9570=VECTOR('',#31927,6.2);
#9571=VECTOR('',#31934,6.14267766952966);
#9572=VECTOR('',#31955,2.78232233047034);
#9573=VECTOR('',#31962,2.75);
#9574=VECTOR('',#31969,2.8);
#9575=VECTOR('',#31972,2.69267766952966);
#9576=VECTOR('',#31981,1.825);
#9577=VECTOR('',#31990,1.8);
#9578=VECTOR('',#31993,0.330000000000002);
#9579=VECTOR('',#31996,0.330000000000002);
#9580=VECTOR('',#31999,0.330000000000002);
#9581=VECTOR('',#32002,0.330000000000002);
#9582=VECTOR('',#32007,3.495);
#9583=VECTOR('',#32010,3.47);
#9584=VECTOR('',#32017,1.05);
#9585=VECTOR('',#32030,2.48232233047034);
#9586=VECTOR('',#32037,2.5);
#9587=VECTOR('',#32048,2.45);
#9588=VECTOR('',#32051,2.48232233047034);
#9589=VECTOR('',#32058,2.45);
#9590=VECTOR('',#32065,2.39267766952966);
#9591=VECTOR('',#32076,2.39267766952966);
#9592=VECTOR('',#32079,1.);
#9593=VECTOR('',#32082,1.);
#9594=VECTOR('',#32083,1.);
#9595=VECTOR('',#32086,1.);
#9596=VECTOR('',#32089,1.);
#9597=VECTOR('',#32094,1.);
#9598=VECTOR('',#32095,1.);
#9599=VECTOR('',#32098,1.);
#9600=VECTOR('',#32101,1.);
#9601=VECTOR('',#32102,1.);
#9602=VECTOR('',#32103,1.);
#9603=VECTOR('',#32106,1.);
#9604=VECTOR('',#32107,1.);
#9605=VECTOR('',#32110,1.);
#9606=VECTOR('',#32111,1.);
#9607=VECTOR('',#32118,0.775);
#9608=VECTOR('',#32121,0.775);
#9609=VECTOR('',#32124,0.775000000000002);
#9610=VECTOR('',#32127,0.774999999999997);
#9611=VECTOR('',#32146,0.46);
#9612=VECTOR('',#32153,0.4);
#9613=VECTOR('',#32158,0.4);
#9614=VECTOR('',#32161,0.4);
#9615=VECTOR('',#32164,0.4);
#9616=VECTOR('',#32167,0.4);
#9617=VECTOR('',#32170,0.4);
#9618=VECTOR('',#32173,0.4);
#9619=VECTOR('',#32176,0.4);
#9620=VECTOR('',#32179,0.4);
#9621=VECTOR('',#32182,0.4);
#9622=VECTOR('',#32185,0.4);
#9623=VECTOR('',#32188,0.4);
#9624=VECTOR('',#32191,0.4);
#9625=VECTOR('',#32194,0.4);
#9626=VECTOR('',#32197,0.4);
#9627=VECTOR('',#32200,0.4);
#9628=VECTOR('',#32203,0.322275);
#9629=VECTOR('',#32208,0.322275);
#9630=VECTOR('',#32211,0.322275);
#9631=VECTOR('',#32214,0.322275);
#9632=VECTOR('',#32217,0.322275);
#9633=VECTOR('',#32220,0.322275);
#9634=VECTOR('',#32223,0.322275);
#9635=VECTOR('',#32226,0.322275);
#9636=VECTOR('',#32229,0.322275);
#9637=VECTOR('',#32232,0.322275);
#9638=VECTOR('',#32235,0.322275);
#9639=VECTOR('',#32238,0.322275);
#9640=VECTOR('',#32241,0.322275);
#9641=VECTOR('',#32244,0.322275);
#9642=VECTOR('',#32247,0.322275);
#9643=VECTOR('',#32280,1.);
#9644=VECTOR('',#32285,1.);
#9645=VECTOR('',#32290,1.);
#9646=VECTOR('',#32295,1.);
#9647=VECTOR('',#32300,1.);
#9648=VECTOR('',#32305,1.);
#9649=VECTOR('',#32310,0.173205080756888);
#9650=VECTOR('',#32313,1.);
#9651=VECTOR('',#32314,1.);
#9652=VECTOR('',#32315,1.);
#9653=VECTOR('',#32318,1.);
#9654=VECTOR('',#32319,1.);
#9655=VECTOR('',#32322,1.);
#9656=VECTOR('',#32323,1.);
#9657=VECTOR('',#32326,1.);
#9658=VECTOR('',#32327,1.);
#9659=VECTOR('',#32330,1.);
#9660=VECTOR('',#32331,1.);
#9661=VECTOR('',#32334,1.);
#9662=VECTOR('',#32337,1.);
#9663=VECTOR('',#32338,1.);
#9664=VECTOR('',#32339,1.);
#9665=VECTOR('',#32340,1.);
#9666=VECTOR('',#32345,1.);
#9667=VECTOR('',#32348,1.);
#9668=VECTOR('',#32349,1.);
#9669=VECTOR('',#32356,1.);
#9670=VECTOR('',#32357,1.);
#9671=VECTOR('',#32358,1.);
#9672=VECTOR('',#32359,1.);
#9673=VECTOR('',#32364,1.);
#9674=VECTOR('',#32367,1.);
#9675=VECTOR('',#32368,1.);
#9676=VECTOR('',#32375,1.);
#9677=VECTOR('',#32376,1.);
#9678=VECTOR('',#32377,1.);
#9679=VECTOR('',#32378,1.);
#9680=VECTOR('',#32383,1.);
#9681=VECTOR('',#32386,1.);
#9682=VECTOR('',#32387,1.);
#9683=VECTOR('',#32394,1.);
#9684=VECTOR('',#32395,1.);
#9685=VECTOR('',#32396,1.);
#9686=VECTOR('',#32397,1.);
#9687=VECTOR('',#32402,1.);
#9688=VECTOR('',#32405,1.);
#9689=VECTOR('',#32406,1.);
#9690=VECTOR('',#32413,1.);
#9691=VECTOR('',#32414,1.);
#9692=VECTOR('',#32415,1.);
#9693=VECTOR('',#32416,1.);
#9694=VECTOR('',#32421,1.);
#9695=VECTOR('',#32424,1.);
#9696=VECTOR('',#32425,1.);
#9697=VECTOR('',#32432,1.);
#9698=VECTOR('',#32433,1.);
#9699=VECTOR('',#32434,1.);
#9700=VECTOR('',#32435,1.);
#9701=VECTOR('',#32440,1.);
#9702=VECTOR('',#32443,1.);
#9703=VECTOR('',#32444,1.);
#9704=VECTOR('',#32451,1.);
#9705=VECTOR('',#32452,1.);
#9706=VECTOR('',#32453,1.);
#9707=VECTOR('',#32454,1.);
#9708=VECTOR('',#32459,1.);
#9709=VECTOR('',#32462,1.);
#9710=VECTOR('',#32463,1.);
#9711=VECTOR('',#32470,1.);
#9712=VECTOR('',#32471,1.);
#9713=VECTOR('',#32472,1.);
#9714=VECTOR('',#32473,1.);
#9715=VECTOR('',#32478,1.);
#9716=VECTOR('',#32481,1.);
#9717=VECTOR('',#32482,1.);
#9718=VECTOR('',#32489,1.);
#9719=VECTOR('',#32490,1.);
#9720=VECTOR('',#32491,1.);
#9721=VECTOR('',#32492,1.);
#9722=VECTOR('',#32497,1.);
#9723=VECTOR('',#32502,1.);
#9724=VECTOR('',#32503,1.);
#9725=VECTOR('',#32512,1.);
#9726=VECTOR('',#32513,1.);
#9727=VECTOR('',#32514,1.);
#9728=VECTOR('',#32515,1.);
#9729=VECTOR('',#32520,1.);
#9730=VECTOR('',#32523,1.);
#9731=VECTOR('',#32524,1.);
#9732=VECTOR('',#32531,1.);
#9733=VECTOR('',#32532,1.);
#9734=VECTOR('',#32533,1.);
#9735=VECTOR('',#32534,1.);
#9736=VECTOR('',#32539,1.);
#9737=VECTOR('',#32542,1.);
#9738=VECTOR('',#32543,1.);
#9739=VECTOR('',#32550,1.);
#9740=VECTOR('',#32551,1.);
#9741=VECTOR('',#32552,1.);
#9742=VECTOR('',#32553,1.);
#9743=VECTOR('',#32558,1.);
#9744=VECTOR('',#32561,1.);
#9745=VECTOR('',#32562,1.);
#9746=VECTOR('',#32569,1.);
#9747=VECTOR('',#32570,1.);
#9748=VECTOR('',#32571,1.);
#9749=VECTOR('',#32572,1.);
#9750=VECTOR('',#32577,1.);
#9751=VECTOR('',#32580,1.);
#9752=VECTOR('',#32581,1.);
#9753=VECTOR('',#32588,1.);
#9754=VECTOR('',#32589,1.);
#9755=VECTOR('',#32590,1.);
#9756=VECTOR('',#32591,1.);
#9757=VECTOR('',#32596,1.);
#9758=VECTOR('',#32599,1.);
#9759=VECTOR('',#32600,1.);
#9760=VECTOR('',#32607,1.);
#9761=VECTOR('',#32608,1.);
#9762=VECTOR('',#32609,1.);
#9763=VECTOR('',#32610,1.);
#9764=VECTOR('',#32615,1.);
#9765=VECTOR('',#32618,1.);
#9766=VECTOR('',#32619,1.);
#9767=VECTOR('',#32626,1.);
#9768=VECTOR('',#32627,1.);
#9769=VECTOR('',#32628,1.);
#9770=VECTOR('',#32629,1.);
#9771=VECTOR('',#32634,1.);
#9772=VECTOR('',#32637,1.);
#9773=VECTOR('',#32638,1.);
#9774=VECTOR('',#32645,1.);
#9775=VECTOR('',#32646,1.);
#9776=VECTOR('',#32647,1.);
#9777=VECTOR('',#32648,1.);
#9778=VECTOR('',#32653,1.);
#9779=VECTOR('',#32656,1.);
#9780=VECTOR('',#32657,1.);
#9781=VECTOR('',#32664,1.);
#9782=VECTOR('',#32665,1.);
#9783=VECTOR('',#32666,1.);
#9784=VECTOR('',#32667,1.);
#9785=VECTOR('',#32672,1.);
#9786=VECTOR('',#32675,1.);
#9787=VECTOR('',#32676,1.);
#9788=VECTOR('',#32683,1.);
#9789=VECTOR('',#32684,1.);
#9790=VECTOR('',#32685,1.);
#9791=VECTOR('',#32686,1.);
#9792=VECTOR('',#32691,1.);
#9793=VECTOR('',#32694,1.);
#9794=VECTOR('',#32695,1.);
#9795=VECTOR('',#32702,1.);
#9796=VECTOR('',#32703,1.);
#9797=VECTOR('',#32704,1.);
#9798=VECTOR('',#32705,1.);
#9799=VECTOR('',#32710,1.);
#9800=VECTOR('',#32713,1.);
#9801=VECTOR('',#32714,1.);
#9802=VECTOR('',#32721,1.);
#9803=VECTOR('',#32722,1.);
#9804=VECTOR('',#32723,1.);
#9805=VECTOR('',#32724,1.);
#9806=VECTOR('',#32729,1.);
#9807=VECTOR('',#32732,1.);
#9808=VECTOR('',#32733,1.);
#9809=VECTOR('',#32740,1.);
#9810=VECTOR('',#32741,1.);
#9811=VECTOR('',#32742,1.);
#9812=VECTOR('',#32743,1.);
#9813=VECTOR('',#32748,1.);
#9814=VECTOR('',#32751,1.);
#9815=VECTOR('',#32752,1.);
#9816=VECTOR('',#32759,1.);
#9817=VECTOR('',#32760,1.);
#9818=VECTOR('',#32761,1.);
#9819=VECTOR('',#32762,1.);
#9820=VECTOR('',#32767,1.);
#9821=VECTOR('',#32770,1.);
#9822=VECTOR('',#32771,1.);
#9823=VECTOR('',#32778,1.);
#9824=VECTOR('',#32779,1.);
#9825=VECTOR('',#32780,1.);
#9826=VECTOR('',#32781,1.);
#9827=VECTOR('',#32786,1.);
#9828=VECTOR('',#32789,1.);
#9829=VECTOR('',#32790,1.);
#9830=VECTOR('',#32797,1.);
#9831=VECTOR('',#32798,1.);
#9832=VECTOR('',#32799,1.);
#9833=VECTOR('',#32800,1.);
#9834=VECTOR('',#32805,1.);
#9835=VECTOR('',#32808,1.);
#9836=VECTOR('',#32809,1.);
#9837=VECTOR('',#32816,1.);
#9838=VECTOR('',#32817,1.);
#9839=VECTOR('',#32818,1.);
#9840=VECTOR('',#32819,1.);
#9841=VECTOR('',#32824,1.);
#9842=VECTOR('',#32827,1.);
#9843=VECTOR('',#32828,1.);
#9844=VECTOR('',#32837,1.);
#9845=VECTOR('',#32838,1.);
#9846=VECTOR('',#32841,1.);
#9847=VECTOR('',#32842,1.);
#9848=VECTOR('',#32843,1.);
#9849=VECTOR('',#32846,1.);
#9850=VECTOR('',#32847,1.);
#9851=VECTOR('',#32854,1.);
#9852=VECTOR('',#32855,1.);
#9853=VECTOR('',#32856,1.);
#9854=VECTOR('',#32857,1.);
#9855=VECTOR('',#32862,1.);
#9856=VECTOR('',#32865,1.);
#9857=VECTOR('',#32866,1.);
#9858=VECTOR('',#32873,1.);
#9859=VECTOR('',#32874,1.);
#9860=VECTOR('',#32875,1.);
#9861=VECTOR('',#32876,1.);
#9862=VECTOR('',#32881,1.);
#9863=VECTOR('',#32884,1.);
#9864=VECTOR('',#32885,1.);
#9865=VECTOR('',#32892,1.);
#9866=VECTOR('',#32893,1.);
#9867=VECTOR('',#32894,1.);
#9868=VECTOR('',#32895,1.);
#9869=VECTOR('',#32900,1.);
#9870=VECTOR('',#32903,1.);
#9871=VECTOR('',#32904,1.);
#9872=VECTOR('',#32911,1.);
#9873=VECTOR('',#32912,1.);
#9874=VECTOR('',#32913,1.);
#9875=VECTOR('',#32914,1.);
#9876=VECTOR('',#32919,1.);
#9877=VECTOR('',#32922,1.);
#9878=VECTOR('',#32923,1.);
#9879=VECTOR('',#32930,1.);
#9880=VECTOR('',#32931,1.);
#9881=VECTOR('',#32932,1.);
#9882=VECTOR('',#32933,1.);
#9883=VECTOR('',#32938,1.);
#9884=VECTOR('',#32941,1.);
#9885=VECTOR('',#32942,1.);
#9886=VECTOR('',#32949,1.);
#9887=VECTOR('',#32950,1.);
#9888=VECTOR('',#32951,1.);
#9889=VECTOR('',#32952,1.);
#9890=VECTOR('',#32957,1.);
#9891=VECTOR('',#32960,1.);
#9892=VECTOR('',#32961,1.);
#9893=VECTOR('',#32968,1.);
#9894=VECTOR('',#32969,1.);
#9895=VECTOR('',#32970,1.);
#9896=VECTOR('',#32971,1.);
#9897=VECTOR('',#32976,1.);
#9898=VECTOR('',#32979,1.);
#9899=VECTOR('',#32980,1.);
#9900=VECTOR('',#32987,1.);
#9901=VECTOR('',#32988,1.);
#9902=VECTOR('',#32989,1.);
#9903=VECTOR('',#32990,1.);
#9904=VECTOR('',#32995,1.);
#9905=VECTOR('',#32998,1.);
#9906=VECTOR('',#32999,1.);
#9907=VECTOR('',#33006,1.);
#9908=VECTOR('',#33007,1.);
#9909=VECTOR('',#33008,1.);
#9910=VECTOR('',#33009,1.);
#9911=VECTOR('',#33014,1.);
#9912=VECTOR('',#33017,1.);
#9913=VECTOR('',#33018,1.);
#9914=VECTOR('',#33029,0.375);
#9915=VECTOR('',#33034,0.635);
#9916=VECTOR('',#33069,0.65);
#9917=VECTOR('',#33114,0.625);
#9918=VECTOR('',#33121,1.);
#9919=VECTOR('',#33122,1.);
#9920=VECTOR('',#33123,1.);
#9921=VECTOR('',#33124,1.);
#9922=VECTOR('',#33127,1.);
#9923=VECTOR('',#33134,1.);
#9924=VECTOR('',#33135,1.);
#9925=VECTOR('',#33136,1.);
#9926=VECTOR('',#33145,1.);
#9927=VECTOR('',#33148,1.);
#9928=VECTOR('',#33151,1.);
#9929=VECTOR('',#33152,1.);
#9930=VECTOR('',#33157,1.);
#9931=VECTOR('',#33158,1.);
#9932=VECTOR('',#33159,1.);
#9933=VECTOR('',#33162,1.);
#9934=VECTOR('',#33169,1.);
#9935=VECTOR('',#33170,1.);
#9936=VECTOR('',#33171,1.);
#9937=VECTOR('',#33178,1.);
#9938=VECTOR('',#33187,0.600000000000001);
#9939=VECTOR('',#33192,0.600000000000001);
#9940=VECTOR('',#33195,0.600000000000001);
#9941=VECTOR('',#33198,0.600000000000001);
#9942=VECTOR('',#33201,0.600000000000001);
#9943=VECTOR('',#33204,0.600000000000001);
#9944=VECTOR('',#33207,0.600000000000001);
#9945=VECTOR('',#33210,0.600000000000001);
#9946=VECTOR('',#33213,0.600000000000001);
#9947=VECTOR('',#33216,0.600000000000001);
#9948=VECTOR('',#33219,0.491824999999999);
#9949=VECTOR('',#33224,0.491824999999999);
#9950=VECTOR('',#33227,0.491824999999999);
#9951=VECTOR('',#33230,0.491824999999999);
#9952=VECTOR('',#33233,0.491824999999999);
#9953=VECTOR('',#33236,0.491824999999999);
#9954=VECTOR('',#33239,0.491824999999999);
#9955=VECTOR('',#33242,0.491824999999999);
#9956=VECTOR('',#33245,0.491824999999999);
#9957=VECTOR('',#33270,0.699999999999994);
#9958=VECTOR('',#33291,1.);
#9959=VECTOR('',#33300,0.575000000000003);
#9960=VECTOR('',#33311,1.5);
#9961=VECTOR('',#33320,1.);
#9962=VECTOR('',#33325,0.975000000000001);
#9963=VECTOR('',#33332,0.4);
#9964=VECTOR('',#33337,0.4);
#9965=VECTOR('',#33340,0.4);
#9966=VECTOR('',#33343,0.4);
#9967=VECTOR('',#33346,0.4);
#9968=VECTOR('',#33349,0.4);
#9969=VECTOR('',#33352,0.4);
#9970=VECTOR('',#33355,0.4);
#9971=VECTOR('',#33358,0.4);
#9972=VECTOR('',#33361,0.4);
#9973=VECTOR('',#33364,0.4);
#9974=VECTOR('',#33367,0.4);
#9975=VECTOR('',#33370,0.4);
#9976=VECTOR('',#33373,0.4);
#9977=VECTOR('',#33376,0.322275);
#9978=VECTOR('',#33381,0.322275);
#9979=VECTOR('',#33384,0.322275);
#9980=VECTOR('',#33387,0.322275);
#9981=VECTOR('',#33390,0.322275);
#9982=VECTOR('',#33393,0.322275);
#9983=VECTOR('',#33396,0.322275);
#9984=VECTOR('',#33399,0.322275);
#9985=VECTOR('',#33402,0.322275);
#9986=VECTOR('',#33405,0.322275);
#9987=VECTOR('',#33408,0.322275);
#9988=VECTOR('',#33411,0.322275);
#9989=VECTOR('',#33414,0.322275);
#9990=VECTOR('',#33417,0.322275);
#9991=VECTOR('',#33436,1.);
#9992=VECTOR('',#33437,1.);
#9993=VECTOR('',#33438,1.);
#9994=VECTOR('',#33439,1.);
#9995=VECTOR('',#33442,1.);
#9996=VECTOR('',#33443,1.);
#9997=VECTOR('',#33444,1.);
#9998=VECTOR('',#33447,1.);
#9999=VECTOR('',#33448,1.);
#10000=VECTOR('',#33449,1.);
#10001=VECTOR('',#33452,1.);
#10002=VECTOR('',#33453,1.);
#10003=VECTOR('',#33454,1.);
#10004=VECTOR('',#33457,1.);
#10005=VECTOR('',#33458,1.);
#10006=VECTOR('',#33459,1.);
#10007=VECTOR('',#33462,1.);
#10008=VECTOR('',#33463,1.);
#10009=VECTOR('',#33472,0.37);
#10010=VECTOR('',#33479,0.275);
#10011=VECTOR('',#33484,0.26);
#10012=VECTOR('',#33491,1.);
#10013=VECTOR('',#33492,1.);
#10014=VECTOR('',#33493,1.);
#10015=VECTOR('',#33494,1.);
#10016=VECTOR('',#33495,1.);
#10017=VECTOR('',#33496,1.);
#10018=VECTOR('',#33499,1.);
#10019=VECTOR('',#33500,1.);
#10020=VECTOR('',#33501,1.);
#10021=VECTOR('',#33504,1.);
#10022=VECTOR('',#33505,1.);
#10023=VECTOR('',#33506,1.);
#10024=VECTOR('',#33507,1.);
#10025=VECTOR('',#33510,1.);
#10026=VECTOR('',#33511,1.);
#10027=VECTOR('',#33512,1.);
#10028=VECTOR('',#33513,1.);
#10029=VECTOR('',#33516,1.);
#10030=VECTOR('',#33517,1.);
#10031=VECTOR('',#33518,1.);
#10032=VECTOR('',#33519,1.);
#10033=VECTOR('',#33522,1.);
#10034=VECTOR('',#33523,1.);
#10035=VECTOR('',#33524,1.);
#10036=VECTOR('',#33525,1.);
#10037=VECTOR('',#33526,1.);
#10038=VECTOR('',#33529,1.);
#10039=VECTOR('',#33530,1.);
#10040=VECTOR('',#33533,1.);
#10041=VECTOR('',#33534,1.);
#10042=VECTOR('',#33535,1.);
#10043=VECTOR('',#33538,1.);
#10044=VECTOR('',#33539,1.);
#10045=VECTOR('',#33540,1.);
#10046=VECTOR('',#33541,1.);
#10047=VECTOR('',#33542,1.);
#10048=VECTOR('',#33545,1.);
#10049=VECTOR('',#33546,1.);
#10050=VECTOR('',#33547,1.);
#10051=VECTOR('',#33550,1.);
#10052=VECTOR('',#33551,1.);
#10053=VECTOR('',#33552,1.);
#10054=VECTOR('',#33555,1.);
#10055=VECTOR('',#33556,1.);
#10056=VECTOR('',#33557,1.);
#10057=VECTOR('',#33560,1.);
#10058=VECTOR('',#33563,1.);
#10059=VECTOR('',#33568,1.);
#10060=VECTOR('',#33577,0.8);
#10061=VECTOR('',#33582,0.8);
#10062=VECTOR('',#33585,0.8);
#10063=VECTOR('',#33588,0.8);
#10064=VECTOR('',#33591,0.8);
#10065=VECTOR('',#33594,0.8);
#10066=VECTOR('',#33597,0.8);
#10067=VECTOR('',#33600,0.8);
#10068=VECTOR('',#33603,0.8);
#10069=VECTOR('',#33606,0.8);
#10070=VECTOR('',#33609,0.8);
#10071=VECTOR('',#33612,0.8);
#10072=VECTOR('',#33615,0.8);
#10073=VECTOR('',#33618,0.8);
#10074=VECTOR('',#33621,0.8);
#10075=VECTOR('',#33624,0.8);
#10076=VECTOR('',#33627,0.8);
#10077=VECTOR('',#33630,0.8);
#10078=VECTOR('',#33633,0.8);
#10079=VECTOR('',#33636,0.8);
#10080=VECTOR('',#33639,0.6767);
#10081=VECTOR('',#33644,0.6767);
#10082=VECTOR('',#33649,0.6767);
#10083=VECTOR('',#33652,0.6767);
#10084=VECTOR('',#33655,0.6767);
#10085=VECTOR('',#33658,0.6767);
#10086=VECTOR('',#33661,0.6767);
#10087=VECTOR('',#33664,0.6767);
#10088=VECTOR('',#33667,0.6767);
#10089=VECTOR('',#33670,0.6767);
#10090=VECTOR('',#33673,0.6767);
#10091=VECTOR('',#33676,0.6767);
#10092=VECTOR('',#33679,0.6767);
#10093=VECTOR('',#33682,0.6767);
#10094=VECTOR('',#33685,0.6767);
#10095=VECTOR('',#33688,0.6767);
#10096=VECTOR('',#33691,0.6767);
#10097=VECTOR('',#33694,0.6767);
#10098=VECTOR('',#33697,0.6767);
#10099=VECTOR('',#33700,0.6767);
#10100=VECTOR('',#33713,1.28782032302755);
#10101=VECTOR('',#33718,1.);
#10102=VECTOR('',#33719,1.);
#10103=VECTOR('',#33720,1.);
#10104=VECTOR('',#33723,1.);
#10105=VECTOR('',#33724,1.);
#10106=VECTOR('',#33727,1.);
#10107=VECTOR('',#33728,1.);
#10108=VECTOR('',#33731,1.);
#10109=VECTOR('',#33732,1.);
#10110=VECTOR('',#33733,1.);
#10111=VECTOR('',#33738,1.);
#10112=VECTOR('',#33741,1.);
#10113=VECTOR('',#33752,0.77);
#10114=VECTOR('',#33763,1.125);
#10115=VECTOR('',#33770,0.912322330470337);
#10116=VECTOR('',#33775,0.855);
#10117=VECTOR('',#33780,1.);
#10118=VECTOR('',#33783,1.);
#10119=VECTOR('',#33786,1.);
#10120=VECTOR('',#33789,1.);
#10121=VECTOR('',#33794,0.822677669529664);
#10122=VECTOR('',#33801,0.805);
#10123=VECTOR('',#33806,0.822677669529664);
#10124=VECTOR('',#33811,0.855000000000001);
#10125=VECTOR('',#33814,0.912322330470337);
#10126=VECTOR('',#33819,1.);
#10127=VECTOR('',#33822,1.);
#10128=VECTOR('',#33825,1.);
#10129=VECTOR('',#33828,1.);
#10130=VECTOR('',#33833,1.);
#10131=VECTOR('',#33836,1.);
#10132=VECTOR('',#33841,1.);
#10133=VECTOR('',#33842,1.);
#10134=VECTOR('',#33843,1.);
#10135=VECTOR('',#33846,1.);
#10136=VECTOR('',#33853,1.);
#10137=VECTOR('',#33854,1.);
#10138=VECTOR('',#33855,1.);
#10139=VECTOR('',#33858,1.);
#10140=VECTOR('',#33865,1.);
#10141=VECTOR('',#33866,1.);
#10142=VECTOR('',#33867,1.);
#10143=VECTOR('',#33870,1.);
#10144=VECTOR('',#33877,1.);
#10145=VECTOR('',#33878,1.);
#10146=VECTOR('',#33881,1.);
#10147=VECTOR('',#33882,1.);
#10148=VECTOR('',#33883,1.);
#10149=VECTOR('',#33886,1.);
#10150=VECTOR('',#33891,1.);
#10151=VECTOR('',#33892,1.);
#10152=VECTOR('',#33895,1.);
#10153=VECTOR('',#33900,1.);
#10154=VECTOR('',#33901,1.);
#10155=VECTOR('',#33904,1.);
#10156=VECTOR('',#33907,1.);
#10157=VECTOR('',#33910,1.);
#10158=VECTOR('',#33913,1.);
#10159=VECTOR('',#33914,1.);
#10160=VECTOR('',#33915,1.);
#10161=VECTOR('',#33918,1.);
#10162=VECTOR('',#33923,1.);
#10163=VECTOR('',#33924,1.);
#10164=VECTOR('',#33927,1.);
#10165=VECTOR('',#33932,1.);
#10166=VECTOR('',#33933,1.);
#10167=VECTOR('',#33936,1.);
#10168=VECTOR('',#33941,1.);
#10169=VECTOR('',#33942,1.);
#10170=VECTOR('',#33949,1.);
#10171=VECTOR('',#33952,1.);
#10172=VECTOR('',#33955,1.);
#10173=VECTOR('',#33956,1.);
#10174=VECTOR('',#33959,1.);
#10175=VECTOR('',#33964,1.);
#10176=VECTOR('',#33965,1.);
#10177=VECTOR('',#33968,1.);
#10178=VECTOR('',#33969,1.);
#10179=VECTOR('',#33972,1.);
#10180=VECTOR('',#33975,1.);
#10181=VECTOR('',#33978,1.);
#10182=VECTOR('',#33981,1.);
#10183=VECTOR('',#33982,1.);
#10184=VECTOR('',#33983,1.);
#10185=VECTOR('',#33986,1.);
#10186=VECTOR('',#33993,1.);
#10187=VECTOR('',#33994,1.);
#10188=VECTOR('',#33995,1.);
#10189=VECTOR('',#34004,1.);
#10190=VECTOR('',#34005,1.);
#10191=VECTOR('',#34008,1.);
#10192=VECTOR('',#34015,1.);
#10193=VECTOR('',#34016,1.);
#10194=VECTOR('',#34021,1.);
#10195=VECTOR('',#34026,1.);
#10196=VECTOR('',#34027,1.);
#10197=VECTOR('',#34030,1.);
#10198=VECTOR('',#34041,1.53);
#10199=VECTOR('',#34048,1.53);
#10200=VECTOR('',#34051,1.56);
#10201=VECTOR('',#34058,1.05);
#10202=VECTOR('',#34069,1.725);
#10203=VECTOR('',#34074,1.75);
#10204=VECTOR('',#34081,1.56);
#10205=VECTOR('',#34090,1.72);
#10206=VECTOR('',#34095,1.695);
#10207=VECTOR('',#34102,1.);
#10208=VECTOR('',#34111,1.24);
#10209=VECTOR('',#34120,0.6);
#10210=VECTOR('',#34125,0.6);
#10211=VECTOR('',#34128,0.6);
#10212=VECTOR('',#34131,0.6);
#10213=VECTOR('',#34134,0.6);
#10214=VECTOR('',#34137,0.6);
#10215=VECTOR('',#34140,0.6);
#10216=VECTOR('',#34143,0.6);
#10217=VECTOR('',#34146,0.6);
#10218=VECTOR('',#34149,0.6);
#10219=VECTOR('',#34152,0.6);
#10220=VECTOR('',#34155,0.6);
#10221=VECTOR('',#34158,0.6);
#10222=VECTOR('',#34161,0.6);
#10223=VECTOR('',#34164,0.6);
#10224=VECTOR('',#34167,0.6);
#10225=VECTOR('',#34170,0.6);
#10226=VECTOR('',#34173,0.6);
#10227=VECTOR('',#34176,0.6);
#10228=VECTOR('',#34179,0.6);
#10229=VECTOR('',#34182,0.6);
#10230=VECTOR('',#34185,0.6);
#10231=VECTOR('',#34188,0.6);
#10232=VECTOR('',#34191,0.491825);
#10233=VECTOR('',#34196,0.491825);
#10234=VECTOR('',#34199,0.491825);
#10235=VECTOR('',#34202,0.491825);
#10236=VECTOR('',#34205,0.491825);
#10237=VECTOR('',#34208,0.491825);
#10238=VECTOR('',#34211,0.491825);
#10239=VECTOR('',#34214,0.491825);
#10240=VECTOR('',#34217,0.491825);
#10241=VECTOR('',#34220,0.491825);
#10242=VECTOR('',#34223,0.491825);
#10243=VECTOR('',#34226,0.491825);
#10244=VECTOR('',#34229,0.491825);
#10245=VECTOR('',#34232,0.491825);
#10246=VECTOR('',#34235,0.491825);
#10247=VECTOR('',#34238,0.491825);
#10248=VECTOR('',#34241,0.491825);
#10249=VECTOR('',#34244,0.491825);
#10250=VECTOR('',#34247,0.491825);
#10251=VECTOR('',#34250,0.491825);
#10252=VECTOR('',#34253,0.491825);
#10253=VECTOR('',#34256,0.491825);
#10254=VECTOR('',#34269,0.972115242270663);
#10255=VECTOR('',#34274,1.);
#10256=VECTOR('',#34275,1.);
#10257=VECTOR('',#34276,1.);
#10258=VECTOR('',#34279,1.);
#10259=VECTOR('',#34280,1.);
#10260=VECTOR('',#34283,1.);
#10261=VECTOR('',#34284,1.);
#10262=VECTOR('',#34287,1.);
#10263=VECTOR('',#34288,1.);
#10264=VECTOR('',#34289,1.);
#10265=VECTOR('',#34294,1.);
#10266=VECTOR('',#34297,1.);
#10267=VECTOR('',#34308,0.57);
#10268=VECTOR('',#34319,0.83);
#10269=VECTOR('',#34324,0.5);
#10270=VECTOR('',#34329,0.5);
#10271=VECTOR('',#34332,0.5);
#10272=VECTOR('',#34335,0.5);
#10273=VECTOR('',#34338,0.5);
#10274=VECTOR('',#34341,0.5);
#10275=VECTOR('',#34344,0.5);
#10276=VECTOR('',#34347,0.5);
#10277=VECTOR('',#34350,0.5);
#10278=VECTOR('',#34353,0.5);
#10279=VECTOR('',#34356,0.5);
#10280=VECTOR('',#34359,0.5);
#10281=VECTOR('',#34362,0.5);
#10282=VECTOR('',#34365,0.5);
#10283=VECTOR('',#34368,0.5);
#10284=VECTOR('',#34371,0.5);
#10285=VECTOR('',#34374,0.5);
#10286=VECTOR('',#34377,0.5);
#10287=VECTOR('',#34380,0.5);
#10288=VECTOR('',#34383,0.5);
#10289=VECTOR('',#34386,0.5);
#10290=VECTOR('',#34389,0.5);
#10291=VECTOR('',#34392,0.5);
#10292=VECTOR('',#34395,0.40705);
#10293=VECTOR('',#34400,0.40705);
#10294=VECTOR('',#34403,0.40705);
#10295=VECTOR('',#34406,0.40705);
#10296=VECTOR('',#34409,0.40705);
#10297=VECTOR('',#34412,0.40705);
#10298=VECTOR('',#34415,0.40705);
#10299=VECTOR('',#34418,0.40705);
#10300=VECTOR('',#34421,0.40705);
#10301=VECTOR('',#34424,0.40705);
#10302=VECTOR('',#34427,0.40705);
#10303=VECTOR('',#34430,0.40705);
#10304=VECTOR('',#34433,0.40705);
#10305=VECTOR('',#34436,0.40705);
#10306=VECTOR('',#34439,0.40705);
#10307=VECTOR('',#34442,0.40705);
#10308=VECTOR('',#34445,0.40705);
#10309=VECTOR('',#34448,0.40705);
#10310=VECTOR('',#34451,0.40705);
#10311=VECTOR('',#34454,0.40705);
#10312=VECTOR('',#34457,0.40705);
#10313=VECTOR('',#34460,0.40705);
#10314=VECTOR('',#34463,0.40705);
#10315=VECTOR('',#34496,1.);
#10316=VECTOR('',#34501,1.);
#10317=VECTOR('',#34506,1.);
#10318=VECTOR('',#34511,1.);
#10319=VECTOR('',#34516,1.);
#10320=VECTOR('',#34521,1.);
#10321=VECTOR('',#34526,0.23094010767585);
#10322=VECTOR('',#34529,1.);
#10323=VECTOR('',#34530,1.);
#10324=VECTOR('',#34531,1.);
#10325=VECTOR('',#34534,1.);
#10326=VECTOR('',#34535,1.);
#10327=VECTOR('',#34538,1.);
#10328=VECTOR('',#34539,1.);
#10329=VECTOR('',#34542,1.);
#10330=VECTOR('',#34543,1.);
#10331=VECTOR('',#34546,1.);
#10332=VECTOR('',#34547,1.);
#10333=VECTOR('',#34550,1.);
#10334=VECTOR('',#34553,1.);
#10335=VECTOR('',#34554,1.);
#10336=VECTOR('',#34555,1.);
#10337=VECTOR('',#34556,1.);
#10338=VECTOR('',#34561,1.);
#10339=VECTOR('',#34564,1.);
#10340=VECTOR('',#34565,1.);
#10341=VECTOR('',#34572,1.);
#10342=VECTOR('',#34573,1.);
#10343=VECTOR('',#34574,1.);
#10344=VECTOR('',#34575,1.);
#10345=VECTOR('',#34580,1.);
#10346=VECTOR('',#34583,1.);
#10347=VECTOR('',#34584,1.);
#10348=VECTOR('',#34591,1.);
#10349=VECTOR('',#34592,1.);
#10350=VECTOR('',#34593,1.);
#10351=VECTOR('',#34594,1.);
#10352=VECTOR('',#34599,1.);
#10353=VECTOR('',#34602,1.);
#10354=VECTOR('',#34603,1.);
#10355=VECTOR('',#34610,1.);
#10356=VECTOR('',#34611,1.);
#10357=VECTOR('',#34612,1.);
#10358=VECTOR('',#34613,1.);
#10359=VECTOR('',#34618,1.);
#10360=VECTOR('',#34621,1.);
#10361=VECTOR('',#34622,1.);
#10362=VECTOR('',#34629,1.);
#10363=VECTOR('',#34630,1.);
#10364=VECTOR('',#34631,1.);
#10365=VECTOR('',#34632,1.);
#10366=VECTOR('',#34637,1.);
#10367=VECTOR('',#34640,1.);
#10368=VECTOR('',#34641,1.);
#10369=VECTOR('',#34648,1.);
#10370=VECTOR('',#34649,1.);
#10371=VECTOR('',#34650,1.);
#10372=VECTOR('',#34651,1.);
#10373=VECTOR('',#34656,1.);
#10374=VECTOR('',#34659,1.);
#10375=VECTOR('',#34660,1.);
#10376=VECTOR('',#34667,1.);
#10377=VECTOR('',#34668,1.);
#10378=VECTOR('',#34669,1.);
#10379=VECTOR('',#34670,1.);
#10380=VECTOR('',#34675,1.);
#10381=VECTOR('',#34678,1.);
#10382=VECTOR('',#34679,1.);
#10383=VECTOR('',#34686,1.);
#10384=VECTOR('',#34687,1.);
#10385=VECTOR('',#34688,1.);
#10386=VECTOR('',#34689,1.);
#10387=VECTOR('',#34694,1.);
#10388=VECTOR('',#34697,1.);
#10389=VECTOR('',#34698,1.);
#10390=VECTOR('',#34705,1.);
#10391=VECTOR('',#34706,1.);
#10392=VECTOR('',#34707,1.);
#10393=VECTOR('',#34708,1.);
#10394=VECTOR('',#34713,1.);
#10395=VECTOR('',#34718,1.);
#10396=VECTOR('',#34719,1.);
#10397=VECTOR('',#34728,1.);
#10398=VECTOR('',#34729,1.);
#10399=VECTOR('',#34730,1.);
#10400=VECTOR('',#34731,1.);
#10401=VECTOR('',#34736,1.);
#10402=VECTOR('',#34739,1.);
#10403=VECTOR('',#34740,1.);
#10404=VECTOR('',#34747,1.);
#10405=VECTOR('',#34748,1.);
#10406=VECTOR('',#34749,1.);
#10407=VECTOR('',#34750,1.);
#10408=VECTOR('',#34755,1.);
#10409=VECTOR('',#34758,1.);
#10410=VECTOR('',#34759,1.);
#10411=VECTOR('',#34766,1.);
#10412=VECTOR('',#34767,1.);
#10413=VECTOR('',#34768,1.);
#10414=VECTOR('',#34769,1.);
#10415=VECTOR('',#34774,1.);
#10416=VECTOR('',#34777,1.);
#10417=VECTOR('',#34778,1.);
#10418=VECTOR('',#34785,1.);
#10419=VECTOR('',#34786,1.);
#10420=VECTOR('',#34787,1.);
#10421=VECTOR('',#34788,1.);
#10422=VECTOR('',#34793,1.);
#10423=VECTOR('',#34796,1.);
#10424=VECTOR('',#34797,1.);
#10425=VECTOR('',#34804,1.);
#10426=VECTOR('',#34805,1.);
#10427=VECTOR('',#34806,1.);
#10428=VECTOR('',#34807,1.);
#10429=VECTOR('',#34812,1.);
#10430=VECTOR('',#34815,1.);
#10431=VECTOR('',#34816,1.);
#10432=VECTOR('',#34823,1.);
#10433=VECTOR('',#34824,1.);
#10434=VECTOR('',#34825,1.);
#10435=VECTOR('',#34826,1.);
#10436=VECTOR('',#34831,1.);
#10437=VECTOR('',#34834,1.);
#10438=VECTOR('',#34835,1.);
#10439=VECTOR('',#34842,1.);
#10440=VECTOR('',#34843,1.);
#10441=VECTOR('',#34844,1.);
#10442=VECTOR('',#34845,1.);
#10443=VECTOR('',#34850,1.);
#10444=VECTOR('',#34853,1.);
#10445=VECTOR('',#34854,1.);
#10446=VECTOR('',#34861,1.);
#10447=VECTOR('',#34862,1.);
#10448=VECTOR('',#34863,1.);
#10449=VECTOR('',#34864,1.);
#10450=VECTOR('',#34869,1.);
#10451=VECTOR('',#34872,1.);
#10452=VECTOR('',#34873,1.);
#10453=VECTOR('',#34880,1.);
#10454=VECTOR('',#34881,1.);
#10455=VECTOR('',#34882,1.);
#10456=VECTOR('',#34883,1.);
#10457=VECTOR('',#34888,1.);
#10458=VECTOR('',#34891,1.);
#10459=VECTOR('',#34892,1.);
#10460=VECTOR('',#34899,1.);
#10461=VECTOR('',#34900,1.);
#10462=VECTOR('',#34901,1.);
#10463=VECTOR('',#34902,1.);
#10464=VECTOR('',#34907,1.);
#10465=VECTOR('',#34910,1.);
#10466=VECTOR('',#34911,1.);
#10467=VECTOR('',#34918,1.);
#10468=VECTOR('',#34919,1.);
#10469=VECTOR('',#34920,1.);
#10470=VECTOR('',#34921,1.);
#10471=VECTOR('',#34926,1.);
#10472=VECTOR('',#34929,1.);
#10473=VECTOR('',#34930,1.);
#10474=VECTOR('',#34937,1.);
#10475=VECTOR('',#34938,1.);
#10476=VECTOR('',#34939,1.);
#10477=VECTOR('',#34940,1.);
#10478=VECTOR('',#34945,1.);
#10479=VECTOR('',#34948,1.);
#10480=VECTOR('',#34949,1.);
#10481=VECTOR('',#34956,1.);
#10482=VECTOR('',#34957,1.);
#10483=VECTOR('',#34958,1.);
#10484=VECTOR('',#34959,1.);
#10485=VECTOR('',#34964,1.);
#10486=VECTOR('',#34967,1.);
#10487=VECTOR('',#34968,1.);
#10488=VECTOR('',#34975,1.);
#10489=VECTOR('',#34976,1.);
#10490=VECTOR('',#34977,1.);
#10491=VECTOR('',#34978,1.);
#10492=VECTOR('',#34983,1.);
#10493=VECTOR('',#34986,1.);
#10494=VECTOR('',#34987,1.);
#10495=VECTOR('',#34994,1.);
#10496=VECTOR('',#34995,1.);
#10497=VECTOR('',#34996,1.);
#10498=VECTOR('',#34997,1.);
#10499=VECTOR('',#35002,1.);
#10500=VECTOR('',#35005,1.);
#10501=VECTOR('',#35006,1.);
#10502=VECTOR('',#35013,1.);
#10503=VECTOR('',#35014,1.);
#10504=VECTOR('',#35015,1.);
#10505=VECTOR('',#35016,1.);
#10506=VECTOR('',#35021,1.);
#10507=VECTOR('',#35024,1.);
#10508=VECTOR('',#35025,1.);
#10509=VECTOR('',#35032,1.);
#10510=VECTOR('',#35033,1.);
#10511=VECTOR('',#35034,1.);
#10512=VECTOR('',#35035,1.);
#10513=VECTOR('',#35040,1.);
#10514=VECTOR('',#35043,1.);
#10515=VECTOR('',#35044,1.);
#10516=VECTOR('',#35053,1.);
#10517=VECTOR('',#35054,1.);
#10518=VECTOR('',#35057,1.);
#10519=VECTOR('',#35058,1.);
#10520=VECTOR('',#35059,1.);
#10521=VECTOR('',#35062,1.);
#10522=VECTOR('',#35063,1.);
#10523=VECTOR('',#35070,1.);
#10524=VECTOR('',#35071,1.);
#10525=VECTOR('',#35072,1.);
#10526=VECTOR('',#35073,1.);
#10527=VECTOR('',#35078,1.);
#10528=VECTOR('',#35081,1.);
#10529=VECTOR('',#35082,1.);
#10530=VECTOR('',#35089,1.);
#10531=VECTOR('',#35090,1.);
#10532=VECTOR('',#35091,1.);
#10533=VECTOR('',#35092,1.);
#10534=VECTOR('',#35097,1.);
#10535=VECTOR('',#35100,1.);
#10536=VECTOR('',#35101,1.);
#10537=VECTOR('',#35108,1.);
#10538=VECTOR('',#35109,1.);
#10539=VECTOR('',#35110,1.);
#10540=VECTOR('',#35111,1.);
#10541=VECTOR('',#35116,1.);
#10542=VECTOR('',#35119,1.);
#10543=VECTOR('',#35120,1.);
#10544=VECTOR('',#35127,1.);
#10545=VECTOR('',#35128,1.);
#10546=VECTOR('',#35129,1.);
#10547=VECTOR('',#35130,1.);
#10548=VECTOR('',#35135,1.);
#10549=VECTOR('',#35138,1.);
#10550=VECTOR('',#35139,1.);
#10551=VECTOR('',#35146,1.);
#10552=VECTOR('',#35147,1.);
#10553=VECTOR('',#35148,1.);
#10554=VECTOR('',#35149,1.);
#10555=VECTOR('',#35154,1.);
#10556=VECTOR('',#35157,1.);
#10557=VECTOR('',#35158,1.);
#10558=VECTOR('',#35165,1.);
#10559=VECTOR('',#35166,1.);
#10560=VECTOR('',#35167,1.);
#10561=VECTOR('',#35168,1.);
#10562=VECTOR('',#35173,1.);
#10563=VECTOR('',#35176,1.);
#10564=VECTOR('',#35177,1.);
#10565=VECTOR('',#35184,1.);
#10566=VECTOR('',#35185,1.);
#10567=VECTOR('',#35186,1.);
#10568=VECTOR('',#35187,1.);
#10569=VECTOR('',#35192,1.);
#10570=VECTOR('',#35195,1.);
#10571=VECTOR('',#35196,1.);
#10572=VECTOR('',#35203,1.);
#10573=VECTOR('',#35204,1.);
#10574=VECTOR('',#35205,1.);
#10575=VECTOR('',#35206,1.);
#10576=VECTOR('',#35211,1.);
#10577=VECTOR('',#35214,1.);
#10578=VECTOR('',#35215,1.);
#10579=VECTOR('',#35222,1.);
#10580=VECTOR('',#35223,1.);
#10581=VECTOR('',#35224,1.);
#10582=VECTOR('',#35225,1.);
#10583=VECTOR('',#35230,1.);
#10584=VECTOR('',#35233,1.);
#10585=VECTOR('',#35234,1.);
#10586=VECTOR('',#35245,0.475);
#10587=VECTOR('',#35250,0.785);
#10588=VECTOR('',#35285,0.8);
#10589=VECTOR('',#35330,0.775);
#10590=VECTOR('',#35337,0.3);
#10591=VECTOR('',#35342,0.3);
#10592=VECTOR('',#35345,0.3);
#10593=VECTOR('',#35348,0.3);
#10594=VECTOR('',#35351,0.3);
#10595=VECTOR('',#35354,0.3);
#10596=VECTOR('',#35357,0.3);
#10597=VECTOR('',#35360,0.3);
#10598=VECTOR('',#35363,0.3);
#10599=VECTOR('',#35366,0.3);
#10600=VECTOR('',#35369,0.3);
#10601=VECTOR('',#35372,0.3);
#10602=VECTOR('',#35375,0.3);
#10603=VECTOR('',#35378,0.3);
#10604=VECTOR('',#35381,0.3);
#10605=VECTOR('',#35384,0.3);
#10606=VECTOR('',#35387,0.3);
#10607=VECTOR('',#35390,0.3);
#10608=VECTOR('',#35393,0.3);
#10609=VECTOR('',#35396,0.3);
#10610=VECTOR('',#35401,0.237175);
#10611=VECTOR('',#35406,0.237175);
#10612=VECTOR('',#35409,0.237175);
#10613=VECTOR('',#35412,0.237175);
#10614=VECTOR('',#35415,0.237175);
#10615=VECTOR('',#35418,0.237175);
#10616=VECTOR('',#35421,0.237175);
#10617=VECTOR('',#35424,0.237175);
#10618=VECTOR('',#35427,0.237175);
#10619=VECTOR('',#35430,0.237175);
#10620=VECTOR('',#35433,0.237175);
#10621=VECTOR('',#35436,0.237175);
#10622=VECTOR('',#35439,0.237175);
#10623=VECTOR('',#35442,0.237175);
#10624=VECTOR('',#35445,0.237175);
#10625=VECTOR('',#35448,0.237175);
#10626=VECTOR('',#35451,0.237175);
#10627=VECTOR('',#35454,0.237175);
#10628=VECTOR('',#35457,0.237175);
#10629=VECTOR('',#35488,1.);
#10630=VECTOR('',#35493,1.);
#10631=VECTOR('',#35498,1.);
#10632=VECTOR('',#35503,1.);
#10633=VECTOR('',#35508,1.);
#10634=VECTOR('',#35513,1.);
#10635=VECTOR('',#35518,0.144337567297406);
#10636=VECTOR('',#35521,1.);
#10637=VECTOR('',#35522,1.);
#10638=VECTOR('',#35523,1.);
#10639=VECTOR('',#35526,1.);
#10640=VECTOR('',#35527,1.);
#10641=VECTOR('',#35530,1.);
#10642=VECTOR('',#35531,1.);
#10643=VECTOR('',#35534,1.);
#10644=VECTOR('',#35535,1.);
#10645=VECTOR('',#35538,1.);
#10646=VECTOR('',#35539,1.);
#10647=VECTOR('',#35542,1.);
#10648=VECTOR('',#35545,1.);
#10649=VECTOR('',#35546,1.);
#10650=VECTOR('',#35547,1.);
#10651=VECTOR('',#35548,1.);
#10652=VECTOR('',#35553,1.);
#10653=VECTOR('',#35556,1.);
#10654=VECTOR('',#35557,1.);
#10655=VECTOR('',#35564,1.);
#10656=VECTOR('',#35565,1.);
#10657=VECTOR('',#35566,1.);
#10658=VECTOR('',#35567,1.);
#10659=VECTOR('',#35572,1.);
#10660=VECTOR('',#35575,1.);
#10661=VECTOR('',#35576,1.);
#10662=VECTOR('',#35583,1.);
#10663=VECTOR('',#35584,1.);
#10664=VECTOR('',#35585,1.);
#10665=VECTOR('',#35586,1.);
#10666=VECTOR('',#35591,1.);
#10667=VECTOR('',#35594,1.);
#10668=VECTOR('',#35595,1.);
#10669=VECTOR('',#35602,1.);
#10670=VECTOR('',#35603,1.);
#10671=VECTOR('',#35604,1.);
#10672=VECTOR('',#35605,1.);
#10673=VECTOR('',#35610,1.);
#10674=VECTOR('',#35613,1.);
#10675=VECTOR('',#35614,1.);
#10676=VECTOR('',#35621,1.);
#10677=VECTOR('',#35622,1.);
#10678=VECTOR('',#35623,1.);
#10679=VECTOR('',#35624,1.);
#10680=VECTOR('',#35629,1.);
#10681=VECTOR('',#35632,1.);
#10682=VECTOR('',#35633,1.);
#10683=VECTOR('',#35640,1.);
#10684=VECTOR('',#35641,1.);
#10685=VECTOR('',#35642,1.);
#10686=VECTOR('',#35643,1.);
#10687=VECTOR('',#35648,1.);
#10688=VECTOR('',#35651,1.);
#10689=VECTOR('',#35652,1.);
#10690=VECTOR('',#35659,1.);
#10691=VECTOR('',#35660,1.);
#10692=VECTOR('',#35661,1.);
#10693=VECTOR('',#35662,1.);
#10694=VECTOR('',#35667,1.);
#10695=VECTOR('',#35670,1.);
#10696=VECTOR('',#35671,1.);
#10697=VECTOR('',#35678,1.);
#10698=VECTOR('',#35679,1.);
#10699=VECTOR('',#35680,1.);
#10700=VECTOR('',#35681,1.);
#10701=VECTOR('',#35686,1.);
#10702=VECTOR('',#35689,1.);
#10703=VECTOR('',#35690,1.);
#10704=VECTOR('',#35697,1.);
#10705=VECTOR('',#35698,1.);
#10706=VECTOR('',#35699,1.);
#10707=VECTOR('',#35700,1.);
#10708=VECTOR('',#35705,1.);
#10709=VECTOR('',#35710,1.);
#10710=VECTOR('',#35711,1.);
#10711=VECTOR('',#35720,1.);
#10712=VECTOR('',#35721,1.);
#10713=VECTOR('',#35722,1.);
#10714=VECTOR('',#35723,1.);
#10715=VECTOR('',#35728,1.);
#10716=VECTOR('',#35731,1.);
#10717=VECTOR('',#35732,1.);
#10718=VECTOR('',#35739,1.);
#10719=VECTOR('',#35740,1.);
#10720=VECTOR('',#35741,1.);
#10721=VECTOR('',#35742,1.);
#10722=VECTOR('',#35747,1.);
#10723=VECTOR('',#35750,1.);
#10724=VECTOR('',#35751,1.);
#10725=VECTOR('',#35758,1.);
#10726=VECTOR('',#35759,1.);
#10727=VECTOR('',#35760,1.);
#10728=VECTOR('',#35761,1.);
#10729=VECTOR('',#35766,1.);
#10730=VECTOR('',#35769,1.);
#10731=VECTOR('',#35770,1.);
#10732=VECTOR('',#35777,1.);
#10733=VECTOR('',#35778,1.);
#10734=VECTOR('',#35779,1.);
#10735=VECTOR('',#35780,1.);
#10736=VECTOR('',#35785,1.);
#10737=VECTOR('',#35788,1.);
#10738=VECTOR('',#35789,1.);
#10739=VECTOR('',#35796,1.);
#10740=VECTOR('',#35797,1.);
#10741=VECTOR('',#35798,1.);
#10742=VECTOR('',#35799,1.);
#10743=VECTOR('',#35804,1.);
#10744=VECTOR('',#35807,1.);
#10745=VECTOR('',#35808,1.);
#10746=VECTOR('',#35815,1.);
#10747=VECTOR('',#35816,1.);
#10748=VECTOR('',#35817,1.);
#10749=VECTOR('',#35818,1.);
#10750=VECTOR('',#35823,1.);
#10751=VECTOR('',#35826,1.);
#10752=VECTOR('',#35827,1.);
#10753=VECTOR('',#35834,1.);
#10754=VECTOR('',#35835,1.);
#10755=VECTOR('',#35836,1.);
#10756=VECTOR('',#35837,1.);
#10757=VECTOR('',#35842,1.);
#10758=VECTOR('',#35845,1.);
#10759=VECTOR('',#35846,1.);
#10760=VECTOR('',#35853,1.);
#10761=VECTOR('',#35854,1.);
#10762=VECTOR('',#35855,1.);
#10763=VECTOR('',#35856,1.);
#10764=VECTOR('',#35861,1.);
#10765=VECTOR('',#35864,1.);
#10766=VECTOR('',#35865,1.);
#10767=VECTOR('',#35872,1.);
#10768=VECTOR('',#35873,1.);
#10769=VECTOR('',#35874,1.);
#10770=VECTOR('',#35875,1.);
#10771=VECTOR('',#35880,1.);
#10772=VECTOR('',#35883,1.);
#10773=VECTOR('',#35884,1.);
#10774=VECTOR('',#35891,1.);
#10775=VECTOR('',#35892,1.);
#10776=VECTOR('',#35893,1.);
#10777=VECTOR('',#35894,1.);
#10778=VECTOR('',#35899,1.);
#10779=VECTOR('',#35902,1.);
#10780=VECTOR('',#35903,1.);
#10781=VECTOR('',#35910,1.);
#10782=VECTOR('',#35911,1.);
#10783=VECTOR('',#35912,1.);
#10784=VECTOR('',#35913,1.);
#10785=VECTOR('',#35918,1.);
#10786=VECTOR('',#35921,1.);
#10787=VECTOR('',#35922,1.);
#10788=VECTOR('',#35929,1.);
#10789=VECTOR('',#35930,1.);
#10790=VECTOR('',#35931,1.);
#10791=VECTOR('',#35932,1.);
#10792=VECTOR('',#35937,1.);
#10793=VECTOR('',#35940,1.);
#10794=VECTOR('',#35941,1.);
#10795=VECTOR('',#35948,1.);
#10796=VECTOR('',#35949,1.);
#10797=VECTOR('',#35950,1.);
#10798=VECTOR('',#35951,1.);
#10799=VECTOR('',#35956,1.);
#10800=VECTOR('',#35959,1.);
#10801=VECTOR('',#35960,1.);
#10802=VECTOR('',#35967,1.);
#10803=VECTOR('',#35968,1.);
#10804=VECTOR('',#35969,1.);
#10805=VECTOR('',#35970,1.);
#10806=VECTOR('',#35975,1.);
#10807=VECTOR('',#35978,1.);
#10808=VECTOR('',#35979,1.);
#10809=VECTOR('',#35986,1.);
#10810=VECTOR('',#35987,1.);
#10811=VECTOR('',#35988,1.);
#10812=VECTOR('',#35989,1.);
#10813=VECTOR('',#35994,1.);
#10814=VECTOR('',#35997,1.);
#10815=VECTOR('',#35998,1.);
#10816=VECTOR('',#36005,1.);
#10817=VECTOR('',#36006,1.);
#10818=VECTOR('',#36007,1.);
#10819=VECTOR('',#36008,1.);
#10820=VECTOR('',#36013,1.);
#10821=VECTOR('',#36016,1.);
#10822=VECTOR('',#36017,1.);
#10823=VECTOR('',#36024,1.);
#10824=VECTOR('',#36025,1.);
#10825=VECTOR('',#36026,1.);
#10826=VECTOR('',#36027,1.);
#10827=VECTOR('',#36032,1.);
#10828=VECTOR('',#36035,1.);
#10829=VECTOR('',#36036,1.);
#10830=VECTOR('',#36045,1.);
#10831=VECTOR('',#36046,1.);
#10832=VECTOR('',#36049,1.);
#10833=VECTOR('',#36050,1.);
#10834=VECTOR('',#36051,1.);
#10835=VECTOR('',#36054,1.);
#10836=VECTOR('',#36055,1.);
#10837=VECTOR('',#36062,1.);
#10838=VECTOR('',#36063,1.);
#10839=VECTOR('',#36064,1.);
#10840=VECTOR('',#36065,1.);
#10841=VECTOR('',#36070,1.);
#10842=VECTOR('',#36073,1.);
#10843=VECTOR('',#36074,1.);
#10844=VECTOR('',#36081,1.);
#10845=VECTOR('',#36082,1.);
#10846=VECTOR('',#36083,1.);
#10847=VECTOR('',#36084,1.);
#10848=VECTOR('',#36089,1.);
#10849=VECTOR('',#36092,1.);
#10850=VECTOR('',#36093,1.);
#10851=VECTOR('',#36100,1.);
#10852=VECTOR('',#36101,1.);
#10853=VECTOR('',#36102,1.);
#10854=VECTOR('',#36103,1.);
#10855=VECTOR('',#36108,1.);
#10856=VECTOR('',#36111,1.);
#10857=VECTOR('',#36112,1.);
#10858=VECTOR('',#36119,1.);
#10859=VECTOR('',#36120,1.);
#10860=VECTOR('',#36121,1.);
#10861=VECTOR('',#36122,1.);
#10862=VECTOR('',#36127,1.);
#10863=VECTOR('',#36130,1.);
#10864=VECTOR('',#36131,1.);
#10865=VECTOR('',#36138,1.);
#10866=VECTOR('',#36139,1.);
#10867=VECTOR('',#36140,1.);
#10868=VECTOR('',#36141,1.);
#10869=VECTOR('',#36146,1.);
#10870=VECTOR('',#36149,1.);
#10871=VECTOR('',#36150,1.);
#10872=VECTOR('',#36157,1.);
#10873=VECTOR('',#36158,1.);
#10874=VECTOR('',#36159,1.);
#10875=VECTOR('',#36160,1.);
#10876=VECTOR('',#36165,1.);
#10877=VECTOR('',#36168,1.);
#10878=VECTOR('',#36169,1.);
#10879=VECTOR('',#36176,1.);
#10880=VECTOR('',#36177,1.);
#10881=VECTOR('',#36178,1.);
#10882=VECTOR('',#36179,1.);
#10883=VECTOR('',#36184,1.);
#10884=VECTOR('',#36187,1.);
#10885=VECTOR('',#36188,1.);
#10886=VECTOR('',#36195,1.);
#10887=VECTOR('',#36196,1.);
#10888=VECTOR('',#36197,1.);
#10889=VECTOR('',#36198,1.);
#10890=VECTOR('',#36203,1.);
#10891=VECTOR('',#36206,1.);
#10892=VECTOR('',#36207,1.);
#10893=VECTOR('',#36214,1.);
#10894=VECTOR('',#36215,1.);
#10895=VECTOR('',#36216,1.);
#10896=VECTOR('',#36217,1.);
#10897=VECTOR('',#36222,1.);
#10898=VECTOR('',#36225,1.);
#10899=VECTOR('',#36226,1.);
#10900=VECTOR('',#36237,0.275);
#10901=VECTOR('',#36242,0.485);
#10902=VECTOR('',#36277,0.5);
#10903=VECTOR('',#36322,0.475);
#10904=VERTEX_POINT('',#36384);
#10905=VERTEX_POINT('',#36385);
#10906=VERTEX_POINT('',#36387);
#10907=VERTEX_POINT('',#36389);
#10908=VERTEX_POINT('',#36393);
#10909=VERTEX_POINT('',#36394);
#10910=VERTEX_POINT('',#36399);
#10911=VERTEX_POINT('',#36400);
#10912=VERTEX_POINT('',#36405);
#10913=VERTEX_POINT('',#36406);
#10914=VERTEX_POINT('',#36411);
#10915=VERTEX_POINT('',#36412);
#10916=VERTEX_POINT('',#36417);
#10917=VERTEX_POINT('',#36418);
#10918=VERTEX_POINT('',#36423);
#10919=VERTEX_POINT('',#36424);
#10920=VERTEX_POINT('',#36432);
#10921=VERTEX_POINT('',#36434);
#10922=VERTEX_POINT('',#36438);
#10923=VERTEX_POINT('',#36442);
#10924=VERTEX_POINT('',#36446);
#10925=VERTEX_POINT('',#36450);
#10926=VERTEX_POINT('',#36451);
#10927=VERTEX_POINT('',#36453);
#10928=VERTEX_POINT('',#36455);
#10929=VERTEX_POINT('',#36457);
#10930=VERTEX_POINT('',#36459);
#10931=VERTEX_POINT('',#36461);
#10932=VERTEX_POINT('',#36463);
#10933=VERTEX_POINT('',#36467);
#10934=VERTEX_POINT('',#36469);
#10935=VERTEX_POINT('',#36473);
#10936=VERTEX_POINT('',#36474);
#10937=VERTEX_POINT('',#36476);
#10938=VERTEX_POINT('',#36478);
#10939=VERTEX_POINT('',#36480);
#10940=VERTEX_POINT('',#36482);
#10941=VERTEX_POINT('',#36484);
#10942=VERTEX_POINT('',#36486);
#10943=VERTEX_POINT('',#36489);
#10944=VERTEX_POINT('',#36491);
#10945=VERTEX_POINT('',#36493);
#10946=VERTEX_POINT('',#36495);
#10947=VERTEX_POINT('',#36496);
#10948=VERTEX_POINT('',#36498);
#10949=VERTEX_POINT('',#36500);
#10950=VERTEX_POINT('',#36503);
#10951=VERTEX_POINT('',#36506);
#10952=VERTEX_POINT('',#36510);
#10953=VERTEX_POINT('',#36514);
#10954=VERTEX_POINT('',#36518);
#10955=VERTEX_POINT('',#36522);
#10956=VERTEX_POINT('',#36526);
#10957=VERTEX_POINT('',#36530);
#10958=VERTEX_POINT('',#36534);
#10959=VERTEX_POINT('',#36536);
#10960=VERTEX_POINT('',#36540);
#10961=VERTEX_POINT('',#36542);
#10962=VERTEX_POINT('',#36550);
#10963=VERTEX_POINT('',#36552);
#10964=VERTEX_POINT('',#36556);
#10965=VERTEX_POINT('',#36560);
#10966=VERTEX_POINT('',#36561);
#10967=VERTEX_POINT('',#36563);
#10968=VERTEX_POINT('',#36566);
#10969=VERTEX_POINT('',#36570);
#10970=VERTEX_POINT('',#36571);
#10971=VERTEX_POINT('',#36576);
#10972=VERTEX_POINT('',#36577);
#10973=VERTEX_POINT('',#36582);
#10974=VERTEX_POINT('',#36583);
#10975=VERTEX_POINT('',#36588);
#10976=VERTEX_POINT('',#36589);
#10977=VERTEX_POINT('',#36591);
#10978=VERTEX_POINT('',#36597);
#10979=VERTEX_POINT('',#36601);
#10980=VERTEX_POINT('',#36607);
#10981=VERTEX_POINT('',#36609);
#10982=VERTEX_POINT('',#36612);
#10983=VERTEX_POINT('',#36616);
#10984=VERTEX_POINT('',#36620);
#10985=VERTEX_POINT('',#36624);
#10986=VERTEX_POINT('',#36628);
#10987=VERTEX_POINT('',#36631);
#10988=VERTEX_POINT('',#36635);
#10989=VERTEX_POINT('',#36637);
#10990=VERTEX_POINT('',#36639);
#10991=VERTEX_POINT('',#36643);
#10992=VERTEX_POINT('',#36644);
#10993=VERTEX_POINT('',#36646);
#10994=VERTEX_POINT('',#36648);
#10995=VERTEX_POINT('',#36650);
#10996=VERTEX_POINT('',#36654);
#10997=VERTEX_POINT('',#36656);
#10998=VERTEX_POINT('',#36660);
#10999=VERTEX_POINT('',#36662);
#11000=VERTEX_POINT('',#36664);
#11001=VERTEX_POINT('',#36668);
#11002=VERTEX_POINT('',#36670);
#11003=VERTEX_POINT('',#36672);
#11004=VERTEX_POINT('',#36674);
#11005=VERTEX_POINT('',#36678);
#11006=VERTEX_POINT('',#36680);
#11007=VERTEX_POINT('',#36682);
#11008=VERTEX_POINT('',#36686);
#11009=VERTEX_POINT('',#36688);
#11010=VERTEX_POINT('',#36690);
#11011=VERTEX_POINT('',#36694);
#11012=VERTEX_POINT('',#36696);
#11013=VERTEX_POINT('',#36700);
#11014=VERTEX_POINT('',#36702);
#11015=VERTEX_POINT('',#36706);
#11016=VERTEX_POINT('',#36708);
#11017=VERTEX_POINT('',#36712);
#11018=VERTEX_POINT('',#36716);
#11019=VERTEX_POINT('',#36718);
#11020=VERTEX_POINT('',#36722);
#11021=VERTEX_POINT('',#36726);
#11022=VERTEX_POINT('',#36730);
#11023=VERTEX_POINT('',#36734);
#11024=VERTEX_POINT('',#36738);
#11025=VERTEX_POINT('',#36742);
#11026=VERTEX_POINT('',#36748);
#11027=VERTEX_POINT('',#36750);
#11028=VERTEX_POINT('',#36754);
#11029=VERTEX_POINT('',#36758);
#11030=VERTEX_POINT('',#36762);
#11031=VERTEX_POINT('',#36766);
#11032=VERTEX_POINT('',#36768);
#11033=VERTEX_POINT('',#36772);
#11034=VERTEX_POINT('',#36773);
#11035=VERTEX_POINT('',#36778);
#11036=VERTEX_POINT('',#36779);
#11037=VERTEX_POINT('',#36781);
#11038=VERTEX_POINT('',#36783);
#11039=VERTEX_POINT('',#36788);
#11040=VERTEX_POINT('',#36796);
#11041=VERTEX_POINT('',#36800);
#11042=VERTEX_POINT('',#36807);
#11043=VERTEX_POINT('',#36809);
#11044=VERTEX_POINT('',#36812);
#11045=VERTEX_POINT('',#36819);
#11046=VERTEX_POINT('',#36821);
#11047=VERTEX_POINT('',#36823);
#11048=VERTEX_POINT('',#36827);
#11049=VERTEX_POINT('',#36831);
#11050=VERTEX_POINT('',#36835);
#11051=VERTEX_POINT('',#36840);
#11052=VERTEX_POINT('',#36846);
#11053=VERTEX_POINT('',#36850);
#11054=VERTEX_POINT('',#36854);
#11055=VERTEX_POINT('',#36860);
#11056=VERTEX_POINT('',#36861);
#11057=VERTEX_POINT('',#36863);
#11058=VERTEX_POINT('',#36867);
#11059=VERTEX_POINT('',#36868);
#11060=VERTEX_POINT('',#36870);
#11061=VERTEX_POINT('',#36874);
#11062=VERTEX_POINT('',#36875);
#11063=VERTEX_POINT('',#36880);
#11064=VERTEX_POINT('',#36881);
#11065=VERTEX_POINT('',#36886);
#11066=VERTEX_POINT('',#36887);
#11067=VERTEX_POINT('',#36892);
#11068=VERTEX_POINT('',#36893);
#11069=VERTEX_POINT('',#36904);
#11070=VERTEX_POINT('',#36905);
#11071=VERTEX_POINT('',#36908);
#11072=VERTEX_POINT('',#36912);
#11073=VERTEX_POINT('',#36913);
#11074=VERTEX_POINT('',#36916);
#11075=VERTEX_POINT('',#36920);
#11076=VERTEX_POINT('',#36926);
#11077=VERTEX_POINT('',#36930);
#11078=VERTEX_POINT('',#36934);
#11079=VERTEX_POINT('',#36938);
#11080=VERTEX_POINT('',#36967);
#11081=VERTEX_POINT('',#36975);
#11082=VERTEX_POINT('',#36990);
#11083=VERTEX_POINT('',#37020);
#11084=VERTEX_POINT('',#37023);
#11085=VERTEX_POINT('',#37026);
#11086=VERTEX_POINT('',#37029);
#11087=VERTEX_POINT('',#37032);
#11088=VERTEX_POINT('',#37041);
#11089=VERTEX_POINT('',#37043);
#11090=VERTEX_POINT('',#37045);
#11091=VERTEX_POINT('',#37049);
#11092=VERTEX_POINT('',#37051);
#11093=VERTEX_POINT('',#37055);
#11094=VERTEX_POINT('',#37058);
#11095=VERTEX_POINT('',#37060);
#11096=VERTEX_POINT('',#37064);
#11097=VERTEX_POINT('',#37066);
#11098=VERTEX_POINT('',#37136);
#11099=VERTEX_POINT('',#37137);
#11100=VERTEX_POINT('',#37144);
#11101=VERTEX_POINT('',#37146);
#11102=VERTEX_POINT('',#37148);
#11103=VERTEX_POINT('',#37153);
#11104=VERTEX_POINT('',#37154);
#11105=VERTEX_POINT('',#37157);
#11106=VERTEX_POINT('',#37160);
#11107=VERTEX_POINT('',#37162);
#11108=VERTEX_POINT('',#37169);
#11109=VERTEX_POINT('',#37171);
#11110=VERTEX_POINT('',#37178);
#11111=VERTEX_POINT('',#37180);
#11112=VERTEX_POINT('',#37189);
#11113=VERTEX_POINT('',#37193);
#11114=VERTEX_POINT('',#37195);
#11115=VERTEX_POINT('',#37200);
#11116=VERTEX_POINT('',#37204);
#11117=VERTEX_POINT('',#37205);
#11118=VERTEX_POINT('',#37207);
#11119=VERTEX_POINT('',#37209);
#11120=VERTEX_POINT('',#37211);
#11121=VERTEX_POINT('',#37213);
#11122=VERTEX_POINT('',#37217);
#11123=VERTEX_POINT('',#37219);
#11124=VERTEX_POINT('',#37221);
#11125=VERTEX_POINT('',#37226);
#11126=VERTEX_POINT('',#37228);
#11127=VERTEX_POINT('',#37233);
#11128=VERTEX_POINT('',#37236);
#11129=VERTEX_POINT('',#37237);
#11130=VERTEX_POINT('',#37239);
#11131=VERTEX_POINT('',#37241);
#11132=VERTEX_POINT('',#37244);
#11133=VERTEX_POINT('',#37245);
#11134=VERTEX_POINT('',#37247);
#11135=VERTEX_POINT('',#37249);
#11136=VERTEX_POINT('',#37253);
#11137=VERTEX_POINT('',#37255);
#11138=VERTEX_POINT('',#37259);
#11139=VERTEX_POINT('',#37261);
#11140=VERTEX_POINT('',#37265);
#11141=VERTEX_POINT('',#37267);
#11142=VERTEX_POINT('',#37271);
#11143=VERTEX_POINT('',#37275);
#11144=VERTEX_POINT('',#37469);
#11145=VERTEX_POINT('',#37470);
#11146=VERTEX_POINT('',#37472);
#11147=VERTEX_POINT('',#37574);
#11148=VERTEX_POINT('',#37575);
#11149=VERTEX_POINT('',#37579);
#11150=VERTEX_POINT('',#37580);
#11151=VERTEX_POINT('',#37582);
#11152=VERTEX_POINT('',#37590);
#11153=VERTEX_POINT('',#37618);
#11154=VERTEX_POINT('',#37626);
#11155=VERTEX_POINT('',#37628);
#11156=VERTEX_POINT('',#37639);
#11157=VERTEX_POINT('',#37652);
#11158=VERTEX_POINT('',#37658);
#11159=VERTEX_POINT('',#37659);
#11160=VERTEX_POINT('',#37661);
#11161=VERTEX_POINT('',#37663);
#11162=VERTEX_POINT('',#37667);
#11163=VERTEX_POINT('',#37669);
#11164=VERTEX_POINT('',#37673);
#11165=VERTEX_POINT('',#37675);
#11166=VERTEX_POINT('',#37710);
#11167=VERTEX_POINT('',#37711);
#11168=VERTEX_POINT('',#37752);
#11169=VERTEX_POINT('',#37757);
#11170=VERTEX_POINT('',#37843);
#11171=VERTEX_POINT('',#37844);
#11172=VERTEX_POINT('',#37897);
#11173=VERTEX_POINT('',#37902);
#11174=VERTEX_POINT('',#37969);
#11175=VERTEX_POINT('',#37977);
#11176=VERTEX_POINT('',#37979);
#11177=VERTEX_POINT('',#37983);
#11178=VERTEX_POINT('',#37985);
#11179=VERTEX_POINT('',#37989);
#11180=VERTEX_POINT('',#37990);
#11181=VERTEX_POINT('',#37992);
#11182=VERTEX_POINT('',#37996);
#11183=VERTEX_POINT('',#37998);
#11184=VERTEX_POINT('',#38002);
#11185=VERTEX_POINT('',#38003);
#11186=VERTEX_POINT('',#38005);
#11187=VERTEX_POINT('',#38009);
#11188=VERTEX_POINT('',#38010);
#11189=VERTEX_POINT('',#38015);
#11190=VERTEX_POINT('',#38016);
#11191=VERTEX_POINT('',#38021);
#11192=VERTEX_POINT('',#38022);
#11193=VERTEX_POINT('',#38027);
#11194=VERTEX_POINT('',#38028);
#11195=VERTEX_POINT('',#38036);
#11196=VERTEX_POINT('',#38038);
#11197=VERTEX_POINT('',#38051);
#11198=VERTEX_POINT('',#38055);
#11199=VERTEX_POINT('',#38098);
#11200=VERTEX_POINT('',#38131);
#11201=VERTEX_POINT('',#38133);
#11202=VERTEX_POINT('',#38137);
#11203=VERTEX_POINT('',#38139);
#11204=VERTEX_POINT('',#38180);
#11205=VERTEX_POINT('',#38191);
#11206=VERTEX_POINT('',#38199);
#11207=VERTEX_POINT('',#38201);
#11208=VERTEX_POINT('',#38203);
#11209=VERTEX_POINT('',#38205);
#11210=VERTEX_POINT('',#38207);
#11211=VERTEX_POINT('',#38209);
#11212=VERTEX_POINT('',#38211);
#11213=VERTEX_POINT('',#38214);
#11214=VERTEX_POINT('',#38215);
#11215=VERTEX_POINT('',#38217);
#11216=VERTEX_POINT('',#38219);
#11217=VERTEX_POINT('',#38229);
#11218=VERTEX_POINT('',#38230);
#11219=VERTEX_POINT('',#38232);
#11220=VERTEX_POINT('',#38234);
#11221=VERTEX_POINT('',#38237);
#11222=VERTEX_POINT('',#38238);
#11223=VERTEX_POINT('',#38240);
#11224=VERTEX_POINT('',#38242);
#11225=VERTEX_POINT('',#38246);
#11226=VERTEX_POINT('',#38248);
#11227=VERTEX_POINT('',#38252);
#11228=VERTEX_POINT('',#38256);
#11229=VERTEX_POINT('',#38262);
#11230=VERTEX_POINT('',#38264);
#11231=VERTEX_POINT('',#38268);
#11232=VERTEX_POINT('',#38272);
#11233=VERTEX_POINT('',#38274);
#11234=VERTEX_POINT('',#38278);
#11235=VERTEX_POINT('',#38282);
#11236=VERTEX_POINT('',#38288);
#11237=VERTEX_POINT('',#38290);
#11238=VERTEX_POINT('',#38294);
#11239=VERTEX_POINT('',#38298);
#11240=VERTEX_POINT('',#38300);
#11241=VERTEX_POINT('',#38304);
#11242=VERTEX_POINT('',#38308);
#11243=VERTEX_POINT('',#38314);
#11244=VERTEX_POINT('',#38316);
#11245=VERTEX_POINT('',#38320);
#11246=VERTEX_POINT('',#38324);
#11247=VERTEX_POINT('',#38326);
#11248=VERTEX_POINT('',#38330);
#11249=VERTEX_POINT('',#38334);
#11250=VERTEX_POINT('',#38340);
#11251=VERTEX_POINT('',#38342);
#11252=VERTEX_POINT('',#38346);
#11253=VERTEX_POINT('',#38350);
#11254=VERTEX_POINT('',#38352);
#11255=VERTEX_POINT('',#38354);
#11256=VERTEX_POINT('',#38359);
#11257=VERTEX_POINT('',#38363);
#11258=VERTEX_POINT('',#38365);
#11259=VERTEX_POINT('',#38370);
#11260=VERTEX_POINT('',#38374);
#11261=VERTEX_POINT('',#38376);
#11262=VERTEX_POINT('',#38380);
#11263=VERTEX_POINT('',#38381);
#11264=VERTEX_POINT('',#38386);
#11265=VERTEX_POINT('',#38395);
#11266=VERTEX_POINT('',#38396);
#11267=VERTEX_POINT('',#38401);
#11268=VERTEX_POINT('',#38403);
#11269=VERTEX_POINT('',#38405);
#11270=VERTEX_POINT('',#38407);
#11271=VERTEX_POINT('',#38409);
#11272=VERTEX_POINT('',#38411);
#11273=VERTEX_POINT('',#38413);
#11274=VERTEX_POINT('',#38416);
#11275=VERTEX_POINT('',#38418);
#11276=VERTEX_POINT('',#38420);
#11277=VERTEX_POINT('',#38422);
#11278=VERTEX_POINT('',#38427);
#11279=VERTEX_POINT('',#38429);
#11280=VERTEX_POINT('',#38431);
#11281=VERTEX_POINT('',#38433);
#11282=VERTEX_POINT('',#38435);
#11283=VERTEX_POINT('',#38437);
#11284=VERTEX_POINT('',#38440);
#11285=VERTEX_POINT('',#38441);
#11286=VERTEX_POINT('',#38443);
#11287=VERTEX_POINT('',#38445);
#11288=VERTEX_POINT('',#38448);
#11289=VERTEX_POINT('',#38449);
#11290=VERTEX_POINT('',#38451);
#11291=VERTEX_POINT('',#38453);
#11292=VERTEX_POINT('',#38456);
#11293=VERTEX_POINT('',#38457);
#11294=VERTEX_POINT('',#38459);
#11295=VERTEX_POINT('',#38461);
#11296=VERTEX_POINT('',#38468);
#11297=VERTEX_POINT('',#38481);
#11298=VERTEX_POINT('',#38494);
#11299=VERTEX_POINT('',#38535);
#11300=VERTEX_POINT('',#38624);
#11301=VERTEX_POINT('',#38665);
#11302=VERTEX_POINT('',#38750);
#11303=VERTEX_POINT('',#38767);
#11304=VERTEX_POINT('',#38769);
#11305=VERTEX_POINT('',#38773);
#11306=VERTEX_POINT('',#38777);
#11307=VERTEX_POINT('',#38781);
#11308=VERTEX_POINT('',#38889);
#11309=VERTEX_POINT('',#38891);
#11310=VERTEX_POINT('',#38898);
#11311=VERTEX_POINT('',#38900);
#11312=VERTEX_POINT('',#38983);
#11313=VERTEX_POINT('',#38984);
#11314=VERTEX_POINT('',#38986);
#11315=VERTEX_POINT('',#39007);
#11316=VERTEX_POINT('',#39078);
#11317=VERTEX_POINT('',#39082);
#11318=VERTEX_POINT('',#39088);
#11319=VERTEX_POINT('',#39090);
#11320=VERTEX_POINT('',#39092);
#11321=VERTEX_POINT('',#39146);
#11322=VERTEX_POINT('',#39156);
#11323=VERTEX_POINT('',#39201);
#11324=VERTEX_POINT('',#39299);
#11325=VERTEX_POINT('',#39330);
#11326=VERTEX_POINT('',#39333);
#11327=VERTEX_POINT('',#39336);
#11328=VERTEX_POINT('',#39339);
#11329=VERTEX_POINT('',#39342);
#11330=VERTEX_POINT('',#39345);
#11331=VERTEX_POINT('',#39347);
#11332=VERTEX_POINT('',#39385);
#11333=VERTEX_POINT('',#39386);
#11334=VERTEX_POINT('',#39423);
#11335=VERTEX_POINT('',#39427);
#11336=VERTEX_POINT('',#39432);
#11337=VERTEX_POINT('',#39438);
#11338=VERTEX_POINT('',#39440);
#11339=VERTEX_POINT('',#39442);
#11340=VERTEX_POINT('',#39446);
#11341=VERTEX_POINT('',#39450);
#11342=VERTEX_POINT('',#39453);
#11343=VERTEX_POINT('',#39454);
#11344=VERTEX_POINT('',#39456);
#11345=VERTEX_POINT('',#39458);
#11346=VERTEX_POINT('',#39462);
#11347=VERTEX_POINT('',#39464);
#11348=VERTEX_POINT('',#39468);
#11349=VERTEX_POINT('',#39470);
#11350=VERTEX_POINT('',#39478);
#11351=VERTEX_POINT('',#39479);
#11352=VERTEX_POINT('',#39481);
#11353=VERTEX_POINT('',#39483);
#11354=VERTEX_POINT('',#39487);
#11355=VERTEX_POINT('',#39489);
#11356=VERTEX_POINT('',#39493);
#11357=VERTEX_POINT('',#39495);
#11358=VERTEX_POINT('',#39503);
#11359=VERTEX_POINT('',#39504);
#11360=VERTEX_POINT('',#39506);
#11361=VERTEX_POINT('',#39508);
#11362=VERTEX_POINT('',#39512);
#11363=VERTEX_POINT('',#39514);
#11364=VERTEX_POINT('',#39518);
#11365=VERTEX_POINT('',#39520);
#11366=VERTEX_POINT('',#39528);
#11367=VERTEX_POINT('',#39529);
#11368=VERTEX_POINT('',#39531);
#11369=VERTEX_POINT('',#39533);
#11370=VERTEX_POINT('',#39537);
#11371=VERTEX_POINT('',#39539);
#11372=VERTEX_POINT('',#39543);
#11373=VERTEX_POINT('',#39545);
#11374=VERTEX_POINT('',#39553);
#11375=VERTEX_POINT('',#39554);
#11376=VERTEX_POINT('',#39556);
#11377=VERTEX_POINT('',#39558);
#11378=VERTEX_POINT('',#39562);
#11379=VERTEX_POINT('',#39564);
#11380=VERTEX_POINT('',#39568);
#11381=VERTEX_POINT('',#39570);
#11382=VERTEX_POINT('',#39578);
#11383=VERTEX_POINT('',#39579);
#11384=VERTEX_POINT('',#39581);
#11385=VERTEX_POINT('',#39583);
#11386=VERTEX_POINT('',#39587);
#11387=VERTEX_POINT('',#39589);
#11388=VERTEX_POINT('',#39593);
#11389=VERTEX_POINT('',#39595);
#11390=VERTEX_POINT('',#39603);
#11391=VERTEX_POINT('',#39604);
#11392=VERTEX_POINT('',#39606);
#11393=VERTEX_POINT('',#39608);
#11394=VERTEX_POINT('',#39612);
#11395=VERTEX_POINT('',#39614);
#11396=VERTEX_POINT('',#39618);
#11397=VERTEX_POINT('',#39620);
#11398=VERTEX_POINT('',#39628);
#11399=VERTEX_POINT('',#39629);
#11400=VERTEX_POINT('',#39631);
#11401=VERTEX_POINT('',#39633);
#11402=VERTEX_POINT('',#39637);
#11403=VERTEX_POINT('',#39639);
#11404=VERTEX_POINT('',#39643);
#11405=VERTEX_POINT('',#39645);
#11406=VERTEX_POINT('',#39653);
#11407=VERTEX_POINT('',#39654);
#11408=VERTEX_POINT('',#39656);
#11409=VERTEX_POINT('',#39658);
#11410=VERTEX_POINT('',#39662);
#11411=VERTEX_POINT('',#39664);
#11412=VERTEX_POINT('',#39668);
#11413=VERTEX_POINT('',#39670);
#11414=VERTEX_POINT('',#39678);
#11415=VERTEX_POINT('',#39679);
#11416=VERTEX_POINT('',#39681);
#11417=VERTEX_POINT('',#39683);
#11418=VERTEX_POINT('',#39687);
#11419=VERTEX_POINT('',#39689);
#11420=VERTEX_POINT('',#39693);
#11421=VERTEX_POINT('',#39695);
#11422=VERTEX_POINT('',#39703);
#11423=VERTEX_POINT('',#39704);
#11424=VERTEX_POINT('',#39706);
#11425=VERTEX_POINT('',#39708);
#11426=VERTEX_POINT('',#39712);
#11427=VERTEX_POINT('',#39714);
#11428=VERTEX_POINT('',#39718);
#11429=VERTEX_POINT('',#39720);
#11430=VERTEX_POINT('',#39728);
#11431=VERTEX_POINT('',#39729);
#11432=VERTEX_POINT('',#39731);
#11433=VERTEX_POINT('',#39733);
#11434=VERTEX_POINT('',#39737);
#11435=VERTEX_POINT('',#39739);
#11436=VERTEX_POINT('',#39743);
#11437=VERTEX_POINT('',#39745);
#11438=VERTEX_POINT('',#39753);
#11439=VERTEX_POINT('',#39754);
#11440=VERTEX_POINT('',#39756);
#11441=VERTEX_POINT('',#39758);
#11442=VERTEX_POINT('',#39762);
#11443=VERTEX_POINT('',#39764);
#11444=VERTEX_POINT('',#39768);
#11445=VERTEX_POINT('',#39770);
#11446=VERTEX_POINT('',#39778);
#11447=VERTEX_POINT('',#39779);
#11448=VERTEX_POINT('',#39781);
#11449=VERTEX_POINT('',#39783);
#11450=VERTEX_POINT('',#39787);
#11451=VERTEX_POINT('',#39789);
#11452=VERTEX_POINT('',#39793);
#11453=VERTEX_POINT('',#39795);
#11454=VERTEX_POINT('',#39803);
#11455=VERTEX_POINT('',#39804);
#11456=VERTEX_POINT('',#39806);
#11457=VERTEX_POINT('',#39808);
#11458=VERTEX_POINT('',#39812);
#11459=VERTEX_POINT('',#39814);
#11460=VERTEX_POINT('',#39818);
#11461=VERTEX_POINT('',#39820);
#11462=VERTEX_POINT('',#39828);
#11463=VERTEX_POINT('',#39829);
#11464=VERTEX_POINT('',#39831);
#11465=VERTEX_POINT('',#39833);
#11466=VERTEX_POINT('',#39837);
#11467=VERTEX_POINT('',#39839);
#11468=VERTEX_POINT('',#39843);
#11469=VERTEX_POINT('',#39845);
#11470=VERTEX_POINT('',#39853);
#11471=VERTEX_POINT('',#39854);
#11472=VERTEX_POINT('',#39856);
#11473=VERTEX_POINT('',#39858);
#11474=VERTEX_POINT('',#39862);
#11475=VERTEX_POINT('',#39864);
#11476=VERTEX_POINT('',#39868);
#11477=VERTEX_POINT('',#39870);
#11478=VERTEX_POINT('',#39878);
#11479=VERTEX_POINT('',#39879);
#11480=VERTEX_POINT('',#39881);
#11481=VERTEX_POINT('',#39883);
#11482=VERTEX_POINT('',#39887);
#11483=VERTEX_POINT('',#39889);
#11484=VERTEX_POINT('',#39893);
#11485=VERTEX_POINT('',#39895);
#11486=VERTEX_POINT('',#39903);
#11487=VERTEX_POINT('',#39904);
#11488=VERTEX_POINT('',#39906);
#11489=VERTEX_POINT('',#39908);
#11490=VERTEX_POINT('',#39912);
#11491=VERTEX_POINT('',#39914);
#11492=VERTEX_POINT('',#39918);
#11493=VERTEX_POINT('',#39920);
#11494=VERTEX_POINT('',#39928);
#11495=VERTEX_POINT('',#39929);
#11496=VERTEX_POINT('',#39931);
#11497=VERTEX_POINT('',#39933);
#11498=VERTEX_POINT('',#39937);
#11499=VERTEX_POINT('',#39939);
#11500=VERTEX_POINT('',#39943);
#11501=VERTEX_POINT('',#39945);
#11502=VERTEX_POINT('',#39953);
#11503=VERTEX_POINT('',#39954);
#11504=VERTEX_POINT('',#39956);
#11505=VERTEX_POINT('',#39958);
#11506=VERTEX_POINT('',#39962);
#11507=VERTEX_POINT('',#39964);
#11508=VERTEX_POINT('',#39968);
#11509=VERTEX_POINT('',#39970);
#11510=VERTEX_POINT('',#39978);
#11511=VERTEX_POINT('',#39979);
#11512=VERTEX_POINT('',#39981);
#11513=VERTEX_POINT('',#39983);
#11514=VERTEX_POINT('',#39987);
#11515=VERTEX_POINT('',#40006);
#11516=VERTEX_POINT('',#40010);
#11517=VERTEX_POINT('',#40012);
#11518=VERTEX_POINT('',#40037);
#11519=VERTEX_POINT('',#40039);
#11520=VERTEX_POINT('',#40043);
#11521=VERTEX_POINT('',#40046);
#11522=VERTEX_POINT('',#40052);
#11523=VERTEX_POINT('',#40056);
#11524=VERTEX_POINT('',#40060);
#11525=VERTEX_POINT('',#40063);
#11526=VERTEX_POINT('',#40069);
#11527=VERTEX_POINT('',#40070);
#11528=VERTEX_POINT('',#40073);
#11529=VERTEX_POINT('',#40075);
#11530=VERTEX_POINT('',#40079);
#11531=VERTEX_POINT('',#40083);
#11532=VERTEX_POINT('',#40086);
#11533=VERTEX_POINT('',#40089);
#11534=VERTEX_POINT('',#40096);
#11535=VERTEX_POINT('',#40097);
#11536=VERTEX_POINT('',#40099);
#11537=VERTEX_POINT('',#40122);
#11538=VERTEX_POINT('',#40129);
#11539=VERTEX_POINT('',#40130);
#11540=VERTEX_POINT('',#40213);
#11541=VERTEX_POINT('',#40214);
#11542=VERTEX_POINT('',#40300);
#11543=VERTEX_POINT('',#40301);
#11544=VERTEX_POINT('',#40384);
#11545=VERTEX_POINT('',#40385);
#11546=VERTEX_POINT('',#40456);
#11547=VERTEX_POINT('',#40457);
#11548=VERTEX_POINT('',#40525);
#11549=VERTEX_POINT('',#40526);
#11550=VERTEX_POINT('',#40609);
#11551=VERTEX_POINT('',#40610);
#11552=VERTEX_POINT('',#40693);
#11553=VERTEX_POINT('',#40694);
#11554=VERTEX_POINT('',#40780);
#11555=VERTEX_POINT('',#40781);
#11556=VERTEX_POINT('',#40864);
#11557=VERTEX_POINT('',#40865);
#11558=VERTEX_POINT('',#40951);
#11559=VERTEX_POINT('',#40952);
#11560=VERTEX_POINT('',#41035);
#11561=VERTEX_POINT('',#41036);
#11562=VERTEX_POINT('',#41119);
#11563=VERTEX_POINT('',#41120);
#11564=VERTEX_POINT('',#41206);
#11565=VERTEX_POINT('',#41207);
#11566=VERTEX_POINT('',#41275);
#11567=VERTEX_POINT('',#41276);
#11568=VERTEX_POINT('',#41347);
#11569=VERTEX_POINT('',#41348);
#11570=VERTEX_POINT('',#41428);
#11571=VERTEX_POINT('',#41429);
#11572=VERTEX_POINT('',#41515);
#11573=VERTEX_POINT('',#41516);
#11574=VERTEX_POINT('',#41602);
#11575=VERTEX_POINT('',#41603);
#11576=VERTEX_POINT('',#41686);
#11577=VERTEX_POINT('',#41687);
#11578=VERTEX_POINT('',#41773);
#11579=VERTEX_POINT('',#41774);
#11580=VERTEX_POINT('',#41845);
#11581=VERTEX_POINT('',#41846);
#11582=VERTEX_POINT('',#41935);
#11583=VERTEX_POINT('',#41936);
#11584=VERTEX_POINT('',#42019);
#11585=VERTEX_POINT('',#42020);
#11586=VERTEX_POINT('',#42103);
#11587=VERTEX_POINT('',#42104);
#11588=VERTEX_POINT('',#42190);
#11589=VERTEX_POINT('',#42191);
#11590=VERTEX_POINT('',#42271);
#11591=VERTEX_POINT('',#42272);
#11592=VERTEX_POINT('',#42343);
#11593=VERTEX_POINT('',#42344);
#11594=VERTEX_POINT('',#42412);
#11595=VERTEX_POINT('',#42413);
#11596=VERTEX_POINT('',#42496);
#11597=VERTEX_POINT('',#42497);
#11598=VERTEX_POINT('',#42580);
#11599=VERTEX_POINT('',#42581);
#11600=VERTEX_POINT('',#42664);
#11601=VERTEX_POINT('',#42665);
#11602=VERTEX_POINT('',#42754);
#11603=VERTEX_POINT('',#42755);
#11604=VERTEX_POINT('',#42838);
#11605=VERTEX_POINT('',#42839);
#11606=VERTEX_POINT('',#42922);
#11607=VERTEX_POINT('',#42923);
#11608=VERTEX_POINT('',#43006);
#11609=VERTEX_POINT('',#43007);
#11610=VERTEX_POINT('',#43090);
#11611=VERTEX_POINT('',#43091);
#11612=VERTEX_POINT('',#43159);
#11613=VERTEX_POINT('',#43160);
#11614=VERTEX_POINT('',#43243);
#11615=VERTEX_POINT('',#43244);
#11616=VERTEX_POINT('',#43330);
#11617=VERTEX_POINT('',#43331);
#11618=VERTEX_POINT('',#43414);
#11619=VERTEX_POINT('',#43415);
#11620=VERTEX_POINT('',#43498);
#11621=VERTEX_POINT('',#43499);
#11622=VERTEX_POINT('',#43501);
#11623=VERTEX_POINT('',#43512);
#11624=VERTEX_POINT('',#43520);
#11625=VERTEX_POINT('',#43521);
#11626=VERTEX_POINT('',#43555);
#11627=VERTEX_POINT('',#43556);
#11628=VERTEX_POINT('',#43592);
#11629=VERTEX_POINT('',#43593);
#11630=VERTEX_POINT('',#43628);
#11631=VERTEX_POINT('',#43629);
#11632=VERTEX_POINT('',#43664);
#11633=VERTEX_POINT('',#43665);
#11634=VERTEX_POINT('',#43710);
#11635=VERTEX_POINT('',#43711);
#11636=VERTEX_POINT('',#43745);
#11637=VERTEX_POINT('',#43746);
#11638=VERTEX_POINT('',#43782);
#11639=VERTEX_POINT('',#43783);
#11640=VERTEX_POINT('',#43817);
#11641=VERTEX_POINT('',#43818);
#11642=VERTEX_POINT('',#43854);
#11643=VERTEX_POINT('',#43855);
#11644=VERTEX_POINT('',#43891);
#11645=VERTEX_POINT('',#43892);
#11646=VERTEX_POINT('',#43927);
#11647=VERTEX_POINT('',#43928);
#11648=VERTEX_POINT('',#43964);
#11649=VERTEX_POINT('',#43965);
#11650=VERTEX_POINT('',#43999);
#11651=VERTEX_POINT('',#44000);
#11652=VERTEX_POINT('',#44036);
#11653=VERTEX_POINT('',#44037);
#11654=VERTEX_POINT('',#44081);
#11655=VERTEX_POINT('',#44082);
#11656=VERTEX_POINT('',#44117);
#11657=VERTEX_POINT('',#44118);
#11658=VERTEX_POINT('',#44153);
#11659=VERTEX_POINT('',#44154);
#11660=VERTEX_POINT('',#44189);
#11661=VERTEX_POINT('',#44190);
#11662=VERTEX_POINT('',#44226);
#11663=VERTEX_POINT('',#44227);
#11664=VERTEX_POINT('',#44263);
#11665=VERTEX_POINT('',#44264);
#11666=VERTEX_POINT('',#44298);
#11667=VERTEX_POINT('',#44299);
#11668=VERTEX_POINT('',#44332);
#11669=VERTEX_POINT('',#44333);
#11670=VERTEX_POINT('',#44369);
#11671=VERTEX_POINT('',#44370);
#11672=VERTEX_POINT('',#44405);
#11673=VERTEX_POINT('',#44406);
#11674=VERTEX_POINT('',#44442);
#11675=VERTEX_POINT('',#44443);
#11676=VERTEX_POINT('',#44478);
#11677=VERTEX_POINT('',#44479);
#11678=VERTEX_POINT('',#44514);
#11679=VERTEX_POINT('',#44515);
#11680=VERTEX_POINT('',#44550);
#11681=VERTEX_POINT('',#44551);
#11682=VERTEX_POINT('',#44586);
#11683=VERTEX_POINT('',#44587);
#11684=VERTEX_POINT('',#44623);
#11685=VERTEX_POINT('',#44624);
#11686=VERTEX_POINT('',#44658);
#11687=VERTEX_POINT('',#44659);
#11688=VERTEX_POINT('',#44695);
#11689=VERTEX_POINT('',#44696);
#11690=VERTEX_POINT('',#44732);
#11691=VERTEX_POINT('',#44733);
#11692=VERTEX_POINT('',#44768);
#11693=VERTEX_POINT('',#44769);
#11694=VERTEX_POINT('',#44805);
#11695=VERTEX_POINT('',#44806);
#11696=VERTEX_POINT('',#44840);
#11697=VERTEX_POINT('',#44841);
#11698=VERTEX_POINT('',#44877);
#11699=VERTEX_POINT('',#44878);
#11700=VERTEX_POINT('',#44912);
#11701=VERTEX_POINT('',#44913);
#11702=VERTEX_POINT('',#44949);
#11703=VERTEX_POINT('',#44950);
#11704=VERTEX_POINT('',#44985);
#11705=VERTEX_POINT('',#44986);
#11706=VERTEX_POINT('',#45021);
#11707=VERTEX_POINT('',#45023);
#11708=VERTEX_POINT('',#45025);
#11709=VERTEX_POINT('',#45029);
#11710=VERTEX_POINT('',#45031);
#11711=VERTEX_POINT('',#45033);
#11712=VERTEX_POINT('',#45038);
#11713=VERTEX_POINT('',#45040);
#11714=VERTEX_POINT('',#45044);
#11715=VERTEX_POINT('',#45048);
#11716=VERTEX_POINT('',#45051);
#11717=VERTEX_POINT('',#45113);
#11718=VERTEX_POINT('',#47152);
#11719=VERTEX_POINT('',#47209);
#11720=VERTEX_POINT('',#47278);
#11721=VERTEX_POINT('',#49486);
#11722=VERTEX_POINT('',#49544);
#11723=VERTEX_POINT('',#49547);
#11724=VERTEX_POINT('',#49548);
#11725=VERTEX_POINT('',#49550);
#11726=VERTEX_POINT('',#49552);
#11727=VERTEX_POINT('',#49556);
#11728=VERTEX_POINT('',#49575);
#11729=VERTEX_POINT('',#49579);
#11730=VERTEX_POINT('',#49581);
#11731=VERTEX_POINT('',#49606);
#11732=VERTEX_POINT('',#49610);
#11733=VERTEX_POINT('',#49614);
#11734=VERTEX_POINT('',#49617);
#11735=VERTEX_POINT('',#49621);
#11736=VERTEX_POINT('',#49625);
#11737=VERTEX_POINT('',#49631);
#11738=VERTEX_POINT('',#49633);
#11739=VERTEX_POINT('',#49635);
#11740=VERTEX_POINT('',#49639);
#11741=VERTEX_POINT('',#49640);
#11742=VERTEX_POINT('',#49645);
#11743=VERTEX_POINT('',#49648);
#11744=VERTEX_POINT('',#49650);
#11745=VERTEX_POINT('',#49654);
#11746=VERTEX_POINT('',#49658);
#11747=VERTEX_POINT('',#49660);
#11748=VERTEX_POINT('',#49663);
#11749=VERTEX_POINT('',#49667);
#11750=VERTEX_POINT('',#49670);
#11751=VERTEX_POINT('',#49676);
#11752=VERTEX_POINT('',#49680);
#11753=VERTEX_POINT('',#49684);
#11754=VERTEX_POINT('',#49690);
#11755=VERTEX_POINT('',#49691);
#11756=VERTEX_POINT('',#49694);
#11757=VERTEX_POINT('',#49698);
#11758=VERTEX_POINT('',#49701);
#11759=VERTEX_POINT('',#49705);
#11760=VERTEX_POINT('',#49707);
#11761=VERTEX_POINT('',#49709);
#11762=VERTEX_POINT('',#49713);
#11763=VERTEX_POINT('',#49715);
#11764=VERTEX_POINT('',#49719);
#11765=VERTEX_POINT('',#49721);
#11766=VERTEX_POINT('',#49723);
#11767=VERTEX_POINT('',#49725);
#11768=VERTEX_POINT('',#49727);
#11769=VERTEX_POINT('',#49730);
#11770=VERTEX_POINT('',#49732);
#11771=VERTEX_POINT('',#49736);
#11772=VERTEX_POINT('',#49738);
#11773=VERTEX_POINT('',#49742);
#11774=VERTEX_POINT('',#49744);
#11775=VERTEX_POINT('',#49748);
#11776=VERTEX_POINT('',#49750);
#11777=VERTEX_POINT('',#49754);
#11778=VERTEX_POINT('',#49758);
#11779=VERTEX_POINT('',#49760);
#11780=VERTEX_POINT('',#49762);
#11781=VERTEX_POINT('',#49764);
#11782=VERTEX_POINT('',#49766);
#11783=VERTEX_POINT('',#49769);
#11784=VERTEX_POINT('',#49770);
#11785=VERTEX_POINT('',#49773);
#11786=VERTEX_POINT('',#49775);
#11787=VERTEX_POINT('',#49779);
#11788=VERTEX_POINT('',#49781);
#11789=VERTEX_POINT('',#49787);
#11790=VERTEX_POINT('',#49791);
#11791=VERTEX_POINT('',#49794);
#11792=VERTEX_POINT('',#49796);
#11793=VERTEX_POINT('',#49800);
#11794=VERTEX_POINT('',#49812);
#11795=VERTEX_POINT('',#49818);
#11796=VERTEX_POINT('',#49821);
#11797=VERTEX_POINT('',#49827);
#11798=VERTEX_POINT('',#49828);
#11799=VERTEX_POINT('',#49831);
#11800=VERTEX_POINT('',#49833);
#11801=VERTEX_POINT('',#49837);
#11802=VERTEX_POINT('',#49839);
#11803=VERTEX_POINT('',#49842);
#11804=VERTEX_POINT('',#49843);
#11805=VERTEX_POINT('',#49880);
#11806=VERTEX_POINT('',#49881);
#11807=VERTEX_POINT('',#49918);
#11808=VERTEX_POINT('',#49919);
#11809=VERTEX_POINT('',#49956);
#11810=VERTEX_POINT('',#49957);
#11811=VERTEX_POINT('',#49995);
#11812=VERTEX_POINT('',#49996);
#11813=VERTEX_POINT('',#50001);
#11814=VERTEX_POINT('',#50003);
#11815=VERTEX_POINT('',#50007);
#11816=VERTEX_POINT('',#50009);
#11817=VERTEX_POINT('',#50013);
#11818=VERTEX_POINT('',#50017);
#11819=VERTEX_POINT('',#50020);
#11820=VERTEX_POINT('',#50024);
#11821=VERTEX_POINT('',#50025);
#11822=VERTEX_POINT('',#50027);
#11823=VERTEX_POINT('',#50029);
#11824=VERTEX_POINT('',#50033);
#11825=VERTEX_POINT('',#50034);
#11826=VERTEX_POINT('',#50039);
#11827=VERTEX_POINT('',#50041);
#11828=VERTEX_POINT('',#50047);
#11829=VERTEX_POINT('',#50049);
#11830=VERTEX_POINT('',#50053);
#11831=VERTEX_POINT('',#50057);
#11832=VERTEX_POINT('',#50063);
#11833=VERTEX_POINT('',#50064);
#11834=VERTEX_POINT('',#50081);
#11835=VERTEX_POINT('',#50122);
#11836=VERTEX_POINT('',#50123);
#11837=VERTEX_POINT('',#50140);
#11838=VERTEX_POINT('',#50181);
#11839=VERTEX_POINT('',#50182);
#11840=VERTEX_POINT('',#50199);
#11841=VERTEX_POINT('',#50240);
#11842=VERTEX_POINT('',#50241);
#11843=VERTEX_POINT('',#50258);
#11844=VERTEX_POINT('',#50299);
#11845=VERTEX_POINT('',#50307);
#11846=VERTEX_POINT('',#50313);
#11847=VERTEX_POINT('',#50314);
#11848=VERTEX_POINT('',#50316);
#11849=VERTEX_POINT('',#50327);
#11850=VERTEX_POINT('',#50337);
#11851=VERTEX_POINT('',#50338);
#11852=VERTEX_POINT('',#50385);
#11853=VERTEX_POINT('',#50386);
#11854=VERTEX_POINT('',#50433);
#11855=VERTEX_POINT('',#50434);
#11856=VERTEX_POINT('',#50487);
#11857=VERTEX_POINT('',#50488);
#11858=VERTEX_POINT('',#50535);
#11859=VERTEX_POINT('',#50536);
#11860=VERTEX_POINT('',#50583);
#11861=VERTEX_POINT('',#50584);
#11862=VERTEX_POINT('',#50637);
#11863=VERTEX_POINT('',#50638);
#11864=VERTEX_POINT('',#50685);
#11865=VERTEX_POINT('',#50686);
#11866=VERTEX_POINT('',#50733);
#11867=VERTEX_POINT('',#50734);
#11868=VERTEX_POINT('',#50787);
#11869=VERTEX_POINT('',#50788);
#11870=VERTEX_POINT('',#50835);
#11871=VERTEX_POINT('',#50836);
#11872=VERTEX_POINT('',#50883);
#11873=VERTEX_POINT('',#50884);
#11874=VERTEX_POINT('',#50937);
#11875=VERTEX_POINT('',#50938);
#11876=VERTEX_POINT('',#50985);
#11877=VERTEX_POINT('',#50986);
#11878=VERTEX_POINT('',#51033);
#11879=VERTEX_POINT('',#51034);
#11880=VERTEX_POINT('',#51087);
#11881=VERTEX_POINT('',#51088);
#11882=VERTEX_POINT('',#51090);
#11883=VERTEX_POINT('',#51100);
#11884=VERTEX_POINT('',#51110);
#11885=VERTEX_POINT('',#51111);
#11886=VERTEX_POINT('',#51135);
#11887=VERTEX_POINT('',#51136);
#11888=VERTEX_POINT('',#51159);
#11889=VERTEX_POINT('',#51160);
#11890=VERTEX_POINT('',#51184);
#11891=VERTEX_POINT('',#51185);
#11892=VERTEX_POINT('',#51209);
#11893=VERTEX_POINT('',#51210);
#11894=VERTEX_POINT('',#51233);
#11895=VERTEX_POINT('',#51234);
#11896=VERTEX_POINT('',#51258);
#11897=VERTEX_POINT('',#51259);
#11898=VERTEX_POINT('',#51283);
#11899=VERTEX_POINT('',#51284);
#11900=VERTEX_POINT('',#51307);
#11901=VERTEX_POINT('',#51308);
#11902=VERTEX_POINT('',#51332);
#11903=VERTEX_POINT('',#51333);
#11904=VERTEX_POINT('',#51357);
#11905=VERTEX_POINT('',#51358);
#11906=VERTEX_POINT('',#51381);
#11907=VERTEX_POINT('',#51382);
#11908=VERTEX_POINT('',#51406);
#11909=VERTEX_POINT('',#51407);
#11910=VERTEX_POINT('',#51431);
#11911=VERTEX_POINT('',#51432);
#11912=VERTEX_POINT('',#51455);
#11913=VERTEX_POINT('',#51517);
#11914=VERTEX_POINT('',#51519);
#11915=VERTEX_POINT('',#52001);
#11916=VERTEX_POINT('',#52073);
#11917=VERTEX_POINT('',#52076);
#11918=VERTEX_POINT('',#52565);
#11919=VERTEX_POINT('',#52571);
#11920=VERTEX_POINT('',#52574);
#11921=VERTEX_POINT('',#52575);
#11922=VERTEX_POINT('',#52579);
#11923=VERTEX_POINT('',#52583);
#11924=VERTEX_POINT('',#52587);
#11925=VERTEX_POINT('',#52591);
#11926=VERTEX_POINT('',#52598);
#11927=VERTEX_POINT('',#52601);
#11928=VERTEX_POINT('',#52602);
#11929=VERTEX_POINT('',#52607);
#11930=VERTEX_POINT('',#52611);
#11931=VERTEX_POINT('',#52615);
#11932=VERTEX_POINT('',#52619);
#11933=VERTEX_POINT('',#52625);
#11934=VERTEX_POINT('',#52626);
#11935=VERTEX_POINT('',#52628);
#11936=VERTEX_POINT('',#52630);
#11937=VERTEX_POINT('',#52634);
#11938=VERTEX_POINT('',#52638);
#11939=VERTEX_POINT('',#52644);
#11940=VERTEX_POINT('',#52645);
#11941=VERTEX_POINT('',#52647);
#11942=VERTEX_POINT('',#52649);
#11943=VERTEX_POINT('',#52653);
#11944=VERTEX_POINT('',#52657);
#11945=VERTEX_POINT('',#52663);
#11946=VERTEX_POINT('',#52664);
#11947=VERTEX_POINT('',#52666);
#11948=VERTEX_POINT('',#52668);
#11949=VERTEX_POINT('',#52672);
#11950=VERTEX_POINT('',#52676);
#11951=VERTEX_POINT('',#52682);
#11952=VERTEX_POINT('',#52683);
#11953=VERTEX_POINT('',#52685);
#11954=VERTEX_POINT('',#52687);
#11955=VERTEX_POINT('',#52691);
#11956=VERTEX_POINT('',#52695);
#11957=VERTEX_POINT('',#52701);
#11958=VERTEX_POINT('',#52702);
#11959=VERTEX_POINT('',#52704);
#11960=VERTEX_POINT('',#52706);
#11961=VERTEX_POINT('',#52710);
#11962=VERTEX_POINT('',#52714);
#11963=VERTEX_POINT('',#52720);
#11964=VERTEX_POINT('',#52721);
#11965=VERTEX_POINT('',#52723);
#11966=VERTEX_POINT('',#52725);
#11967=VERTEX_POINT('',#52729);
#11968=VERTEX_POINT('',#52733);
#11969=VERTEX_POINT('',#52739);
#11970=VERTEX_POINT('',#52740);
#11971=VERTEX_POINT('',#52742);
#11972=VERTEX_POINT('',#52744);
#11973=VERTEX_POINT('',#52748);
#11974=VERTEX_POINT('',#52752);
#11975=VERTEX_POINT('',#52758);
#11976=VERTEX_POINT('',#52759);
#11977=VERTEX_POINT('',#52761);
#11978=VERTEX_POINT('',#52763);
#11979=VERTEX_POINT('',#52767);
#11980=VERTEX_POINT('',#52771);
#11981=VERTEX_POINT('',#52777);
#11982=VERTEX_POINT('',#52778);
#11983=VERTEX_POINT('',#52780);
#11984=VERTEX_POINT('',#52782);
#11985=VERTEX_POINT('',#52786);
#11986=VERTEX_POINT('',#52788);
#11987=VERTEX_POINT('',#52792);
#11988=VERTEX_POINT('',#52796);
#11989=VERTEX_POINT('',#52800);
#11990=VERTEX_POINT('',#52801);
#11991=VERTEX_POINT('',#52803);
#11992=VERTEX_POINT('',#52805);
#11993=VERTEX_POINT('',#52809);
#11994=VERTEX_POINT('',#52813);
#11995=VERTEX_POINT('',#52819);
#11996=VERTEX_POINT('',#52820);
#11997=VERTEX_POINT('',#52822);
#11998=VERTEX_POINT('',#52824);
#11999=VERTEX_POINT('',#52828);
#12000=VERTEX_POINT('',#52832);
#12001=VERTEX_POINT('',#52838);
#12002=VERTEX_POINT('',#52839);
#12003=VERTEX_POINT('',#52841);
#12004=VERTEX_POINT('',#52843);
#12005=VERTEX_POINT('',#52847);
#12006=VERTEX_POINT('',#52851);
#12007=VERTEX_POINT('',#52857);
#12008=VERTEX_POINT('',#52858);
#12009=VERTEX_POINT('',#52860);
#12010=VERTEX_POINT('',#52862);
#12011=VERTEX_POINT('',#52866);
#12012=VERTEX_POINT('',#52870);
#12013=VERTEX_POINT('',#52876);
#12014=VERTEX_POINT('',#52877);
#12015=VERTEX_POINT('',#52879);
#12016=VERTEX_POINT('',#52881);
#12017=VERTEX_POINT('',#52885);
#12018=VERTEX_POINT('',#52889);
#12019=VERTEX_POINT('',#52895);
#12020=VERTEX_POINT('',#52896);
#12021=VERTEX_POINT('',#52898);
#12022=VERTEX_POINT('',#52900);
#12023=VERTEX_POINT('',#52904);
#12024=VERTEX_POINT('',#52908);
#12025=VERTEX_POINT('',#52914);
#12026=VERTEX_POINT('',#52915);
#12027=VERTEX_POINT('',#52917);
#12028=VERTEX_POINT('',#52919);
#12029=VERTEX_POINT('',#52923);
#12030=VERTEX_POINT('',#52927);
#12031=VERTEX_POINT('',#52933);
#12032=VERTEX_POINT('',#52934);
#12033=VERTEX_POINT('',#52936);
#12034=VERTEX_POINT('',#52938);
#12035=VERTEX_POINT('',#52942);
#12036=VERTEX_POINT('',#52946);
#12037=VERTEX_POINT('',#52952);
#12038=VERTEX_POINT('',#52953);
#12039=VERTEX_POINT('',#52955);
#12040=VERTEX_POINT('',#52957);
#12041=VERTEX_POINT('',#52961);
#12042=VERTEX_POINT('',#52965);
#12043=VERTEX_POINT('',#52971);
#12044=VERTEX_POINT('',#52972);
#12045=VERTEX_POINT('',#52974);
#12046=VERTEX_POINT('',#52976);
#12047=VERTEX_POINT('',#52980);
#12048=VERTEX_POINT('',#52984);
#12049=VERTEX_POINT('',#52990);
#12050=VERTEX_POINT('',#52991);
#12051=VERTEX_POINT('',#52993);
#12052=VERTEX_POINT('',#52995);
#12053=VERTEX_POINT('',#52999);
#12054=VERTEX_POINT('',#53003);
#12055=VERTEX_POINT('',#53009);
#12056=VERTEX_POINT('',#53010);
#12057=VERTEX_POINT('',#53012);
#12058=VERTEX_POINT('',#53014);
#12059=VERTEX_POINT('',#53018);
#12060=VERTEX_POINT('',#53022);
#12061=VERTEX_POINT('',#53028);
#12062=VERTEX_POINT('',#53029);
#12063=VERTEX_POINT('',#53031);
#12064=VERTEX_POINT('',#53033);
#12065=VERTEX_POINT('',#53037);
#12066=VERTEX_POINT('',#53041);
#12067=VERTEX_POINT('',#53047);
#12068=VERTEX_POINT('',#53048);
#12069=VERTEX_POINT('',#53050);
#12070=VERTEX_POINT('',#53052);
#12071=VERTEX_POINT('',#53056);
#12072=VERTEX_POINT('',#53060);
#12073=VERTEX_POINT('',#53066);
#12074=VERTEX_POINT('',#53067);
#12075=VERTEX_POINT('',#53069);
#12076=VERTEX_POINT('',#53071);
#12077=VERTEX_POINT('',#53075);
#12078=VERTEX_POINT('',#53079);
#12079=VERTEX_POINT('',#53085);
#12080=VERTEX_POINT('',#53086);
#12081=VERTEX_POINT('',#53088);
#12082=VERTEX_POINT('',#53090);
#12083=VERTEX_POINT('',#53094);
#12084=VERTEX_POINT('',#53098);
#12085=VERTEX_POINT('',#53104);
#12086=VERTEX_POINT('',#53105);
#12087=VERTEX_POINT('',#53107);
#12088=VERTEX_POINT('',#53109);
#12089=VERTEX_POINT('',#53113);
#12090=VERTEX_POINT('',#53117);
#12091=VERTEX_POINT('',#53123);
#12092=VERTEX_POINT('',#53124);
#12093=VERTEX_POINT('',#53126);
#12094=VERTEX_POINT('',#53130);
#12095=VERTEX_POINT('',#53132);
#12096=VERTEX_POINT('',#53136);
#12097=VERTEX_POINT('',#53142);
#12098=VERTEX_POINT('',#53143);
#12099=VERTEX_POINT('',#53145);
#12100=VERTEX_POINT('',#53147);
#12101=VERTEX_POINT('',#53151);
#12102=VERTEX_POINT('',#53155);
#12103=VERTEX_POINT('',#53161);
#12104=VERTEX_POINT('',#53162);
#12105=VERTEX_POINT('',#53164);
#12106=VERTEX_POINT('',#53166);
#12107=VERTEX_POINT('',#53170);
#12108=VERTEX_POINT('',#53174);
#12109=VERTEX_POINT('',#53180);
#12110=VERTEX_POINT('',#53181);
#12111=VERTEX_POINT('',#53183);
#12112=VERTEX_POINT('',#53185);
#12113=VERTEX_POINT('',#53189);
#12114=VERTEX_POINT('',#53193);
#12115=VERTEX_POINT('',#53199);
#12116=VERTEX_POINT('',#53200);
#12117=VERTEX_POINT('',#53202);
#12118=VERTEX_POINT('',#53204);
#12119=VERTEX_POINT('',#53208);
#12120=VERTEX_POINT('',#53212);
#12121=VERTEX_POINT('',#53218);
#12122=VERTEX_POINT('',#53219);
#12123=VERTEX_POINT('',#53221);
#12124=VERTEX_POINT('',#53223);
#12125=VERTEX_POINT('',#53227);
#12126=VERTEX_POINT('',#53231);
#12127=VERTEX_POINT('',#53237);
#12128=VERTEX_POINT('',#53238);
#12129=VERTEX_POINT('',#53240);
#12130=VERTEX_POINT('',#53242);
#12131=VERTEX_POINT('',#53246);
#12132=VERTEX_POINT('',#53250);
#12133=VERTEX_POINT('',#53256);
#12134=VERTEX_POINT('',#53257);
#12135=VERTEX_POINT('',#53259);
#12136=VERTEX_POINT('',#53261);
#12137=VERTEX_POINT('',#53265);
#12138=VERTEX_POINT('',#53269);
#12139=VERTEX_POINT('',#53275);
#12140=VERTEX_POINT('',#53276);
#12141=VERTEX_POINT('',#53278);
#12142=VERTEX_POINT('',#53280);
#12143=VERTEX_POINT('',#53284);
#12144=VERTEX_POINT('',#53288);
#12145=VERTEX_POINT('',#53294);
#12146=VERTEX_POINT('',#53295);
#12147=VERTEX_POINT('',#53297);
#12148=VERTEX_POINT('',#53299);
#12149=VERTEX_POINT('',#53303);
#12150=VERTEX_POINT('',#53307);
#12151=VERTEX_POINT('',#53313);
#12152=VERTEX_POINT('',#53318);
#12153=VERTEX_POINT('',#53360);
#12154=VERTEX_POINT('',#53366);
#12155=VERTEX_POINT('',#53367);
#12156=VERTEX_POINT('',#53369);
#12157=VERTEX_POINT('',#53371);
#12158=VERTEX_POINT('',#53375);
#12159=VERTEX_POINT('',#53376);
#12160=VERTEX_POINT('',#53381);
#12161=VERTEX_POINT('',#53382);
#12162=VERTEX_POINT('',#53390);
#12163=VERTEX_POINT('',#53392);
#12164=VERTEX_POINT('',#53396);
#12165=VERTEX_POINT('',#53401);
#12166=VERTEX_POINT('',#53403);
#12167=VERTEX_POINT('',#53407);
#12168=VERTEX_POINT('',#53408);
#12169=VERTEX_POINT('',#53413);
#12170=VERTEX_POINT('',#53425);
#12171=VERTEX_POINT('',#53426);
#12172=VERTEX_POINT('',#53428);
#12173=VERTEX_POINT('',#53445);
#12174=VERTEX_POINT('',#53458);
#12175=VERTEX_POINT('',#53459);
#12176=VERTEX_POINT('',#53542);
#12177=VERTEX_POINT('',#53543);
#12178=VERTEX_POINT('',#53632);
#12179=VERTEX_POINT('',#53633);
#12180=VERTEX_POINT('',#53722);
#12181=VERTEX_POINT('',#53723);
#12182=VERTEX_POINT('',#53806);
#12183=VERTEX_POINT('',#53807);
#12184=VERTEX_POINT('',#53896);
#12185=VERTEX_POINT('',#53897);
#12186=VERTEX_POINT('',#53986);
#12187=VERTEX_POINT('',#53987);
#12188=VERTEX_POINT('',#54070);
#12189=VERTEX_POINT('',#54071);
#12190=VERTEX_POINT('',#54160);
#12191=VERTEX_POINT('',#54161);
#12192=VERTEX_POINT('',#54250);
#12193=VERTEX_POINT('',#54251);
#12194=VERTEX_POINT('',#54253);
#12195=VERTEX_POINT('',#54268);
#12196=VERTEX_POINT('',#54282);
#12197=VERTEX_POINT('',#54283);
#12198=VERTEX_POINT('',#54320);
#12199=VERTEX_POINT('',#54321);
#12200=VERTEX_POINT('',#54357);
#12201=VERTEX_POINT('',#54358);
#12202=VERTEX_POINT('',#54394);
#12203=VERTEX_POINT('',#54395);
#12204=VERTEX_POINT('',#54432);
#12205=VERTEX_POINT('',#54433);
#12206=VERTEX_POINT('',#54469);
#12207=VERTEX_POINT('',#54470);
#12208=VERTEX_POINT('',#54506);
#12209=VERTEX_POINT('',#54507);
#12210=VERTEX_POINT('',#54544);
#12211=VERTEX_POINT('',#54545);
#12212=VERTEX_POINT('',#54581);
#12213=VERTEX_POINT('',#54582);
#12214=VERTEX_POINT('',#54589);
#12215=VERTEX_POINT('',#54591);
#12216=VERTEX_POINT('',#54600);
#12217=VERTEX_POINT('',#54607);
#12218=VERTEX_POINT('',#54609);
#12219=VERTEX_POINT('',#55125);
#12220=VERTEX_POINT('',#55209);
#12221=VERTEX_POINT('',#55298);
#12222=VERTEX_POINT('',#55301);
#12223=VERTEX_POINT('',#55894);
#12224=VERTEX_POINT('',#55976);
#12225=VERTEX_POINT('',#55992);
#12226=VERTEX_POINT('',#55994);
#12227=VERTEX_POINT('',#55996);
#12228=VERTEX_POINT('',#56013);
#12229=VERTEX_POINT('',#56015);
#12230=VERTEX_POINT('',#56019);
#12231=VERTEX_POINT('',#56021);
#12232=VERTEX_POINT('',#56027);
#12233=VERTEX_POINT('',#56034);
#12234=VERTEX_POINT('',#56040);
#12235=VERTEX_POINT('',#56041);
#12236=VERTEX_POINT('',#56079);
#12237=VERTEX_POINT('',#56083);
#12238=VERTEX_POINT('',#56089);
#12239=VERTEX_POINT('',#56090);
#12240=VERTEX_POINT('',#56092);
#12241=VERTEX_POINT('',#56103);
#12242=VERTEX_POINT('',#56113);
#12243=VERTEX_POINT('',#56114);
#12244=VERTEX_POINT('',#56161);
#12245=VERTEX_POINT('',#56162);
#12246=VERTEX_POINT('',#56209);
#12247=VERTEX_POINT('',#56210);
#12248=VERTEX_POINT('',#56257);
#12249=VERTEX_POINT('',#56258);
#12250=VERTEX_POINT('',#56311);
#12251=VERTEX_POINT('',#56312);
#12252=VERTEX_POINT('',#56359);
#12253=VERTEX_POINT('',#56360);
#12254=VERTEX_POINT('',#56407);
#12255=VERTEX_POINT('',#56408);
#12256=VERTEX_POINT('',#56461);
#12257=VERTEX_POINT('',#56462);
#12258=VERTEX_POINT('',#56509);
#12259=VERTEX_POINT('',#56510);
#12260=VERTEX_POINT('',#56557);
#12261=VERTEX_POINT('',#56558);
#12262=VERTEX_POINT('',#56611);
#12263=VERTEX_POINT('',#56612);
#12264=VERTEX_POINT('',#56659);
#12265=VERTEX_POINT('',#56660);
#12266=VERTEX_POINT('',#56707);
#12267=VERTEX_POINT('',#56708);
#12268=VERTEX_POINT('',#56755);
#12269=VERTEX_POINT('',#56756);
#12270=VERTEX_POINT('',#56758);
#12271=VERTEX_POINT('',#56765);
#12272=VERTEX_POINT('',#56772);
#12273=VERTEX_POINT('',#56773);
#12274=VERTEX_POINT('',#56797);
#12275=VERTEX_POINT('',#56798);
#12276=VERTEX_POINT('',#56821);
#12277=VERTEX_POINT('',#56822);
#12278=VERTEX_POINT('',#56845);
#12279=VERTEX_POINT('',#56846);
#12280=VERTEX_POINT('',#56870);
#12281=VERTEX_POINT('',#56871);
#12282=VERTEX_POINT('',#56895);
#12283=VERTEX_POINT('',#56896);
#12284=VERTEX_POINT('',#56919);
#12285=VERTEX_POINT('',#56920);
#12286=VERTEX_POINT('',#56944);
#12287=VERTEX_POINT('',#56945);
#12288=VERTEX_POINT('',#56969);
#12289=VERTEX_POINT('',#56970);
#12290=VERTEX_POINT('',#56993);
#12291=VERTEX_POINT('',#56994);
#12292=VERTEX_POINT('',#57018);
#12293=VERTEX_POINT('',#57019);
#12294=VERTEX_POINT('',#57043);
#12295=VERTEX_POINT('',#57044);
#12296=VERTEX_POINT('',#57067);
#12297=VERTEX_POINT('',#57068);
#12298=VERTEX_POINT('',#57462);
#12299=VERTEX_POINT('',#57549);
#12300=VERTEX_POINT('',#57627);
#12301=VERTEX_POINT('',#57630);
#12302=VERTEX_POINT('',#58074);
#12303=VERTEX_POINT('',#58157);
#12304=VERTEX_POINT('',#58160);
#12305=VERTEX_POINT('',#58161);
#12306=VERTEX_POINT('',#58163);
#12307=VERTEX_POINT('',#58165);
#12308=VERTEX_POINT('',#58169);
#12309=VERTEX_POINT('',#58171);
#12310=VERTEX_POINT('',#58175);
#12311=VERTEX_POINT('',#58177);
#12312=VERTEX_POINT('',#58181);
#12313=VERTEX_POINT('',#58183);
#12314=VERTEX_POINT('',#58187);
#12315=VERTEX_POINT('',#58189);
#12316=VERTEX_POINT('',#58197);
#12317=VERTEX_POINT('',#58203);
#12318=VERTEX_POINT('',#58207);
#12319=VERTEX_POINT('',#58213);
#12320=VERTEX_POINT('',#58214);
#12321=VERTEX_POINT('',#58216);
#12322=VERTEX_POINT('',#58218);
#12323=VERTEX_POINT('',#58220);
#12324=VERTEX_POINT('',#58222);
#12325=VERTEX_POINT('',#58226);
#12326=VERTEX_POINT('',#58228);
#12327=VERTEX_POINT('',#58232);
#12328=VERTEX_POINT('',#58234);
#12329=VERTEX_POINT('',#58236);
#12330=VERTEX_POINT('',#58240);
#12331=VERTEX_POINT('',#58242);
#12332=VERTEX_POINT('',#58244);
#12333=VERTEX_POINT('',#58248);
#12334=VERTEX_POINT('',#58250);
#12335=VERTEX_POINT('',#58252);
#12336=VERTEX_POINT('',#58256);
#12337=VERTEX_POINT('',#58258);
#12338=VERTEX_POINT('',#58260);
#12339=VERTEX_POINT('',#58262);
#12340=VERTEX_POINT('',#58266);
#12341=VERTEX_POINT('',#58270);
#12342=VERTEX_POINT('',#58272);
#12343=VERTEX_POINT('',#58276);
#12344=VERTEX_POINT('',#58278);
#12345=VERTEX_POINT('',#58280);
#12346=VERTEX_POINT('',#58282);
#12347=VERTEX_POINT('',#58286);
#12348=VERTEX_POINT('',#58288);
#12349=VERTEX_POINT('',#58292);
#12350=VERTEX_POINT('',#58297);
#12351=VERTEX_POINT('',#58312);
#12352=VERTEX_POINT('',#58313);
#12353=VERTEX_POINT('',#58315);
#12354=VERTEX_POINT('',#58332);
#12355=VERTEX_POINT('',#58345);
#12356=VERTEX_POINT('',#58346);
#12357=VERTEX_POINT('',#58429);
#12358=VERTEX_POINT('',#58430);
#12359=VERTEX_POINT('',#58519);
#12360=VERTEX_POINT('',#58520);
#12361=VERTEX_POINT('',#58609);
#12362=VERTEX_POINT('',#58610);
#12363=VERTEX_POINT('',#58693);
#12364=VERTEX_POINT('',#58694);
#12365=VERTEX_POINT('',#58783);
#12366=VERTEX_POINT('',#58784);
#12367=VERTEX_POINT('',#58873);
#12368=VERTEX_POINT('',#58874);
#12369=VERTEX_POINT('',#58957);
#12370=VERTEX_POINT('',#58958);
#12371=VERTEX_POINT('',#59047);
#12372=VERTEX_POINT('',#59048);
#12373=VERTEX_POINT('',#59137);
#12374=VERTEX_POINT('',#59138);
#12375=VERTEX_POINT('',#59221);
#12376=VERTEX_POINT('',#59222);
#12377=VERTEX_POINT('',#59311);
#12378=VERTEX_POINT('',#59312);
#12379=VERTEX_POINT('',#59401);
#12380=VERTEX_POINT('',#59402);
#12381=VERTEX_POINT('',#59485);
#12382=VERTEX_POINT('',#59486);
#12383=VERTEX_POINT('',#59575);
#12384=VERTEX_POINT('',#59576);
#12385=VERTEX_POINT('',#59665);
#12386=VERTEX_POINT('',#59666);
#12387=VERTEX_POINT('',#59749);
#12388=VERTEX_POINT('',#59750);
#12389=VERTEX_POINT('',#59839);
#12390=VERTEX_POINT('',#59840);
#12391=VERTEX_POINT('',#59926);
#12392=VERTEX_POINT('',#59927);
#12393=VERTEX_POINT('',#60013);
#12394=VERTEX_POINT('',#60014);
#12395=VERTEX_POINT('',#60016);
#12396=VERTEX_POINT('',#60024);
#12397=VERTEX_POINT('',#60025);
#12398=VERTEX_POINT('',#60044);
#12399=VERTEX_POINT('',#60062);
#12400=VERTEX_POINT('',#60063);
#12401=VERTEX_POINT('',#60098);
#12402=VERTEX_POINT('',#60099);
#12403=VERTEX_POINT('',#60136);
#12404=VERTEX_POINT('',#60137);
#12405=VERTEX_POINT('',#60173);
#12406=VERTEX_POINT('',#60174);
#12407=VERTEX_POINT('',#60210);
#12408=VERTEX_POINT('',#60211);
#12409=VERTEX_POINT('',#60248);
#12410=VERTEX_POINT('',#60249);
#12411=VERTEX_POINT('',#60285);
#12412=VERTEX_POINT('',#60286);
#12413=VERTEX_POINT('',#60322);
#12414=VERTEX_POINT('',#60323);
#12415=VERTEX_POINT('',#60360);
#12416=VERTEX_POINT('',#60361);
#12417=VERTEX_POINT('',#60397);
#12418=VERTEX_POINT('',#60398);
#12419=VERTEX_POINT('',#60434);
#12420=VERTEX_POINT('',#60435);
#12421=VERTEX_POINT('',#60472);
#12422=VERTEX_POINT('',#60473);
#12423=VERTEX_POINT('',#60509);
#12424=VERTEX_POINT('',#60510);
#12425=VERTEX_POINT('',#60546);
#12426=VERTEX_POINT('',#60547);
#12427=VERTEX_POINT('',#60584);
#12428=VERTEX_POINT('',#60585);
#12429=VERTEX_POINT('',#60621);
#12430=VERTEX_POINT('',#60622);
#12431=VERTEX_POINT('',#60658);
#12432=VERTEX_POINT('',#60659);
#12433=VERTEX_POINT('',#60696);
#12434=VERTEX_POINT('',#60697);
#12435=VERTEX_POINT('',#61760);
#12436=VERTEX_POINT('',#61862);
#12437=VERTEX_POINT('',#61951);
#12438=VERTEX_POINT('',#61954);
#12439=VERTEX_POINT('',#63073);
#12440=VERTEX_POINT('',#63167);
#12441=VERTEX_POINT('',#63168);
#12442=VERTEX_POINT('',#63172);
#12443=VERTEX_POINT('',#63176);
#12444=VERTEX_POINT('',#63180);
#12445=VERTEX_POINT('',#63184);
#12446=VERTEX_POINT('',#63188);
#12447=VERTEX_POINT('',#63191);
#12448=VERTEX_POINT('',#63199);
#12449=VERTEX_POINT('',#63201);
#12450=VERTEX_POINT('',#63205);
#12451=VERTEX_POINT('',#63209);
#12452=VERTEX_POINT('',#63213);
#12453=VERTEX_POINT('',#63215);
#12454=VERTEX_POINT('',#63218);
#12455=VERTEX_POINT('',#63227);
#12456=VERTEX_POINT('',#63234);
#12457=VERTEX_POINT('',#63240);
#12458=VERTEX_POINT('',#63242);
#12459=VERTEX_POINT('',#63246);
#12460=VERTEX_POINT('',#63250);
#12461=VERTEX_POINT('',#63251);
#12462=VERTEX_POINT('',#63253);
#12463=VERTEX_POINT('',#63255);
#12464=VERTEX_POINT('',#63257);
#12465=VERTEX_POINT('',#63259);
#12466=VERTEX_POINT('',#63261);
#12467=VERTEX_POINT('',#63263);
#12468=VERTEX_POINT('',#63267);
#12469=VERTEX_POINT('',#63271);
#12470=VERTEX_POINT('',#63275);
#12471=VERTEX_POINT('',#63279);
#12472=VERTEX_POINT('',#63283);
#12473=VERTEX_POINT('',#63287);
#12474=VERTEX_POINT('',#63288);
#12475=VERTEX_POINT('',#63290);
#12476=VERTEX_POINT('',#63292);
#12477=VERTEX_POINT('',#63294);
#12478=VERTEX_POINT('',#63296);
#12479=VERTEX_POINT('',#63298);
#12480=VERTEX_POINT('',#63300);
#12481=VERTEX_POINT('',#63304);
#12482=VERTEX_POINT('',#63305);
#12483=VERTEX_POINT('',#63307);
#12484=VERTEX_POINT('',#63309);
#12485=VERTEX_POINT('',#63313);
#12486=VERTEX_POINT('',#63314);
#12487=VERTEX_POINT('',#63319);
#12488=VERTEX_POINT('',#63320);
#12489=VERTEX_POINT('',#63325);
#12490=VERTEX_POINT('',#63326);
#12491=VERTEX_POINT('',#63331);
#12492=VERTEX_POINT('',#63332);
#12493=VERTEX_POINT('',#63337);
#12494=VERTEX_POINT('',#63338);
#12495=VERTEX_POINT('',#63343);
#12496=VERTEX_POINT('',#63344);
#12497=VERTEX_POINT('',#63352);
#12498=VERTEX_POINT('',#63354);
#12499=VERTEX_POINT('',#63358);
#12500=VERTEX_POINT('',#63362);
#12501=VERTEX_POINT('',#63366);
#12502=VERTEX_POINT('',#63379);
#12503=VERTEX_POINT('',#63381);
#12504=VERTEX_POINT('',#63385);
#12505=VERTEX_POINT('',#63389);
#12506=VERTEX_POINT('',#63393);
#12507=VERTEX_POINT('',#63397);
#12508=VERTEX_POINT('',#63401);
#12509=VERTEX_POINT('',#63405);
#12510=VERTEX_POINT('',#63411);
#12511=VERTEX_POINT('',#63413);
#12512=VERTEX_POINT('',#63417);
#12513=VERTEX_POINT('',#63421);
#12514=VERTEX_POINT('',#63425);
#12515=VERTEX_POINT('',#63438);
#12516=VERTEX_POINT('',#63439);
#12517=VERTEX_POINT('',#63444);
#12518=VERTEX_POINT('',#63445);
#12519=VERTEX_POINT('',#63450);
#12520=VERTEX_POINT('',#63451);
#12521=VERTEX_POINT('',#63481);
#12522=VERTEX_POINT('',#63483);
#12523=VERTEX_POINT('',#63487);
#12524=VERTEX_POINT('',#63491);
#12525=VERTEX_POINT('',#63495);
#12526=VERTEX_POINT('',#63497);
#12527=VERTEX_POINT('',#63501);
#12528=VERTEX_POINT('',#63504);
#12529=VERTEX_POINT('',#63508);
#12530=VERTEX_POINT('',#63513);
#12531=VERTEX_POINT('',#63517);
#12532=VERTEX_POINT('',#63520);
#12533=VERTEX_POINT('',#63524);
#12534=VERTEX_POINT('',#63528);
#12535=VERTEX_POINT('',#63531);
#12536=VERTEX_POINT('',#63535);
#12537=VERTEX_POINT('',#63538);
#12538=VERTEX_POINT('',#63544);
#12539=VERTEX_POINT('',#63545);
#12540=VERTEX_POINT('',#63547);
#12541=VERTEX_POINT('',#63564);
#12542=VERTEX_POINT('',#63577);
#12543=VERTEX_POINT('',#63578);
#12544=VERTEX_POINT('',#63661);
#12545=VERTEX_POINT('',#63662);
#12546=VERTEX_POINT('',#63751);
#12547=VERTEX_POINT('',#63752);
#12548=VERTEX_POINT('',#63835);
#12549=VERTEX_POINT('',#63836);
#12550=VERTEX_POINT('',#63925);
#12551=VERTEX_POINT('',#63926);
#12552=VERTEX_POINT('',#64015);
#12553=VERTEX_POINT('',#64016);
#12554=VERTEX_POINT('',#64099);
#12555=VERTEX_POINT('',#64100);
#12556=VERTEX_POINT('',#64189);
#12557=VERTEX_POINT('',#64190);
#12558=VERTEX_POINT('',#64273);
#12559=VERTEX_POINT('',#64274);
#12560=VERTEX_POINT('',#64363);
#12561=VERTEX_POINT('',#64364);
#12562=VERTEX_POINT('',#64453);
#12563=VERTEX_POINT('',#64454);
#12564=VERTEX_POINT('',#64537);
#12565=VERTEX_POINT('',#64538);
#12566=VERTEX_POINT('',#64627);
#12567=VERTEX_POINT('',#64628);
#12568=VERTEX_POINT('',#64711);
#12569=VERTEX_POINT('',#64712);
#12570=VERTEX_POINT('',#64801);
#12571=VERTEX_POINT('',#64802);
#12572=VERTEX_POINT('',#64885);
#12573=VERTEX_POINT('',#64886);
#12574=VERTEX_POINT('',#64975);
#12575=VERTEX_POINT('',#64976);
#12576=VERTEX_POINT('',#65065);
#12577=VERTEX_POINT('',#65066);
#12578=VERTEX_POINT('',#65149);
#12579=VERTEX_POINT('',#65150);
#12580=VERTEX_POINT('',#65239);
#12581=VERTEX_POINT('',#65240);
#12582=VERTEX_POINT('',#65323);
#12583=VERTEX_POINT('',#65324);
#12584=VERTEX_POINT('',#65413);
#12585=VERTEX_POINT('',#65414);
#12586=VERTEX_POINT('',#65500);
#12587=VERTEX_POINT('',#65501);
#12588=VERTEX_POINT('',#65503);
#12589=VERTEX_POINT('',#65519);
#12590=VERTEX_POINT('',#65534);
#12591=VERTEX_POINT('',#65535);
#12592=VERTEX_POINT('',#65572);
#12593=VERTEX_POINT('',#65573);
#12594=VERTEX_POINT('',#65609);
#12595=VERTEX_POINT('',#65610);
#12596=VERTEX_POINT('',#65646);
#12597=VERTEX_POINT('',#65647);
#12598=VERTEX_POINT('',#65683);
#12599=VERTEX_POINT('',#65684);
#12600=VERTEX_POINT('',#65720);
#12601=VERTEX_POINT('',#65721);
#12602=VERTEX_POINT('',#65758);
#12603=VERTEX_POINT('',#65759);
#12604=VERTEX_POINT('',#65795);
#12605=VERTEX_POINT('',#65796);
#12606=VERTEX_POINT('',#65832);
#12607=VERTEX_POINT('',#65833);
#12608=VERTEX_POINT('',#65869);
#12609=VERTEX_POINT('',#65870);
#12610=VERTEX_POINT('',#65906);
#12611=VERTEX_POINT('',#65907);
#12612=VERTEX_POINT('',#65943);
#12613=VERTEX_POINT('',#65944);
#12614=VERTEX_POINT('',#65980);
#12615=VERTEX_POINT('',#65981);
#12616=VERTEX_POINT('',#66018);
#12617=VERTEX_POINT('',#66019);
#12618=VERTEX_POINT('',#66055);
#12619=VERTEX_POINT('',#66056);
#12620=VERTEX_POINT('',#66092);
#12621=VERTEX_POINT('',#66093);
#12622=VERTEX_POINT('',#66129);
#12623=VERTEX_POINT('',#66130);
#12624=VERTEX_POINT('',#66166);
#12625=VERTEX_POINT('',#66167);
#12626=VERTEX_POINT('',#66204);
#12627=VERTEX_POINT('',#66205);
#12628=VERTEX_POINT('',#66241);
#12629=VERTEX_POINT('',#66242);
#12630=VERTEX_POINT('',#66278);
#12631=VERTEX_POINT('',#66279);
#12632=VERTEX_POINT('',#67478);
#12633=VERTEX_POINT('',#67565);
#12634=VERTEX_POINT('',#67654);
#12635=VERTEX_POINT('',#67657);
#12636=VERTEX_POINT('',#68906);
#12637=VERTEX_POINT('',#68994);
#12638=VERTEX_POINT('',#68995);
#12639=VERTEX_POINT('',#68999);
#12640=VERTEX_POINT('',#69003);
#12641=VERTEX_POINT('',#69007);
#12642=VERTEX_POINT('',#69011);
#12643=VERTEX_POINT('',#69015);
#12644=VERTEX_POINT('',#69018);
#12645=VERTEX_POINT('',#69026);
#12646=VERTEX_POINT('',#69028);
#12647=VERTEX_POINT('',#69032);
#12648=VERTEX_POINT('',#69036);
#12649=VERTEX_POINT('',#69040);
#12650=VERTEX_POINT('',#69042);
#12651=VERTEX_POINT('',#69045);
#12652=VERTEX_POINT('',#69054);
#12653=VERTEX_POINT('',#69061);
#12654=VERTEX_POINT('',#69067);
#12655=VERTEX_POINT('',#69068);
#12656=VERTEX_POINT('',#69070);
#12657=VERTEX_POINT('',#69081);
#12658=VERTEX_POINT('',#69094);
#12659=VERTEX_POINT('',#69095);
#12660=VERTEX_POINT('',#69142);
#12661=VERTEX_POINT('',#69143);
#12662=VERTEX_POINT('',#69190);
#12663=VERTEX_POINT('',#69191);
#12664=VERTEX_POINT('',#69238);
#12665=VERTEX_POINT('',#69239);
#12666=VERTEX_POINT('',#69292);
#12667=VERTEX_POINT('',#69293);
#12668=VERTEX_POINT('',#69340);
#12669=VERTEX_POINT('',#69341);
#12670=VERTEX_POINT('',#69388);
#12671=VERTEX_POINT('',#69389);
#12672=VERTEX_POINT('',#69442);
#12673=VERTEX_POINT('',#69443);
#12674=VERTEX_POINT('',#69490);
#12675=VERTEX_POINT('',#69491);
#12676=VERTEX_POINT('',#69538);
#12677=VERTEX_POINT('',#69539);
#12678=VERTEX_POINT('',#69589);
#12679=VERTEX_POINT('',#69590);
#12680=VERTEX_POINT('',#69640);
#12681=VERTEX_POINT('',#69641);
#12682=VERTEX_POINT('',#69688);
#12683=VERTEX_POINT('',#69689);
#12684=VERTEX_POINT('',#69736);
#12685=VERTEX_POINT('',#69737);
#12686=VERTEX_POINT('',#69790);
#12687=VERTEX_POINT('',#69791);
#12688=VERTEX_POINT('',#69838);
#12689=VERTEX_POINT('',#69839);
#12690=VERTEX_POINT('',#69886);
#12691=VERTEX_POINT('',#69887);
#12692=VERTEX_POINT('',#69940);
#12693=VERTEX_POINT('',#69941);
#12694=VERTEX_POINT('',#69988);
#12695=VERTEX_POINT('',#69989);
#12696=VERTEX_POINT('',#70036);
#12697=VERTEX_POINT('',#70037);
#12698=VERTEX_POINT('',#70084);
#12699=VERTEX_POINT('',#70085);
#12700=VERTEX_POINT('',#70138);
#12701=VERTEX_POINT('',#70139);
#12702=VERTEX_POINT('',#70186);
#12703=VERTEX_POINT('',#70187);
#12704=VERTEX_POINT('',#70189);
#12705=VERTEX_POINT('',#70195);
#12706=VERTEX_POINT('',#70202);
#12707=VERTEX_POINT('',#70203);
#12708=VERTEX_POINT('',#70227);
#12709=VERTEX_POINT('',#70228);
#12710=VERTEX_POINT('',#70252);
#12711=VERTEX_POINT('',#70253);
#12712=VERTEX_POINT('',#70277);
#12713=VERTEX_POINT('',#70278);
#12714=VERTEX_POINT('',#70301);
#12715=VERTEX_POINT('',#70302);
#12716=VERTEX_POINT('',#70325);
#12717=VERTEX_POINT('',#70326);
#12718=VERTEX_POINT('',#70350);
#12719=VERTEX_POINT('',#70351);
#12720=VERTEX_POINT('',#70375);
#12721=VERTEX_POINT('',#70376);
#12722=VERTEX_POINT('',#70399);
#12723=VERTEX_POINT('',#70400);
#12724=VERTEX_POINT('',#70424);
#12725=VERTEX_POINT('',#70425);
#12726=VERTEX_POINT('',#70449);
#12727=VERTEX_POINT('',#70450);
#12728=VERTEX_POINT('',#70473);
#12729=VERTEX_POINT('',#70474);
#12730=VERTEX_POINT('',#70498);
#12731=VERTEX_POINT('',#70499);
#12732=VERTEX_POINT('',#70522);
#12733=VERTEX_POINT('',#70523);
#12734=VERTEX_POINT('',#70547);
#12735=VERTEX_POINT('',#70548);
#12736=VERTEX_POINT('',#70571);
#12737=VERTEX_POINT('',#70572);
#12738=VERTEX_POINT('',#70596);
#12739=VERTEX_POINT('',#70597);
#12740=VERTEX_POINT('',#70621);
#12741=VERTEX_POINT('',#70622);
#12742=VERTEX_POINT('',#70645);
#12743=VERTEX_POINT('',#70646);
#12744=VERTEX_POINT('',#70670);
#12745=VERTEX_POINT('',#70671);
#12746=VERTEX_POINT('',#70695);
#12747=VERTEX_POINT('',#70696);
#12748=VERTEX_POINT('',#70719);
#12749=VERTEX_POINT('',#70720);
#12750=VERTEX_POINT('',#70743);
#12751=VERTEX_POINT('',#70811);
#12752=VERTEX_POINT('',#70813);
#12753=VERTEX_POINT('',#71502);
#12754=VERTEX_POINT('',#71580);
#12755=VERTEX_POINT('',#71583);
#12756=VERTEX_POINT('',#72283);
#12757=VERTEX_POINT('',#72289);
#12758=VERTEX_POINT('',#72292);
#12759=VERTEX_POINT('',#72293);
#12760=VERTEX_POINT('',#72297);
#12761=VERTEX_POINT('',#72301);
#12762=VERTEX_POINT('',#72305);
#12763=VERTEX_POINT('',#72309);
#12764=VERTEX_POINT('',#72316);
#12765=VERTEX_POINT('',#72319);
#12766=VERTEX_POINT('',#72320);
#12767=VERTEX_POINT('',#72325);
#12768=VERTEX_POINT('',#72329);
#12769=VERTEX_POINT('',#72333);
#12770=VERTEX_POINT('',#72337);
#12771=VERTEX_POINT('',#72343);
#12772=VERTEX_POINT('',#72344);
#12773=VERTEX_POINT('',#72346);
#12774=VERTEX_POINT('',#72348);
#12775=VERTEX_POINT('',#72352);
#12776=VERTEX_POINT('',#72356);
#12777=VERTEX_POINT('',#72362);
#12778=VERTEX_POINT('',#72363);
#12779=VERTEX_POINT('',#72365);
#12780=VERTEX_POINT('',#72367);
#12781=VERTEX_POINT('',#72371);
#12782=VERTEX_POINT('',#72375);
#12783=VERTEX_POINT('',#72381);
#12784=VERTEX_POINT('',#72382);
#12785=VERTEX_POINT('',#72384);
#12786=VERTEX_POINT('',#72386);
#12787=VERTEX_POINT('',#72390);
#12788=VERTEX_POINT('',#72394);
#12789=VERTEX_POINT('',#72400);
#12790=VERTEX_POINT('',#72401);
#12791=VERTEX_POINT('',#72403);
#12792=VERTEX_POINT('',#72405);
#12793=VERTEX_POINT('',#72409);
#12794=VERTEX_POINT('',#72413);
#12795=VERTEX_POINT('',#72419);
#12796=VERTEX_POINT('',#72420);
#12797=VERTEX_POINT('',#72422);
#12798=VERTEX_POINT('',#72424);
#12799=VERTEX_POINT('',#72428);
#12800=VERTEX_POINT('',#72432);
#12801=VERTEX_POINT('',#72438);
#12802=VERTEX_POINT('',#72439);
#12803=VERTEX_POINT('',#72441);
#12804=VERTEX_POINT('',#72443);
#12805=VERTEX_POINT('',#72447);
#12806=VERTEX_POINT('',#72451);
#12807=VERTEX_POINT('',#72457);
#12808=VERTEX_POINT('',#72458);
#12809=VERTEX_POINT('',#72460);
#12810=VERTEX_POINT('',#72462);
#12811=VERTEX_POINT('',#72466);
#12812=VERTEX_POINT('',#72470);
#12813=VERTEX_POINT('',#72476);
#12814=VERTEX_POINT('',#72477);
#12815=VERTEX_POINT('',#72479);
#12816=VERTEX_POINT('',#72481);
#12817=VERTEX_POINT('',#72485);
#12818=VERTEX_POINT('',#72489);
#12819=VERTEX_POINT('',#72495);
#12820=VERTEX_POINT('',#72496);
#12821=VERTEX_POINT('',#72498);
#12822=VERTEX_POINT('',#72500);
#12823=VERTEX_POINT('',#72504);
#12824=VERTEX_POINT('',#72506);
#12825=VERTEX_POINT('',#72510);
#12826=VERTEX_POINT('',#72514);
#12827=VERTEX_POINT('',#72518);
#12828=VERTEX_POINT('',#72519);
#12829=VERTEX_POINT('',#72521);
#12830=VERTEX_POINT('',#72523);
#12831=VERTEX_POINT('',#72527);
#12832=VERTEX_POINT('',#72531);
#12833=VERTEX_POINT('',#72537);
#12834=VERTEX_POINT('',#72538);
#12835=VERTEX_POINT('',#72540);
#12836=VERTEX_POINT('',#72542);
#12837=VERTEX_POINT('',#72546);
#12838=VERTEX_POINT('',#72550);
#12839=VERTEX_POINT('',#72556);
#12840=VERTEX_POINT('',#72557);
#12841=VERTEX_POINT('',#72559);
#12842=VERTEX_POINT('',#72561);
#12843=VERTEX_POINT('',#72565);
#12844=VERTEX_POINT('',#72569);
#12845=VERTEX_POINT('',#72575);
#12846=VERTEX_POINT('',#72576);
#12847=VERTEX_POINT('',#72578);
#12848=VERTEX_POINT('',#72580);
#12849=VERTEX_POINT('',#72584);
#12850=VERTEX_POINT('',#72588);
#12851=VERTEX_POINT('',#72594);
#12852=VERTEX_POINT('',#72595);
#12853=VERTEX_POINT('',#72597);
#12854=VERTEX_POINT('',#72599);
#12855=VERTEX_POINT('',#72603);
#12856=VERTEX_POINT('',#72607);
#12857=VERTEX_POINT('',#72613);
#12858=VERTEX_POINT('',#72614);
#12859=VERTEX_POINT('',#72616);
#12860=VERTEX_POINT('',#72618);
#12861=VERTEX_POINT('',#72622);
#12862=VERTEX_POINT('',#72626);
#12863=VERTEX_POINT('',#72632);
#12864=VERTEX_POINT('',#72633);
#12865=VERTEX_POINT('',#72635);
#12866=VERTEX_POINT('',#72637);
#12867=VERTEX_POINT('',#72641);
#12868=VERTEX_POINT('',#72645);
#12869=VERTEX_POINT('',#72651);
#12870=VERTEX_POINT('',#72652);
#12871=VERTEX_POINT('',#72654);
#12872=VERTEX_POINT('',#72656);
#12873=VERTEX_POINT('',#72660);
#12874=VERTEX_POINT('',#72664);
#12875=VERTEX_POINT('',#72670);
#12876=VERTEX_POINT('',#72671);
#12877=VERTEX_POINT('',#72673);
#12878=VERTEX_POINT('',#72675);
#12879=VERTEX_POINT('',#72679);
#12880=VERTEX_POINT('',#72683);
#12881=VERTEX_POINT('',#72689);
#12882=VERTEX_POINT('',#72690);
#12883=VERTEX_POINT('',#72692);
#12884=VERTEX_POINT('',#72694);
#12885=VERTEX_POINT('',#72698);
#12886=VERTEX_POINT('',#72702);
#12887=VERTEX_POINT('',#72708);
#12888=VERTEX_POINT('',#72709);
#12889=VERTEX_POINT('',#72711);
#12890=VERTEX_POINT('',#72713);
#12891=VERTEX_POINT('',#72717);
#12892=VERTEX_POINT('',#72721);
#12893=VERTEX_POINT('',#72727);
#12894=VERTEX_POINT('',#72728);
#12895=VERTEX_POINT('',#72730);
#12896=VERTEX_POINT('',#72732);
#12897=VERTEX_POINT('',#72736);
#12898=VERTEX_POINT('',#72740);
#12899=VERTEX_POINT('',#72746);
#12900=VERTEX_POINT('',#72747);
#12901=VERTEX_POINT('',#72749);
#12902=VERTEX_POINT('',#72751);
#12903=VERTEX_POINT('',#72755);
#12904=VERTEX_POINT('',#72759);
#12905=VERTEX_POINT('',#72765);
#12906=VERTEX_POINT('',#72766);
#12907=VERTEX_POINT('',#72768);
#12908=VERTEX_POINT('',#72770);
#12909=VERTEX_POINT('',#72774);
#12910=VERTEX_POINT('',#72778);
#12911=VERTEX_POINT('',#72784);
#12912=VERTEX_POINT('',#72785);
#12913=VERTEX_POINT('',#72787);
#12914=VERTEX_POINT('',#72789);
#12915=VERTEX_POINT('',#72793);
#12916=VERTEX_POINT('',#72797);
#12917=VERTEX_POINT('',#72803);
#12918=VERTEX_POINT('',#72804);
#12919=VERTEX_POINT('',#72806);
#12920=VERTEX_POINT('',#72808);
#12921=VERTEX_POINT('',#72812);
#12922=VERTEX_POINT('',#72816);
#12923=VERTEX_POINT('',#72822);
#12924=VERTEX_POINT('',#72823);
#12925=VERTEX_POINT('',#72825);
#12926=VERTEX_POINT('',#72827);
#12927=VERTEX_POINT('',#72831);
#12928=VERTEX_POINT('',#72835);
#12929=VERTEX_POINT('',#72841);
#12930=VERTEX_POINT('',#72842);
#12931=VERTEX_POINT('',#72844);
#12932=VERTEX_POINT('',#72848);
#12933=VERTEX_POINT('',#72850);
#12934=VERTEX_POINT('',#72854);
#12935=VERTEX_POINT('',#72860);
#12936=VERTEX_POINT('',#72861);
#12937=VERTEX_POINT('',#72863);
#12938=VERTEX_POINT('',#72865);
#12939=VERTEX_POINT('',#72869);
#12940=VERTEX_POINT('',#72873);
#12941=VERTEX_POINT('',#72879);
#12942=VERTEX_POINT('',#72880);
#12943=VERTEX_POINT('',#72882);
#12944=VERTEX_POINT('',#72884);
#12945=VERTEX_POINT('',#72888);
#12946=VERTEX_POINT('',#72892);
#12947=VERTEX_POINT('',#72898);
#12948=VERTEX_POINT('',#72899);
#12949=VERTEX_POINT('',#72901);
#12950=VERTEX_POINT('',#72903);
#12951=VERTEX_POINT('',#72907);
#12952=VERTEX_POINT('',#72911);
#12953=VERTEX_POINT('',#72917);
#12954=VERTEX_POINT('',#72918);
#12955=VERTEX_POINT('',#72920);
#12956=VERTEX_POINT('',#72922);
#12957=VERTEX_POINT('',#72926);
#12958=VERTEX_POINT('',#72930);
#12959=VERTEX_POINT('',#72936);
#12960=VERTEX_POINT('',#72937);
#12961=VERTEX_POINT('',#72939);
#12962=VERTEX_POINT('',#72941);
#12963=VERTEX_POINT('',#72945);
#12964=VERTEX_POINT('',#72949);
#12965=VERTEX_POINT('',#72955);
#12966=VERTEX_POINT('',#72956);
#12967=VERTEX_POINT('',#72958);
#12968=VERTEX_POINT('',#72960);
#12969=VERTEX_POINT('',#72964);
#12970=VERTEX_POINT('',#72968);
#12971=VERTEX_POINT('',#72974);
#12972=VERTEX_POINT('',#72975);
#12973=VERTEX_POINT('',#72977);
#12974=VERTEX_POINT('',#72979);
#12975=VERTEX_POINT('',#72983);
#12976=VERTEX_POINT('',#72987);
#12977=VERTEX_POINT('',#72993);
#12978=VERTEX_POINT('',#72994);
#12979=VERTEX_POINT('',#72996);
#12980=VERTEX_POINT('',#72998);
#12981=VERTEX_POINT('',#73002);
#12982=VERTEX_POINT('',#73006);
#12983=VERTEX_POINT('',#73012);
#12984=VERTEX_POINT('',#73013);
#12985=VERTEX_POINT('',#73015);
#12986=VERTEX_POINT('',#73017);
#12987=VERTEX_POINT('',#73021);
#12988=VERTEX_POINT('',#73025);
#12989=VERTEX_POINT('',#73031);
#12990=VERTEX_POINT('',#73036);
#12991=VERTEX_POINT('',#73078);
#12992=VERTEX_POINT('',#73084);
#12993=VERTEX_POINT('',#73085);
#12994=VERTEX_POINT('',#73087);
#12995=VERTEX_POINT('',#73098);
#12996=VERTEX_POINT('',#73108);
#12997=VERTEX_POINT('',#73109);
#12998=VERTEX_POINT('',#73156);
#12999=VERTEX_POINT('',#73157);
#13000=VERTEX_POINT('',#73204);
#13001=VERTEX_POINT('',#73205);
#13002=VERTEX_POINT('',#73258);
#13003=VERTEX_POINT('',#73259);
#13004=VERTEX_POINT('',#73306);
#13005=VERTEX_POINT('',#73307);
#13006=VERTEX_POINT('',#73354);
#13007=VERTEX_POINT('',#73355);
#13008=VERTEX_POINT('',#73405);
#13009=VERTEX_POINT('',#73406);
#13010=VERTEX_POINT('',#73453);
#13011=VERTEX_POINT('',#73454);
#13012=VERTEX_POINT('',#73501);
#13013=VERTEX_POINT('',#73502);
#13014=VERTEX_POINT('',#73549);
#13015=VERTEX_POINT('',#73550);
#13016=VERTEX_POINT('',#73603);
#13017=VERTEX_POINT('',#73604);
#13018=VERTEX_POINT('',#73651);
#13019=VERTEX_POINT('',#73652);
#13020=VERTEX_POINT('',#73699);
#13021=VERTEX_POINT('',#73700);
#13022=VERTEX_POINT('',#73753);
#13023=VERTEX_POINT('',#73754);
#13024=VERTEX_POINT('',#73801);
#13025=VERTEX_POINT('',#73802);
#13026=VERTEX_POINT('',#73849);
#13027=VERTEX_POINT('',#73850);
#13028=VERTEX_POINT('',#73903);
#13029=VERTEX_POINT('',#73904);
#13030=VERTEX_POINT('',#73951);
#13031=VERTEX_POINT('',#73952);
#13032=VERTEX_POINT('',#73999);
#13033=VERTEX_POINT('',#74000);
#13034=VERTEX_POINT('',#74002);
#13035=VERTEX_POINT('',#74052);
#13036=VERTEX_POINT('',#74053);
#13037=VERTEX_POINT('',#74055);
#13038=VERTEX_POINT('',#74064);
#13039=VERTEX_POINT('',#74073);
#13040=VERTEX_POINT('',#74074);
#13041=VERTEX_POINT('',#74098);
#13042=VERTEX_POINT('',#74099);
#13043=VERTEX_POINT('',#74122);
#13044=VERTEX_POINT('',#74123);
#13045=VERTEX_POINT('',#74147);
#13046=VERTEX_POINT('',#74148);
#13047=VERTEX_POINT('',#74172);
#13048=VERTEX_POINT('',#74173);
#13049=VERTEX_POINT('',#74196);
#13050=VERTEX_POINT('',#74197);
#13051=VERTEX_POINT('',#74221);
#13052=VERTEX_POINT('',#74222);
#13053=VERTEX_POINT('',#74246);
#13054=VERTEX_POINT('',#74247);
#13055=VERTEX_POINT('',#74270);
#13056=VERTEX_POINT('',#74271);
#13057=VERTEX_POINT('',#74295);
#13058=VERTEX_POINT('',#74296);
#13059=VERTEX_POINT('',#74320);
#13060=VERTEX_POINT('',#74321);
#13061=VERTEX_POINT('',#74344);
#13062=VERTEX_POINT('',#74345);
#13063=VERTEX_POINT('',#74368);
#13064=VERTEX_POINT('',#74369);
#13065=VERTEX_POINT('',#74393);
#13066=VERTEX_POINT('',#74394);
#13067=VERTEX_POINT('',#74418);
#13068=VERTEX_POINT('',#74419);
#13069=VERTEX_POINT('',#74442);
#13070=VERTEX_POINT('',#74443);
#13071=VERTEX_POINT('',#74467);
#13072=VERTEX_POINT('',#74468);
#13073=VERTEX_POINT('',#74492);
#13074=VERTEX_POINT('',#74493);
#13075=VERTEX_POINT('',#74571);
#13076=VERTEX_POINT('',#75143);
#13077=VERTEX_POINT('',#75209);
#13078=VERTEX_POINT('',#75212);
#13079=VERTEX_POINT('',#75790);
#13080=VERTEX_POINT('',#75796);
#13081=VERTEX_POINT('',#75799);
#13082=VERTEX_POINT('',#75800);
#13083=VERTEX_POINT('',#75804);
#13084=VERTEX_POINT('',#75808);
#13085=VERTEX_POINT('',#75812);
#13086=VERTEX_POINT('',#75816);
#13087=VERTEX_POINT('',#75823);
#13088=VERTEX_POINT('',#75826);
#13089=VERTEX_POINT('',#75827);
#13090=VERTEX_POINT('',#75832);
#13091=VERTEX_POINT('',#75836);
#13092=VERTEX_POINT('',#75840);
#13093=VERTEX_POINT('',#75844);
#13094=VERTEX_POINT('',#75850);
#13095=VERTEX_POINT('',#75851);
#13096=VERTEX_POINT('',#75853);
#13097=VERTEX_POINT('',#75855);
#13098=VERTEX_POINT('',#75859);
#13099=VERTEX_POINT('',#75863);
#13100=VERTEX_POINT('',#75869);
#13101=VERTEX_POINT('',#75870);
#13102=VERTEX_POINT('',#75872);
#13103=VERTEX_POINT('',#75874);
#13104=VERTEX_POINT('',#75878);
#13105=VERTEX_POINT('',#75882);
#13106=VERTEX_POINT('',#75888);
#13107=VERTEX_POINT('',#75889);
#13108=VERTEX_POINT('',#75891);
#13109=VERTEX_POINT('',#75893);
#13110=VERTEX_POINT('',#75897);
#13111=VERTEX_POINT('',#75901);
#13112=VERTEX_POINT('',#75907);
#13113=VERTEX_POINT('',#75908);
#13114=VERTEX_POINT('',#75910);
#13115=VERTEX_POINT('',#75912);
#13116=VERTEX_POINT('',#75916);
#13117=VERTEX_POINT('',#75920);
#13118=VERTEX_POINT('',#75926);
#13119=VERTEX_POINT('',#75927);
#13120=VERTEX_POINT('',#75929);
#13121=VERTEX_POINT('',#75931);
#13122=VERTEX_POINT('',#75935);
#13123=VERTEX_POINT('',#75939);
#13124=VERTEX_POINT('',#75945);
#13125=VERTEX_POINT('',#75946);
#13126=VERTEX_POINT('',#75948);
#13127=VERTEX_POINT('',#75950);
#13128=VERTEX_POINT('',#75954);
#13129=VERTEX_POINT('',#75958);
#13130=VERTEX_POINT('',#75964);
#13131=VERTEX_POINT('',#75965);
#13132=VERTEX_POINT('',#75967);
#13133=VERTEX_POINT('',#75969);
#13134=VERTEX_POINT('',#75973);
#13135=VERTEX_POINT('',#75977);
#13136=VERTEX_POINT('',#75983);
#13137=VERTEX_POINT('',#75984);
#13138=VERTEX_POINT('',#75986);
#13139=VERTEX_POINT('',#75988);
#13140=VERTEX_POINT('',#75992);
#13141=VERTEX_POINT('',#75996);
#13142=VERTEX_POINT('',#76002);
#13143=VERTEX_POINT('',#76003);
#13144=VERTEX_POINT('',#76005);
#13145=VERTEX_POINT('',#76007);
#13146=VERTEX_POINT('',#76011);
#13147=VERTEX_POINT('',#76013);
#13148=VERTEX_POINT('',#76017);
#13149=VERTEX_POINT('',#76021);
#13150=VERTEX_POINT('',#76025);
#13151=VERTEX_POINT('',#76026);
#13152=VERTEX_POINT('',#76028);
#13153=VERTEX_POINT('',#76030);
#13154=VERTEX_POINT('',#76034);
#13155=VERTEX_POINT('',#76038);
#13156=VERTEX_POINT('',#76044);
#13157=VERTEX_POINT('',#76045);
#13158=VERTEX_POINT('',#76047);
#13159=VERTEX_POINT('',#76049);
#13160=VERTEX_POINT('',#76053);
#13161=VERTEX_POINT('',#76057);
#13162=VERTEX_POINT('',#76063);
#13163=VERTEX_POINT('',#76064);
#13164=VERTEX_POINT('',#76066);
#13165=VERTEX_POINT('',#76068);
#13166=VERTEX_POINT('',#76072);
#13167=VERTEX_POINT('',#76076);
#13168=VERTEX_POINT('',#76082);
#13169=VERTEX_POINT('',#76083);
#13170=VERTEX_POINT('',#76085);
#13171=VERTEX_POINT('',#76087);
#13172=VERTEX_POINT('',#76091);
#13173=VERTEX_POINT('',#76095);
#13174=VERTEX_POINT('',#76101);
#13175=VERTEX_POINT('',#76102);
#13176=VERTEX_POINT('',#76104);
#13177=VERTEX_POINT('',#76106);
#13178=VERTEX_POINT('',#76110);
#13179=VERTEX_POINT('',#76114);
#13180=VERTEX_POINT('',#76120);
#13181=VERTEX_POINT('',#76121);
#13182=VERTEX_POINT('',#76123);
#13183=VERTEX_POINT('',#76125);
#13184=VERTEX_POINT('',#76129);
#13185=VERTEX_POINT('',#76133);
#13186=VERTEX_POINT('',#76139);
#13187=VERTEX_POINT('',#76140);
#13188=VERTEX_POINT('',#76142);
#13189=VERTEX_POINT('',#76144);
#13190=VERTEX_POINT('',#76148);
#13191=VERTEX_POINT('',#76152);
#13192=VERTEX_POINT('',#76158);
#13193=VERTEX_POINT('',#76159);
#13194=VERTEX_POINT('',#76161);
#13195=VERTEX_POINT('',#76163);
#13196=VERTEX_POINT('',#76167);
#13197=VERTEX_POINT('',#76171);
#13198=VERTEX_POINT('',#76177);
#13199=VERTEX_POINT('',#76178);
#13200=VERTEX_POINT('',#76180);
#13201=VERTEX_POINT('',#76182);
#13202=VERTEX_POINT('',#76186);
#13203=VERTEX_POINT('',#76190);
#13204=VERTEX_POINT('',#76196);
#13205=VERTEX_POINT('',#76197);
#13206=VERTEX_POINT('',#76199);
#13207=VERTEX_POINT('',#76201);
#13208=VERTEX_POINT('',#76205);
#13209=VERTEX_POINT('',#76209);
#13210=VERTEX_POINT('',#76215);
#13211=VERTEX_POINT('',#76216);
#13212=VERTEX_POINT('',#76218);
#13213=VERTEX_POINT('',#76220);
#13214=VERTEX_POINT('',#76224);
#13215=VERTEX_POINT('',#76228);
#13216=VERTEX_POINT('',#76234);
#13217=VERTEX_POINT('',#76235);
#13218=VERTEX_POINT('',#76237);
#13219=VERTEX_POINT('',#76239);
#13220=VERTEX_POINT('',#76243);
#13221=VERTEX_POINT('',#76247);
#13222=VERTEX_POINT('',#76253);
#13223=VERTEX_POINT('',#76254);
#13224=VERTEX_POINT('',#76256);
#13225=VERTEX_POINT('',#76258);
#13226=VERTEX_POINT('',#76262);
#13227=VERTEX_POINT('',#76266);
#13228=VERTEX_POINT('',#76272);
#13229=VERTEX_POINT('',#76273);
#13230=VERTEX_POINT('',#76275);
#13231=VERTEX_POINT('',#76277);
#13232=VERTEX_POINT('',#76281);
#13233=VERTEX_POINT('',#76285);
#13234=VERTEX_POINT('',#76291);
#13235=VERTEX_POINT('',#76292);
#13236=VERTEX_POINT('',#76294);
#13237=VERTEX_POINT('',#76296);
#13238=VERTEX_POINT('',#76300);
#13239=VERTEX_POINT('',#76304);
#13240=VERTEX_POINT('',#76310);
#13241=VERTEX_POINT('',#76311);
#13242=VERTEX_POINT('',#76313);
#13243=VERTEX_POINT('',#76315);
#13244=VERTEX_POINT('',#76319);
#13245=VERTEX_POINT('',#76323);
#13246=VERTEX_POINT('',#76329);
#13247=VERTEX_POINT('',#76330);
#13248=VERTEX_POINT('',#76332);
#13249=VERTEX_POINT('',#76334);
#13250=VERTEX_POINT('',#76338);
#13251=VERTEX_POINT('',#76342);
#13252=VERTEX_POINT('',#76348);
#13253=VERTEX_POINT('',#76349);
#13254=VERTEX_POINT('',#76351);
#13255=VERTEX_POINT('',#76355);
#13256=VERTEX_POINT('',#76357);
#13257=VERTEX_POINT('',#76361);
#13258=VERTEX_POINT('',#76367);
#13259=VERTEX_POINT('',#76368);
#13260=VERTEX_POINT('',#76370);
#13261=VERTEX_POINT('',#76372);
#13262=VERTEX_POINT('',#76376);
#13263=VERTEX_POINT('',#76380);
#13264=VERTEX_POINT('',#76386);
#13265=VERTEX_POINT('',#76387);
#13266=VERTEX_POINT('',#76389);
#13267=VERTEX_POINT('',#76391);
#13268=VERTEX_POINT('',#76395);
#13269=VERTEX_POINT('',#76399);
#13270=VERTEX_POINT('',#76405);
#13271=VERTEX_POINT('',#76406);
#13272=VERTEX_POINT('',#76408);
#13273=VERTEX_POINT('',#76410);
#13274=VERTEX_POINT('',#76414);
#13275=VERTEX_POINT('',#76418);
#13276=VERTEX_POINT('',#76424);
#13277=VERTEX_POINT('',#76425);
#13278=VERTEX_POINT('',#76427);
#13279=VERTEX_POINT('',#76429);
#13280=VERTEX_POINT('',#76433);
#13281=VERTEX_POINT('',#76437);
#13282=VERTEX_POINT('',#76443);
#13283=VERTEX_POINT('',#76444);
#13284=VERTEX_POINT('',#76446);
#13285=VERTEX_POINT('',#76448);
#13286=VERTEX_POINT('',#76452);
#13287=VERTEX_POINT('',#76456);
#13288=VERTEX_POINT('',#76462);
#13289=VERTEX_POINT('',#76463);
#13290=VERTEX_POINT('',#76465);
#13291=VERTEX_POINT('',#76467);
#13292=VERTEX_POINT('',#76471);
#13293=VERTEX_POINT('',#76475);
#13294=VERTEX_POINT('',#76481);
#13295=VERTEX_POINT('',#76482);
#13296=VERTEX_POINT('',#76484);
#13297=VERTEX_POINT('',#76486);
#13298=VERTEX_POINT('',#76490);
#13299=VERTEX_POINT('',#76494);
#13300=VERTEX_POINT('',#76500);
#13301=VERTEX_POINT('',#76501);
#13302=VERTEX_POINT('',#76503);
#13303=VERTEX_POINT('',#76505);
#13304=VERTEX_POINT('',#76509);
#13305=VERTEX_POINT('',#76513);
#13306=VERTEX_POINT('',#76519);
#13307=VERTEX_POINT('',#76520);
#13308=VERTEX_POINT('',#76522);
#13309=VERTEX_POINT('',#76524);
#13310=VERTEX_POINT('',#76528);
#13311=VERTEX_POINT('',#76532);
#13312=VERTEX_POINT('',#76538);
#13313=VERTEX_POINT('',#76543);
#13314=VERTEX_POINT('',#76585);
#13315=EDGE_CURVE('',#10904,#10905,#6592,.T.);
#13316=EDGE_CURVE('',#10905,#10906,#5731,.T.);
#13317=EDGE_CURVE('',#10906,#10907,#6593,.T.);
#13318=EDGE_CURVE('',#10907,#10904,#5732,.T.);
#13319=EDGE_CURVE('',#10908,#10909,#6594,.T.);
#13320=EDGE_CURVE('',#10909,#10905,#6595,.T.);
#13321=EDGE_CURVE('',#10904,#10908,#6596,.T.);
#13322=EDGE_CURVE('',#10910,#10911,#6597,.T.);
#13323=EDGE_CURVE('',#10911,#10909,#5733,.T.);
#13324=EDGE_CURVE('',#10908,#10910,#5734,.T.);
#13325=EDGE_CURVE('',#10912,#10913,#6598,.T.);
#13326=EDGE_CURVE('',#10913,#10911,#6599,.T.);
#13327=EDGE_CURVE('',#10910,#10912,#6600,.T.);
#13328=EDGE_CURVE('',#10914,#10915,#6601,.T.);
#13329=EDGE_CURVE('',#10915,#10913,#5735,.T.);
#13330=EDGE_CURVE('',#10912,#10914,#5736,.T.);
#13331=EDGE_CURVE('',#10916,#10917,#6602,.T.);
#13332=EDGE_CURVE('',#10917,#10915,#6603,.T.);
#13333=EDGE_CURVE('',#10914,#10916,#6604,.T.);
#13334=EDGE_CURVE('',#10918,#10919,#6605,.T.);
#13335=EDGE_CURVE('',#10919,#10917,#5737,.T.);
#13336=EDGE_CURVE('',#10916,#10918,#5738,.T.);
#13337=EDGE_CURVE('',#10906,#10919,#6606,.T.);
#13338=EDGE_CURVE('',#10918,#10907,#6607,.T.);
#13339=EDGE_CURVE('',#10917,#10920,#6608,.T.);
#13340=EDGE_CURVE('',#10921,#10920,#6609,.T.);
#13341=EDGE_CURVE('',#10921,#10915,#6610,.T.);
#13342=EDGE_CURVE('',#10922,#10919,#6611,.T.);
#13343=EDGE_CURVE('',#10920,#10922,#5739,.T.);
#13344=EDGE_CURVE('',#10923,#10906,#6612,.T.);
#13345=EDGE_CURVE('',#10922,#10923,#6613,.T.);
#13346=EDGE_CURVE('',#10924,#10905,#6614,.T.);
#13347=EDGE_CURVE('',#10923,#10924,#5740,.T.);
#13348=EDGE_CURVE('',#10925,#10926,#5741,.T.);
#13349=EDGE_CURVE('',#10927,#10925,#6615,.T.);
#13350=EDGE_CURVE('',#10928,#10927,#5742,.T.);
#13351=EDGE_CURVE('',#10929,#10928,#6616,.T.);
#13352=EDGE_CURVE('',#10930,#10929,#5743,.T.);
#13353=EDGE_CURVE('',#10931,#10930,#6617,.T.);
#13354=EDGE_CURVE('',#10932,#10931,#5744,.T.);
#13355=EDGE_CURVE('',#10926,#10932,#6618,.T.);
#13356=EDGE_CURVE('',#10933,#10933,#5745,.T.);
#13357=EDGE_CURVE('',#10933,#10934,#6619,.T.);
#13358=EDGE_CURVE('',#10934,#10934,#5746,.T.);
#13359=EDGE_CURVE('',#10935,#10936,#5747,.T.);
#13360=EDGE_CURVE('',#10937,#10935,#6620,.T.);
#13361=EDGE_CURVE('',#10938,#10937,#5748,.T.);
#13362=EDGE_CURVE('',#10939,#10938,#6621,.T.);
#13363=EDGE_CURVE('',#10940,#10939,#5749,.T.);
#13364=EDGE_CURVE('',#10941,#10940,#6622,.T.);
#13365=EDGE_CURVE('',#10942,#10941,#5750,.T.);
#13366=EDGE_CURVE('',#10936,#10942,#6623,.T.);
#13367=EDGE_CURVE('',#10943,#10943,#5751,.T.);
#13368=EDGE_CURVE('',#10944,#10944,#5752,.T.);
#13369=EDGE_CURVE('',#10945,#10945,#5753,.T.);
#13370=EDGE_CURVE('',#10946,#10947,#6624,.T.);
#13371=EDGE_CURVE('',#10948,#10946,#6625,.T.);
#13372=EDGE_CURVE('',#10949,#10948,#6626,.T.);
#13373=EDGE_CURVE('',#10947,#10949,#6627,.T.);
#13374=EDGE_CURVE('',#10950,#10950,#5754,.T.);
#13375=EDGE_CURVE('',#10951,#10951,#5755,.T.);
#13376=EDGE_CURVE('',#10951,#10934,#6628,.T.);
#13377=EDGE_CURVE('',#10943,#10952,#6629,.T.);
#13378=EDGE_CURVE('',#10952,#10952,#5756,.T.);
#13379=EDGE_CURVE('',#10953,#10953,#5757,.T.);
#13380=EDGE_CURVE('',#10953,#10952,#6630,.T.);
#13381=EDGE_CURVE('',#10950,#10954,#6631,.T.);
#13382=EDGE_CURVE('',#10954,#10954,#5758,.T.);
#13383=EDGE_CURVE('',#10955,#10955,#5759,.T.);
#13384=EDGE_CURVE('',#10955,#10954,#6632,.T.);
#13385=EDGE_CURVE('',#10944,#10956,#6633,.T.);
#13386=EDGE_CURVE('',#10956,#10956,#5760,.T.);
#13387=EDGE_CURVE('',#10957,#10957,#5761,.T.);
#13388=EDGE_CURVE('',#10957,#10956,#6634,.T.);
#13389=EDGE_CURVE('',#10948,#10958,#6635,.T.);
#13390=EDGE_CURVE('',#10958,#10959,#6636,.T.);
#13391=EDGE_CURVE('',#10949,#10959,#6637,.T.);
#13392=EDGE_CURVE('',#10947,#10960,#6638,.T.);
#13393=EDGE_CURVE('',#10960,#10961,#6639,.T.);
#13394=EDGE_CURVE('',#10961,#10946,#6640,.T.);
#13395=EDGE_CURVE('',#10959,#10960,#6641,.T.);
#13396=EDGE_CURVE('',#10961,#10958,#6642,.T.);
#13397=EDGE_CURVE('',#10961,#10962,#6643,.T.);
#13398=EDGE_CURVE('',#10962,#10963,#6644,.T.);
#13399=EDGE_CURVE('',#10958,#10963,#6645,.T.);
#13400=EDGE_CURVE('',#10960,#10964,#6646,.T.);
#13401=EDGE_CURVE('',#10964,#10962,#6647,.T.);
#13402=EDGE_CURVE('',#10965,#10966,#1089,.T.);
#13403=EDGE_CURVE('',#10966,#10967,#6648,.T.);
#13404=EDGE_CURVE('',#10967,#10921,#6649,.T.);
#13405=EDGE_CURVE('',#10920,#10968,#6650,.T.);
#13406=EDGE_CURVE('',#10968,#10965,#6651,.T.);
#13407=EDGE_CURVE('',#10969,#10970,#6652,.T.);
#13408=EDGE_CURVE('',#10970,#10921,#5762,.T.);
#13409=EDGE_CURVE('',#10967,#10969,#5763,.T.);
#13410=EDGE_CURVE('',#10971,#10972,#6653,.T.);
#13411=EDGE_CURVE('',#10972,#10970,#6654,.T.);
#13412=EDGE_CURVE('',#10969,#10971,#6655,.T.);
#13413=EDGE_CURVE('',#10973,#10974,#6656,.T.);
#13414=EDGE_CURVE('',#10974,#10972,#5764,.T.);
#13415=EDGE_CURVE('',#10971,#10973,#5765,.T.);
#13416=EDGE_CURVE('',#10975,#10976,#1090,.T.);
#13417=EDGE_CURVE('',#10976,#10977,#6657,.T.);
#13418=EDGE_CURVE('',#10977,#10924,#6658,.T.);
#13419=EDGE_CURVE('',#10924,#10974,#6659,.T.);
#13420=EDGE_CURVE('',#10973,#10975,#6660,.T.);
#13421=EDGE_CURVE('',#10978,#10923,#6661,.T.);
#13422=EDGE_CURVE('',#10977,#10978,#5766,.T.);
#13423=EDGE_CURVE('',#10979,#10922,#6662,.T.);
#13424=EDGE_CURVE('',#10978,#10979,#6663,.T.);
#13425=EDGE_CURVE('',#10979,#10968,#5767,.T.);
#13426=EDGE_CURVE('',#10968,#10980,#6664,.T.);
#13427=EDGE_CURVE('',#10981,#10980,#6665,.T.);
#13428=EDGE_CURVE('',#10967,#10981,#6666,.T.);
#13429=EDGE_CURVE('',#10966,#10982,#5768,.T.);
#13430=EDGE_CURVE('',#10982,#10965,#5769,.T.);
#13431=EDGE_CURVE('',#10979,#10983,#6667,.T.);
#13432=EDGE_CURVE('',#10980,#10983,#5770,.T.);
#13433=EDGE_CURVE('',#10978,#10984,#6668,.T.);
#13434=EDGE_CURVE('',#10983,#10984,#6669,.T.);
#13435=EDGE_CURVE('',#10977,#10985,#6670,.T.);
#13436=EDGE_CURVE('',#10984,#10985,#5771,.T.);
#13437=EDGE_CURVE('',#10976,#10986,#5772,.T.);
#13438=EDGE_CURVE('',#10986,#10975,#5773,.T.);
#13439=EDGE_CURVE('',#10973,#10987,#6671,.T.);
#13440=EDGE_CURVE('',#10985,#10987,#6672,.T.);
#13441=EDGE_CURVE('',#10986,#10988,#6673,.T.);
#13442=EDGE_CURVE('',#10989,#10988,#5774,.T.);
#13443=EDGE_CURVE('',#10990,#10989,#1091,.T.);
#13444=EDGE_CURVE('',#10988,#10990,#5775,.T.);
#13445=EDGE_CURVE('',#10991,#10992,#6674,.T.);
#13446=EDGE_CURVE('',#10992,#10993,#6675,.T.);
#13447=EDGE_CURVE('',#10993,#10994,#6676,.T.);
#13448=EDGE_CURVE('',#10994,#10995,#6677,.T.);
#13449=EDGE_CURVE('',#10995,#10991,#6678,.T.);
#13450=EDGE_CURVE('',#10995,#10996,#6679,.T.);
#13451=EDGE_CURVE('',#10996,#10997,#6680,.F.);
#13452=EDGE_CURVE('',#10997,#10991,#6681,.T.);
#13453=EDGE_CURVE('',#10992,#10998,#6682,.T.);
#13454=EDGE_CURVE('',#10998,#10999,#6683,.T.);
#13455=EDGE_CURVE('',#10999,#11000,#6684,.T.);
#13456=EDGE_CURVE('',#10993,#11000,#6685,.T.);
#13457=EDGE_CURVE('',#11001,#10997,#6686,.T.);
#13458=EDGE_CURVE('',#11002,#11001,#6687,.T.);
#13459=EDGE_CURVE('',#11002,#11003,#6688,.T.);
#13460=EDGE_CURVE('',#11004,#11003,#6689,.T.);
#13461=EDGE_CURVE('',#10998,#11004,#6690,.T.);
#13462=EDGE_CURVE('',#11000,#11005,#6691,.T.);
#13463=EDGE_CURVE('',#11005,#11006,#6692,.T.);
#13464=EDGE_CURVE('',#11006,#11007,#6693,.T.);
#13465=EDGE_CURVE('',#11007,#10994,#6694,.T.);
#13466=EDGE_CURVE('',#11008,#11006,#6695,.T.);
#13467=EDGE_CURVE('',#11008,#11009,#6696,.T.);
#13468=EDGE_CURVE('',#11009,#11010,#6697,.T.);
#13469=EDGE_CURVE('',#11010,#11007,#6698,.T.);
#13470=EDGE_CURVE('',#11005,#11011,#6699,.T.);
#13471=EDGE_CURVE('',#11012,#11011,#6700,.T.);
#13472=EDGE_CURVE('',#11012,#11008,#6701,.T.);
#13473=EDGE_CURVE('',#11013,#11000,#6702,.T.);
#13474=EDGE_CURVE('',#11014,#11013,#6703,.T.);
#13475=EDGE_CURVE('',#11005,#11014,#6704,.T.);
#13476=EDGE_CURVE('',#11015,#11014,#6705,.T.);
#13477=EDGE_CURVE('',#11013,#11016,#6706,.T.);
#13478=EDGE_CURVE('',#11016,#11015,#6707,.T.);
#13479=EDGE_CURVE('',#11015,#11017,#6708,.T.);
#13480=EDGE_CURVE('',#11017,#11011,#6709,.T.);
#13481=EDGE_CURVE('',#10926,#11018,#6710,.T.);
#13482=EDGE_CURVE('',#11018,#11019,#5776,.T.);
#13483=EDGE_CURVE('',#11019,#10925,#6711,.T.);
#13484=EDGE_CURVE('',#10932,#11020,#6712,.T.);
#13485=EDGE_CURVE('',#11020,#11018,#6713,.T.);
#13486=EDGE_CURVE('',#10931,#11021,#6714,.T.);
#13487=EDGE_CURVE('',#11021,#11020,#5777,.T.);
#13488=EDGE_CURVE('',#10930,#11022,#6715,.T.);
#13489=EDGE_CURVE('',#11022,#11021,#6716,.T.);
#13490=EDGE_CURVE('',#10929,#11023,#6717,.T.);
#13491=EDGE_CURVE('',#11023,#11022,#5778,.T.);
#13492=EDGE_CURVE('',#10928,#11024,#6718,.T.);
#13493=EDGE_CURVE('',#11024,#11023,#6719,.T.);
#13494=EDGE_CURVE('',#10927,#11025,#6720,.T.);
#13495=EDGE_CURVE('',#11025,#11024,#5779,.T.);
#13496=EDGE_CURVE('',#11019,#11025,#6721,.T.);
#13497=EDGE_CURVE('',#11024,#11026,#6722,.T.);
#13498=EDGE_CURVE('',#11027,#11026,#6723,.T.);
#13499=EDGE_CURVE('',#11027,#11023,#6724,.T.);
#13500=EDGE_CURVE('',#11028,#11025,#6725,.T.);
#13501=EDGE_CURVE('',#11026,#11028,#5780,.T.);
#13502=EDGE_CURVE('',#11029,#11019,#6726,.T.);
#13503=EDGE_CURVE('',#11028,#11029,#6727,.T.);
#13504=EDGE_CURVE('',#11030,#11018,#6728,.T.);
#13505=EDGE_CURVE('',#11029,#11030,#5781,.T.);
#13506=EDGE_CURVE('',#11031,#11027,#6729,.T.);
#13507=EDGE_CURVE('',#11026,#11032,#6730,.T.);
#13508=EDGE_CURVE('',#11032,#11031,#6731,.T.);
#13509=EDGE_CURVE('',#11033,#11034,#6732,.T.);
#13510=EDGE_CURVE('',#11034,#11027,#5782,.T.);
#13511=EDGE_CURVE('',#11031,#11033,#5783,.T.);
#13512=EDGE_CURVE('',#11035,#11036,#1092,.T.);
#13513=EDGE_CURVE('',#11036,#11037,#6733,.T.);
#13514=EDGE_CURVE('',#11037,#11038,#6734,.T.);
#13515=EDGE_CURVE('',#11038,#11034,#6735,.T.);
#13516=EDGE_CURVE('',#11033,#11035,#6736,.T.);
#13517=EDGE_CURVE('',#11004,#11039,#6737,.T.);
#13518=EDGE_CURVE('',#11039,#11038,#5784,.T.);
#13519=EDGE_CURVE('',#11037,#11004,#5785,.T.);
#13520=EDGE_CURVE('',#11003,#11030,#6738,.T.);
#13521=EDGE_CURVE('',#11030,#11039,#6739,.T.);
#13522=EDGE_CURVE('',#11040,#11029,#6740,.T.);
#13523=EDGE_CURVE('',#11003,#11040,#5786,.T.);
#13524=EDGE_CURVE('',#10989,#11041,#6741,.T.);
#13525=EDGE_CURVE('',#11041,#11028,#6742,.T.);
#13526=EDGE_CURVE('',#11040,#10990,#6743,.T.);
#13527=EDGE_CURVE('',#11041,#11032,#5787,.T.);
#13528=EDGE_CURVE('',#11042,#11033,#6744,.T.);
#13529=EDGE_CURVE('',#11043,#11042,#6745,.T.);
#13530=EDGE_CURVE('',#11043,#11037,#6746,.T.);
#13531=EDGE_CURVE('',#11036,#11044,#5788,.T.);
#13532=EDGE_CURVE('',#11044,#11035,#5789,.T.);
#13533=EDGE_CURVE('',#11012,#11031,#6747,.T.);
#13534=EDGE_CURVE('',#11042,#11012,#5790,.T.);
#13535=EDGE_CURVE('',#11045,#11032,#6748,.T.);
#13536=EDGE_CURVE('',#11046,#11045,#6749,.T.);
#13537=EDGE_CURVE('',#11047,#11046,#6750,.T.);
#13538=EDGE_CURVE('',#11009,#11047,#6751,.T.);
#13539=EDGE_CURVE('',#11048,#11041,#6752,.T.);
#13540=EDGE_CURVE('',#11045,#11048,#5791,.T.);
#13541=EDGE_CURVE('',#11049,#11040,#6753,.T.);
#13542=EDGE_CURVE('',#11048,#11049,#6754,.T.);
#13543=EDGE_CURVE('',#11043,#11050,#6755,.T.);
#13544=EDGE_CURVE('',#11050,#10999,#5792,.T.);
#13545=EDGE_CURVE('',#10998,#11043,#5793,.T.);
#13546=EDGE_CURVE('',#11042,#11051,#6756,.T.);
#13547=EDGE_CURVE('',#11051,#11050,#6757,.T.);
#13548=EDGE_CURVE('',#11011,#11051,#5794,.T.);
#13549=EDGE_CURVE('',#11052,#10999,#6758,.T.);
#13550=EDGE_CURVE('',#11052,#11016,#6759,.T.);
#13551=EDGE_CURVE('',#11053,#11050,#6760,.T.);
#13552=EDGE_CURVE('',#11053,#11052,#5795,.T.);
#13553=EDGE_CURVE('',#11054,#11051,#6761,.T.);
#13554=EDGE_CURVE('',#11054,#11053,#6762,.T.);
#13555=EDGE_CURVE('',#11017,#11054,#5796,.T.);
#13556=EDGE_CURVE('',#11055,#11056,#6763,.T.);
#13557=EDGE_CURVE('',#11057,#11055,#6764,.T.);
#13558=EDGE_CURVE('',#11056,#11057,#6765,.T.);
#13559=EDGE_CURVE('',#11058,#11059,#6766,.T.);
#13560=EDGE_CURVE('',#11060,#11058,#6767,.T.);
#13561=EDGE_CURVE('',#11059,#11060,#6768,.T.);
#13562=EDGE_CURVE('',#11061,#11062,#6769,.T.);
#13563=EDGE_CURVE('',#11062,#11057,#6770,.T.);
#13564=EDGE_CURVE('',#11055,#11061,#6771,.T.);
#13565=EDGE_CURVE('',#11063,#11064,#6772,.T.);
#13566=EDGE_CURVE('',#11064,#11062,#5797,.T.);
#13567=EDGE_CURVE('',#11061,#11063,#5798,.T.);
#13568=EDGE_CURVE('',#11065,#11066,#6773,.T.);
#13569=EDGE_CURVE('',#11066,#11064,#6774,.T.);
#13570=EDGE_CURVE('',#11063,#11065,#6775,.T.);
#13571=EDGE_CURVE('',#11067,#11068,#6776,.T.);
#13572=EDGE_CURVE('',#11068,#11066,#5799,.T.);
#13573=EDGE_CURVE('',#11065,#11067,#5800,.T.);
#13574=EDGE_CURVE('',#11067,#11060,#6777,.T.);
#13575=EDGE_CURVE('',#11058,#11068,#6778,.T.);
#13576=EDGE_CURVE('',#11056,#11059,#6779,.T.);
#13577=EDGE_CURVE('',#11060,#11055,#6780,.T.);
#13578=EDGE_CURVE('',#11069,#11070,#6781,.F.);
#13579=EDGE_CURVE('',#11001,#11069,#6782,.F.);
#13580=EDGE_CURVE('',#11071,#11001,#6783,.F.);
#13581=EDGE_CURVE('',#11070,#11071,#6784,.F.);
#13582=EDGE_CURVE('',#11072,#11073,#6785,.F.);
#13583=EDGE_CURVE('',#11046,#11072,#6786,.F.);
#13584=EDGE_CURVE('',#11074,#11046,#6787,.F.);
#13585=EDGE_CURVE('',#11073,#11074,#6788,.F.);
#13586=EDGE_CURVE('',#11072,#11075,#6789,.T.);
#13587=EDGE_CURVE('',#11075,#11047,#6790,.T.);
#13588=EDGE_CURVE('',#11075,#11010,#6791,.T.);
#13589=EDGE_CURVE('',#11045,#11076,#6792,.T.);
#13590=EDGE_CURVE('',#11076,#11074,#6793,.T.);
#13591=EDGE_CURVE('',#11048,#11077,#6794,.T.);
#13592=EDGE_CURVE('',#11077,#11076,#5801,.T.);
#13593=EDGE_CURVE('',#11049,#11078,#6795,.T.);
#13594=EDGE_CURVE('',#11078,#11077,#6796,.T.);
#13595=EDGE_CURVE('',#11002,#11079,#6797,.T.);
#13596=EDGE_CURVE('',#11079,#11078,#5802,.T.);
#13597=EDGE_CURVE('',#11049,#11002,#5803,.T.);
#13598=EDGE_CURVE('',#11069,#11079,#6798,.T.);
#13599=EDGE_CURVE('',#11059,#11073,#6799,.T.);
#13600=EDGE_CURVE('',#11074,#11058,#6800,.T.);
#13601=EDGE_CURVE('',#11073,#11070,#6801,.T.);
#13602=EDGE_CURVE('',#11071,#11072,#6802,.T.);
#13603=EDGE_CURVE('',#10996,#11071,#6803,.T.);
#13604=EDGE_CURVE('',#11057,#11069,#6804,.T.);
#13605=EDGE_CURVE('',#11070,#11056,#6805,.T.);
#13606=EDGE_CURVE('',#11064,#11078,#6806,.T.);
#13607=EDGE_CURVE('',#11062,#11079,#6807,.T.);
#13608=EDGE_CURVE('',#11068,#11076,#6808,.T.);
#13609=EDGE_CURVE('',#11066,#11077,#6809,.T.);
#13610=EDGE_CURVE('',#11010,#10995,#6810,.T.);
#13611=EDGE_CURVE('',#10996,#11075,#6811,.T.);
#13612=EDGE_CURVE('',#11080,#11080,#5804,.T.);
#13613=EDGE_CURVE('',#11081,#10935,#5805,.T.);
#13614=EDGE_CURVE('',#10936,#10987,#5806,.T.);
#13615=EDGE_CURVE('',#10987,#11081,#5807,.T.);
#13616=EDGE_CURVE('',#10942,#10985,#5808,.T.);
#13617=EDGE_CURVE('',#10941,#10984,#5809,.T.);
#13618=EDGE_CURVE('',#10940,#10983,#5810,.T.);
#13619=EDGE_CURVE('',#10939,#10980,#5811,.T.);
#13620=EDGE_CURVE('',#10938,#10981,#5812,.T.);
#13621=EDGE_CURVE('',#10937,#11082,#5813,.T.);
#13622=EDGE_CURVE('',#11082,#10981,#5814,.T.);
#13623=EDGE_CURVE('',#11081,#11082,#6812,.T.);
#13624=EDGE_CURVE('',#10969,#11082,#6813,.T.);
#13625=EDGE_CURVE('',#10971,#11081,#6814,.T.);
#13626=EDGE_CURVE('',#10970,#10913,#6815,.T.);
#13627=EDGE_CURVE('',#10972,#10911,#6816,.T.);
#13628=EDGE_CURVE('',#10974,#10909,#6817,.T.);
#13629=EDGE_CURVE('',#11034,#11022,#6818,.T.);
#13630=EDGE_CURVE('',#11038,#11021,#6819,.T.);
#13631=EDGE_CURVE('',#11039,#11020,#6820,.T.);
#13632=EDGE_CURVE('',#11044,#10982,#6821,.T.);
#13633=EDGE_CURVE('',#11080,#10945,#6822,.T.);
#13634=EDGE_CURVE('',#11083,#10951,#6823,.T.);
#13635=EDGE_CURVE('',#11084,#10953,#6824,.T.);
#13636=EDGE_CURVE('',#11085,#10955,#6825,.T.);
#13637=EDGE_CURVE('',#11086,#10957,#6826,.T.);
#13638=EDGE_CURVE('',#10959,#11087,#6827,.T.);
#13639=EDGE_CURVE('',#11087,#10964,#6828,.T.);
#13640=EDGE_CURVE('',#10963,#11087,#6829,.T.);
#13641=EDGE_CURVE('',#11088,#11088,#5815,.T.);
#13642=EDGE_CURVE('',#11088,#11089,#6830,.T.);
#13643=EDGE_CURVE('',#11089,#11090,#5816,.T.);
#13644=EDGE_CURVE('',#11090,#11089,#5817,.T.);
#13645=EDGE_CURVE('',#11090,#11091,#6831,.T.);
#13646=EDGE_CURVE('',#11092,#11091,#5818,.T.);
#13647=EDGE_CURVE('',#11091,#11092,#5819,.T.);
#13648=EDGE_CURVE('',#11093,#11093,#5820,.T.);
#13649=EDGE_CURVE('',#11092,#11094,#6832,.T.);
#13650=EDGE_CURVE('',#11094,#11095,#5821,.T.);
#13651=EDGE_CURVE('',#11095,#11094,#5822,.T.);
#13652=EDGE_CURVE('',#11095,#11096,#6833,.T.);
#13653=EDGE_CURVE('',#11097,#11096,#174,.T.);
#13654=EDGE_CURVE('',#11096,#11097,#175,.T.);
#13655=EDGE_CURVE('',#11098,#11099,#176,.T.);
#13656=EDGE_CURVE('',#11099,#11100,#5823,.T.);
#13657=EDGE_CURVE('',#11100,#11101,#6834,.T.);
#13658=EDGE_CURVE('',#11101,#11102,#5824,.T.);
#13659=EDGE_CURVE('',#11102,#11101,#5825,.T.);
#13660=EDGE_CURVE('',#11100,#11098,#5826,.T.);
#13661=EDGE_CURVE('',#11103,#11104,#5827,.T.);
#13662=EDGE_CURVE('',#11104,#11103,#5828,.T.);
#13663=EDGE_CURVE('',#11103,#11105,#6835,.T.);
#13664=EDGE_CURVE('',#11105,#11099,#5829,.T.);
#13665=EDGE_CURVE('',#11098,#11106,#5830,.T.);
#13666=EDGE_CURVE('',#11107,#11106,#177,.T.);
#13667=EDGE_CURVE('',#11107,#11108,#5831,.T.);
#13668=EDGE_CURVE('',#11109,#11108,#178,.T.);
#13669=EDGE_CURVE('',#11109,#11110,#5832,.T.);
#13670=EDGE_CURVE('',#11111,#11110,#179,.T.);
#13671=EDGE_CURVE('',#11111,#11105,#5833,.T.);
#13672=EDGE_CURVE('',#11112,#11112,#5834,.T.);
#13673=EDGE_CURVE('',#11112,#11102,#6836,.T.);
#13674=EDGE_CURVE('',#11110,#11113,#5835,.T.);
#13675=EDGE_CURVE('',#11113,#11114,#6837,.T.);
#13676=EDGE_CURVE('',#11114,#11114,#5836,.T.);
#13677=EDGE_CURVE('',#11113,#11111,#5837,.T.);
#13678=EDGE_CURVE('',#11115,#11115,#5838,.T.);
#13679=EDGE_CURVE('',#11115,#11114,#6838,.T.);
#13680=EDGE_CURVE('',#11116,#11117,#6839,.T.);
#13681=EDGE_CURVE('',#11117,#11118,#6840,.T.);
#13682=EDGE_CURVE('',#11118,#11119,#6841,.T.);
#13683=EDGE_CURVE('',#11119,#11120,#6842,.T.);
#13684=EDGE_CURVE('',#11120,#11121,#6843,.T.);
#13685=EDGE_CURVE('',#11121,#11116,#6844,.T.);
#13686=EDGE_CURVE('',#11122,#11117,#6845,.T.);
#13687=EDGE_CURVE('',#11123,#11122,#5839,.T.);
#13688=EDGE_CURVE('',#11124,#11123,#180,.T.);
#13689=EDGE_CURVE('',#11125,#11124,#6846,.T.);
#13690=EDGE_CURVE('',#11126,#11125,#181,.T.);
#13691=EDGE_CURVE('',#11127,#11126,#5840,.T.);
#13692=EDGE_CURVE('',#11118,#11127,#6847,.T.);
#13693=EDGE_CURVE('',#11128,#11129,#6848,.T.);
#13694=EDGE_CURVE('',#11130,#11128,#5841,.T.);
#13695=EDGE_CURVE('',#11131,#11130,#6849,.T.);
#13696=EDGE_CURVE('',#11129,#11131,#5842,.T.);
#13697=EDGE_CURVE('',#11132,#11133,#6850,.T.);
#13698=EDGE_CURVE('',#11134,#11132,#5843,.T.);
#13699=EDGE_CURVE('',#11135,#11134,#6851,.T.);
#13700=EDGE_CURVE('',#11133,#11135,#5844,.T.);
#13701=EDGE_CURVE('',#11136,#11116,#6852,.T.);
#13702=EDGE_CURVE('',#11136,#11137,#6853,.T.);
#13703=EDGE_CURVE('',#11137,#11122,#6854,.T.);
#13704=EDGE_CURVE('',#11121,#11138,#6855,.T.);
#13705=EDGE_CURVE('',#11138,#11139,#6856,.T.);
#13706=EDGE_CURVE('',#11139,#11136,#6857,.T.);
#13707=EDGE_CURVE('',#11140,#11140,#5845,.T.);
#13708=EDGE_CURVE('',#11140,#11141,#6858,.T.);
#13709=EDGE_CURVE('',#11141,#11141,#5846,.T.);
#13710=EDGE_CURVE('',#11140,#11142,#6859,.T.);
#13711=EDGE_CURVE('',#11142,#11142,#5847,.T.);
#13712=EDGE_CURVE('',#11143,#11143,#5848,.T.);
#13713=EDGE_CURVE('',#11144,#11145,#6860,.T.);
#13714=EDGE_CURVE('',#11145,#11146,#182,.T.);
#13715=EDGE_CURVE('',#11146,#11145,#183,.T.);
#13716=EDGE_CURVE('',#11144,#11144,#184,.T.);
#13717=EDGE_CURVE('',#11147,#11148,#5849,.T.);
#13718=EDGE_CURVE('',#11148,#11147,#5850,.T.);
#13719=EDGE_CURVE('',#11148,#11104,#6861,.T.);
#13720=EDGE_CURVE('',#11149,#11150,#6862,.T.);
#13721=EDGE_CURVE('',#11151,#11150,#185,.F.);
#13722=EDGE_CURVE('',#11151,#11152,#186,.T.);
#13723=EDGE_CURVE('',#11153,#11152,#187,.F.);
#13724=EDGE_CURVE('',#11153,#11154,#6863,.T.);
#13725=EDGE_CURVE('',#11155,#11154,#188,.F.);
#13726=EDGE_CURVE('',#11156,#11155,#5851,.T.);
#13727=EDGE_CURVE('',#11149,#11156,#189,.F.);
#13728=EDGE_CURVE('',#11146,#11157,#6864,.T.);
#13729=EDGE_CURVE('',#11157,#11157,#5852,.T.);
#13730=EDGE_CURVE('',#11142,#11147,#6865,.T.);
#13731=EDGE_CURVE('',#11158,#11159,#6866,.T.);
#13732=EDGE_CURVE('',#11159,#11160,#6867,.T.);
#13733=EDGE_CURVE('',#11160,#11161,#6868,.F.);
#13734=EDGE_CURVE('',#11161,#11158,#6869,.T.);
#13735=EDGE_CURVE('',#11159,#11162,#6870,.T.);
#13736=EDGE_CURVE('',#11163,#11162,#6871,.T.);
#13737=EDGE_CURVE('',#11163,#11160,#6872,.T.);
#13738=EDGE_CURVE('',#11158,#11164,#5853,.T.);
#13739=EDGE_CURVE('',#11164,#11165,#6873,.T.);
#13740=EDGE_CURVE('',#11165,#11159,#5854,.T.);
#13741=EDGE_CURVE('',#11166,#11167,#190,.T.);
#13742=EDGE_CURVE('',#11168,#11167,#191,.T.);
#13743=EDGE_CURVE('',#11168,#11169,#192,.T.);
#13744=EDGE_CURVE('',#11169,#11166,#6874,.T.);
#13745=EDGE_CURVE('',#11170,#11171,#193,.T.);
#13746=EDGE_CURVE('',#11172,#11171,#194,.T.);
#13747=EDGE_CURVE('',#11172,#11173,#195,.T.);
#13748=EDGE_CURVE('',#11173,#11170,#6875,.T.);
#13749=EDGE_CURVE('',#11171,#11124,#196,.T.);
#13750=EDGE_CURVE('',#11124,#11174,#6876,.T.);
#13751=EDGE_CURVE('',#11174,#11172,#197,.T.);
#13752=EDGE_CURVE('',#11127,#11175,#6877,.T.);
#13753=EDGE_CURVE('',#11175,#11176,#6878,.T.);
#13754=EDGE_CURVE('',#11176,#11119,#6879,.T.);
#13755=EDGE_CURVE('',#11176,#11177,#6880,.T.);
#13756=EDGE_CURVE('',#11177,#11178,#6881,.T.);
#13757=EDGE_CURVE('',#11178,#11120,#6882,.T.);
#13758=EDGE_CURVE('',#11179,#11180,#6883,.T.);
#13759=EDGE_CURVE('',#11181,#11179,#6884,.T.);
#13760=EDGE_CURVE('',#11180,#11181,#6885,.T.);
#13761=EDGE_CURVE('',#11182,#11181,#6886,.T.);
#13762=EDGE_CURVE('',#11179,#11183,#6887,.T.);
#13763=EDGE_CURVE('',#11183,#11182,#6888,.T.);
#13764=EDGE_CURVE('',#11184,#11185,#6889,.T.);
#13765=EDGE_CURVE('',#11186,#11184,#6890,.T.);
#13766=EDGE_CURVE('',#11185,#11186,#6891,.T.);
#13767=EDGE_CURVE('',#11187,#11188,#6892,.T.);
#13768=EDGE_CURVE('',#11188,#11186,#6893,.T.);
#13769=EDGE_CURVE('',#11184,#11187,#6894,.T.);
#13770=EDGE_CURVE('',#11189,#11190,#6895,.T.);
#13771=EDGE_CURVE('',#11190,#11188,#5855,.T.);
#13772=EDGE_CURVE('',#11187,#11189,#5856,.T.);
#13773=EDGE_CURVE('',#11191,#11192,#6896,.T.);
#13774=EDGE_CURVE('',#11192,#11190,#6897,.T.);
#13775=EDGE_CURVE('',#11189,#11191,#6898,.T.);
#13776=EDGE_CURVE('',#11193,#11194,#6899,.T.);
#13777=EDGE_CURVE('',#11194,#11192,#5857,.T.);
#13778=EDGE_CURVE('',#11191,#11193,#5858,.T.);
#13779=EDGE_CURVE('',#11193,#11180,#6900,.T.);
#13780=EDGE_CURVE('',#11181,#11194,#6901,.T.);
#13781=EDGE_CURVE('',#11195,#11185,#6902,.T.);
#13782=EDGE_CURVE('',#11186,#11196,#6903,.T.);
#13783=EDGE_CURVE('',#11196,#11195,#6904,.T.);
#13784=EDGE_CURVE('',#11180,#11184,#6905,.T.);
#13785=EDGE_CURVE('',#11185,#11179,#6906,.T.);
#13786=EDGE_CURVE('',#11138,#11195,#6907,.T.);
#13787=EDGE_CURVE('',#11196,#11139,#6908,.T.);
#13788=EDGE_CURVE('',#11177,#11182,#6909,.T.);
#13789=EDGE_CURVE('',#11183,#11178,#6910,.T.);
#13790=EDGE_CURVE('',#11137,#11197,#5859,.T.);
#13791=EDGE_CURVE('',#11197,#11123,#6911,.T.);
#13792=EDGE_CURVE('',#11126,#11198,#6912,.T.);
#13793=EDGE_CURVE('',#11198,#11175,#5860,.T.);
#13794=EDGE_CURVE('',#11197,#11174,#198,.T.);
#13795=EDGE_CURVE('',#11167,#11199,#199,.T.);
#13796=EDGE_CURVE('',#11199,#11125,#6913,.T.);
#13797=EDGE_CURVE('',#11125,#11168,#200,.T.);
#13798=EDGE_CURVE('',#11199,#11198,#201,.T.);
#13799=EDGE_CURVE('',#11175,#11200,#6914,.T.);
#13800=EDGE_CURVE('',#11201,#11200,#6915,.T.);
#13801=EDGE_CURVE('',#11194,#11201,#6916,.T.);
#13802=EDGE_CURVE('',#11166,#11202,#6917,.T.);
#13803=EDGE_CURVE('',#11203,#11202,#202,.T.);
#13804=EDGE_CURVE('',#11204,#11203,#203,.T.);
#13805=EDGE_CURVE('',#11205,#11204,#204,.T.);
#13806=EDGE_CURVE('',#11200,#11205,#5861,.T.);
#13807=EDGE_CURVE('',#11170,#11169,#6918,.T.);
#13808=EDGE_CURVE('',#11173,#11206,#6919,.T.);
#13809=EDGE_CURVE('',#11207,#11206,#6920,.T.);
#13810=EDGE_CURVE('',#11208,#11207,#6921,.T.);
#13811=EDGE_CURVE('',#11209,#11208,#6922,.T.);
#13812=EDGE_CURVE('',#11210,#11209,#5862,.T.);
#13813=EDGE_CURVE('',#11211,#11210,#6923,.T.);
#13814=EDGE_CURVE('',#11212,#11211,#6924,.T.);
#13815=EDGE_CURVE('',#11202,#11212,#6925,.T.);
#13816=EDGE_CURVE('',#11213,#11214,#6926,.T.);
#13817=EDGE_CURVE('',#11215,#11213,#5863,.T.);
#13818=EDGE_CURVE('',#11216,#11215,#6927,.T.);
#13819=EDGE_CURVE('',#11214,#11216,#6928,.T.);
#13820=EDGE_CURVE('',#11195,#11183,#6929,.T.);
#13821=EDGE_CURVE('',#11178,#11138,#6930,.T.);
#13822=EDGE_CURVE('',#11217,#11218,#6931,.T.);
#13823=EDGE_CURVE('',#11219,#11217,#5864,.T.);
#13824=EDGE_CURVE('',#11220,#11219,#6932,.T.);
#13825=EDGE_CURVE('',#11218,#11220,#5865,.T.);
#13826=EDGE_CURVE('',#11221,#11222,#6933,.T.);
#13827=EDGE_CURVE('',#11223,#11221,#5866,.T.);
#13828=EDGE_CURVE('',#11224,#11223,#6934,.T.);
#13829=EDGE_CURVE('',#11222,#11224,#5867,.T.);
#13830=EDGE_CURVE('',#11225,#11132,#6935,.T.);
#13831=EDGE_CURVE('',#11133,#11226,#6936,.T.);
#13832=EDGE_CURVE('',#11226,#11225,#6937,.T.);
#13833=EDGE_CURVE('',#11227,#11134,#6938,.T.);
#13834=EDGE_CURVE('',#11225,#11227,#5868,.T.);
#13835=EDGE_CURVE('',#11228,#11135,#6939,.T.);
#13836=EDGE_CURVE('',#11227,#11228,#6940,.T.);
#13837=EDGE_CURVE('',#11228,#11226,#5869,.T.);
#13838=EDGE_CURVE('',#11229,#11225,#6941,.T.);
#13839=EDGE_CURVE('',#11230,#11229,#5870,.T.);
#13840=EDGE_CURVE('',#11230,#11227,#6942,.T.);
#13841=EDGE_CURVE('',#11231,#11226,#6943,.T.);
#13842=EDGE_CURVE('',#11229,#11231,#6944,.T.);
#13843=EDGE_CURVE('',#11232,#11217,#6945,.T.);
#13844=EDGE_CURVE('',#11218,#11233,#6946,.T.);
#13845=EDGE_CURVE('',#11233,#11232,#6947,.T.);
#13846=EDGE_CURVE('',#11234,#11219,#6948,.T.);
#13847=EDGE_CURVE('',#11232,#11234,#5871,.T.);
#13848=EDGE_CURVE('',#11235,#11220,#6949,.T.);
#13849=EDGE_CURVE('',#11234,#11235,#6950,.T.);
#13850=EDGE_CURVE('',#11235,#11233,#5872,.T.);
#13851=EDGE_CURVE('',#11236,#11232,#6951,.T.);
#13852=EDGE_CURVE('',#11237,#11236,#5873,.T.);
#13853=EDGE_CURVE('',#11237,#11234,#6952,.T.);
#13854=EDGE_CURVE('',#11238,#11233,#6953,.T.);
#13855=EDGE_CURVE('',#11236,#11238,#6954,.T.);
#13856=EDGE_CURVE('',#11239,#11221,#6955,.T.);
#13857=EDGE_CURVE('',#11222,#11240,#6956,.T.);
#13858=EDGE_CURVE('',#11240,#11239,#6957,.T.);
#13859=EDGE_CURVE('',#11241,#11223,#6958,.T.);
#13860=EDGE_CURVE('',#11239,#11241,#5874,.T.);
#13861=EDGE_CURVE('',#11242,#11224,#6959,.T.);
#13862=EDGE_CURVE('',#11241,#11242,#6960,.T.);
#13863=EDGE_CURVE('',#11242,#11240,#5875,.T.);
#13864=EDGE_CURVE('',#11243,#11239,#6961,.T.);
#13865=EDGE_CURVE('',#11244,#11243,#5876,.T.);
#13866=EDGE_CURVE('',#11244,#11241,#6962,.T.);
#13867=EDGE_CURVE('',#11245,#11240,#6963,.T.);
#13868=EDGE_CURVE('',#11243,#11245,#6964,.T.);
#13869=EDGE_CURVE('',#11246,#11128,#6965,.T.);
#13870=EDGE_CURVE('',#11129,#11247,#6966,.T.);
#13871=EDGE_CURVE('',#11247,#11246,#6967,.T.);
#13872=EDGE_CURVE('',#11248,#11130,#6968,.T.);
#13873=EDGE_CURVE('',#11246,#11248,#5877,.T.);
#13874=EDGE_CURVE('',#11249,#11131,#6969,.T.);
#13875=EDGE_CURVE('',#11248,#11249,#6970,.T.);
#13876=EDGE_CURVE('',#11249,#11247,#5878,.T.);
#13877=EDGE_CURVE('',#11250,#11246,#6971,.T.);
#13878=EDGE_CURVE('',#11251,#11250,#5879,.T.);
#13879=EDGE_CURVE('',#11251,#11248,#6972,.T.);
#13880=EDGE_CURVE('',#11252,#11247,#6973,.T.);
#13881=EDGE_CURVE('',#11250,#11252,#6974,.T.);
#13882=EDGE_CURVE('',#11106,#11253,#5880,.T.);
#13883=EDGE_CURVE('',#11253,#11254,#6975,.T.);
#13884=EDGE_CURVE('',#11254,#11255,#5881,.T.);
#13885=EDGE_CURVE('',#11255,#11254,#5882,.T.);
#13886=EDGE_CURVE('',#11253,#11107,#5883,.T.);
#13887=EDGE_CURVE('',#11256,#11256,#5884,.T.);
#13888=EDGE_CURVE('',#11256,#11255,#6976,.T.);
#13889=EDGE_CURVE('',#11108,#11257,#5885,.T.);
#13890=EDGE_CURVE('',#11257,#11258,#6977,.T.);
#13891=EDGE_CURVE('',#11258,#11258,#5886,.T.);
#13892=EDGE_CURVE('',#11257,#11109,#5887,.T.);
#13893=EDGE_CURVE('',#11259,#11259,#5888,.T.);
#13894=EDGE_CURVE('',#11259,#11258,#6978,.T.);
#13895=EDGE_CURVE('',#11252,#11260,#6979,.T.);
#13896=EDGE_CURVE('',#11260,#11261,#6980,.T.);
#13897=EDGE_CURVE('',#11261,#11250,#6981,.T.);
#13898=EDGE_CURVE('',#11262,#11263,#6982,.T.);
#13899=EDGE_CURVE('',#11263,#11260,#5889,.T.);
#13900=EDGE_CURVE('',#11252,#11262,#5890,.T.);
#13901=EDGE_CURVE('',#11251,#11264,#6983,.T.);
#13902=EDGE_CURVE('',#11264,#11263,#6984,.T.);
#13903=EDGE_CURVE('',#11262,#11251,#6985,.T.);
#13904=EDGE_CURVE('',#11261,#11264,#5891,.T.);
#13905=EDGE_CURVE('',#11262,#11249,#6986,.T.);
#13906=EDGE_CURVE('',#11265,#11266,#205,.T.);
#13907=EDGE_CURVE('',#11267,#11265,#6987,.T.);
#13908=EDGE_CURVE('',#11268,#11267,#6988,.T.);
#13909=EDGE_CURVE('',#11269,#11268,#6989,.F.);
#13910=EDGE_CURVE('',#11270,#11269,#6990,.T.);
#13911=EDGE_CURVE('',#11271,#11270,#6991,.F.);
#13912=EDGE_CURVE('',#11271,#11272,#6992,.T.);
#13913=EDGE_CURVE('',#11273,#11272,#6993,.T.);
#13914=EDGE_CURVE('',#11161,#11273,#6994,.T.);
#13915=EDGE_CURVE('',#11274,#11163,#6995,.F.);
#13916=EDGE_CURVE('',#11274,#11275,#6996,.T.);
#13917=EDGE_CURVE('',#11276,#11275,#6997,.T.);
#13918=EDGE_CURVE('',#11277,#11276,#206,.T.);
#13919=EDGE_CURVE('',#11278,#11277,#5892,.T.);
#13920=EDGE_CURVE('',#11279,#11278,#6998,.T.);
#13921=EDGE_CURVE('',#11280,#11279,#5893,.T.);
#13922=EDGE_CURVE('',#11281,#11280,#6999,.T.);
#13923=EDGE_CURVE('',#11282,#11281,#5894,.T.);
#13924=EDGE_CURVE('',#11283,#11282,#7000,.T.);
#13925=EDGE_CURVE('',#11266,#11283,#5895,.T.);
#13926=EDGE_CURVE('',#11284,#11285,#7001,.T.);
#13927=EDGE_CURVE('',#11286,#11284,#5896,.T.);
#13928=EDGE_CURVE('',#11287,#11286,#7002,.T.);
#13929=EDGE_CURVE('',#11285,#11287,#5897,.T.);
#13930=EDGE_CURVE('',#11288,#11289,#7003,.T.);
#13931=EDGE_CURVE('',#11290,#11288,#5898,.T.);
#13932=EDGE_CURVE('',#11291,#11290,#7004,.T.);
#13933=EDGE_CURVE('',#11289,#11291,#5899,.T.);
#13934=EDGE_CURVE('',#11292,#11293,#7005,.T.);
#13935=EDGE_CURVE('',#11294,#11292,#5900,.T.);
#13936=EDGE_CURVE('',#11295,#11294,#7006,.T.);
#13937=EDGE_CURVE('',#11293,#11295,#5901,.T.);
#13938=EDGE_CURVE('',#11245,#11284,#7007,.T.);
#13939=EDGE_CURVE('',#11285,#11243,#7008,.T.);
#13940=EDGE_CURVE('',#11296,#11286,#7009,.T.);
#13941=EDGE_CURVE('',#11245,#11296,#5902,.T.);
#13942=EDGE_CURVE('',#11244,#11287,#7010,.T.);
#13943=EDGE_CURVE('',#11296,#11244,#7011,.T.);
#13944=EDGE_CURVE('',#11296,#11242,#7012,.T.);
#13945=EDGE_CURVE('',#11238,#11292,#7013,.T.);
#13946=EDGE_CURVE('',#11293,#11236,#7014,.T.);
#13947=EDGE_CURVE('',#11297,#11294,#7015,.T.);
#13948=EDGE_CURVE('',#11238,#11297,#5903,.T.);
#13949=EDGE_CURVE('',#11237,#11295,#7016,.T.);
#13950=EDGE_CURVE('',#11297,#11237,#7017,.T.);
#13951=EDGE_CURVE('',#11297,#11235,#7018,.T.);
#13952=EDGE_CURVE('',#11231,#11288,#7019,.T.);
#13953=EDGE_CURVE('',#11289,#11229,#7020,.T.);
#13954=EDGE_CURVE('',#11298,#11290,#7021,.T.);
#13955=EDGE_CURVE('',#11231,#11298,#5904,.T.);
#13956=EDGE_CURVE('',#11230,#11291,#7022,.T.);
#13957=EDGE_CURVE('',#11298,#11230,#7023,.T.);
#13958=EDGE_CURVE('',#11298,#11228,#7024,.T.);
#13959=EDGE_CURVE('',#11212,#11299,#207,.T.);
#13960=EDGE_CURVE('',#11203,#11299,#208,.T.);
#13961=EDGE_CURVE('',#11206,#11300,#209,.T.);
#13962=EDGE_CURVE('',#11301,#11300,#210,.T.);
#13963=EDGE_CURVE('',#11301,#11207,#211,.T.);
#13964=EDGE_CURVE('',#11300,#11302,#212,.T.);
#13965=EDGE_CURVE('',#11302,#11276,#7025,.T.);
#13966=EDGE_CURVE('',#11276,#11301,#213,.T.);
#13967=EDGE_CURVE('',#11303,#11278,#7026,.T.);
#13968=EDGE_CURVE('',#11277,#11304,#7027,.T.);
#13969=EDGE_CURVE('',#11304,#11303,#5905,.T.);
#13970=EDGE_CURVE('',#11305,#11279,#7028,.T.);
#13971=EDGE_CURVE('',#11303,#11305,#7029,.T.);
#13972=EDGE_CURVE('',#11306,#11280,#7030,.T.);
#13973=EDGE_CURVE('',#11305,#11306,#5906,.T.);
#13974=EDGE_CURVE('',#11307,#11281,#7031,.T.);
#13975=EDGE_CURVE('',#11306,#11307,#7032,.T.);
#13976=EDGE_CURVE('',#11201,#11282,#7033,.T.);
#13977=EDGE_CURVE('',#11307,#11201,#5907,.T.);
#13978=EDGE_CURVE('',#11200,#11283,#7034,.T.);
#13979=EDGE_CURVE('',#11205,#11266,#7035,.T.);
#13980=EDGE_CURVE('',#11302,#11304,#214,.T.);
#13981=EDGE_CURVE('',#11299,#11265,#215,.T.);
#13982=EDGE_CURVE('',#11265,#11204,#7036,.T.);
#13983=EDGE_CURVE('',#11267,#11211,#1093,.F.);
#13984=EDGE_CURVE('',#11192,#11307,#7037,.T.);
#13985=EDGE_CURVE('',#11190,#11306,#7038,.T.);
#13986=EDGE_CURVE('',#11188,#11305,#7039,.T.);
#13987=EDGE_CURVE('',#11137,#11303,#7040,.T.);
#13988=EDGE_CURVE('',#11308,#11271,#7041,.T.);
#13989=EDGE_CURVE('',#11270,#11309,#7042,.T.);
#13990=EDGE_CURVE('',#11309,#11308,#216,.T.);
#13991=EDGE_CURVE('',#11309,#11310,#5908,.T.);
#13992=EDGE_CURVE('',#11310,#11311,#7043,.T.);
#13993=EDGE_CURVE('',#11311,#11308,#5909,.T.);
#13994=EDGE_CURVE('',#11312,#11313,#7044,.T.);
#13995=EDGE_CURVE('',#11313,#11314,#217,.T.);
#13996=EDGE_CURVE('',#11314,#11315,#7045,.T.);
#13997=EDGE_CURVE('',#11315,#11312,#218,.T.);
#13998=EDGE_CURVE('',#11312,#11311,#219,.T.);
#13999=EDGE_CURVE('',#11310,#11313,#220,.T.);
#14000=EDGE_CURVE('',#11164,#11315,#221,.T.);
#14001=EDGE_CURVE('',#11314,#11165,#222,.T.);
#14002=EDGE_CURVE('',#11312,#11316,#7046,.T.);
#14003=EDGE_CURVE('',#11272,#11316,#7047,.T.);
#14004=EDGE_CURVE('',#11315,#11317,#7048,.T.);
#14005=EDGE_CURVE('',#11316,#11317,#5910,.T.);
#14006=EDGE_CURVE('',#11317,#11273,#7049,.T.);
#14007=EDGE_CURVE('',#11318,#11269,#7050,.T.);
#14008=EDGE_CURVE('',#11268,#11319,#7051,.T.);
#14009=EDGE_CURVE('',#11319,#11320,#223,.T.);
#14010=EDGE_CURVE('',#11320,#11318,#1094,.T.);
#14011=EDGE_CURVE('',#11319,#11153,#224,.T.);
#14012=EDGE_CURVE('',#11152,#11320,#225,.T.);
#14013=EDGE_CURVE('',#11318,#11309,#7052,.T.);
#14014=EDGE_CURVE('',#11321,#11151,#226,.T.);
#14015=EDGE_CURVE('',#11162,#11321,#1095,.T.);
#14016=EDGE_CURVE('',#11322,#11274,#7053,.T.);
#14017=EDGE_CURVE('',#11321,#11322,#227,.T.);
#14018=EDGE_CURVE('',#11150,#11322,#228,.T.);
#14019=EDGE_CURVE('',#11323,#11149,#229,.T.);
#14020=EDGE_CURVE('',#11275,#11323,#7054,.T.);
#14021=EDGE_CURVE('',#11323,#11209,#5911,.T.);
#14022=EDGE_CURVE('',#11208,#11275,#1096,.F.);
#14023=EDGE_CURVE('',#11156,#11209,#230,.T.);
#14024=EDGE_CURVE('',#11324,#11210,#5912,.T.);
#14025=EDGE_CURVE('',#11210,#11155,#231,.T.);
#14026=EDGE_CURVE('',#11154,#11324,#232,.T.);
#14027=EDGE_CURVE('',#11324,#11267,#7055,.T.);
#14028=EDGE_CURVE('',#11316,#11213,#5913,.T.);
#14029=EDGE_CURVE('',#11214,#11272,#1097,.T.);
#14030=EDGE_CURVE('',#11216,#11273,#1098,.T.);
#14031=EDGE_CURVE('',#11317,#11215,#5914,.T.);
#14032=EDGE_CURVE('',#11325,#11115,#7056,.T.);
#14033=EDGE_CURVE('',#11326,#11259,#7057,.T.);
#14034=EDGE_CURVE('',#11327,#11256,#7058,.T.);
#14035=EDGE_CURVE('',#11328,#11112,#7059,.T.);
#14036=EDGE_CURVE('',#11329,#11329,#5915,.T.);
#14037=EDGE_CURVE('',#11329,#11330,#7060,.T.);
#14038=EDGE_CURVE('',#11331,#11330,#233,.T.);
#14039=EDGE_CURVE('',#11330,#11331,#234,.T.);
#14040=EDGE_CURVE('',#11332,#11333,#235,.T.);
#14041=EDGE_CURVE('',#11333,#11332,#236,.T.);
#14042=EDGE_CURVE('',#11333,#11334,#7061,.T.);
#14043=EDGE_CURVE('',#11334,#11334,#5916,.T.);
#14044=EDGE_CURVE('',#11335,#11335,#5917,.T.);
#14045=EDGE_CURVE('',#11335,#11093,#7062,.T.);
#14046=EDGE_CURVE('',#11336,#11336,#5918,.T.);
#14047=EDGE_CURVE('',#11336,#11143,#7063,.T.);
#14048=EDGE_CURVE('',#11337,#11337,#5919,.T.);
#14049=EDGE_CURVE('',#11337,#11338,#7064,.T.);
#14050=EDGE_CURVE('',#11338,#11339,#5920,.T.);
#14051=EDGE_CURVE('',#11339,#11338,#5921,.T.);
#14052=EDGE_CURVE('',#11339,#11340,#7065,.T.);
#14053=EDGE_CURVE('',#11340,#11340,#5922,.T.);
#14054=EDGE_CURVE('',#11341,#11341,#5923,.T.);
#14055=EDGE_CURVE('',#11342,#11343,#7066,.T.);
#14056=EDGE_CURVE('',#11342,#11344,#7067,.T.);
#14057=EDGE_CURVE('',#11344,#11345,#7068,.T.);
#14058=EDGE_CURVE('',#11343,#11345,#7069,.T.);
#14059=EDGE_CURVE('',#11343,#11346,#5924,.T.);
#14060=EDGE_CURVE('',#11345,#11347,#7070,.T.);
#14061=EDGE_CURVE('',#11346,#11347,#7071,.T.);
#14062=EDGE_CURVE('',#11346,#11348,#7072,.T.);
#14063=EDGE_CURVE('',#11347,#11349,#7073,.T.);
#14064=EDGE_CURVE('',#11348,#11349,#7074,.T.);
#14065=EDGE_CURVE('',#11348,#11342,#5925,.T.);
#14066=EDGE_CURVE('',#11349,#11344,#7075,.T.);
#14067=EDGE_CURVE('',#11350,#11351,#7076,.T.);
#14068=EDGE_CURVE('',#11350,#11352,#7077,.T.);
#14069=EDGE_CURVE('',#11352,#11353,#7078,.T.);
#14070=EDGE_CURVE('',#11351,#11353,#7079,.T.);
#14071=EDGE_CURVE('',#11351,#11354,#5926,.T.);
#14072=EDGE_CURVE('',#11353,#11355,#7080,.T.);
#14073=EDGE_CURVE('',#11354,#11355,#7081,.T.);
#14074=EDGE_CURVE('',#11354,#11356,#7082,.T.);
#14075=EDGE_CURVE('',#11355,#11357,#7083,.T.);
#14076=EDGE_CURVE('',#11356,#11357,#7084,.T.);
#14077=EDGE_CURVE('',#11356,#11350,#5927,.T.);
#14078=EDGE_CURVE('',#11357,#11352,#7085,.T.);
#14079=EDGE_CURVE('',#11358,#11359,#7086,.T.);
#14080=EDGE_CURVE('',#11358,#11360,#7087,.T.);
#14081=EDGE_CURVE('',#11360,#11361,#7088,.T.);
#14082=EDGE_CURVE('',#11359,#11361,#7089,.T.);
#14083=EDGE_CURVE('',#11359,#11362,#5928,.T.);
#14084=EDGE_CURVE('',#11361,#11363,#7090,.T.);
#14085=EDGE_CURVE('',#11362,#11363,#7091,.T.);
#14086=EDGE_CURVE('',#11362,#11364,#7092,.T.);
#14087=EDGE_CURVE('',#11363,#11365,#7093,.T.);
#14088=EDGE_CURVE('',#11364,#11365,#7094,.T.);
#14089=EDGE_CURVE('',#11364,#11358,#5929,.T.);
#14090=EDGE_CURVE('',#11365,#11360,#7095,.T.);
#14091=EDGE_CURVE('',#11366,#11367,#7096,.T.);
#14092=EDGE_CURVE('',#11366,#11368,#7097,.T.);
#14093=EDGE_CURVE('',#11368,#11369,#7098,.T.);
#14094=EDGE_CURVE('',#11367,#11369,#7099,.T.);
#14095=EDGE_CURVE('',#11367,#11370,#5930,.T.);
#14096=EDGE_CURVE('',#11369,#11371,#7100,.T.);
#14097=EDGE_CURVE('',#11370,#11371,#7101,.T.);
#14098=EDGE_CURVE('',#11370,#11372,#7102,.T.);
#14099=EDGE_CURVE('',#11371,#11373,#7103,.T.);
#14100=EDGE_CURVE('',#11372,#11373,#7104,.T.);
#14101=EDGE_CURVE('',#11372,#11366,#5931,.T.);
#14102=EDGE_CURVE('',#11373,#11368,#7105,.T.);
#14103=EDGE_CURVE('',#11374,#11375,#7106,.T.);
#14104=EDGE_CURVE('',#11374,#11376,#7107,.T.);
#14105=EDGE_CURVE('',#11376,#11377,#7108,.T.);
#14106=EDGE_CURVE('',#11375,#11377,#7109,.T.);
#14107=EDGE_CURVE('',#11375,#11378,#5932,.T.);
#14108=EDGE_CURVE('',#11377,#11379,#7110,.T.);
#14109=EDGE_CURVE('',#11378,#11379,#7111,.T.);
#14110=EDGE_CURVE('',#11378,#11380,#7112,.T.);
#14111=EDGE_CURVE('',#11379,#11381,#7113,.T.);
#14112=EDGE_CURVE('',#11380,#11381,#7114,.T.);
#14113=EDGE_CURVE('',#11380,#11374,#5933,.T.);
#14114=EDGE_CURVE('',#11381,#11376,#7115,.T.);
#14115=EDGE_CURVE('',#11382,#11383,#7116,.T.);
#14116=EDGE_CURVE('',#11382,#11384,#7117,.T.);
#14117=EDGE_CURVE('',#11384,#11385,#7118,.T.);
#14118=EDGE_CURVE('',#11383,#11385,#7119,.T.);
#14119=EDGE_CURVE('',#11383,#11386,#5934,.T.);
#14120=EDGE_CURVE('',#11385,#11387,#7120,.T.);
#14121=EDGE_CURVE('',#11386,#11387,#7121,.T.);
#14122=EDGE_CURVE('',#11386,#11388,#7122,.T.);
#14123=EDGE_CURVE('',#11387,#11389,#7123,.T.);
#14124=EDGE_CURVE('',#11388,#11389,#7124,.T.);
#14125=EDGE_CURVE('',#11388,#11382,#5935,.T.);
#14126=EDGE_CURVE('',#11389,#11384,#7125,.T.);
#14127=EDGE_CURVE('',#11390,#11391,#7126,.T.);
#14128=EDGE_CURVE('',#11390,#11392,#7127,.T.);
#14129=EDGE_CURVE('',#11392,#11393,#7128,.T.);
#14130=EDGE_CURVE('',#11391,#11393,#7129,.T.);
#14131=EDGE_CURVE('',#11391,#11394,#5936,.T.);
#14132=EDGE_CURVE('',#11393,#11395,#7130,.T.);
#14133=EDGE_CURVE('',#11394,#11395,#7131,.T.);
#14134=EDGE_CURVE('',#11394,#11396,#7132,.T.);
#14135=EDGE_CURVE('',#11395,#11397,#7133,.T.);
#14136=EDGE_CURVE('',#11396,#11397,#7134,.T.);
#14137=EDGE_CURVE('',#11396,#11390,#5937,.T.);
#14138=EDGE_CURVE('',#11397,#11392,#7135,.T.);
#14139=EDGE_CURVE('',#11398,#11399,#7136,.T.);
#14140=EDGE_CURVE('',#11398,#11400,#7137,.T.);
#14141=EDGE_CURVE('',#11400,#11401,#7138,.T.);
#14142=EDGE_CURVE('',#11399,#11401,#7139,.T.);
#14143=EDGE_CURVE('',#11399,#11402,#5938,.T.);
#14144=EDGE_CURVE('',#11401,#11403,#7140,.T.);
#14145=EDGE_CURVE('',#11402,#11403,#7141,.T.);
#14146=EDGE_CURVE('',#11402,#11404,#7142,.T.);
#14147=EDGE_CURVE('',#11403,#11405,#7143,.T.);
#14148=EDGE_CURVE('',#11404,#11405,#7144,.T.);
#14149=EDGE_CURVE('',#11404,#11398,#5939,.T.);
#14150=EDGE_CURVE('',#11405,#11400,#7145,.T.);
#14151=EDGE_CURVE('',#11406,#11407,#7146,.T.);
#14152=EDGE_CURVE('',#11406,#11408,#7147,.T.);
#14153=EDGE_CURVE('',#11408,#11409,#7148,.T.);
#14154=EDGE_CURVE('',#11407,#11409,#7149,.T.);
#14155=EDGE_CURVE('',#11407,#11410,#5940,.T.);
#14156=EDGE_CURVE('',#11409,#11411,#7150,.T.);
#14157=EDGE_CURVE('',#11410,#11411,#7151,.T.);
#14158=EDGE_CURVE('',#11410,#11412,#7152,.T.);
#14159=EDGE_CURVE('',#11411,#11413,#7153,.T.);
#14160=EDGE_CURVE('',#11412,#11413,#7154,.T.);
#14161=EDGE_CURVE('',#11412,#11406,#5941,.T.);
#14162=EDGE_CURVE('',#11413,#11408,#7155,.T.);
#14163=EDGE_CURVE('',#11414,#11415,#7156,.T.);
#14164=EDGE_CURVE('',#11414,#11416,#7157,.T.);
#14165=EDGE_CURVE('',#11416,#11417,#7158,.T.);
#14166=EDGE_CURVE('',#11415,#11417,#7159,.T.);
#14167=EDGE_CURVE('',#11415,#11418,#5942,.T.);
#14168=EDGE_CURVE('',#11417,#11419,#7160,.T.);
#14169=EDGE_CURVE('',#11418,#11419,#7161,.T.);
#14170=EDGE_CURVE('',#11418,#11420,#7162,.T.);
#14171=EDGE_CURVE('',#11419,#11421,#7163,.T.);
#14172=EDGE_CURVE('',#11420,#11421,#7164,.T.);
#14173=EDGE_CURVE('',#11420,#11414,#5943,.T.);
#14174=EDGE_CURVE('',#11421,#11416,#7165,.T.);
#14175=EDGE_CURVE('',#11422,#11423,#7166,.T.);
#14176=EDGE_CURVE('',#11422,#11424,#7167,.T.);
#14177=EDGE_CURVE('',#11424,#11425,#7168,.T.);
#14178=EDGE_CURVE('',#11423,#11425,#7169,.T.);
#14179=EDGE_CURVE('',#11423,#11426,#5944,.T.);
#14180=EDGE_CURVE('',#11425,#11427,#7170,.T.);
#14181=EDGE_CURVE('',#11426,#11427,#7171,.T.);
#14182=EDGE_CURVE('',#11426,#11428,#7172,.T.);
#14183=EDGE_CURVE('',#11427,#11429,#7173,.T.);
#14184=EDGE_CURVE('',#11428,#11429,#7174,.T.);
#14185=EDGE_CURVE('',#11428,#11422,#5945,.T.);
#14186=EDGE_CURVE('',#11429,#11424,#7175,.T.);
#14187=EDGE_CURVE('',#11430,#11431,#7176,.T.);
#14188=EDGE_CURVE('',#11430,#11432,#7177,.T.);
#14189=EDGE_CURVE('',#11432,#11433,#7178,.T.);
#14190=EDGE_CURVE('',#11431,#11433,#7179,.T.);
#14191=EDGE_CURVE('',#11431,#11434,#5946,.T.);
#14192=EDGE_CURVE('',#11433,#11435,#7180,.T.);
#14193=EDGE_CURVE('',#11434,#11435,#7181,.T.);
#14194=EDGE_CURVE('',#11434,#11436,#7182,.T.);
#14195=EDGE_CURVE('',#11435,#11437,#7183,.T.);
#14196=EDGE_CURVE('',#11436,#11437,#7184,.T.);
#14197=EDGE_CURVE('',#11436,#11430,#5947,.T.);
#14198=EDGE_CURVE('',#11437,#11432,#7185,.T.);
#14199=EDGE_CURVE('',#11438,#11439,#7186,.T.);
#14200=EDGE_CURVE('',#11438,#11440,#7187,.T.);
#14201=EDGE_CURVE('',#11440,#11441,#7188,.T.);
#14202=EDGE_CURVE('',#11439,#11441,#7189,.T.);
#14203=EDGE_CURVE('',#11439,#11442,#5948,.T.);
#14204=EDGE_CURVE('',#11441,#11443,#7190,.T.);
#14205=EDGE_CURVE('',#11442,#11443,#7191,.T.);
#14206=EDGE_CURVE('',#11442,#11444,#7192,.T.);
#14207=EDGE_CURVE('',#11443,#11445,#7193,.T.);
#14208=EDGE_CURVE('',#11444,#11445,#7194,.T.);
#14209=EDGE_CURVE('',#11444,#11438,#5949,.T.);
#14210=EDGE_CURVE('',#11445,#11440,#7195,.T.);
#14211=EDGE_CURVE('',#11446,#11447,#7196,.T.);
#14212=EDGE_CURVE('',#11446,#11448,#7197,.T.);
#14213=EDGE_CURVE('',#11448,#11449,#7198,.T.);
#14214=EDGE_CURVE('',#11447,#11449,#7199,.T.);
#14215=EDGE_CURVE('',#11447,#11450,#5950,.T.);
#14216=EDGE_CURVE('',#11449,#11451,#7200,.T.);
#14217=EDGE_CURVE('',#11450,#11451,#7201,.T.);
#14218=EDGE_CURVE('',#11450,#11452,#7202,.T.);
#14219=EDGE_CURVE('',#11451,#11453,#7203,.T.);
#14220=EDGE_CURVE('',#11452,#11453,#7204,.T.);
#14221=EDGE_CURVE('',#11452,#11446,#5951,.T.);
#14222=EDGE_CURVE('',#11453,#11448,#7205,.T.);
#14223=EDGE_CURVE('',#11454,#11455,#7206,.T.);
#14224=EDGE_CURVE('',#11454,#11456,#7207,.T.);
#14225=EDGE_CURVE('',#11456,#11457,#7208,.T.);
#14226=EDGE_CURVE('',#11455,#11457,#7209,.T.);
#14227=EDGE_CURVE('',#11455,#11458,#5952,.T.);
#14228=EDGE_CURVE('',#11457,#11459,#7210,.T.);
#14229=EDGE_CURVE('',#11458,#11459,#7211,.T.);
#14230=EDGE_CURVE('',#11458,#11460,#7212,.T.);
#14231=EDGE_CURVE('',#11459,#11461,#7213,.T.);
#14232=EDGE_CURVE('',#11460,#11461,#7214,.T.);
#14233=EDGE_CURVE('',#11460,#11454,#5953,.T.);
#14234=EDGE_CURVE('',#11461,#11456,#7215,.T.);
#14235=EDGE_CURVE('',#11462,#11463,#7216,.T.);
#14236=EDGE_CURVE('',#11462,#11464,#7217,.T.);
#14237=EDGE_CURVE('',#11464,#11465,#7218,.T.);
#14238=EDGE_CURVE('',#11463,#11465,#7219,.T.);
#14239=EDGE_CURVE('',#11463,#11466,#5954,.T.);
#14240=EDGE_CURVE('',#11465,#11467,#7220,.T.);
#14241=EDGE_CURVE('',#11466,#11467,#7221,.T.);
#14242=EDGE_CURVE('',#11466,#11468,#7222,.T.);
#14243=EDGE_CURVE('',#11467,#11469,#7223,.T.);
#14244=EDGE_CURVE('',#11468,#11469,#7224,.T.);
#14245=EDGE_CURVE('',#11468,#11462,#5955,.T.);
#14246=EDGE_CURVE('',#11469,#11464,#7225,.T.);
#14247=EDGE_CURVE('',#11470,#11471,#7226,.T.);
#14248=EDGE_CURVE('',#11470,#11472,#7227,.T.);
#14249=EDGE_CURVE('',#11472,#11473,#7228,.T.);
#14250=EDGE_CURVE('',#11471,#11473,#7229,.T.);
#14251=EDGE_CURVE('',#11471,#11474,#5956,.T.);
#14252=EDGE_CURVE('',#11473,#11475,#7230,.T.);
#14253=EDGE_CURVE('',#11474,#11475,#7231,.T.);
#14254=EDGE_CURVE('',#11474,#11476,#7232,.T.);
#14255=EDGE_CURVE('',#11475,#11477,#7233,.T.);
#14256=EDGE_CURVE('',#11476,#11477,#7234,.T.);
#14257=EDGE_CURVE('',#11476,#11470,#5957,.T.);
#14258=EDGE_CURVE('',#11477,#11472,#7235,.T.);
#14259=EDGE_CURVE('',#11478,#11479,#7236,.T.);
#14260=EDGE_CURVE('',#11478,#11480,#7237,.T.);
#14261=EDGE_CURVE('',#11480,#11481,#7238,.T.);
#14262=EDGE_CURVE('',#11479,#11481,#7239,.T.);
#14263=EDGE_CURVE('',#11479,#11482,#5958,.T.);
#14264=EDGE_CURVE('',#11481,#11483,#7240,.T.);
#14265=EDGE_CURVE('',#11482,#11483,#7241,.T.);
#14266=EDGE_CURVE('',#11482,#11484,#7242,.T.);
#14267=EDGE_CURVE('',#11483,#11485,#7243,.T.);
#14268=EDGE_CURVE('',#11484,#11485,#7244,.T.);
#14269=EDGE_CURVE('',#11484,#11478,#5959,.T.);
#14270=EDGE_CURVE('',#11485,#11480,#7245,.T.);
#14271=EDGE_CURVE('',#11486,#11487,#7246,.T.);
#14272=EDGE_CURVE('',#11486,#11488,#7247,.T.);
#14273=EDGE_CURVE('',#11488,#11489,#7248,.T.);
#14274=EDGE_CURVE('',#11487,#11489,#7249,.T.);
#14275=EDGE_CURVE('',#11487,#11490,#5960,.T.);
#14276=EDGE_CURVE('',#11489,#11491,#7250,.T.);
#14277=EDGE_CURVE('',#11490,#11491,#7251,.T.);
#14278=EDGE_CURVE('',#11490,#11492,#7252,.T.);
#14279=EDGE_CURVE('',#11491,#11493,#7253,.T.);
#14280=EDGE_CURVE('',#11492,#11493,#7254,.T.);
#14281=EDGE_CURVE('',#11492,#11486,#5961,.T.);
#14282=EDGE_CURVE('',#11493,#11488,#7255,.T.);
#14283=EDGE_CURVE('',#11494,#11495,#7256,.T.);
#14284=EDGE_CURVE('',#11494,#11496,#7257,.T.);
#14285=EDGE_CURVE('',#11496,#11497,#7258,.T.);
#14286=EDGE_CURVE('',#11495,#11497,#7259,.T.);
#14287=EDGE_CURVE('',#11495,#11498,#5962,.T.);
#14288=EDGE_CURVE('',#11497,#11499,#7260,.T.);
#14289=EDGE_CURVE('',#11498,#11499,#7261,.T.);
#14290=EDGE_CURVE('',#11498,#11500,#7262,.T.);
#14291=EDGE_CURVE('',#11499,#11501,#7263,.T.);
#14292=EDGE_CURVE('',#11500,#11501,#7264,.T.);
#14293=EDGE_CURVE('',#11500,#11494,#5963,.T.);
#14294=EDGE_CURVE('',#11501,#11496,#7265,.T.);
#14295=EDGE_CURVE('',#11502,#11503,#7266,.T.);
#14296=EDGE_CURVE('',#11502,#11504,#7267,.T.);
#14297=EDGE_CURVE('',#11504,#11505,#7268,.T.);
#14298=EDGE_CURVE('',#11503,#11505,#7269,.T.);
#14299=EDGE_CURVE('',#11503,#11506,#5964,.T.);
#14300=EDGE_CURVE('',#11505,#11507,#7270,.T.);
#14301=EDGE_CURVE('',#11506,#11507,#7271,.T.);
#14302=EDGE_CURVE('',#11506,#11508,#7272,.T.);
#14303=EDGE_CURVE('',#11507,#11509,#7273,.T.);
#14304=EDGE_CURVE('',#11508,#11509,#7274,.T.);
#14305=EDGE_CURVE('',#11508,#11502,#5965,.T.);
#14306=EDGE_CURVE('',#11509,#11504,#7275,.T.);
#14307=EDGE_CURVE('',#11510,#11511,#7276,.T.);
#14308=EDGE_CURVE('',#11512,#11510,#7277,.T.);
#14309=EDGE_CURVE('',#11512,#11513,#7278,.T.);
#14310=EDGE_CURVE('',#11513,#11511,#7279,.T.);
#14311=EDGE_CURVE('',#11511,#11514,#237,.T.);
#14312=EDGE_CURVE('',#11513,#11515,#5966,.T.);
#14313=EDGE_CURVE('',#11515,#11514,#7280,.T.);
#14314=EDGE_CURVE('',#11514,#11516,#7281,.T.);
#14315=EDGE_CURVE('',#11515,#11517,#7282,.T.);
#14316=EDGE_CURVE('',#11517,#11516,#7283,.T.);
#14317=EDGE_CURVE('',#11516,#11510,#238,.T.);
#14318=EDGE_CURVE('',#11517,#11512,#5967,.T.);
#14319=EDGE_CURVE('',#11518,#11518,#5968,.T.);
#14320=EDGE_CURVE('',#11518,#11519,#7284,.T.);
#14321=EDGE_CURVE('',#11519,#11519,#5969,.T.);
#14322=EDGE_CURVE('',#11520,#11520,#5970,.T.);
#14323=EDGE_CURVE('',#11521,#11521,#5971,.T.);
#14324=EDGE_CURVE('',#11521,#11520,#7285,.T.);
#14325=EDGE_CURVE('',#11340,#11521,#7286,.T.);
#14326=EDGE_CURVE('',#11341,#11522,#7287,.T.);
#14327=EDGE_CURVE('',#11522,#11522,#5972,.T.);
#14328=EDGE_CURVE('',#11522,#11523,#7288,.T.);
#14329=EDGE_CURVE('',#11523,#11523,#5973,.T.);
#14330=EDGE_CURVE('',#11524,#11524,#5974,.T.);
#14331=EDGE_CURVE('',#11524,#11525,#7289,.T.);
#14332=EDGE_CURVE('',#11525,#11525,#5975,.T.);
#14333=EDGE_CURVE('',#11526,#11527,#5976,.T.);
#14334=EDGE_CURVE('',#11527,#11526,#5977,.T.);
#14335=EDGE_CURVE('',#11526,#11528,#7290,.T.);
#14336=EDGE_CURVE('',#11528,#11529,#5978,.T.);
#14337=EDGE_CURVE('',#11529,#11528,#5979,.T.);
#14338=EDGE_CURVE('',#11529,#11530,#7291,.T.);
#14339=EDGE_CURVE('',#11530,#11530,#5980,.T.);
#14340=EDGE_CURVE('',#11531,#11527,#7292,.T.);
#14341=EDGE_CURVE('',#11532,#11532,#5981,.T.);
#14342=EDGE_CURVE('',#11533,#11533,#5982,.T.);
#14343=EDGE_CURVE('',#11533,#11532,#7293,.T.);
#14344=EDGE_CURVE('',#11530,#11533,#7294,.T.);
#14345=EDGE_CURVE('',#11534,#11535,#7295,.T.);
#14346=EDGE_CURVE('',#11534,#11536,#239,.T.);
#14347=EDGE_CURVE('',#11536,#11537,#5983,.F.);
#14348=EDGE_CURVE('',#11537,#11535,#240,.T.);
#14349=EDGE_CURVE('',#11538,#11539,#7296,.T.);
#14350=EDGE_CURVE('',#11538,#11534,#241,.T.);
#14351=EDGE_CURVE('',#11535,#11539,#242,.T.);
#14352=EDGE_CURVE('',#11540,#11541,#7297,.T.);
#14353=EDGE_CURVE('',#11540,#11538,#243,.T.);
#14354=EDGE_CURVE('',#11539,#11541,#244,.T.);
#14355=EDGE_CURVE('',#11542,#11543,#7298,.T.);
#14356=EDGE_CURVE('',#11542,#11540,#245,.T.);
#14357=EDGE_CURVE('',#11541,#11543,#246,.T.);
#14358=EDGE_CURVE('',#11544,#11545,#7299,.T.);
#14359=EDGE_CURVE('',#11544,#11542,#247,.T.);
#14360=EDGE_CURVE('',#11543,#11545,#248,.T.);
#14361=EDGE_CURVE('',#11546,#11547,#7300,.T.);
#14362=EDGE_CURVE('',#11546,#11544,#249,.T.);
#14363=EDGE_CURVE('',#11545,#11547,#250,.T.);
#14364=EDGE_CURVE('',#11548,#11549,#7301,.T.);
#14365=EDGE_CURVE('',#11548,#11546,#251,.T.);
#14366=EDGE_CURVE('',#11547,#11549,#252,.T.);
#14367=EDGE_CURVE('',#11550,#11551,#7302,.T.);
#14368=EDGE_CURVE('',#11550,#11548,#253,.T.);
#14369=EDGE_CURVE('',#11549,#11551,#254,.T.);
#14370=EDGE_CURVE('',#11552,#11553,#7303,.T.);
#14371=EDGE_CURVE('',#11552,#11550,#255,.T.);
#14372=EDGE_CURVE('',#11551,#11553,#256,.T.);
#14373=EDGE_CURVE('',#11554,#11555,#7304,.T.);
#14374=EDGE_CURVE('',#11554,#11552,#257,.T.);
#14375=EDGE_CURVE('',#11553,#11555,#258,.T.);
#14376=EDGE_CURVE('',#11556,#11557,#7305,.T.);
#14377=EDGE_CURVE('',#11556,#11554,#259,.T.);
#14378=EDGE_CURVE('',#11555,#11557,#260,.T.);
#14379=EDGE_CURVE('',#11558,#11559,#7306,.T.);
#14380=EDGE_CURVE('',#11558,#11556,#261,.T.);
#14381=EDGE_CURVE('',#11557,#11559,#262,.T.);
#14382=EDGE_CURVE('',#11560,#11561,#7307,.T.);
#14383=EDGE_CURVE('',#11560,#11558,#263,.T.);
#14384=EDGE_CURVE('',#11559,#11561,#264,.T.);
#14385=EDGE_CURVE('',#11562,#11563,#7308,.T.);
#14386=EDGE_CURVE('',#11562,#11560,#265,.T.);
#14387=EDGE_CURVE('',#11561,#11563,#266,.T.);
#14388=EDGE_CURVE('',#11564,#11565,#7309,.T.);
#14389=EDGE_CURVE('',#11564,#11562,#267,.T.);
#14390=EDGE_CURVE('',#11563,#11565,#268,.T.);
#14391=EDGE_CURVE('',#11566,#11567,#7310,.T.);
#14392=EDGE_CURVE('',#11566,#11564,#269,.T.);
#14393=EDGE_CURVE('',#11565,#11567,#270,.T.);
#14394=EDGE_CURVE('',#11568,#11569,#7311,.T.);
#14395=EDGE_CURVE('',#11568,#11566,#271,.T.);
#14396=EDGE_CURVE('',#11567,#11569,#272,.T.);
#14397=EDGE_CURVE('',#11570,#11571,#7312,.T.);
#14398=EDGE_CURVE('',#11570,#11568,#273,.T.);
#14399=EDGE_CURVE('',#11569,#11571,#274,.T.);
#14400=EDGE_CURVE('',#11572,#11573,#7313,.T.);
#14401=EDGE_CURVE('',#11572,#11570,#275,.T.);
#14402=EDGE_CURVE('',#11571,#11573,#276,.T.);
#14403=EDGE_CURVE('',#11574,#11575,#7314,.T.);
#14404=EDGE_CURVE('',#11574,#11572,#277,.T.);
#14405=EDGE_CURVE('',#11573,#11575,#278,.T.);
#14406=EDGE_CURVE('',#11576,#11577,#7315,.T.);
#14407=EDGE_CURVE('',#11576,#11574,#279,.T.);
#14408=EDGE_CURVE('',#11575,#11577,#280,.T.);
#14409=EDGE_CURVE('',#11578,#11579,#7316,.T.);
#14410=EDGE_CURVE('',#11578,#11576,#281,.T.);
#14411=EDGE_CURVE('',#11577,#11579,#282,.T.);
#14412=EDGE_CURVE('',#11580,#11581,#7317,.T.);
#14413=EDGE_CURVE('',#11580,#11578,#283,.T.);
#14414=EDGE_CURVE('',#11579,#11581,#284,.T.);
#14415=EDGE_CURVE('',#11582,#11583,#7318,.T.);
#14416=EDGE_CURVE('',#11582,#11580,#285,.T.);
#14417=EDGE_CURVE('',#11581,#11583,#286,.T.);
#14418=EDGE_CURVE('',#11584,#11585,#7319,.T.);
#14419=EDGE_CURVE('',#11584,#11582,#287,.T.);
#14420=EDGE_CURVE('',#11583,#11585,#288,.T.);
#14421=EDGE_CURVE('',#11586,#11587,#7320,.T.);
#14422=EDGE_CURVE('',#11586,#11584,#289,.T.);
#14423=EDGE_CURVE('',#11585,#11587,#290,.T.);
#14424=EDGE_CURVE('',#11588,#11589,#7321,.T.);
#14425=EDGE_CURVE('',#11588,#11586,#291,.T.);
#14426=EDGE_CURVE('',#11587,#11589,#292,.T.);
#14427=EDGE_CURVE('',#11590,#11591,#7322,.T.);
#14428=EDGE_CURVE('',#11590,#11588,#293,.T.);
#14429=EDGE_CURVE('',#11589,#11591,#294,.T.);
#14430=EDGE_CURVE('',#11592,#11593,#7323,.T.);
#14431=EDGE_CURVE('',#11592,#11590,#295,.T.);
#14432=EDGE_CURVE('',#11591,#11593,#296,.T.);
#14433=EDGE_CURVE('',#11594,#11595,#7324,.T.);
#14434=EDGE_CURVE('',#11594,#11592,#297,.T.);
#14435=EDGE_CURVE('',#11593,#11595,#298,.T.);
#14436=EDGE_CURVE('',#11596,#11597,#7325,.T.);
#14437=EDGE_CURVE('',#11596,#11594,#299,.T.);
#14438=EDGE_CURVE('',#11595,#11597,#300,.T.);
#14439=EDGE_CURVE('',#11598,#11599,#7326,.T.);
#14440=EDGE_CURVE('',#11598,#11596,#301,.T.);
#14441=EDGE_CURVE('',#11597,#11599,#302,.T.);
#14442=EDGE_CURVE('',#11600,#11601,#7327,.T.);
#14443=EDGE_CURVE('',#11600,#11598,#303,.T.);
#14444=EDGE_CURVE('',#11599,#11601,#304,.T.);
#14445=EDGE_CURVE('',#11602,#11603,#7328,.T.);
#14446=EDGE_CURVE('',#11602,#11600,#305,.T.);
#14447=EDGE_CURVE('',#11601,#11603,#306,.T.);
#14448=EDGE_CURVE('',#11604,#11605,#7329,.T.);
#14449=EDGE_CURVE('',#11604,#11602,#307,.T.);
#14450=EDGE_CURVE('',#11603,#11605,#308,.T.);
#14451=EDGE_CURVE('',#11606,#11607,#7330,.T.);
#14452=EDGE_CURVE('',#11606,#11604,#309,.T.);
#14453=EDGE_CURVE('',#11605,#11607,#310,.T.);
#14454=EDGE_CURVE('',#11608,#11609,#7331,.T.);
#14455=EDGE_CURVE('',#11608,#11606,#311,.T.);
#14456=EDGE_CURVE('',#11607,#11609,#312,.T.);
#14457=EDGE_CURVE('',#11610,#11611,#7332,.T.);
#14458=EDGE_CURVE('',#11610,#11608,#313,.T.);
#14459=EDGE_CURVE('',#11609,#11611,#314,.T.);
#14460=EDGE_CURVE('',#11612,#11613,#7333,.T.);
#14461=EDGE_CURVE('',#11612,#11610,#315,.T.);
#14462=EDGE_CURVE('',#11611,#11613,#316,.T.);
#14463=EDGE_CURVE('',#11614,#11615,#7334,.T.);
#14464=EDGE_CURVE('',#11614,#11612,#317,.T.);
#14465=EDGE_CURVE('',#11613,#11615,#318,.T.);
#14466=EDGE_CURVE('',#11616,#11617,#7335,.T.);
#14467=EDGE_CURVE('',#11616,#11614,#319,.T.);
#14468=EDGE_CURVE('',#11615,#11617,#320,.T.);
#14469=EDGE_CURVE('',#11618,#11619,#7336,.T.);
#14470=EDGE_CURVE('',#11618,#11616,#321,.T.);
#14471=EDGE_CURVE('',#11617,#11619,#322,.T.);
#14472=EDGE_CURVE('',#11620,#11621,#7337,.T.);
#14473=EDGE_CURVE('',#11620,#11622,#323,.T.);
#14474=EDGE_CURVE('',#11623,#11622,#5984,.T.);
#14475=EDGE_CURVE('',#11621,#11623,#324,.T.);
#14476=EDGE_CURVE('',#11624,#11625,#7338,.T.);
#14477=EDGE_CURVE('',#11624,#11620,#325,.T.);
#14478=EDGE_CURVE('',#11625,#11621,#326,.T.);
#14479=EDGE_CURVE('',#11626,#11627,#7339,.T.);
#14480=EDGE_CURVE('',#11626,#11624,#327,.T.);
#14481=EDGE_CURVE('',#11627,#11625,#328,.T.);
#14482=EDGE_CURVE('',#11628,#11629,#7340,.T.);
#14483=EDGE_CURVE('',#11628,#11626,#329,.T.);
#14484=EDGE_CURVE('',#11629,#11627,#330,.T.);
#14485=EDGE_CURVE('',#11630,#11631,#7341,.T.);
#14486=EDGE_CURVE('',#11630,#11628,#331,.T.);
#14487=EDGE_CURVE('',#11631,#11629,#332,.T.);
#14488=EDGE_CURVE('',#11632,#11633,#7342,.T.);
#14489=EDGE_CURVE('',#11632,#11630,#333,.T.);
#14490=EDGE_CURVE('',#11633,#11631,#334,.T.);
#14491=EDGE_CURVE('',#11634,#11635,#7343,.T.);
#14492=EDGE_CURVE('',#11634,#11632,#335,.T.);
#14493=EDGE_CURVE('',#11635,#11633,#336,.T.);
#14494=EDGE_CURVE('',#11636,#11637,#7344,.T.);
#14495=EDGE_CURVE('',#11636,#11634,#337,.T.);
#14496=EDGE_CURVE('',#11637,#11635,#338,.T.);
#14497=EDGE_CURVE('',#11638,#11639,#7345,.T.);
#14498=EDGE_CURVE('',#11638,#11636,#339,.T.);
#14499=EDGE_CURVE('',#11639,#11637,#340,.T.);
#14500=EDGE_CURVE('',#11640,#11641,#7346,.T.);
#14501=EDGE_CURVE('',#11640,#11638,#341,.T.);
#14502=EDGE_CURVE('',#11641,#11639,#342,.T.);
#14503=EDGE_CURVE('',#11642,#11643,#7347,.T.);
#14504=EDGE_CURVE('',#11642,#11640,#343,.T.);
#14505=EDGE_CURVE('',#11643,#11641,#344,.T.);
#14506=EDGE_CURVE('',#11644,#11645,#7348,.T.);
#14507=EDGE_CURVE('',#11644,#11642,#345,.T.);
#14508=EDGE_CURVE('',#11645,#11643,#346,.T.);
#14509=EDGE_CURVE('',#11646,#11647,#7349,.T.);
#14510=EDGE_CURVE('',#11646,#11644,#347,.T.);
#14511=EDGE_CURVE('',#11647,#11645,#348,.T.);
#14512=EDGE_CURVE('',#11648,#11649,#7350,.T.);
#14513=EDGE_CURVE('',#11648,#11646,#349,.T.);
#14514=EDGE_CURVE('',#11649,#11647,#350,.T.);
#14515=EDGE_CURVE('',#11650,#11651,#7351,.T.);
#14516=EDGE_CURVE('',#11650,#11648,#351,.T.);
#14517=EDGE_CURVE('',#11651,#11649,#352,.T.);
#14518=EDGE_CURVE('',#11652,#11653,#7352,.T.);
#14519=EDGE_CURVE('',#11652,#11650,#353,.T.);
#14520=EDGE_CURVE('',#11653,#11651,#354,.T.);
#14521=EDGE_CURVE('',#11654,#11655,#7353,.T.);
#14522=EDGE_CURVE('',#11654,#11652,#355,.T.);
#14523=EDGE_CURVE('',#11655,#11653,#356,.T.);
#14524=EDGE_CURVE('',#11656,#11657,#7354,.T.);
#14525=EDGE_CURVE('',#11656,#11654,#357,.T.);
#14526=EDGE_CURVE('',#11657,#11655,#358,.T.);
#14527=EDGE_CURVE('',#11658,#11659,#7355,.T.);
#14528=EDGE_CURVE('',#11658,#11656,#359,.T.);
#14529=EDGE_CURVE('',#11659,#11657,#360,.T.);
#14530=EDGE_CURVE('',#11660,#11661,#7356,.T.);
#14531=EDGE_CURVE('',#11660,#11658,#361,.T.);
#14532=EDGE_CURVE('',#11661,#11659,#362,.T.);
#14533=EDGE_CURVE('',#11662,#11663,#7357,.T.);
#14534=EDGE_CURVE('',#11662,#11660,#363,.T.);
#14535=EDGE_CURVE('',#11663,#11661,#364,.T.);
#14536=EDGE_CURVE('',#11664,#11665,#7358,.T.);
#14537=EDGE_CURVE('',#11664,#11662,#365,.T.);
#14538=EDGE_CURVE('',#11665,#11663,#366,.T.);
#14539=EDGE_CURVE('',#11666,#11667,#7359,.T.);
#14540=EDGE_CURVE('',#11666,#11664,#367,.T.);
#14541=EDGE_CURVE('',#11667,#11665,#368,.T.);
#14542=EDGE_CURVE('',#11668,#11669,#7360,.T.);
#14543=EDGE_CURVE('',#11668,#11666,#369,.T.);
#14544=EDGE_CURVE('',#11669,#11667,#370,.T.);
#14545=EDGE_CURVE('',#11670,#11671,#7361,.T.);
#14546=EDGE_CURVE('',#11670,#11668,#371,.T.);
#14547=EDGE_CURVE('',#11671,#11669,#372,.T.);
#14548=EDGE_CURVE('',#11672,#11673,#7362,.T.);
#14549=EDGE_CURVE('',#11672,#11670,#373,.T.);
#14550=EDGE_CURVE('',#11673,#11671,#374,.T.);
#14551=EDGE_CURVE('',#11674,#11675,#7363,.T.);
#14552=EDGE_CURVE('',#11674,#11672,#375,.T.);
#14553=EDGE_CURVE('',#11675,#11673,#376,.T.);
#14554=EDGE_CURVE('',#11676,#11677,#7364,.T.);
#14555=EDGE_CURVE('',#11676,#11674,#377,.T.);
#14556=EDGE_CURVE('',#11677,#11675,#378,.T.);
#14557=EDGE_CURVE('',#11678,#11679,#7365,.T.);
#14558=EDGE_CURVE('',#11678,#11676,#379,.T.);
#14559=EDGE_CURVE('',#11679,#11677,#380,.T.);
#14560=EDGE_CURVE('',#11680,#11681,#7366,.T.);
#14561=EDGE_CURVE('',#11680,#11678,#381,.T.);
#14562=EDGE_CURVE('',#11681,#11679,#382,.T.);
#14563=EDGE_CURVE('',#11682,#11683,#7367,.T.);
#14564=EDGE_CURVE('',#11682,#11680,#383,.T.);
#14565=EDGE_CURVE('',#11683,#11681,#384,.T.);
#14566=EDGE_CURVE('',#11684,#11685,#7368,.T.);
#14567=EDGE_CURVE('',#11684,#11682,#385,.T.);
#14568=EDGE_CURVE('',#11685,#11683,#386,.T.);
#14569=EDGE_CURVE('',#11686,#11687,#7369,.T.);
#14570=EDGE_CURVE('',#11686,#11684,#387,.T.);
#14571=EDGE_CURVE('',#11687,#11685,#388,.T.);
#14572=EDGE_CURVE('',#11688,#11689,#7370,.T.);
#14573=EDGE_CURVE('',#11688,#11686,#389,.T.);
#14574=EDGE_CURVE('',#11689,#11687,#390,.T.);
#14575=EDGE_CURVE('',#11690,#11691,#7371,.T.);
#14576=EDGE_CURVE('',#11690,#11688,#391,.T.);
#14577=EDGE_CURVE('',#11691,#11689,#392,.T.);
#14578=EDGE_CURVE('',#11692,#11693,#7372,.T.);
#14579=EDGE_CURVE('',#11692,#11690,#393,.T.);
#14580=EDGE_CURVE('',#11693,#11691,#394,.T.);
#14581=EDGE_CURVE('',#11694,#11695,#7373,.T.);
#14582=EDGE_CURVE('',#11694,#11692,#395,.T.);
#14583=EDGE_CURVE('',#11695,#11693,#396,.T.);
#14584=EDGE_CURVE('',#11696,#11697,#7374,.T.);
#14585=EDGE_CURVE('',#11696,#11694,#397,.T.);
#14586=EDGE_CURVE('',#11697,#11695,#398,.T.);
#14587=EDGE_CURVE('',#11698,#11699,#7375,.T.);
#14588=EDGE_CURVE('',#11698,#11696,#399,.T.);
#14589=EDGE_CURVE('',#11699,#11697,#400,.T.);
#14590=EDGE_CURVE('',#11700,#11701,#7376,.T.);
#14591=EDGE_CURVE('',#11700,#11698,#401,.T.);
#14592=EDGE_CURVE('',#11701,#11699,#402,.T.);
#14593=EDGE_CURVE('',#11702,#11703,#7377,.T.);
#14594=EDGE_CURVE('',#11702,#11700,#403,.T.);
#14595=EDGE_CURVE('',#11703,#11701,#404,.T.);
#14596=EDGE_CURVE('',#11704,#11705,#7378,.T.);
#14597=EDGE_CURVE('',#11704,#11702,#405,.T.);
#14598=EDGE_CURVE('',#11705,#11703,#406,.T.);
#14599=EDGE_CURVE('',#11706,#11706,#5985,.T.);
#14600=EDGE_CURVE('',#11706,#11707,#7379,.T.);
#14601=EDGE_CURVE('',#11707,#11708,#5986,.T.);
#14602=EDGE_CURVE('',#11708,#11707,#5987,.T.);
#14603=EDGE_CURVE('',#11708,#11709,#7380,.T.);
#14604=EDGE_CURVE('',#11710,#11709,#5988,.T.);
#14605=EDGE_CURVE('',#11711,#11710,#5989,.T.);
#14606=EDGE_CURVE('',#11709,#11711,#5990,.T.);
#14607=EDGE_CURVE('',#11712,#11712,#5991,.T.);
#14608=EDGE_CURVE('',#11712,#11713,#7381,.T.);
#14609=EDGE_CURVE('',#11713,#11713,#5992,.T.);
#14610=EDGE_CURVE('',#11714,#11714,#5993,.T.);
#14611=EDGE_CURVE('',#11714,#11713,#7382,.T.);
#14612=EDGE_CURVE('',#11715,#11715,#5994,.T.);
#14613=EDGE_CURVE('',#11716,#11710,#407,.T.);
#14614=EDGE_CURVE('',#11711,#11717,#408,.T.);
#14615=EDGE_CURVE('',#11717,#11716,#5995,.T.);
#14616=EDGE_CURVE('',#11711,#11718,#409,.T.);
#14617=EDGE_CURVE('',#11622,#11718,#410,.T.);
#14618=EDGE_CURVE('',#11719,#11704,#411,.T.);
#14619=EDGE_CURVE('',#11536,#11719,#412,.T.);
#14620=EDGE_CURVE('',#11717,#11618,#413,.T.);
#14621=EDGE_CURVE('',#11710,#11720,#414,.F.);
#14622=EDGE_CURVE('',#11720,#11718,#5996,.T.);
#14623=EDGE_CURVE('',#11720,#11623,#415,.T.);
#14624=EDGE_CURVE('',#11619,#11716,#416,.T.);
#14625=EDGE_CURVE('',#11721,#11537,#417,.T.);
#14626=EDGE_CURVE('',#11721,#11705,#418,.T.);
#14627=EDGE_CURVE('',#11719,#11721,#5997,.T.);
#14628=EDGE_CURVE('',#11722,#11714,#7383,.T.);
#14629=EDGE_CURVE('',#11723,#11724,#7384,.T.);
#14630=EDGE_CURVE('',#11725,#11723,#7385,.T.);
#14631=EDGE_CURVE('',#11726,#11725,#7386,.T.);
#14632=EDGE_CURVE('',#11726,#11724,#7387,.T.);
#14633=EDGE_CURVE('',#11724,#11727,#419,.T.);
#14634=EDGE_CURVE('',#11728,#11726,#5998,.T.);
#14635=EDGE_CURVE('',#11728,#11727,#7388,.T.);
#14636=EDGE_CURVE('',#11727,#11729,#7389,.T.);
#14637=EDGE_CURVE('',#11730,#11728,#7390,.T.);
#14638=EDGE_CURVE('',#11730,#11729,#7391,.T.);
#14639=EDGE_CURVE('',#11729,#11723,#420,.T.);
#14640=EDGE_CURVE('',#11725,#11730,#5999,.T.);
#14641=EDGE_CURVE('',#11731,#11731,#6000,.T.);
#14642=EDGE_CURVE('',#11731,#11715,#7392,.T.);
#14643=EDGE_CURVE('',#11732,#11732,#6001,.T.);
#14644=EDGE_CURVE('',#11732,#11731,#7393,.T.);
#14645=EDGE_CURVE('',#11733,#11733,#6002,.T.);
#14646=EDGE_CURVE('',#11734,#11734,#6003,.T.);
#14647=EDGE_CURVE('',#11734,#11733,#7394,.T.);
#14648=EDGE_CURVE('',#11735,#11735,#6004,.T.);
#14649=EDGE_CURVE('',#11735,#11734,#7395,.T.);
#14650=EDGE_CURVE('',#11736,#11736,#6005,.T.);
#14651=EDGE_CURVE('',#11736,#11735,#7396,.T.);
#14652=EDGE_CURVE('',#11737,#11737,#6006,.T.);
#14653=EDGE_CURVE('',#11737,#11738,#7397,.T.);
#14654=EDGE_CURVE('',#11738,#11739,#6007,.T.);
#14655=EDGE_CURVE('',#11739,#11738,#6008,.T.);
#14656=EDGE_CURVE('',#11740,#11741,#6009,.T.);
#14657=EDGE_CURVE('',#11741,#11740,#6010,.T.);
#14658=EDGE_CURVE('',#11741,#11739,#7398,.T.);
#14659=EDGE_CURVE('',#11742,#11742,#6011,.T.);
#14660=EDGE_CURVE('',#11740,#11743,#7399,.T.);
#14661=EDGE_CURVE('',#11743,#11744,#6012,.T.);
#14662=EDGE_CURVE('',#11744,#11743,#6013,.T.);
#14663=EDGE_CURVE('',#11745,#11745,#6014,.T.);
#14664=EDGE_CURVE('',#11745,#11744,#7400,.T.);
#14665=EDGE_CURVE('',#11746,#11746,#6015,.T.);
#14666=EDGE_CURVE('',#11747,#11747,#6016,.T.);
#14667=EDGE_CURVE('',#11748,#11748,#6017,.T.);
#14668=EDGE_CURVE('',#11748,#11747,#7401,.T.);
#14669=EDGE_CURVE('',#11749,#11749,#6018,.T.);
#14670=EDGE_CURVE('',#11749,#11750,#7402,.T.);
#14671=EDGE_CURVE('',#11750,#11750,#6019,.T.);
#14672=EDGE_CURVE('',#11750,#11742,#7403,.T.);
#14673=EDGE_CURVE('',#11751,#11751,#6020,.T.);
#14674=EDGE_CURVE('',#11751,#11746,#7404,.T.);
#14675=EDGE_CURVE('',#11752,#11752,#6021,.T.);
#14676=EDGE_CURVE('',#11752,#11751,#7405,.T.);
#14677=EDGE_CURVE('',#11753,#11753,#6022,.T.);
#14678=EDGE_CURVE('',#11753,#11745,#7406,.T.);
#14679=EDGE_CURVE('',#11754,#11755,#6023,.T.);
#14680=EDGE_CURVE('',#11755,#11754,#6024,.T.);
#14681=EDGE_CURVE('',#11754,#11756,#7407,.T.);
#14682=EDGE_CURVE('',#11756,#11756,#6025,.T.);
#14683=EDGE_CURVE('',#11757,#11757,#6026,.T.);
#14684=EDGE_CURVE('',#11755,#11758,#7408,.T.);
#14685=EDGE_CURVE('',#11758,#11758,#6027,.T.);
#14686=EDGE_CURVE('',#11759,#11759,#6028,.T.);
#14687=EDGE_CURVE('',#11759,#11760,#7409,.T.);
#14688=EDGE_CURVE('',#11760,#11761,#6029,.T.);
#14689=EDGE_CURVE('',#11761,#11760,#6030,.T.);
#14690=EDGE_CURVE('',#11761,#11762,#7410,.T.);
#14691=EDGE_CURVE('',#11763,#11762,#6031,.T.);
#14692=EDGE_CURVE('',#11762,#11763,#6032,.T.);
#14693=EDGE_CURVE('',#11764,#11764,#6033,.T.);
#14694=EDGE_CURVE('',#11765,#11765,#6034,.T.);
#14695=EDGE_CURVE('',#11766,#11766,#6035,.T.);
#14696=EDGE_CURVE('',#11767,#11767,#6036,.T.);
#14697=EDGE_CURVE('',#11768,#11768,#6037,.T.);
#14698=EDGE_CURVE('',#11763,#11769,#7411,.T.);
#14699=EDGE_CURVE('',#11769,#11770,#6038,.T.);
#14700=EDGE_CURVE('',#11770,#11769,#6039,.T.);
#14701=EDGE_CURVE('',#11770,#11771,#7412,.T.);
#14702=EDGE_CURVE('',#11772,#11771,#6040,.T.);
#14703=EDGE_CURVE('',#11771,#11772,#6041,.T.);
#14704=EDGE_CURVE('',#11772,#11773,#7413,.T.);
#14705=EDGE_CURVE('',#11773,#11774,#6042,.T.);
#14706=EDGE_CURVE('',#11774,#11773,#6043,.T.);
#14707=EDGE_CURVE('',#11774,#11775,#7414,.T.);
#14708=EDGE_CURVE('',#11776,#11775,#6044,.T.);
#14709=EDGE_CURVE('',#11775,#11776,#6045,.T.);
#14710=EDGE_CURVE('',#11776,#11777,#7415,.T.);
#14711=EDGE_CURVE('',#11777,#11777,#6046,.T.);
#14712=EDGE_CURVE('',#11778,#11778,#6047,.T.);
#14713=EDGE_CURVE('',#11779,#11779,#6048,.T.);
#14714=EDGE_CURVE('',#11780,#11780,#6049,.T.);
#14715=EDGE_CURVE('',#11781,#11781,#6050,.T.);
#14716=EDGE_CURVE('',#11782,#11782,#6051,.T.);
#14717=EDGE_CURVE('',#11783,#11784,#6052,.T.);
#14718=EDGE_CURVE('',#11784,#11783,#6053,.T.);
#14719=EDGE_CURVE('',#11783,#11785,#7416,.T.);
#14720=EDGE_CURVE('',#11785,#11786,#6054,.T.);
#14721=EDGE_CURVE('',#11786,#11785,#6055,.T.);
#14722=EDGE_CURVE('',#11786,#11787,#7417,.T.);
#14723=EDGE_CURVE('',#11788,#11787,#6056,.T.);
#14724=EDGE_CURVE('',#11787,#11788,#6057,.T.);
#14725=EDGE_CURVE('',#11778,#11784,#7418,.T.);
#14726=EDGE_CURVE('',#11788,#11789,#7419,.T.);
#14727=EDGE_CURVE('',#11789,#11789,#6058,.T.);
#14728=EDGE_CURVE('',#11790,#11790,#6059,.T.);
#14729=EDGE_CURVE('',#11790,#11791,#7420,.T.);
#14730=EDGE_CURVE('',#11791,#11792,#6060,.T.);
#14731=EDGE_CURVE('',#11792,#11791,#6061,.T.);
#14732=EDGE_CURVE('',#11793,#11793,#6062,.T.);
#14733=EDGE_CURVE('',#11793,#11792,#7421,.T.);
#14734=EDGE_CURVE('',#11768,#11782,#7422,.T.);
#14735=EDGE_CURVE('',#11767,#11781,#7423,.T.);
#14736=EDGE_CURVE('',#11766,#11780,#7424,.T.);
#14737=EDGE_CURVE('',#11765,#11779,#7425,.T.);
#14738=EDGE_CURVE('',#11794,#11794,#6063,.T.);
#14739=EDGE_CURVE('',#11794,#11764,#7426,.T.);
#14740=EDGE_CURVE('',#11757,#11794,#7427,.T.);
#14741=EDGE_CURVE('',#11795,#11795,#6064,.T.);
#14742=EDGE_CURVE('',#11795,#11796,#7428,.T.);
#14743=EDGE_CURVE('',#11796,#11796,#6065,.T.);
#14744=EDGE_CURVE('',#11797,#11798,#6066,.T.);
#14745=EDGE_CURVE('',#11798,#11797,#6067,.T.);
#14746=EDGE_CURVE('',#11797,#11799,#7429,.T.);
#14747=EDGE_CURVE('',#11799,#11800,#6068,.T.);
#14748=EDGE_CURVE('',#11800,#11799,#6069,.T.);
#14749=EDGE_CURVE('',#11800,#11801,#7430,.T.);
#14750=EDGE_CURVE('',#11802,#11801,#6070,.T.);
#14751=EDGE_CURVE('',#11801,#11802,#6071,.T.);
#14752=EDGE_CURVE('',#11803,#11804,#421,.T.);
#14753=EDGE_CURVE('',#11804,#11803,#422,.T.);
#14754=EDGE_CURVE('',#11805,#11806,#423,.T.);
#14755=EDGE_CURVE('',#11806,#11805,#424,.T.);
#14756=EDGE_CURVE('',#11807,#11808,#425,.T.);
#14757=EDGE_CURVE('',#11808,#11807,#426,.T.);
#14758=EDGE_CURVE('',#11809,#11810,#427,.T.);
#14759=EDGE_CURVE('',#11810,#11809,#428,.T.);
#14760=EDGE_CURVE('',#11811,#11812,#6072,.T.);
#14761=EDGE_CURVE('',#11812,#11811,#6073,.T.);
#14762=EDGE_CURVE('',#11812,#11798,#7431,.T.);
#14763=EDGE_CURVE('',#11802,#11813,#7432,.T.);
#14764=EDGE_CURVE('',#11813,#11814,#6074,.T.);
#14765=EDGE_CURVE('',#11814,#11813,#6075,.T.);
#14766=EDGE_CURVE('',#11814,#11815,#7433,.T.);
#14767=EDGE_CURVE('',#11816,#11815,#6076,.T.);
#14768=EDGE_CURVE('',#11815,#11816,#6077,.T.);
#14769=EDGE_CURVE('',#11816,#11817,#7434,.T.);
#14770=EDGE_CURVE('',#11817,#11817,#6078,.T.);
#14771=EDGE_CURVE('',#11818,#11818,#6079,.T.);
#14772=EDGE_CURVE('',#11819,#11819,#6080,.T.);
#14773=EDGE_CURVE('',#11819,#11811,#7435,.T.);
#14774=EDGE_CURVE('',#11820,#11821,#7436,.T.);
#14775=EDGE_CURVE('',#11822,#11820,#6081,.T.);
#14776=EDGE_CURVE('',#11823,#11822,#7437,.T.);
#14777=EDGE_CURVE('',#11821,#11823,#7438,.T.);
#14778=EDGE_CURVE('',#11824,#11825,#7439,.T.);
#14779=EDGE_CURVE('',#11825,#11820,#1099,.T.);
#14780=EDGE_CURVE('',#11821,#11824,#7440,.T.);
#14781=EDGE_CURVE('',#11822,#11826,#1100,.T.);
#14782=EDGE_CURVE('',#11826,#11827,#7441,.T.);
#14783=EDGE_CURVE('',#11827,#11823,#7442,.T.);
#14784=EDGE_CURVE('',#11827,#11824,#7443,.T.);
#14785=EDGE_CURVE('',#11828,#11827,#7444,.T.);
#14786=EDGE_CURVE('',#11829,#11828,#7445,.T.);
#14787=EDGE_CURVE('',#11824,#11829,#7446,.T.);
#14788=EDGE_CURVE('',#11830,#11826,#7447,.T.);
#14789=EDGE_CURVE('',#11828,#11830,#7448,.T.);
#14790=EDGE_CURVE('',#11829,#11831,#7449,.T.);
#14791=EDGE_CURVE('',#11825,#11831,#7450,.T.);
#14792=EDGE_CURVE('',#11830,#11831,#6082,.T.);
#14793=EDGE_CURVE('',#11832,#11833,#429,.T.);
#14794=EDGE_CURVE('',#11834,#11832,#430,.T.);
#14795=EDGE_CURVE('',#11833,#11834,#431,.T.);
#14796=EDGE_CURVE('',#11833,#11804,#7451,.T.);
#14797=EDGE_CURVE('',#11835,#11836,#432,.T.);
#14798=EDGE_CURVE('',#11837,#11835,#433,.T.);
#14799=EDGE_CURVE('',#11836,#11837,#434,.T.);
#14800=EDGE_CURVE('',#11836,#11806,#7452,.T.);
#14801=EDGE_CURVE('',#11838,#11839,#435,.T.);
#14802=EDGE_CURVE('',#11840,#11838,#436,.T.);
#14803=EDGE_CURVE('',#11839,#11840,#437,.T.);
#14804=EDGE_CURVE('',#11839,#11808,#7453,.T.);
#14805=EDGE_CURVE('',#11841,#11842,#438,.T.);
#14806=EDGE_CURVE('',#11843,#11841,#439,.T.);
#14807=EDGE_CURVE('',#11842,#11843,#440,.T.);
#14808=EDGE_CURVE('',#11842,#11810,#7454,.T.);
#14809=EDGE_CURVE('',#11844,#11844,#6083,.T.);
#14810=EDGE_CURVE('',#11839,#11844,#6084,.T.);
#14811=EDGE_CURVE('',#11836,#11840,#6085,.T.);
#14812=EDGE_CURVE('',#11833,#11837,#6086,.T.);
#14813=EDGE_CURVE('',#11842,#11834,#6087,.T.);
#14814=EDGE_CURVE('',#11844,#11843,#6088,.T.);
#14815=EDGE_CURVE('',#11845,#11845,#6089,.T.);
#14816=EDGE_CURVE('',#11845,#11818,#7455,.T.);
#14817=EDGE_CURVE('',#11846,#11847,#7456,.T.);
#14818=EDGE_CURVE('',#11846,#11848,#441,.T.);
#14819=EDGE_CURVE('',#11848,#11849,#6090,.T.);
#14820=EDGE_CURVE('',#11849,#11847,#442,.T.);
#14821=EDGE_CURVE('',#11850,#11851,#7457,.T.);
#14822=EDGE_CURVE('',#11850,#11846,#443,.T.);
#14823=EDGE_CURVE('',#11847,#11851,#444,.T.);
#14824=EDGE_CURVE('',#11852,#11853,#7458,.T.);
#14825=EDGE_CURVE('',#11852,#11850,#445,.T.);
#14826=EDGE_CURVE('',#11851,#11853,#446,.T.);
#14827=EDGE_CURVE('',#11854,#11855,#7459,.T.);
#14828=EDGE_CURVE('',#11854,#11852,#447,.T.);
#14829=EDGE_CURVE('',#11853,#11855,#448,.T.);
#14830=EDGE_CURVE('',#11856,#11857,#7460,.T.);
#14831=EDGE_CURVE('',#11856,#11854,#449,.T.);
#14832=EDGE_CURVE('',#11855,#11857,#450,.T.);
#14833=EDGE_CURVE('',#11858,#11859,#7461,.T.);
#14834=EDGE_CURVE('',#11858,#11856,#451,.T.);
#14835=EDGE_CURVE('',#11857,#11859,#452,.T.);
#14836=EDGE_CURVE('',#11860,#11861,#7462,.T.);
#14837=EDGE_CURVE('',#11860,#11858,#453,.T.);
#14838=EDGE_CURVE('',#11859,#11861,#454,.T.);
#14839=EDGE_CURVE('',#11862,#11863,#7463,.T.);
#14840=EDGE_CURVE('',#11862,#11860,#455,.T.);
#14841=EDGE_CURVE('',#11861,#11863,#456,.T.);
#14842=EDGE_CURVE('',#11864,#11865,#7464,.T.);
#14843=EDGE_CURVE('',#11864,#11862,#457,.T.);
#14844=EDGE_CURVE('',#11863,#11865,#458,.T.);
#14845=EDGE_CURVE('',#11866,#11867,#7465,.T.);
#14846=EDGE_CURVE('',#11866,#11864,#459,.T.);
#14847=EDGE_CURVE('',#11865,#11867,#460,.T.);
#14848=EDGE_CURVE('',#11868,#11869,#7466,.T.);
#14849=EDGE_CURVE('',#11868,#11866,#461,.T.);
#14850=EDGE_CURVE('',#11867,#11869,#462,.T.);
#14851=EDGE_CURVE('',#11870,#11871,#7467,.T.);
#14852=EDGE_CURVE('',#11870,#11868,#463,.T.);
#14853=EDGE_CURVE('',#11869,#11871,#464,.T.);
#14854=EDGE_CURVE('',#11872,#11873,#7468,.T.);
#14855=EDGE_CURVE('',#11872,#11870,#465,.T.);
#14856=EDGE_CURVE('',#11871,#11873,#466,.T.);
#14857=EDGE_CURVE('',#11874,#11875,#7469,.T.);
#14858=EDGE_CURVE('',#11874,#11872,#467,.T.);
#14859=EDGE_CURVE('',#11873,#11875,#468,.T.);
#14860=EDGE_CURVE('',#11876,#11877,#7470,.T.);
#14861=EDGE_CURVE('',#11876,#11874,#469,.T.);
#14862=EDGE_CURVE('',#11875,#11877,#470,.T.);
#14863=EDGE_CURVE('',#11878,#11879,#7471,.T.);
#14864=EDGE_CURVE('',#11878,#11876,#471,.T.);
#14865=EDGE_CURVE('',#11877,#11879,#472,.T.);
#14866=EDGE_CURVE('',#11880,#11881,#7472,.T.);
#14867=EDGE_CURVE('',#11880,#11882,#473,.T.);
#14868=EDGE_CURVE('',#11883,#11882,#6091,.T.);
#14869=EDGE_CURVE('',#11881,#11883,#474,.T.);
#14870=EDGE_CURVE('',#11884,#11885,#7473,.T.);
#14871=EDGE_CURVE('',#11884,#11880,#475,.T.);
#14872=EDGE_CURVE('',#11885,#11881,#476,.T.);
#14873=EDGE_CURVE('',#11886,#11887,#7474,.T.);
#14874=EDGE_CURVE('',#11886,#11884,#477,.T.);
#14875=EDGE_CURVE('',#11887,#11885,#478,.T.);
#14876=EDGE_CURVE('',#11888,#11889,#7475,.T.);
#14877=EDGE_CURVE('',#11888,#11886,#479,.T.);
#14878=EDGE_CURVE('',#11889,#11887,#480,.T.);
#14879=EDGE_CURVE('',#11890,#11891,#7476,.T.);
#14880=EDGE_CURVE('',#11890,#11888,#481,.T.);
#14881=EDGE_CURVE('',#11891,#11889,#482,.T.);
#14882=EDGE_CURVE('',#11892,#11893,#7477,.T.);
#14883=EDGE_CURVE('',#11892,#11890,#483,.T.);
#14884=EDGE_CURVE('',#11893,#11891,#484,.T.);
#14885=EDGE_CURVE('',#11894,#11895,#7478,.T.);
#14886=EDGE_CURVE('',#11894,#11892,#485,.T.);
#14887=EDGE_CURVE('',#11895,#11893,#486,.T.);
#14888=EDGE_CURVE('',#11896,#11897,#7479,.T.);
#14889=EDGE_CURVE('',#11896,#11894,#487,.T.);
#14890=EDGE_CURVE('',#11897,#11895,#488,.T.);
#14891=EDGE_CURVE('',#11898,#11899,#7480,.T.);
#14892=EDGE_CURVE('',#11898,#11896,#489,.T.);
#14893=EDGE_CURVE('',#11899,#11897,#490,.T.);
#14894=EDGE_CURVE('',#11900,#11901,#7481,.T.);
#14895=EDGE_CURVE('',#11900,#11898,#491,.T.);
#14896=EDGE_CURVE('',#11901,#11899,#492,.T.);
#14897=EDGE_CURVE('',#11902,#11903,#7482,.T.);
#14898=EDGE_CURVE('',#11902,#11900,#493,.T.);
#14899=EDGE_CURVE('',#11903,#11901,#494,.T.);
#14900=EDGE_CURVE('',#11904,#11905,#7483,.T.);
#14901=EDGE_CURVE('',#11904,#11902,#495,.T.);
#14902=EDGE_CURVE('',#11905,#11903,#496,.T.);
#14903=EDGE_CURVE('',#11906,#11907,#7484,.T.);
#14904=EDGE_CURVE('',#11906,#11904,#497,.T.);
#14905=EDGE_CURVE('',#11907,#11905,#498,.T.);
#14906=EDGE_CURVE('',#11908,#11909,#7485,.T.);
#14907=EDGE_CURVE('',#11908,#11906,#499,.T.);
#14908=EDGE_CURVE('',#11909,#11907,#500,.T.);
#14909=EDGE_CURVE('',#11910,#11911,#7486,.T.);
#14910=EDGE_CURVE('',#11910,#11908,#501,.T.);
#14911=EDGE_CURVE('',#11911,#11909,#502,.T.);
#14912=EDGE_CURVE('',#11882,#11912,#503,.T.);
#14913=EDGE_CURVE('',#11913,#11912,#6092,.T.);
#14914=EDGE_CURVE('',#11914,#11913,#6093,.T.);
#14915=EDGE_CURVE('',#11914,#11883,#504,.T.);
#14916=EDGE_CURVE('',#11879,#11914,#505,.T.);
#14917=EDGE_CURVE('',#11915,#11849,#506,.T.);
#14918=EDGE_CURVE('',#11915,#11911,#507,.T.);
#14919=EDGE_CURVE('',#11849,#11916,#6094,.T.);
#14920=EDGE_CURVE('',#11916,#11848,#6095,.T.);
#14921=EDGE_CURVE('',#11848,#11917,#508,.T.);
#14922=EDGE_CURVE('',#11917,#11915,#6096,.T.);
#14923=EDGE_CURVE('',#11917,#11910,#509,.T.);
#14924=EDGE_CURVE('',#11912,#11878,#510,.T.);
#14925=EDGE_CURVE('',#11913,#11918,#6097,.T.);
#14926=EDGE_CURVE('',#11918,#11918,#6098,.T.);
#14927=EDGE_CURVE('',#11912,#11914,#6099,.T.);
#14928=EDGE_CURVE('',#11919,#11919,#6100,.T.);
#14929=EDGE_CURVE('',#11920,#11921,#7487,.T.);
#14930=EDGE_CURVE('',#11921,#11920,#6101,.T.);
#14931=EDGE_CURVE('',#11921,#11922,#7488,.T.);
#14932=EDGE_CURVE('',#11922,#11921,#6102,.T.);
#14933=EDGE_CURVE('',#11922,#11923,#7489,.T.);
#14934=EDGE_CURVE('',#11923,#11922,#6103,.T.);
#14935=EDGE_CURVE('',#11923,#11924,#7490,.T.);
#14936=EDGE_CURVE('',#11924,#11923,#6104,.T.);
#14937=EDGE_CURVE('',#11924,#11925,#7491,.T.);
#14938=EDGE_CURVE('',#11925,#11924,#6105,.T.);
#14939=EDGE_CURVE('',#11925,#11920,#7492,.T.);
#14940=EDGE_CURVE('',#11920,#11925,#6106,.T.);
#14941=EDGE_CURVE('',#11926,#11924,#7493,.T.);
#14942=EDGE_CURVE('',#11927,#11928,#7494,.T.);
#14943=EDGE_CURVE('',#11927,#11920,#7495,.T.);
#14944=EDGE_CURVE('',#11928,#11921,#7496,.T.);
#14945=EDGE_CURVE('',#11929,#11927,#7497,.T.);
#14946=EDGE_CURVE('',#11929,#11925,#7498,.T.);
#14947=EDGE_CURVE('',#11930,#11929,#7499,.T.);
#14948=EDGE_CURVE('',#11930,#11924,#7500,.T.);
#14949=EDGE_CURVE('',#11931,#11930,#7501,.T.);
#14950=EDGE_CURVE('',#11931,#11923,#7502,.T.);
#14951=EDGE_CURVE('',#11932,#11931,#7503,.T.);
#14952=EDGE_CURVE('',#11932,#11922,#7504,.T.);
#14953=EDGE_CURVE('',#11928,#11932,#7505,.T.);
#14954=EDGE_CURVE('',#11933,#11934,#7506,.T.);
#14955=EDGE_CURVE('',#11933,#11935,#7507,.T.);
#14956=EDGE_CURVE('',#11936,#11935,#7508,.T.);
#14957=EDGE_CURVE('',#11934,#11936,#7509,.T.);
#14958=EDGE_CURVE('',#11934,#11937,#6107,.T.);
#14959=EDGE_CURVE('',#11936,#11937,#7510,.T.);
#14960=EDGE_CURVE('',#11937,#11938,#7511,.T.);
#14961=EDGE_CURVE('',#11935,#11938,#7512,.T.);
#14962=EDGE_CURVE('',#11938,#11933,#6108,.T.);
#14963=EDGE_CURVE('',#11939,#11940,#7513,.T.);
#14964=EDGE_CURVE('',#11939,#11941,#7514,.T.);
#14965=EDGE_CURVE('',#11942,#11941,#7515,.T.);
#14966=EDGE_CURVE('',#11940,#11942,#7516,.T.);
#14967=EDGE_CURVE('',#11940,#11943,#6109,.T.);
#14968=EDGE_CURVE('',#11942,#11943,#7517,.T.);
#14969=EDGE_CURVE('',#11943,#11944,#7518,.T.);
#14970=EDGE_CURVE('',#11941,#11944,#7519,.T.);
#14971=EDGE_CURVE('',#11944,#11939,#6110,.T.);
#14972=EDGE_CURVE('',#11945,#11946,#7520,.T.);
#14973=EDGE_CURVE('',#11945,#11947,#7521,.T.);
#14974=EDGE_CURVE('',#11948,#11947,#7522,.T.);
#14975=EDGE_CURVE('',#11946,#11948,#7523,.T.);
#14976=EDGE_CURVE('',#11946,#11949,#6111,.T.);
#14977=EDGE_CURVE('',#11948,#11949,#7524,.T.);
#14978=EDGE_CURVE('',#11949,#11950,#7525,.T.);
#14979=EDGE_CURVE('',#11947,#11950,#7526,.T.);
#14980=EDGE_CURVE('',#11950,#11945,#6112,.T.);
#14981=EDGE_CURVE('',#11951,#11952,#7527,.T.);
#14982=EDGE_CURVE('',#11951,#11953,#7528,.T.);
#14983=EDGE_CURVE('',#11954,#11953,#7529,.T.);
#14984=EDGE_CURVE('',#11952,#11954,#7530,.T.);
#14985=EDGE_CURVE('',#11952,#11955,#6113,.T.);
#14986=EDGE_CURVE('',#11954,#11955,#7531,.T.);
#14987=EDGE_CURVE('',#11955,#11956,#7532,.T.);
#14988=EDGE_CURVE('',#11953,#11956,#7533,.T.);
#14989=EDGE_CURVE('',#11956,#11951,#6114,.T.);
#14990=EDGE_CURVE('',#11957,#11958,#7534,.T.);
#14991=EDGE_CURVE('',#11957,#11959,#7535,.T.);
#14992=EDGE_CURVE('',#11960,#11959,#7536,.T.);
#14993=EDGE_CURVE('',#11958,#11960,#7537,.T.);
#14994=EDGE_CURVE('',#11958,#11961,#6115,.T.);
#14995=EDGE_CURVE('',#11960,#11961,#7538,.T.);
#14996=EDGE_CURVE('',#11961,#11962,#7539,.T.);
#14997=EDGE_CURVE('',#11959,#11962,#7540,.T.);
#14998=EDGE_CURVE('',#11962,#11957,#6116,.T.);
#14999=EDGE_CURVE('',#11963,#11964,#7541,.T.);
#15000=EDGE_CURVE('',#11963,#11965,#7542,.T.);
#15001=EDGE_CURVE('',#11966,#11965,#7543,.T.);
#15002=EDGE_CURVE('',#11964,#11966,#7544,.T.);
#15003=EDGE_CURVE('',#11964,#11967,#6117,.T.);
#15004=EDGE_CURVE('',#11966,#11967,#7545,.T.);
#15005=EDGE_CURVE('',#11967,#11968,#7546,.T.);
#15006=EDGE_CURVE('',#11965,#11968,#7547,.T.);
#15007=EDGE_CURVE('',#11968,#11963,#6118,.T.);
#15008=EDGE_CURVE('',#11969,#11970,#7548,.T.);
#15009=EDGE_CURVE('',#11969,#11971,#7549,.T.);
#15010=EDGE_CURVE('',#11972,#11971,#7550,.T.);
#15011=EDGE_CURVE('',#11970,#11972,#7551,.T.);
#15012=EDGE_CURVE('',#11970,#11973,#6119,.T.);
#15013=EDGE_CURVE('',#11972,#11973,#7552,.T.);
#15014=EDGE_CURVE('',#11973,#11974,#7553,.T.);
#15015=EDGE_CURVE('',#11971,#11974,#7554,.T.);
#15016=EDGE_CURVE('',#11974,#11969,#6120,.T.);
#15017=EDGE_CURVE('',#11975,#11976,#7555,.T.);
#15018=EDGE_CURVE('',#11975,#11977,#7556,.T.);
#15019=EDGE_CURVE('',#11978,#11977,#7557,.T.);
#15020=EDGE_CURVE('',#11976,#11978,#7558,.T.);
#15021=EDGE_CURVE('',#11976,#11979,#6121,.T.);
#15022=EDGE_CURVE('',#11978,#11979,#7559,.T.);
#15023=EDGE_CURVE('',#11979,#11980,#7560,.T.);
#15024=EDGE_CURVE('',#11977,#11980,#7561,.T.);
#15025=EDGE_CURVE('',#11980,#11975,#6122,.T.);
#15026=EDGE_CURVE('',#11981,#11982,#7562,.T.);
#15027=EDGE_CURVE('',#11981,#11983,#7563,.T.);
#15028=EDGE_CURVE('',#11984,#11983,#7564,.T.);
#15029=EDGE_CURVE('',#11982,#11984,#7565,.T.);
#15030=EDGE_CURVE('',#11982,#11985,#6123,.T.);
#15031=EDGE_CURVE('',#11984,#11986,#7566,.T.);
#15032=EDGE_CURVE('',#11985,#11986,#6124,.T.);
#15033=EDGE_CURVE('',#11986,#11987,#7567,.T.);
#15034=EDGE_CURVE('',#11983,#11987,#7568,.T.);
#15035=EDGE_CURVE('',#11987,#11988,#6125,.T.);
#15036=EDGE_CURVE('',#11988,#11981,#6126,.T.);
#15037=EDGE_CURVE('',#11989,#11990,#7569,.T.);
#15038=EDGE_CURVE('',#11989,#11991,#7570,.T.);
#15039=EDGE_CURVE('',#11992,#11991,#7571,.T.);
#15040=EDGE_CURVE('',#11990,#11992,#7572,.T.);
#15041=EDGE_CURVE('',#11990,#11993,#6127,.T.);
#15042=EDGE_CURVE('',#11992,#11993,#7573,.T.);
#15043=EDGE_CURVE('',#11993,#11994,#7574,.T.);
#15044=EDGE_CURVE('',#11991,#11994,#7575,.T.);
#15045=EDGE_CURVE('',#11994,#11989,#6128,.T.);
#15046=EDGE_CURVE('',#11995,#11996,#7576,.T.);
#15047=EDGE_CURVE('',#11995,#11997,#7577,.T.);
#15048=EDGE_CURVE('',#11998,#11997,#7578,.T.);
#15049=EDGE_CURVE('',#11996,#11998,#7579,.T.);
#15050=EDGE_CURVE('',#11996,#11999,#6129,.T.);
#15051=EDGE_CURVE('',#11998,#11999,#7580,.T.);
#15052=EDGE_CURVE('',#11999,#12000,#7581,.T.);
#15053=EDGE_CURVE('',#11997,#12000,#7582,.T.);
#15054=EDGE_CURVE('',#12000,#11995,#6130,.T.);
#15055=EDGE_CURVE('',#12001,#12002,#7583,.T.);
#15056=EDGE_CURVE('',#12001,#12003,#7584,.T.);
#15057=EDGE_CURVE('',#12004,#12003,#7585,.T.);
#15058=EDGE_CURVE('',#12002,#12004,#7586,.T.);
#15059=EDGE_CURVE('',#12002,#12005,#6131,.T.);
#15060=EDGE_CURVE('',#12004,#12005,#7587,.T.);
#15061=EDGE_CURVE('',#12005,#12006,#7588,.T.);
#15062=EDGE_CURVE('',#12003,#12006,#7589,.T.);
#15063=EDGE_CURVE('',#12006,#12001,#6132,.T.);
#15064=EDGE_CURVE('',#12007,#12008,#7590,.T.);
#15065=EDGE_CURVE('',#12007,#12009,#7591,.T.);
#15066=EDGE_CURVE('',#12010,#12009,#7592,.T.);
#15067=EDGE_CURVE('',#12008,#12010,#7593,.T.);
#15068=EDGE_CURVE('',#12008,#12011,#6133,.T.);
#15069=EDGE_CURVE('',#12010,#12011,#7594,.T.);
#15070=EDGE_CURVE('',#12011,#12012,#7595,.T.);
#15071=EDGE_CURVE('',#12009,#12012,#7596,.T.);
#15072=EDGE_CURVE('',#12012,#12007,#6134,.T.);
#15073=EDGE_CURVE('',#12013,#12014,#7597,.T.);
#15074=EDGE_CURVE('',#12013,#12015,#7598,.T.);
#15075=EDGE_CURVE('',#12016,#12015,#7599,.T.);
#15076=EDGE_CURVE('',#12014,#12016,#7600,.T.);
#15077=EDGE_CURVE('',#12014,#12017,#6135,.T.);
#15078=EDGE_CURVE('',#12016,#12017,#7601,.T.);
#15079=EDGE_CURVE('',#12017,#12018,#7602,.T.);
#15080=EDGE_CURVE('',#12015,#12018,#7603,.T.);
#15081=EDGE_CURVE('',#12018,#12013,#6136,.T.);
#15082=EDGE_CURVE('',#12019,#12020,#7604,.T.);
#15083=EDGE_CURVE('',#12019,#12021,#7605,.T.);
#15084=EDGE_CURVE('',#12022,#12021,#7606,.T.);
#15085=EDGE_CURVE('',#12020,#12022,#7607,.T.);
#15086=EDGE_CURVE('',#12020,#12023,#6137,.T.);
#15087=EDGE_CURVE('',#12022,#12023,#7608,.T.);
#15088=EDGE_CURVE('',#12023,#12024,#7609,.T.);
#15089=EDGE_CURVE('',#12021,#12024,#7610,.T.);
#15090=EDGE_CURVE('',#12024,#12019,#6138,.T.);
#15091=EDGE_CURVE('',#12025,#12026,#7611,.T.);
#15092=EDGE_CURVE('',#12025,#12027,#7612,.T.);
#15093=EDGE_CURVE('',#12028,#12027,#7613,.T.);
#15094=EDGE_CURVE('',#12026,#12028,#7614,.T.);
#15095=EDGE_CURVE('',#12026,#12029,#6139,.T.);
#15096=EDGE_CURVE('',#12028,#12029,#7615,.T.);
#15097=EDGE_CURVE('',#12029,#12030,#7616,.T.);
#15098=EDGE_CURVE('',#12027,#12030,#7617,.T.);
#15099=EDGE_CURVE('',#12030,#12025,#6140,.T.);
#15100=EDGE_CURVE('',#12031,#12032,#7618,.T.);
#15101=EDGE_CURVE('',#12031,#12033,#7619,.T.);
#15102=EDGE_CURVE('',#12034,#12033,#7620,.T.);
#15103=EDGE_CURVE('',#12032,#12034,#7621,.T.);
#15104=EDGE_CURVE('',#12032,#12035,#6141,.T.);
#15105=EDGE_CURVE('',#12034,#12035,#7622,.T.);
#15106=EDGE_CURVE('',#12035,#12036,#7623,.T.);
#15107=EDGE_CURVE('',#12033,#12036,#7624,.T.);
#15108=EDGE_CURVE('',#12036,#12031,#6142,.T.);
#15109=EDGE_CURVE('',#12037,#12038,#7625,.T.);
#15110=EDGE_CURVE('',#12037,#12039,#7626,.T.);
#15111=EDGE_CURVE('',#12040,#12039,#7627,.T.);
#15112=EDGE_CURVE('',#12038,#12040,#7628,.T.);
#15113=EDGE_CURVE('',#12038,#12041,#6143,.T.);
#15114=EDGE_CURVE('',#12040,#12041,#7629,.T.);
#15115=EDGE_CURVE('',#12041,#12042,#7630,.T.);
#15116=EDGE_CURVE('',#12039,#12042,#7631,.T.);
#15117=EDGE_CURVE('',#12042,#12037,#6144,.T.);
#15118=EDGE_CURVE('',#12043,#12044,#7632,.T.);
#15119=EDGE_CURVE('',#12043,#12045,#7633,.T.);
#15120=EDGE_CURVE('',#12046,#12045,#7634,.T.);
#15121=EDGE_CURVE('',#12044,#12046,#7635,.T.);
#15122=EDGE_CURVE('',#12044,#12047,#6145,.T.);
#15123=EDGE_CURVE('',#12046,#12047,#7636,.T.);
#15124=EDGE_CURVE('',#12047,#12048,#7637,.T.);
#15125=EDGE_CURVE('',#12045,#12048,#7638,.T.);
#15126=EDGE_CURVE('',#12048,#12043,#6146,.T.);
#15127=EDGE_CURVE('',#12049,#12050,#7639,.T.);
#15128=EDGE_CURVE('',#12049,#12051,#7640,.T.);
#15129=EDGE_CURVE('',#12052,#12051,#7641,.T.);
#15130=EDGE_CURVE('',#12050,#12052,#7642,.T.);
#15131=EDGE_CURVE('',#12050,#12053,#6147,.T.);
#15132=EDGE_CURVE('',#12052,#12053,#7643,.T.);
#15133=EDGE_CURVE('',#12053,#12054,#7644,.T.);
#15134=EDGE_CURVE('',#12051,#12054,#7645,.T.);
#15135=EDGE_CURVE('',#12054,#12049,#6148,.T.);
#15136=EDGE_CURVE('',#12055,#12056,#7646,.T.);
#15137=EDGE_CURVE('',#12055,#12057,#7647,.T.);
#15138=EDGE_CURVE('',#12058,#12057,#7648,.T.);
#15139=EDGE_CURVE('',#12056,#12058,#7649,.T.);
#15140=EDGE_CURVE('',#12056,#12059,#6149,.T.);
#15141=EDGE_CURVE('',#12058,#12059,#7650,.T.);
#15142=EDGE_CURVE('',#12059,#12060,#7651,.T.);
#15143=EDGE_CURVE('',#12057,#12060,#7652,.T.);
#15144=EDGE_CURVE('',#12060,#12055,#6150,.T.);
#15145=EDGE_CURVE('',#12061,#12062,#7653,.T.);
#15146=EDGE_CURVE('',#12061,#12063,#7654,.T.);
#15147=EDGE_CURVE('',#12064,#12063,#7655,.T.);
#15148=EDGE_CURVE('',#12062,#12064,#7656,.T.);
#15149=EDGE_CURVE('',#12062,#12065,#6151,.T.);
#15150=EDGE_CURVE('',#12064,#12065,#7657,.T.);
#15151=EDGE_CURVE('',#12065,#12066,#7658,.T.);
#15152=EDGE_CURVE('',#12063,#12066,#7659,.T.);
#15153=EDGE_CURVE('',#12066,#12061,#6152,.T.);
#15154=EDGE_CURVE('',#12067,#12068,#7660,.T.);
#15155=EDGE_CURVE('',#12067,#12069,#7661,.T.);
#15156=EDGE_CURVE('',#12070,#12069,#7662,.T.);
#15157=EDGE_CURVE('',#12068,#12070,#7663,.T.);
#15158=EDGE_CURVE('',#12068,#12071,#6153,.T.);
#15159=EDGE_CURVE('',#12070,#12071,#7664,.T.);
#15160=EDGE_CURVE('',#12071,#12072,#7665,.T.);
#15161=EDGE_CURVE('',#12069,#12072,#7666,.T.);
#15162=EDGE_CURVE('',#12072,#12067,#6154,.T.);
#15163=EDGE_CURVE('',#12073,#12074,#7667,.T.);
#15164=EDGE_CURVE('',#12073,#12075,#7668,.T.);
#15165=EDGE_CURVE('',#12076,#12075,#7669,.T.);
#15166=EDGE_CURVE('',#12074,#12076,#7670,.T.);
#15167=EDGE_CURVE('',#12074,#12077,#6155,.T.);
#15168=EDGE_CURVE('',#12076,#12077,#7671,.T.);
#15169=EDGE_CURVE('',#12077,#12078,#7672,.T.);
#15170=EDGE_CURVE('',#12075,#12078,#7673,.T.);
#15171=EDGE_CURVE('',#12078,#12073,#6156,.T.);
#15172=EDGE_CURVE('',#12079,#12080,#7674,.T.);
#15173=EDGE_CURVE('',#12079,#12081,#7675,.T.);
#15174=EDGE_CURVE('',#12082,#12081,#7676,.T.);
#15175=EDGE_CURVE('',#12080,#12082,#7677,.T.);
#15176=EDGE_CURVE('',#12080,#12083,#6157,.T.);
#15177=EDGE_CURVE('',#12082,#12083,#7678,.T.);
#15178=EDGE_CURVE('',#12083,#12084,#7679,.T.);
#15179=EDGE_CURVE('',#12081,#12084,#7680,.T.);
#15180=EDGE_CURVE('',#12084,#12079,#6158,.T.);
#15181=EDGE_CURVE('',#12085,#12086,#7681,.T.);
#15182=EDGE_CURVE('',#12085,#12087,#7682,.T.);
#15183=EDGE_CURVE('',#12088,#12087,#7683,.T.);
#15184=EDGE_CURVE('',#12086,#12088,#7684,.T.);
#15185=EDGE_CURVE('',#12086,#12089,#6159,.T.);
#15186=EDGE_CURVE('',#12088,#12089,#7685,.T.);
#15187=EDGE_CURVE('',#12089,#12090,#7686,.T.);
#15188=EDGE_CURVE('',#12087,#12090,#7687,.T.);
#15189=EDGE_CURVE('',#12090,#12085,#6160,.T.);
#15190=EDGE_CURVE('',#12091,#12092,#6161,.T.);
#15191=EDGE_CURVE('',#12091,#12093,#7688,.T.);
#15192=EDGE_CURVE('',#12093,#12092,#7689,.T.);
#15193=EDGE_CURVE('',#12094,#12091,#7690,.T.);
#15194=EDGE_CURVE('',#12094,#12095,#7691,.T.);
#15195=EDGE_CURVE('',#12093,#12095,#7692,.T.);
#15196=EDGE_CURVE('',#12092,#12096,#7693,.T.);
#15197=EDGE_CURVE('',#12095,#12096,#7694,.T.);
#15198=EDGE_CURVE('',#12096,#12094,#6162,.T.);
#15199=EDGE_CURVE('',#12097,#12098,#7695,.T.);
#15200=EDGE_CURVE('',#12097,#12099,#7696,.T.);
#15201=EDGE_CURVE('',#12100,#12099,#7697,.T.);
#15202=EDGE_CURVE('',#12098,#12100,#7698,.T.);
#15203=EDGE_CURVE('',#12098,#12101,#6163,.T.);
#15204=EDGE_CURVE('',#12100,#12101,#7699,.T.);
#15205=EDGE_CURVE('',#12101,#12102,#7700,.T.);
#15206=EDGE_CURVE('',#12099,#12102,#7701,.T.);
#15207=EDGE_CURVE('',#12102,#12097,#6164,.T.);
#15208=EDGE_CURVE('',#12103,#12104,#7702,.T.);
#15209=EDGE_CURVE('',#12103,#12105,#7703,.T.);
#15210=EDGE_CURVE('',#12106,#12105,#7704,.T.);
#15211=EDGE_CURVE('',#12104,#12106,#7705,.T.);
#15212=EDGE_CURVE('',#12104,#12107,#6165,.T.);
#15213=EDGE_CURVE('',#12106,#12107,#7706,.T.);
#15214=EDGE_CURVE('',#12107,#12108,#7707,.T.);
#15215=EDGE_CURVE('',#12105,#12108,#7708,.T.);
#15216=EDGE_CURVE('',#12108,#12103,#6166,.T.);
#15217=EDGE_CURVE('',#12109,#12110,#7709,.T.);
#15218=EDGE_CURVE('',#12109,#12111,#7710,.T.);
#15219=EDGE_CURVE('',#12112,#12111,#7711,.T.);
#15220=EDGE_CURVE('',#12110,#12112,#7712,.T.);
#15221=EDGE_CURVE('',#12110,#12113,#6167,.T.);
#15222=EDGE_CURVE('',#12112,#12113,#7713,.T.);
#15223=EDGE_CURVE('',#12113,#12114,#7714,.T.);
#15224=EDGE_CURVE('',#12111,#12114,#7715,.T.);
#15225=EDGE_CURVE('',#12114,#12109,#6168,.T.);
#15226=EDGE_CURVE('',#12115,#12116,#7716,.T.);
#15227=EDGE_CURVE('',#12115,#12117,#7717,.T.);
#15228=EDGE_CURVE('',#12118,#12117,#7718,.T.);
#15229=EDGE_CURVE('',#12116,#12118,#7719,.T.);
#15230=EDGE_CURVE('',#12116,#12119,#6169,.T.);
#15231=EDGE_CURVE('',#12118,#12119,#7720,.T.);
#15232=EDGE_CURVE('',#12119,#12120,#7721,.T.);
#15233=EDGE_CURVE('',#12117,#12120,#7722,.T.);
#15234=EDGE_CURVE('',#12120,#12115,#6170,.T.);
#15235=EDGE_CURVE('',#12121,#12122,#7723,.T.);
#15236=EDGE_CURVE('',#12121,#12123,#7724,.T.);
#15237=EDGE_CURVE('',#12124,#12123,#7725,.T.);
#15238=EDGE_CURVE('',#12122,#12124,#7726,.T.);
#15239=EDGE_CURVE('',#12122,#12125,#6171,.T.);
#15240=EDGE_CURVE('',#12124,#12125,#7727,.T.);
#15241=EDGE_CURVE('',#12125,#12126,#7728,.T.);
#15242=EDGE_CURVE('',#12123,#12126,#7729,.T.);
#15243=EDGE_CURVE('',#12126,#12121,#6172,.T.);
#15244=EDGE_CURVE('',#12127,#12128,#7730,.T.);
#15245=EDGE_CURVE('',#12127,#12129,#7731,.T.);
#15246=EDGE_CURVE('',#12130,#12129,#7732,.T.);
#15247=EDGE_CURVE('',#12128,#12130,#7733,.T.);
#15248=EDGE_CURVE('',#12128,#12131,#6173,.T.);
#15249=EDGE_CURVE('',#12130,#12131,#7734,.T.);
#15250=EDGE_CURVE('',#12131,#12132,#7735,.T.);
#15251=EDGE_CURVE('',#12129,#12132,#7736,.T.);
#15252=EDGE_CURVE('',#12132,#12127,#6174,.T.);
#15253=EDGE_CURVE('',#12133,#12134,#7737,.T.);
#15254=EDGE_CURVE('',#12133,#12135,#7738,.T.);
#15255=EDGE_CURVE('',#12136,#12135,#7739,.T.);
#15256=EDGE_CURVE('',#12134,#12136,#7740,.T.);
#15257=EDGE_CURVE('',#12134,#12137,#6175,.T.);
#15258=EDGE_CURVE('',#12136,#12137,#7741,.T.);
#15259=EDGE_CURVE('',#12137,#12138,#7742,.T.);
#15260=EDGE_CURVE('',#12135,#12138,#7743,.T.);
#15261=EDGE_CURVE('',#12138,#12133,#6176,.T.);
#15262=EDGE_CURVE('',#12139,#12140,#7744,.T.);
#15263=EDGE_CURVE('',#12139,#12141,#7745,.T.);
#15264=EDGE_CURVE('',#12142,#12141,#7746,.T.);
#15265=EDGE_CURVE('',#12140,#12142,#7747,.T.);
#15266=EDGE_CURVE('',#12140,#12143,#6177,.T.);
#15267=EDGE_CURVE('',#12142,#12143,#7748,.T.);
#15268=EDGE_CURVE('',#12143,#12144,#7749,.T.);
#15269=EDGE_CURVE('',#12141,#12144,#7750,.T.);
#15270=EDGE_CURVE('',#12144,#12139,#6178,.T.);
#15271=EDGE_CURVE('',#12145,#12146,#7751,.T.);
#15272=EDGE_CURVE('',#12145,#12147,#7752,.T.);
#15273=EDGE_CURVE('',#12148,#12147,#7753,.T.);
#15274=EDGE_CURVE('',#12146,#12148,#7754,.T.);
#15275=EDGE_CURVE('',#12146,#12149,#6179,.T.);
#15276=EDGE_CURVE('',#12148,#12149,#7755,.T.);
#15277=EDGE_CURVE('',#12149,#12150,#7756,.T.);
#15278=EDGE_CURVE('',#12147,#12150,#7757,.T.);
#15279=EDGE_CURVE('',#12150,#12145,#6180,.T.);
#15280=EDGE_CURVE('',#12151,#12151,#6181,.T.);
#15281=EDGE_CURVE('',#11916,#12151,#7758,.T.);
#15282=EDGE_CURVE('',#12152,#12152,#6182,.T.);
#15283=EDGE_CURVE('',#12152,#11919,#7759,.T.);
#15284=EDGE_CURVE('',#12143,#11934,#6183,.T.);
#15285=EDGE_CURVE('',#11943,#12140,#6184,.T.);
#15286=EDGE_CURVE('',#12137,#11940,#6185,.T.);
#15287=EDGE_CURVE('',#11949,#12134,#6186,.T.);
#15288=EDGE_CURVE('',#12131,#11946,#6187,.T.);
#15289=EDGE_CURVE('',#11955,#12128,#6188,.T.);
#15290=EDGE_CURVE('',#12125,#11952,#6189,.T.);
#15291=EDGE_CURVE('',#11961,#12122,#6190,.T.);
#15292=EDGE_CURVE('',#12119,#11958,#6191,.T.);
#15293=EDGE_CURVE('',#11967,#12116,#6192,.T.);
#15294=EDGE_CURVE('',#12113,#11964,#6193,.T.);
#15295=EDGE_CURVE('',#11973,#12110,#6194,.T.);
#15296=EDGE_CURVE('',#12107,#11970,#6195,.T.);
#15297=EDGE_CURVE('',#11979,#12104,#6196,.T.);
#15298=EDGE_CURVE('',#12101,#11976,#6197,.T.);
#15299=EDGE_CURVE('',#11986,#12098,#6198,.T.);
#15300=EDGE_CURVE('',#11988,#12152,#7760,.T.);
#15301=EDGE_CURVE('',#11993,#11982,#6199,.T.);
#15302=EDGE_CURVE('',#12089,#11990,#6200,.T.);
#15303=EDGE_CURVE('',#11999,#12086,#6201,.T.);
#15304=EDGE_CURVE('',#12083,#11996,#6202,.T.);
#15305=EDGE_CURVE('',#12005,#12080,#6203,.T.);
#15306=EDGE_CURVE('',#12077,#12002,#6204,.T.);
#15307=EDGE_CURVE('',#12011,#12074,#6205,.T.);
#15308=EDGE_CURVE('',#12071,#12008,#6206,.T.);
#15309=EDGE_CURVE('',#12017,#12068,#6207,.T.);
#15310=EDGE_CURVE('',#12065,#12014,#6208,.T.);
#15311=EDGE_CURVE('',#12023,#12062,#6209,.T.);
#15312=EDGE_CURVE('',#12059,#12020,#6210,.T.);
#15313=EDGE_CURVE('',#12029,#12056,#6211,.T.);
#15314=EDGE_CURVE('',#12053,#12026,#6212,.T.);
#15315=EDGE_CURVE('',#12035,#12050,#6213,.T.);
#15316=EDGE_CURVE('',#12047,#12032,#6214,.T.);
#15317=EDGE_CURVE('',#12041,#12044,#6215,.T.);
#15318=EDGE_CURVE('',#12092,#12038,#6216,.T.);
#15319=EDGE_CURVE('',#12149,#12091,#6217,.T.);
#15320=EDGE_CURVE('',#11937,#12146,#6218,.T.);
#15321=EDGE_CURVE('',#12153,#12153,#6219,.T.);
#15322=EDGE_CURVE('',#12153,#11985,#7761,.T.);
#15323=EDGE_CURVE('',#12154,#12155,#7762,.T.);
#15324=EDGE_CURVE('',#12155,#12156,#7763,.T.);
#15325=EDGE_CURVE('',#12156,#12157,#7764,.T.);
#15326=EDGE_CURVE('',#12157,#12154,#7765,.T.);
#15327=EDGE_CURVE('',#12158,#12159,#7766,.T.);
#15328=EDGE_CURVE('',#12159,#12155,#6220,.T.);
#15329=EDGE_CURVE('',#12154,#12158,#6221,.T.);
#15330=EDGE_CURVE('',#12160,#12161,#7767,.T.);
#15331=EDGE_CURVE('',#12161,#12159,#7768,.T.);
#15332=EDGE_CURVE('',#12158,#12160,#7769,.T.);
#15333=EDGE_CURVE('',#12156,#12161,#6222,.T.);
#15334=EDGE_CURVE('',#12160,#12157,#6223,.T.);
#15335=EDGE_CURVE('',#12156,#12162,#7770,.T.);
#15336=EDGE_CURVE('',#12163,#12162,#6224,.T.);
#15337=EDGE_CURVE('',#12161,#12163,#7771,.T.);
#15338=EDGE_CURVE('',#12155,#12164,#7772,.T.);
#15339=EDGE_CURVE('',#12162,#12164,#7773,.T.);
#15340=EDGE_CURVE('',#12164,#12165,#7774,.T.);
#15341=EDGE_CURVE('',#12165,#12166,#7775,.T.);
#15342=EDGE_CURVE('',#12166,#12162,#7776,.T.);
#15343=EDGE_CURVE('',#12167,#12168,#7777,.T.);
#15344=EDGE_CURVE('',#12168,#12165,#6225,.T.);
#15345=EDGE_CURVE('',#12164,#12167,#6226,.T.);
#15346=EDGE_CURVE('',#12163,#12169,#7778,.T.);
#15347=EDGE_CURVE('',#12169,#12168,#7779,.T.);
#15348=EDGE_CURVE('',#12167,#12163,#7780,.T.);
#15349=EDGE_CURVE('',#12166,#12169,#6227,.T.);
#15350=EDGE_CURVE('',#12159,#12167,#7781,.T.);
#15351=EDGE_CURVE('',#12170,#12171,#7782,.T.);
#15352=EDGE_CURVE('',#12170,#12172,#511,.T.);
#15353=EDGE_CURVE('',#12172,#12173,#6228,.T.);
#15354=EDGE_CURVE('',#12173,#12171,#512,.T.);
#15355=EDGE_CURVE('',#12174,#12175,#7783,.T.);
#15356=EDGE_CURVE('',#12174,#12170,#513,.T.);
#15357=EDGE_CURVE('',#12171,#12175,#514,.T.);
#15358=EDGE_CURVE('',#12176,#12177,#7784,.T.);
#15359=EDGE_CURVE('',#12176,#12174,#515,.T.);
#15360=EDGE_CURVE('',#12175,#12177,#516,.T.);
#15361=EDGE_CURVE('',#12178,#12179,#7785,.T.);
#15362=EDGE_CURVE('',#12178,#12176,#517,.T.);
#15363=EDGE_CURVE('',#12177,#12179,#518,.T.);
#15364=EDGE_CURVE('',#12180,#12181,#7786,.T.);
#15365=EDGE_CURVE('',#12180,#12178,#519,.T.);
#15366=EDGE_CURVE('',#12179,#12181,#520,.T.);
#15367=EDGE_CURVE('',#12182,#12183,#7787,.T.);
#15368=EDGE_CURVE('',#12182,#12180,#521,.T.);
#15369=EDGE_CURVE('',#12181,#12183,#522,.T.);
#15370=EDGE_CURVE('',#12184,#12185,#7788,.T.);
#15371=EDGE_CURVE('',#12184,#12182,#523,.T.);
#15372=EDGE_CURVE('',#12183,#12185,#524,.T.);
#15373=EDGE_CURVE('',#12186,#12187,#7789,.T.);
#15374=EDGE_CURVE('',#12186,#12184,#525,.T.);
#15375=EDGE_CURVE('',#12185,#12187,#526,.T.);
#15376=EDGE_CURVE('',#12188,#12189,#7790,.T.);
#15377=EDGE_CURVE('',#12188,#12186,#527,.T.);
#15378=EDGE_CURVE('',#12187,#12189,#528,.T.);
#15379=EDGE_CURVE('',#12190,#12191,#7791,.T.);
#15380=EDGE_CURVE('',#12190,#12188,#529,.T.);
#15381=EDGE_CURVE('',#12189,#12191,#530,.T.);
#15382=EDGE_CURVE('',#12192,#12193,#7792,.T.);
#15383=EDGE_CURVE('',#12192,#12194,#531,.T.);
#15384=EDGE_CURVE('',#12195,#12194,#6229,.T.);
#15385=EDGE_CURVE('',#12193,#12195,#532,.T.);
#15386=EDGE_CURVE('',#12196,#12197,#7793,.T.);
#15387=EDGE_CURVE('',#12196,#12192,#533,.T.);
#15388=EDGE_CURVE('',#12197,#12193,#534,.T.);
#15389=EDGE_CURVE('',#12198,#12199,#7794,.T.);
#15390=EDGE_CURVE('',#12198,#12196,#535,.T.);
#15391=EDGE_CURVE('',#12199,#12197,#536,.T.);
#15392=EDGE_CURVE('',#12200,#12201,#7795,.T.);
#15393=EDGE_CURVE('',#12200,#12198,#537,.T.);
#15394=EDGE_CURVE('',#12201,#12199,#538,.T.);
#15395=EDGE_CURVE('',#12202,#12203,#7796,.T.);
#15396=EDGE_CURVE('',#12202,#12200,#539,.T.);
#15397=EDGE_CURVE('',#12203,#12201,#540,.T.);
#15398=EDGE_CURVE('',#12204,#12205,#7797,.T.);
#15399=EDGE_CURVE('',#12204,#12202,#541,.T.);
#15400=EDGE_CURVE('',#12205,#12203,#542,.T.);
#15401=EDGE_CURVE('',#12206,#12207,#7798,.T.);
#15402=EDGE_CURVE('',#12206,#12204,#543,.T.);
#15403=EDGE_CURVE('',#12207,#12205,#544,.T.);
#15404=EDGE_CURVE('',#12208,#12209,#7799,.T.);
#15405=EDGE_CURVE('',#12208,#12206,#545,.T.);
#15406=EDGE_CURVE('',#12209,#12207,#546,.T.);
#15407=EDGE_CURVE('',#12210,#12211,#7800,.T.);
#15408=EDGE_CURVE('',#12210,#12208,#547,.T.);
#15409=EDGE_CURVE('',#12211,#12209,#548,.T.);
#15410=EDGE_CURVE('',#12212,#12213,#549,.F.);
#15411=EDGE_CURVE('',#12213,#12214,#6230,.T.);
#15412=EDGE_CURVE('',#12214,#12215,#550,.F.);
#15413=EDGE_CURVE('',#12215,#12212,#6231,.T.);
#15414=EDGE_CURVE('',#12213,#12216,#551,.T.);
#15415=EDGE_CURVE('',#12216,#12217,#6232,.T.);
#15416=EDGE_CURVE('',#12217,#12218,#6233,.T.);
#15417=EDGE_CURVE('',#12218,#12214,#552,.T.);
#15418=EDGE_CURVE('',#12219,#12195,#553,.T.);
#15419=EDGE_CURVE('',#12191,#12219,#554,.T.);
#15420=EDGE_CURVE('',#12220,#12173,#555,.T.);
#15421=EDGE_CURVE('',#12220,#12211,#556,.T.);
#15422=EDGE_CURVE('',#12173,#12221,#6234,.T.);
#15423=EDGE_CURVE('',#12221,#12172,#6235,.T.);
#15424=EDGE_CURVE('',#12172,#12222,#557,.T.);
#15425=EDGE_CURVE('',#12222,#12220,#6236,.T.);
#15426=EDGE_CURVE('',#12222,#12210,#558,.T.);
#15427=EDGE_CURVE('',#12194,#12223,#559,.T.);
#15428=EDGE_CURVE('',#12223,#12190,#560,.T.);
#15429=EDGE_CURVE('',#12224,#12218,#561,.T.);
#15430=EDGE_CURVE('',#12224,#12225,#7801,.T.);
#15431=EDGE_CURVE('',#12225,#12226,#6237,.T.);
#15432=EDGE_CURVE('',#12226,#12227,#6238,.T.);
#15433=EDGE_CURVE('',#12227,#12225,#6239,.T.);
#15434=EDGE_CURVE('',#12216,#12224,#562,.T.);
#15435=EDGE_CURVE('',#12228,#12212,#1101,.T.);
#15436=EDGE_CURVE('',#12229,#12228,#6240,.T.);
#15437=EDGE_CURVE('',#12215,#12229,#1102,.T.);
#15438=EDGE_CURVE('',#12226,#12230,#6241,.T.);
#15439=EDGE_CURVE('',#12231,#12227,#6242,.T.);
#15440=EDGE_CURVE('',#12229,#12228,#7802,.T.);
#15441=EDGE_CURVE('',#12232,#12232,#6243,.T.);
#15442=EDGE_CURVE('',#12221,#12232,#7803,.T.);
#15443=EDGE_CURVE('',#12223,#12219,#6244,.T.);
#15444=EDGE_CURVE('',#12233,#12233,#6245,.T.);
#15445=EDGE_CURVE('',#12217,#12233,#7804,.T.);
#15446=EDGE_CURVE('',#12234,#12235,#563,.T.);
#15447=EDGE_CURVE('',#12235,#12234,#564,.T.);
#15448=EDGE_CURVE('',#12236,#12236,#6246,.T.);
#15449=EDGE_CURVE('',#12236,#12235,#7805,.T.);
#15450=EDGE_CURVE('',#12237,#12237,#6247,.T.);
#15451=EDGE_CURVE('',#12237,#12236,#7806,.T.);
#15452=EDGE_CURVE('',#12238,#12239,#7807,.T.);
#15453=EDGE_CURVE('',#12238,#12240,#565,.T.);
#15454=EDGE_CURVE('',#12240,#12241,#6248,.T.);
#15455=EDGE_CURVE('',#12241,#12239,#566,.T.);
#15456=EDGE_CURVE('',#12242,#12243,#7808,.T.);
#15457=EDGE_CURVE('',#12242,#12238,#567,.T.);
#15458=EDGE_CURVE('',#12239,#12243,#568,.T.);
#15459=EDGE_CURVE('',#12244,#12245,#7809,.T.);
#15460=EDGE_CURVE('',#12244,#12242,#569,.T.);
#15461=EDGE_CURVE('',#12243,#12245,#570,.T.);
#15462=EDGE_CURVE('',#12246,#12247,#7810,.T.);
#15463=EDGE_CURVE('',#12246,#12244,#571,.T.);
#15464=EDGE_CURVE('',#12245,#12247,#572,.T.);
#15465=EDGE_CURVE('',#12248,#12249,#7811,.T.);
#15466=EDGE_CURVE('',#12248,#12246,#573,.T.);
#15467=EDGE_CURVE('',#12247,#12249,#574,.T.);
#15468=EDGE_CURVE('',#12250,#12251,#7812,.T.);
#15469=EDGE_CURVE('',#12250,#12248,#575,.T.);
#15470=EDGE_CURVE('',#12249,#12251,#576,.T.);
#15471=EDGE_CURVE('',#12252,#12253,#7813,.T.);
#15472=EDGE_CURVE('',#12252,#12250,#577,.T.);
#15473=EDGE_CURVE('',#12251,#12253,#578,.T.);
#15474=EDGE_CURVE('',#12254,#12255,#7814,.T.);
#15475=EDGE_CURVE('',#12254,#12252,#579,.T.);
#15476=EDGE_CURVE('',#12253,#12255,#580,.T.);
#15477=EDGE_CURVE('',#12256,#12257,#7815,.T.);
#15478=EDGE_CURVE('',#12256,#12254,#581,.T.);
#15479=EDGE_CURVE('',#12255,#12257,#582,.T.);
#15480=EDGE_CURVE('',#12258,#12259,#7816,.T.);
#15481=EDGE_CURVE('',#12258,#12256,#583,.T.);
#15482=EDGE_CURVE('',#12257,#12259,#584,.T.);
#15483=EDGE_CURVE('',#12260,#12261,#7817,.T.);
#15484=EDGE_CURVE('',#12260,#12258,#585,.T.);
#15485=EDGE_CURVE('',#12259,#12261,#586,.T.);
#15486=EDGE_CURVE('',#12262,#12263,#7818,.T.);
#15487=EDGE_CURVE('',#12262,#12260,#587,.T.);
#15488=EDGE_CURVE('',#12261,#12263,#588,.T.);
#15489=EDGE_CURVE('',#12264,#12265,#7819,.T.);
#15490=EDGE_CURVE('',#12264,#12262,#589,.T.);
#15491=EDGE_CURVE('',#12263,#12265,#590,.T.);
#15492=EDGE_CURVE('',#12266,#12267,#7820,.T.);
#15493=EDGE_CURVE('',#12266,#12264,#591,.T.);
#15494=EDGE_CURVE('',#12265,#12267,#592,.T.);
#15495=EDGE_CURVE('',#12268,#12269,#7821,.T.);
#15496=EDGE_CURVE('',#12268,#12270,#593,.T.);
#15497=EDGE_CURVE('',#12271,#12270,#6249,.T.);
#15498=EDGE_CURVE('',#12269,#12271,#594,.T.);
#15499=EDGE_CURVE('',#12272,#12273,#7822,.T.);
#15500=EDGE_CURVE('',#12272,#12268,#595,.T.);
#15501=EDGE_CURVE('',#12273,#12269,#596,.T.);
#15502=EDGE_CURVE('',#12274,#12275,#7823,.T.);
#15503=EDGE_CURVE('',#12274,#12272,#597,.T.);
#15504=EDGE_CURVE('',#12275,#12273,#598,.T.);
#15505=EDGE_CURVE('',#12276,#12277,#7824,.T.);
#15506=EDGE_CURVE('',#12276,#12274,#599,.T.);
#15507=EDGE_CURVE('',#12277,#12275,#600,.T.);
#15508=EDGE_CURVE('',#12278,#12279,#7825,.T.);
#15509=EDGE_CURVE('',#12278,#12276,#601,.T.);
#15510=EDGE_CURVE('',#12279,#12277,#602,.T.);
#15511=EDGE_CURVE('',#12280,#12281,#7826,.T.);
#15512=EDGE_CURVE('',#12280,#12278,#603,.T.);
#15513=EDGE_CURVE('',#12281,#12279,#604,.T.);
#15514=EDGE_CURVE('',#12282,#12283,#7827,.T.);
#15515=EDGE_CURVE('',#12282,#12280,#605,.T.);
#15516=EDGE_CURVE('',#12283,#12281,#606,.T.);
#15517=EDGE_CURVE('',#12284,#12285,#7828,.T.);
#15518=EDGE_CURVE('',#12284,#12282,#607,.T.);
#15519=EDGE_CURVE('',#12285,#12283,#608,.T.);
#15520=EDGE_CURVE('',#12286,#12287,#7829,.T.);
#15521=EDGE_CURVE('',#12286,#12284,#609,.T.);
#15522=EDGE_CURVE('',#12287,#12285,#610,.T.);
#15523=EDGE_CURVE('',#12288,#12289,#7830,.T.);
#15524=EDGE_CURVE('',#12288,#12286,#611,.T.);
#15525=EDGE_CURVE('',#12289,#12287,#612,.T.);
#15526=EDGE_CURVE('',#12290,#12291,#7831,.T.);
#15527=EDGE_CURVE('',#12290,#12288,#613,.T.);
#15528=EDGE_CURVE('',#12291,#12289,#614,.T.);
#15529=EDGE_CURVE('',#12292,#12293,#7832,.T.);
#15530=EDGE_CURVE('',#12292,#12290,#615,.T.);
#15531=EDGE_CURVE('',#12293,#12291,#616,.T.);
#15532=EDGE_CURVE('',#12294,#12295,#7833,.T.);
#15533=EDGE_CURVE('',#12294,#12292,#617,.T.);
#15534=EDGE_CURVE('',#12295,#12293,#618,.T.);
#15535=EDGE_CURVE('',#12296,#12297,#7834,.T.);
#15536=EDGE_CURVE('',#12296,#12294,#619,.T.);
#15537=EDGE_CURVE('',#12297,#12295,#620,.T.);
#15538=EDGE_CURVE('',#12298,#12271,#621,.T.);
#15539=EDGE_CURVE('',#12267,#12298,#622,.T.);
#15540=EDGE_CURVE('',#12299,#12241,#623,.T.);
#15541=EDGE_CURVE('',#12299,#12297,#624,.T.);
#15542=EDGE_CURVE('',#12241,#12300,#6250,.T.);
#15543=EDGE_CURVE('',#12300,#12240,#6251,.T.);
#15544=EDGE_CURVE('',#12240,#12301,#625,.T.);
#15545=EDGE_CURVE('',#12301,#12299,#6252,.T.);
#15546=EDGE_CURVE('',#12301,#12296,#626,.T.);
#15547=EDGE_CURVE('',#12270,#12302,#627,.T.);
#15548=EDGE_CURVE('',#12302,#12266,#628,.T.);
#15549=EDGE_CURVE('',#12302,#12298,#6253,.F.);
#15550=EDGE_CURVE('',#12303,#12303,#6254,.T.);
#15551=EDGE_CURVE('',#12304,#12305,#7835,.T.);
#15552=EDGE_CURVE('',#12304,#12306,#7836,.T.);
#15553=EDGE_CURVE('',#12306,#12307,#7837,.T.);
#15554=EDGE_CURVE('',#12305,#12307,#7838,.T.);
#15555=EDGE_CURVE('',#12308,#12304,#7839,.T.);
#15556=EDGE_CURVE('',#12308,#12309,#7840,.T.);
#15557=EDGE_CURVE('',#12309,#12306,#7841,.T.);
#15558=EDGE_CURVE('',#12310,#12308,#7842,.T.);
#15559=EDGE_CURVE('',#12310,#12311,#7843,.T.);
#15560=EDGE_CURVE('',#12311,#12309,#7844,.T.);
#15561=EDGE_CURVE('',#12312,#12310,#7845,.T.);
#15562=EDGE_CURVE('',#12312,#12313,#7846,.T.);
#15563=EDGE_CURVE('',#12313,#12311,#7847,.T.);
#15564=EDGE_CURVE('',#12314,#12312,#7848,.T.);
#15565=EDGE_CURVE('',#12314,#12315,#7849,.T.);
#15566=EDGE_CURVE('',#12315,#12313,#7850,.T.);
#15567=EDGE_CURVE('',#12305,#12314,#7851,.T.);
#15568=EDGE_CURVE('',#12307,#12315,#7852,.T.);
#15569=EDGE_CURVE('',#12316,#12316,#6255,.T.);
#15570=EDGE_CURVE('',#12300,#12316,#7853,.T.);
#15571=EDGE_CURVE('',#12317,#12317,#6256,.T.);
#15572=EDGE_CURVE('',#12317,#12303,#7854,.T.);
#15573=EDGE_CURVE('',#12318,#12318,#6257,.T.);
#15574=EDGE_CURVE('',#12318,#12317,#7855,.T.);
#15575=EDGE_CURVE('',#12319,#12320,#7856,.T.);
#15576=EDGE_CURVE('',#12320,#12321,#7857,.T.);
#15577=EDGE_CURVE('',#12321,#12322,#7858,.T.);
#15578=EDGE_CURVE('',#12322,#12323,#7859,.T.);
#15579=EDGE_CURVE('',#12323,#12324,#7860,.T.);
#15580=EDGE_CURVE('',#12324,#12319,#7861,.T.);
#15581=EDGE_CURVE('',#12325,#12320,#7862,.T.);
#15582=EDGE_CURVE('',#12326,#12325,#7863,.T.);
#15583=EDGE_CURVE('',#12321,#12326,#7864,.T.);
#15584=EDGE_CURVE('',#12327,#12319,#7865,.T.);
#15585=EDGE_CURVE('',#12327,#12328,#7866,.T.);
#15586=EDGE_CURVE('',#12328,#12329,#7867,.T.);
#15587=EDGE_CURVE('',#12325,#12329,#7868,.T.);
#15588=EDGE_CURVE('',#12324,#12330,#7869,.T.);
#15589=EDGE_CURVE('',#12331,#12330,#7870,.T.);
#15590=EDGE_CURVE('',#12332,#12331,#7871,.T.);
#15591=EDGE_CURVE('',#12332,#12327,#7872,.T.);
#15592=EDGE_CURVE('',#12329,#12333,#7873,.T.);
#15593=EDGE_CURVE('',#12333,#12334,#7874,.T.);
#15594=EDGE_CURVE('',#12334,#12335,#7875,.T.);
#15595=EDGE_CURVE('',#12335,#12326,#7876,.T.);
#15596=EDGE_CURVE('',#12334,#12336,#7877,.T.);
#15597=EDGE_CURVE('',#12337,#12336,#7878,.T.);
#15598=EDGE_CURVE('',#12338,#12337,#7879,.T.);
#15599=EDGE_CURVE('',#12338,#12339,#7880,.T.);
#15600=EDGE_CURVE('',#12339,#12335,#7881,.T.);
#15601=EDGE_CURVE('',#12340,#12333,#7882,.T.);
#15602=EDGE_CURVE('',#12336,#12340,#7883,.T.);
#15603=EDGE_CURVE('',#12328,#12341,#7884,.T.);
#15604=EDGE_CURVE('',#12341,#12342,#7885,.T.);
#15605=EDGE_CURVE('',#12340,#12342,#7886,.T.);
#15606=EDGE_CURVE('',#12330,#12343,#7887,.T.);
#15607=EDGE_CURVE('',#12343,#12344,#7888,.T.);
#15608=EDGE_CURVE('',#12344,#12345,#7889,.T.);
#15609=EDGE_CURVE('',#12345,#12346,#7890,.T.);
#15610=EDGE_CURVE('',#12346,#12331,#7891,.T.);
#15611=EDGE_CURVE('',#12347,#12345,#7892,.T.);
#15612=EDGE_CURVE('',#12348,#12347,#7893,.T.);
#15613=EDGE_CURVE('',#12346,#12348,#7894,.T.);
#15614=EDGE_CURVE('',#12349,#12344,#7895,.T.);
#15615=EDGE_CURVE('',#12349,#12338,#7896,.T.);
#15616=EDGE_CURVE('',#12347,#12337,#7897,.T.);
#15617=EDGE_CURVE('',#12322,#12350,#7898,.T.);
#15618=EDGE_CURVE('',#12350,#12349,#7899,.T.);
#15619=EDGE_CURVE('',#12343,#12323,#7900,.T.);
#15620=EDGE_CURVE('',#12342,#12348,#7901,.T.);
#15621=EDGE_CURVE('',#12339,#12350,#7902,.T.);
#15622=EDGE_CURVE('',#12341,#12332,#7903,.T.);
#15623=EDGE_CURVE('',#12351,#12352,#7904,.T.);
#15624=EDGE_CURVE('',#12351,#12353,#629,.T.);
#15625=EDGE_CURVE('',#12353,#12354,#6258,.T.);
#15626=EDGE_CURVE('',#12354,#12352,#630,.T.);
#15627=EDGE_CURVE('',#12355,#12356,#7905,.T.);
#15628=EDGE_CURVE('',#12355,#12351,#631,.T.);
#15629=EDGE_CURVE('',#12352,#12356,#632,.T.);
#15630=EDGE_CURVE('',#12357,#12358,#7906,.T.);
#15631=EDGE_CURVE('',#12357,#12355,#633,.T.);
#15632=EDGE_CURVE('',#12356,#12358,#634,.T.);
#15633=EDGE_CURVE('',#12359,#12360,#7907,.T.);
#15634=EDGE_CURVE('',#12359,#12357,#635,.T.);
#15635=EDGE_CURVE('',#12358,#12360,#636,.T.);
#15636=EDGE_CURVE('',#12361,#12362,#7908,.T.);
#15637=EDGE_CURVE('',#12361,#12359,#637,.T.);
#15638=EDGE_CURVE('',#12360,#12362,#638,.T.);
#15639=EDGE_CURVE('',#12363,#12364,#7909,.T.);
#15640=EDGE_CURVE('',#12363,#12361,#639,.T.);
#15641=EDGE_CURVE('',#12362,#12364,#640,.T.);
#15642=EDGE_CURVE('',#12365,#12366,#7910,.T.);
#15643=EDGE_CURVE('',#12365,#12363,#641,.T.);
#15644=EDGE_CURVE('',#12364,#12366,#642,.T.);
#15645=EDGE_CURVE('',#12367,#12368,#7911,.T.);
#15646=EDGE_CURVE('',#12367,#12365,#643,.T.);
#15647=EDGE_CURVE('',#12366,#12368,#644,.T.);
#15648=EDGE_CURVE('',#12369,#12370,#7912,.T.);
#15649=EDGE_CURVE('',#12369,#12367,#645,.T.);
#15650=EDGE_CURVE('',#12368,#12370,#646,.T.);
#15651=EDGE_CURVE('',#12371,#12372,#7913,.T.);
#15652=EDGE_CURVE('',#12371,#12369,#647,.T.);
#15653=EDGE_CURVE('',#12370,#12372,#648,.T.);
#15654=EDGE_CURVE('',#12373,#12374,#7914,.T.);
#15655=EDGE_CURVE('',#12373,#12371,#649,.T.);
#15656=EDGE_CURVE('',#12372,#12374,#650,.T.);
#15657=EDGE_CURVE('',#12375,#12376,#7915,.T.);
#15658=EDGE_CURVE('',#12375,#12373,#651,.T.);
#15659=EDGE_CURVE('',#12374,#12376,#652,.T.);
#15660=EDGE_CURVE('',#12377,#12378,#7916,.T.);
#15661=EDGE_CURVE('',#12377,#12375,#653,.T.);
#15662=EDGE_CURVE('',#12376,#12378,#654,.T.);
#15663=EDGE_CURVE('',#12379,#12380,#7917,.T.);
#15664=EDGE_CURVE('',#12379,#12377,#655,.T.);
#15665=EDGE_CURVE('',#12378,#12380,#656,.T.);
#15666=EDGE_CURVE('',#12381,#12382,#7918,.T.);
#15667=EDGE_CURVE('',#12381,#12379,#657,.T.);
#15668=EDGE_CURVE('',#12380,#12382,#658,.T.);
#15669=EDGE_CURVE('',#12383,#12384,#7919,.T.);
#15670=EDGE_CURVE('',#12383,#12381,#659,.T.);
#15671=EDGE_CURVE('',#12382,#12384,#660,.T.);
#15672=EDGE_CURVE('',#12385,#12386,#7920,.T.);
#15673=EDGE_CURVE('',#12385,#12383,#661,.T.);
#15674=EDGE_CURVE('',#12384,#12386,#662,.T.);
#15675=EDGE_CURVE('',#12387,#12388,#7921,.T.);
#15676=EDGE_CURVE('',#12387,#12385,#663,.T.);
#15677=EDGE_CURVE('',#12386,#12388,#664,.T.);
#15678=EDGE_CURVE('',#12389,#12390,#7922,.T.);
#15679=EDGE_CURVE('',#12389,#12387,#665,.T.);
#15680=EDGE_CURVE('',#12388,#12390,#666,.T.);
#15681=EDGE_CURVE('',#12391,#12392,#7923,.T.);
#15682=EDGE_CURVE('',#12391,#12389,#667,.T.);
#15683=EDGE_CURVE('',#12390,#12392,#668,.T.);
#15684=EDGE_CURVE('',#12393,#12394,#7924,.T.);
#15685=EDGE_CURVE('',#12393,#12395,#669,.T.);
#15686=EDGE_CURVE('',#12394,#12395,#6259,.T.);
#15687=EDGE_CURVE('',#12396,#12397,#7925,.T.);
#15688=EDGE_CURVE('',#12396,#12393,#670,.T.);
#15689=EDGE_CURVE('',#12398,#12394,#6260,.T.);
#15690=EDGE_CURVE('',#12397,#12398,#671,.T.);
#15691=EDGE_CURVE('',#12399,#12400,#7926,.T.);
#15692=EDGE_CURVE('',#12399,#12396,#672,.T.);
#15693=EDGE_CURVE('',#12400,#12397,#673,.T.);
#15694=EDGE_CURVE('',#12401,#12402,#7927,.T.);
#15695=EDGE_CURVE('',#12401,#12399,#674,.T.);
#15696=EDGE_CURVE('',#12402,#12400,#675,.T.);
#15697=EDGE_CURVE('',#12403,#12404,#7928,.T.);
#15698=EDGE_CURVE('',#12403,#12401,#676,.T.);
#15699=EDGE_CURVE('',#12404,#12402,#677,.T.);
#15700=EDGE_CURVE('',#12405,#12406,#7929,.T.);
#15701=EDGE_CURVE('',#12405,#12403,#678,.T.);
#15702=EDGE_CURVE('',#12406,#12404,#679,.T.);
#15703=EDGE_CURVE('',#12407,#12408,#7930,.T.);
#15704=EDGE_CURVE('',#12407,#12405,#680,.T.);
#15705=EDGE_CURVE('',#12408,#12406,#681,.T.);
#15706=EDGE_CURVE('',#12409,#12410,#7931,.T.);
#15707=EDGE_CURVE('',#12409,#12407,#682,.T.);
#15708=EDGE_CURVE('',#12410,#12408,#683,.T.);
#15709=EDGE_CURVE('',#12411,#12412,#7932,.T.);
#15710=EDGE_CURVE('',#12411,#12409,#684,.T.);
#15711=EDGE_CURVE('',#12412,#12410,#685,.T.);
#15712=EDGE_CURVE('',#12413,#12414,#7933,.T.);
#15713=EDGE_CURVE('',#12413,#12411,#686,.T.);
#15714=EDGE_CURVE('',#12414,#12412,#687,.T.);
#15715=EDGE_CURVE('',#12415,#12416,#7934,.T.);
#15716=EDGE_CURVE('',#12415,#12413,#688,.T.);
#15717=EDGE_CURVE('',#12416,#12414,#689,.T.);
#15718=EDGE_CURVE('',#12417,#12418,#7935,.T.);
#15719=EDGE_CURVE('',#12417,#12415,#690,.T.);
#15720=EDGE_CURVE('',#12418,#12416,#691,.T.);
#15721=EDGE_CURVE('',#12419,#12420,#7936,.T.);
#15722=EDGE_CURVE('',#12419,#12417,#692,.T.);
#15723=EDGE_CURVE('',#12420,#12418,#693,.T.);
#15724=EDGE_CURVE('',#12421,#12422,#7937,.T.);
#15725=EDGE_CURVE('',#12421,#12419,#694,.T.);
#15726=EDGE_CURVE('',#12422,#12420,#695,.T.);
#15727=EDGE_CURVE('',#12423,#12424,#7938,.T.);
#15728=EDGE_CURVE('',#12423,#12421,#696,.T.);
#15729=EDGE_CURVE('',#12424,#12422,#697,.T.);
#15730=EDGE_CURVE('',#12425,#12426,#7939,.T.);
#15731=EDGE_CURVE('',#12425,#12423,#698,.T.);
#15732=EDGE_CURVE('',#12426,#12424,#699,.T.);
#15733=EDGE_CURVE('',#12427,#12428,#7940,.T.);
#15734=EDGE_CURVE('',#12427,#12425,#700,.T.);
#15735=EDGE_CURVE('',#12428,#12426,#701,.T.);
#15736=EDGE_CURVE('',#12429,#12430,#7941,.T.);
#15737=EDGE_CURVE('',#12429,#12427,#702,.T.);
#15738=EDGE_CURVE('',#12430,#12428,#703,.T.);
#15739=EDGE_CURVE('',#12431,#12432,#7942,.T.);
#15740=EDGE_CURVE('',#12431,#12429,#704,.T.);
#15741=EDGE_CURVE('',#12432,#12430,#705,.T.);
#15742=EDGE_CURVE('',#12433,#12434,#7943,.T.);
#15743=EDGE_CURVE('',#12433,#12431,#706,.T.);
#15744=EDGE_CURVE('',#12434,#12432,#707,.T.);
#15745=EDGE_CURVE('',#12435,#12398,#708,.T.);
#15746=EDGE_CURVE('',#12392,#12435,#709,.T.);
#15747=EDGE_CURVE('',#12436,#12354,#710,.T.);
#15748=EDGE_CURVE('',#12436,#12434,#711,.T.);
#15749=EDGE_CURVE('',#12354,#12437,#6261,.T.);
#15750=EDGE_CURVE('',#12437,#12353,#6262,.T.);
#15751=EDGE_CURVE('',#12353,#12438,#712,.T.);
#15752=EDGE_CURVE('',#12438,#12436,#6263,.T.);
#15753=EDGE_CURVE('',#12438,#12433,#713,.T.);
#15754=EDGE_CURVE('',#12395,#12439,#714,.T.);
#15755=EDGE_CURVE('',#12439,#12391,#715,.T.);
#15756=EDGE_CURVE('',#12440,#12441,#123,.T.);
#15757=EDGE_CURVE('',#12442,#12440,#124,.T.);
#15758=EDGE_CURVE('',#12443,#12442,#125,.T.);
#15759=EDGE_CURVE('',#12444,#12443,#126,.T.);
#15760=EDGE_CURVE('',#12445,#12444,#127,.T.);
#15761=EDGE_CURVE('',#12445,#12446,#7944,.T.);
#15762=EDGE_CURVE('',#12446,#12446,#6264,.T.);
#15763=EDGE_CURVE('',#12447,#12445,#128,.T.);
#15764=EDGE_CURVE('',#12441,#12447,#129,.T.);
#15765=EDGE_CURVE('',#12448,#12443,#7945,.T.);
#15766=EDGE_CURVE('',#12448,#12449,#7946,.T.);
#15767=EDGE_CURVE('',#12449,#12444,#7947,.T.);
#15768=EDGE_CURVE('',#12450,#12442,#7948,.T.);
#15769=EDGE_CURVE('',#12450,#12448,#7949,.T.);
#15770=EDGE_CURVE('',#12451,#12440,#7950,.T.);
#15771=EDGE_CURVE('',#12451,#12450,#7951,.T.);
#15772=EDGE_CURVE('',#12452,#12451,#7952,.T.);
#15773=EDGE_CURVE('',#12453,#12452,#7953,.T.);
#15774=EDGE_CURVE('',#12449,#12453,#7954,.T.);
#15775=EDGE_CURVE('',#12454,#12454,#6265,.T.);
#15776=EDGE_CURVE('',#12452,#12441,#7955,.T.);
#15777=EDGE_CURVE('',#12453,#12447,#7956,.T.);
#15778=EDGE_CURVE('',#12455,#12455,#6266,.T.);
#15779=EDGE_CURVE('',#12437,#12455,#7957,.T.);
#15780=EDGE_CURVE('',#12439,#12435,#6267,.T.);
#15781=EDGE_CURVE('',#12456,#12456,#6268,.T.);
#15782=EDGE_CURVE('',#12454,#12456,#7958,.T.);
#15783=EDGE_CURVE('',#12457,#12457,#6269,.T.);
#15784=EDGE_CURVE('',#12457,#12458,#7959,.T.);
#15785=EDGE_CURVE('',#12458,#12458,#6270,.T.);
#15786=EDGE_CURVE('',#12457,#12459,#7960,.T.);
#15787=EDGE_CURVE('',#12459,#12459,#6271,.T.);
#15788=EDGE_CURVE('',#12460,#12461,#7961,.T.);
#15789=EDGE_CURVE('',#12462,#12460,#6272,.T.);
#15790=EDGE_CURVE('',#12463,#12462,#7962,.T.);
#15791=EDGE_CURVE('',#12464,#12463,#6273,.T.);
#15792=EDGE_CURVE('',#12465,#12464,#7963,.T.);
#15793=EDGE_CURVE('',#12466,#12465,#6274,.T.);
#15794=EDGE_CURVE('',#12467,#12466,#7964,.T.);
#15795=EDGE_CURVE('',#12461,#12467,#6275,.T.);
#15796=EDGE_CURVE('',#12459,#12468,#7965,.T.);
#15797=EDGE_CURVE('',#12468,#12468,#6276,.T.);
#15798=EDGE_CURVE('',#12469,#12469,#6277,.T.);
#15799=EDGE_CURVE('',#12469,#12468,#7966,.T.);
#15800=EDGE_CURVE('',#12470,#12470,#6278,.T.);
#15801=EDGE_CURVE('',#12470,#12469,#7967,.T.);
#15802=EDGE_CURVE('',#12471,#12471,#6279,.T.);
#15803=EDGE_CURVE('',#12471,#12470,#7968,.T.);
#15804=EDGE_CURVE('',#12471,#12472,#7969,.T.);
#15805=EDGE_CURVE('',#12472,#12472,#6280,.T.);
#15806=EDGE_CURVE('',#12473,#12474,#7970,.T.);
#15807=EDGE_CURVE('',#12475,#12473,#6281,.T.);
#15808=EDGE_CURVE('',#12476,#12475,#7971,.T.);
#15809=EDGE_CURVE('',#12477,#12476,#6282,.T.);
#15810=EDGE_CURVE('',#12478,#12477,#7972,.T.);
#15811=EDGE_CURVE('',#12479,#12478,#6283,.T.);
#15812=EDGE_CURVE('',#12480,#12479,#7973,.T.);
#15813=EDGE_CURVE('',#12474,#12480,#6284,.T.);
#15814=EDGE_CURVE('',#12481,#12482,#7974,.T.);
#15815=EDGE_CURVE('',#12482,#12483,#6285,.T.);
#15816=EDGE_CURVE('',#12483,#12484,#7975,.T.);
#15817=EDGE_CURVE('',#12484,#12481,#6286,.T.);
#15818=EDGE_CURVE('',#12485,#12486,#7976,.T.);
#15819=EDGE_CURVE('',#12486,#12482,#7977,.T.);
#15820=EDGE_CURVE('',#12481,#12485,#7978,.T.);
#15821=EDGE_CURVE('',#12487,#12488,#7979,.T.);
#15822=EDGE_CURVE('',#12488,#12486,#6287,.T.);
#15823=EDGE_CURVE('',#12485,#12487,#6288,.T.);
#15824=EDGE_CURVE('',#12489,#12490,#7980,.T.);
#15825=EDGE_CURVE('',#12490,#12488,#7981,.T.);
#15826=EDGE_CURVE('',#12487,#12489,#7982,.T.);
#15827=EDGE_CURVE('',#12491,#12492,#7983,.T.);
#15828=EDGE_CURVE('',#12492,#12490,#6289,.T.);
#15829=EDGE_CURVE('',#12489,#12491,#6290,.T.);
#15830=EDGE_CURVE('',#12493,#12494,#7984,.T.);
#15831=EDGE_CURVE('',#12494,#12492,#7985,.T.);
#15832=EDGE_CURVE('',#12491,#12493,#7986,.T.);
#15833=EDGE_CURVE('',#12495,#12496,#7987,.T.);
#15834=EDGE_CURVE('',#12496,#12494,#6291,.T.);
#15835=EDGE_CURVE('',#12493,#12495,#6292,.T.);
#15836=EDGE_CURVE('',#12483,#12496,#7988,.T.);
#15837=EDGE_CURVE('',#12495,#12484,#7989,.T.);
#15838=EDGE_CURVE('',#12497,#12487,#7990,.T.);
#15839=EDGE_CURVE('',#12498,#12497,#7991,.T.);
#15840=EDGE_CURVE('',#12498,#12489,#7992,.T.);
#15841=EDGE_CURVE('',#12499,#12485,#7993,.T.);
#15842=EDGE_CURVE('',#12497,#12499,#6293,.T.);
#15843=EDGE_CURVE('',#12500,#12481,#7994,.T.);
#15844=EDGE_CURVE('',#12499,#12500,#7995,.T.);
#15845=EDGE_CURVE('',#12501,#12484,#7996,.T.);
#15846=EDGE_CURVE('',#12500,#12501,#6294,.T.);
#15847=EDGE_CURVE('',#12494,#12463,#7997,.T.);
#15848=EDGE_CURVE('',#12492,#12462,#7998,.T.);
#15849=EDGE_CURVE('',#12496,#12464,#7999,.T.);
#15850=EDGE_CURVE('',#12483,#12465,#8000,.T.);
#15851=EDGE_CURVE('',#12482,#12466,#8001,.T.);
#15852=EDGE_CURVE('',#12474,#12502,#8002,.T.);
#15853=EDGE_CURVE('',#12502,#12503,#8003,.T.);
#15854=EDGE_CURVE('',#12503,#12473,#8004,.T.);
#15855=EDGE_CURVE('',#12480,#12504,#8005,.T.);
#15856=EDGE_CURVE('',#12504,#12502,#6295,.T.);
#15857=EDGE_CURVE('',#12479,#12505,#8006,.T.);
#15858=EDGE_CURVE('',#12505,#12504,#8007,.T.);
#15859=EDGE_CURVE('',#12478,#12506,#8008,.T.);
#15860=EDGE_CURVE('',#12506,#12505,#6296,.T.);
#15861=EDGE_CURVE('',#12477,#12507,#8009,.T.);
#15862=EDGE_CURVE('',#12507,#12506,#8010,.T.);
#15863=EDGE_CURVE('',#12476,#12508,#8011,.T.);
#15864=EDGE_CURVE('',#12508,#12507,#6297,.T.);
#15865=EDGE_CURVE('',#12475,#12509,#8012,.T.);
#15866=EDGE_CURVE('',#12509,#12508,#8013,.T.);
#15867=EDGE_CURVE('',#12503,#12509,#6298,.T.);
#15868=EDGE_CURVE('',#12508,#12510,#8014,.T.);
#15869=EDGE_CURVE('',#12511,#12510,#6299,.T.);
#15870=EDGE_CURVE('',#12507,#12511,#8015,.T.);
#15871=EDGE_CURVE('',#12509,#12512,#8016,.T.);
#15872=EDGE_CURVE('',#12510,#12512,#8017,.T.);
#15873=EDGE_CURVE('',#12513,#12503,#8018,.T.);
#15874=EDGE_CURVE('',#12512,#12513,#6300,.T.);
#15875=EDGE_CURVE('',#12502,#12514,#8019,.T.);
#15876=EDGE_CURVE('',#12513,#12514,#8020,.T.);
#15877=EDGE_CURVE('',#12497,#12513,#8021,.T.);
#15878=EDGE_CURVE('',#12514,#12498,#8022,.T.);
#15879=EDGE_CURVE('',#12499,#12512,#8023,.T.);
#15880=EDGE_CURVE('',#12500,#12510,#8024,.T.);
#15881=EDGE_CURVE('',#12501,#12511,#8025,.T.);
#15882=EDGE_CURVE('',#12515,#12516,#8026,.T.);
#15883=EDGE_CURVE('',#12516,#12511,#8027,.T.);
#15884=EDGE_CURVE('',#12501,#12515,#8028,.T.);
#15885=EDGE_CURVE('',#12517,#12518,#8029,.T.);
#15886=EDGE_CURVE('',#12518,#12516,#6301,.T.);
#15887=EDGE_CURVE('',#12515,#12517,#6302,.T.);
#15888=EDGE_CURVE('',#12519,#12520,#8030,.T.);
#15889=EDGE_CURVE('',#12520,#12518,#8031,.T.);
#15890=EDGE_CURVE('',#12517,#12519,#8032,.T.);
#15891=EDGE_CURVE('',#12514,#12520,#6303,.T.);
#15892=EDGE_CURVE('',#12519,#12498,#6304,.T.);
#15893=EDGE_CURVE('',#12506,#12516,#8033,.T.);
#15894=EDGE_CURVE('',#12505,#12518,#8034,.T.);
#15895=EDGE_CURVE('',#12504,#12520,#8035,.T.);
#15896=EDGE_CURVE('',#12490,#12460,#8036,.T.);
#15897=EDGE_CURVE('',#12461,#12488,#8037,.T.);
#15898=EDGE_CURVE('',#12486,#12467,#8038,.T.);
#15899=EDGE_CURVE('',#12517,#12493,#8039,.T.);
#15900=EDGE_CURVE('',#12515,#12495,#8040,.T.);
#15901=EDGE_CURVE('',#12519,#12491,#8041,.T.);
#15902=EDGE_CURVE('',#12521,#12521,#6305,.T.);
#15903=EDGE_CURVE('',#12521,#12522,#8042,.T.);
#15904=EDGE_CURVE('',#12522,#12522,#6306,.T.);
#15905=EDGE_CURVE('',#12523,#12523,#6307,.T.);
#15906=EDGE_CURVE('',#12523,#12521,#8043,.T.);
#15907=EDGE_CURVE('',#12523,#12524,#8044,.T.);
#15908=EDGE_CURVE('',#12524,#12524,#6308,.T.);
#15909=EDGE_CURVE('',#12525,#12525,#6309,.T.);
#15910=EDGE_CURVE('',#12525,#12526,#8045,.T.);
#15911=EDGE_CURVE('',#12526,#12526,#6310,.T.);
#15912=EDGE_CURVE('',#12527,#12527,#6311,.T.);
#15913=EDGE_CURVE('',#12528,#12528,#6312,.T.);
#15914=EDGE_CURVE('',#12528,#12527,#8046,.T.);
#15915=EDGE_CURVE('',#12529,#12529,#6313,.T.);
#15916=EDGE_CURVE('',#12529,#12528,#8047,.T.);
#15917=EDGE_CURVE('',#12530,#12530,#6314,.T.);
#15918=EDGE_CURVE('',#12530,#12522,#8048,.T.);
#15919=EDGE_CURVE('',#12531,#12531,#6315,.T.);
#15920=EDGE_CURVE('',#12532,#12532,#6316,.T.);
#15921=EDGE_CURVE('',#12532,#12531,#8049,.T.);
#15922=EDGE_CURVE('',#12533,#12533,#6317,.T.);
#15923=EDGE_CURVE('',#12533,#12532,#8050,.T.);
#15924=EDGE_CURVE('',#12534,#12534,#6318,.T.);
#15925=EDGE_CURVE('',#12534,#12535,#8051,.T.);
#15926=EDGE_CURVE('',#12535,#12535,#6319,.T.);
#15927=EDGE_CURVE('',#12536,#12536,#6320,.T.);
#15928=EDGE_CURVE('',#12536,#12537,#8052,.T.);
#15929=EDGE_CURVE('',#12537,#12537,#6321,.T.);
#15930=EDGE_CURVE('',#12538,#12539,#8053,.T.);
#15931=EDGE_CURVE('',#12538,#12540,#716,.T.);
#15932=EDGE_CURVE('',#12540,#12541,#6322,.T.);
#15933=EDGE_CURVE('',#12541,#12539,#717,.T.);
#15934=EDGE_CURVE('',#12542,#12543,#8054,.T.);
#15935=EDGE_CURVE('',#12542,#12538,#718,.T.);
#15936=EDGE_CURVE('',#12539,#12543,#719,.T.);
#15937=EDGE_CURVE('',#12544,#12545,#8055,.T.);
#15938=EDGE_CURVE('',#12544,#12542,#720,.T.);
#15939=EDGE_CURVE('',#12543,#12545,#721,.T.);
#15940=EDGE_CURVE('',#12546,#12547,#8056,.T.);
#15941=EDGE_CURVE('',#12546,#12544,#722,.T.);
#15942=EDGE_CURVE('',#12545,#12547,#723,.T.);
#15943=EDGE_CURVE('',#12548,#12549,#8057,.T.);
#15944=EDGE_CURVE('',#12548,#12546,#724,.T.);
#15945=EDGE_CURVE('',#12547,#12549,#725,.T.);
#15946=EDGE_CURVE('',#12550,#12551,#8058,.T.);
#15947=EDGE_CURVE('',#12550,#12548,#726,.T.);
#15948=EDGE_CURVE('',#12549,#12551,#727,.T.);
#15949=EDGE_CURVE('',#12552,#12553,#8059,.T.);
#15950=EDGE_CURVE('',#12552,#12550,#728,.T.);
#15951=EDGE_CURVE('',#12551,#12553,#729,.T.);
#15952=EDGE_CURVE('',#12554,#12555,#8060,.T.);
#15953=EDGE_CURVE('',#12554,#12552,#730,.T.);
#15954=EDGE_CURVE('',#12553,#12555,#731,.T.);
#15955=EDGE_CURVE('',#12556,#12557,#8061,.T.);
#15956=EDGE_CURVE('',#12556,#12554,#732,.T.);
#15957=EDGE_CURVE('',#12555,#12557,#733,.T.);
#15958=EDGE_CURVE('',#12558,#12559,#8062,.T.);
#15959=EDGE_CURVE('',#12558,#12556,#734,.T.);
#15960=EDGE_CURVE('',#12557,#12559,#735,.T.);
#15961=EDGE_CURVE('',#12560,#12561,#8063,.T.);
#15962=EDGE_CURVE('',#12560,#12558,#736,.T.);
#15963=EDGE_CURVE('',#12559,#12561,#737,.T.);
#15964=EDGE_CURVE('',#12562,#12563,#8064,.T.);
#15965=EDGE_CURVE('',#12562,#12560,#738,.T.);
#15966=EDGE_CURVE('',#12561,#12563,#739,.T.);
#15967=EDGE_CURVE('',#12564,#12565,#8065,.T.);
#15968=EDGE_CURVE('',#12564,#12562,#740,.T.);
#15969=EDGE_CURVE('',#12563,#12565,#741,.T.);
#15970=EDGE_CURVE('',#12566,#12567,#8066,.T.);
#15971=EDGE_CURVE('',#12566,#12564,#742,.T.);
#15972=EDGE_CURVE('',#12565,#12567,#743,.T.);
#15973=EDGE_CURVE('',#12568,#12569,#8067,.T.);
#15974=EDGE_CURVE('',#12568,#12566,#744,.T.);
#15975=EDGE_CURVE('',#12567,#12569,#745,.T.);
#15976=EDGE_CURVE('',#12570,#12571,#8068,.T.);
#15977=EDGE_CURVE('',#12570,#12568,#746,.T.);
#15978=EDGE_CURVE('',#12569,#12571,#747,.T.);
#15979=EDGE_CURVE('',#12572,#12573,#8069,.T.);
#15980=EDGE_CURVE('',#12572,#12570,#748,.T.);
#15981=EDGE_CURVE('',#12571,#12573,#749,.T.);
#15982=EDGE_CURVE('',#12574,#12575,#8070,.T.);
#15983=EDGE_CURVE('',#12574,#12572,#750,.T.);
#15984=EDGE_CURVE('',#12573,#12575,#751,.T.);
#15985=EDGE_CURVE('',#12576,#12577,#8071,.T.);
#15986=EDGE_CURVE('',#12576,#12574,#752,.T.);
#15987=EDGE_CURVE('',#12575,#12577,#753,.T.);
#15988=EDGE_CURVE('',#12578,#12579,#8072,.T.);
#15989=EDGE_CURVE('',#12578,#12576,#754,.T.);
#15990=EDGE_CURVE('',#12577,#12579,#755,.T.);
#15991=EDGE_CURVE('',#12580,#12581,#8073,.T.);
#15992=EDGE_CURVE('',#12580,#12578,#756,.T.);
#15993=EDGE_CURVE('',#12579,#12581,#757,.T.);
#15994=EDGE_CURVE('',#12582,#12583,#8074,.T.);
#15995=EDGE_CURVE('',#12582,#12580,#758,.T.);
#15996=EDGE_CURVE('',#12581,#12583,#759,.T.);
#15997=EDGE_CURVE('',#12584,#12585,#8075,.T.);
#15998=EDGE_CURVE('',#12584,#12582,#760,.T.);
#15999=EDGE_CURVE('',#12583,#12585,#761,.T.);
#16000=EDGE_CURVE('',#12586,#12587,#8076,.T.);
#16001=EDGE_CURVE('',#12586,#12588,#762,.T.);
#16002=EDGE_CURVE('',#12589,#12588,#6323,.T.);
#16003=EDGE_CURVE('',#12587,#12589,#763,.T.);
#16004=EDGE_CURVE('',#12590,#12591,#8077,.T.);
#16005=EDGE_CURVE('',#12590,#12586,#764,.T.);
#16006=EDGE_CURVE('',#12591,#12587,#765,.T.);
#16007=EDGE_CURVE('',#12592,#12593,#8078,.T.);
#16008=EDGE_CURVE('',#12592,#12590,#766,.T.);
#16009=EDGE_CURVE('',#12593,#12591,#767,.T.);
#16010=EDGE_CURVE('',#12594,#12595,#8079,.T.);
#16011=EDGE_CURVE('',#12594,#12592,#768,.T.);
#16012=EDGE_CURVE('',#12595,#12593,#769,.T.);
#16013=EDGE_CURVE('',#12596,#12597,#8080,.T.);
#16014=EDGE_CURVE('',#12596,#12594,#770,.T.);
#16015=EDGE_CURVE('',#12597,#12595,#771,.T.);
#16016=EDGE_CURVE('',#12598,#12599,#8081,.T.);
#16017=EDGE_CURVE('',#12598,#12596,#772,.T.);
#16018=EDGE_CURVE('',#12599,#12597,#773,.T.);
#16019=EDGE_CURVE('',#12600,#12601,#8082,.T.);
#16020=EDGE_CURVE('',#12600,#12598,#774,.T.);
#16021=EDGE_CURVE('',#12601,#12599,#775,.T.);
#16022=EDGE_CURVE('',#12602,#12603,#8083,.T.);
#16023=EDGE_CURVE('',#12602,#12600,#776,.T.);
#16024=EDGE_CURVE('',#12603,#12601,#777,.T.);
#16025=EDGE_CURVE('',#12604,#12605,#8084,.T.);
#16026=EDGE_CURVE('',#12604,#12602,#778,.T.);
#16027=EDGE_CURVE('',#12605,#12603,#779,.T.);
#16028=EDGE_CURVE('',#12606,#12607,#8085,.T.);
#16029=EDGE_CURVE('',#12606,#12604,#780,.T.);
#16030=EDGE_CURVE('',#12607,#12605,#781,.T.);
#16031=EDGE_CURVE('',#12608,#12609,#8086,.T.);
#16032=EDGE_CURVE('',#12608,#12606,#782,.T.);
#16033=EDGE_CURVE('',#12609,#12607,#783,.T.);
#16034=EDGE_CURVE('',#12610,#12611,#8087,.T.);
#16035=EDGE_CURVE('',#12610,#12608,#784,.T.);
#16036=EDGE_CURVE('',#12611,#12609,#785,.T.);
#16037=EDGE_CURVE('',#12612,#12613,#8088,.T.);
#16038=EDGE_CURVE('',#12612,#12610,#786,.T.);
#16039=EDGE_CURVE('',#12613,#12611,#787,.T.);
#16040=EDGE_CURVE('',#12614,#12615,#8089,.T.);
#16041=EDGE_CURVE('',#12614,#12612,#788,.T.);
#16042=EDGE_CURVE('',#12615,#12613,#789,.T.);
#16043=EDGE_CURVE('',#12616,#12617,#8090,.T.);
#16044=EDGE_CURVE('',#12616,#12614,#790,.T.);
#16045=EDGE_CURVE('',#12617,#12615,#791,.T.);
#16046=EDGE_CURVE('',#12618,#12619,#8091,.T.);
#16047=EDGE_CURVE('',#12618,#12616,#792,.T.);
#16048=EDGE_CURVE('',#12619,#12617,#793,.T.);
#16049=EDGE_CURVE('',#12620,#12621,#8092,.T.);
#16050=EDGE_CURVE('',#12620,#12618,#794,.T.);
#16051=EDGE_CURVE('',#12621,#12619,#795,.T.);
#16052=EDGE_CURVE('',#12622,#12623,#8093,.T.);
#16053=EDGE_CURVE('',#12622,#12620,#796,.T.);
#16054=EDGE_CURVE('',#12623,#12621,#797,.T.);
#16055=EDGE_CURVE('',#12624,#12625,#8094,.T.);
#16056=EDGE_CURVE('',#12624,#12622,#798,.T.);
#16057=EDGE_CURVE('',#12625,#12623,#799,.T.);
#16058=EDGE_CURVE('',#12626,#12627,#8095,.T.);
#16059=EDGE_CURVE('',#12626,#12624,#800,.T.);
#16060=EDGE_CURVE('',#12627,#12625,#801,.T.);
#16061=EDGE_CURVE('',#12628,#12629,#8096,.T.);
#16062=EDGE_CURVE('',#12628,#12626,#802,.T.);
#16063=EDGE_CURVE('',#12629,#12627,#803,.T.);
#16064=EDGE_CURVE('',#12630,#12631,#8097,.T.);
#16065=EDGE_CURVE('',#12630,#12628,#804,.T.);
#16066=EDGE_CURVE('',#12631,#12629,#805,.T.);
#16067=EDGE_CURVE('',#12632,#12589,#806,.T.);
#16068=EDGE_CURVE('',#12585,#12632,#807,.T.);
#16069=EDGE_CURVE('',#12633,#12541,#808,.T.);
#16070=EDGE_CURVE('',#12633,#12631,#809,.T.);
#16071=EDGE_CURVE('',#12541,#12634,#6324,.T.);
#16072=EDGE_CURVE('',#12634,#12540,#6325,.T.);
#16073=EDGE_CURVE('',#12540,#12635,#810,.T.);
#16074=EDGE_CURVE('',#12635,#12633,#6326,.T.);
#16075=EDGE_CURVE('',#12635,#12630,#811,.T.);
#16076=EDGE_CURVE('',#12588,#12636,#812,.T.);
#16077=EDGE_CURVE('',#12636,#12584,#813,.T.);
#16078=EDGE_CURVE('',#12637,#12638,#130,.T.);
#16079=EDGE_CURVE('',#12639,#12637,#131,.T.);
#16080=EDGE_CURVE('',#12640,#12639,#132,.T.);
#16081=EDGE_CURVE('',#12641,#12640,#133,.T.);
#16082=EDGE_CURVE('',#12642,#12641,#134,.T.);
#16083=EDGE_CURVE('',#12642,#12643,#8098,.T.);
#16084=EDGE_CURVE('',#12643,#12643,#6327,.T.);
#16085=EDGE_CURVE('',#12644,#12642,#135,.T.);
#16086=EDGE_CURVE('',#12638,#12644,#136,.T.);
#16087=EDGE_CURVE('',#12645,#12640,#8099,.T.);
#16088=EDGE_CURVE('',#12645,#12646,#8100,.T.);
#16089=EDGE_CURVE('',#12646,#12641,#8101,.T.);
#16090=EDGE_CURVE('',#12647,#12639,#8102,.T.);
#16091=EDGE_CURVE('',#12647,#12645,#8103,.T.);
#16092=EDGE_CURVE('',#12648,#12637,#8104,.T.);
#16093=EDGE_CURVE('',#12648,#12647,#8105,.T.);
#16094=EDGE_CURVE('',#12649,#12648,#8106,.T.);
#16095=EDGE_CURVE('',#12650,#12649,#8107,.T.);
#16096=EDGE_CURVE('',#12646,#12650,#8108,.T.);
#16097=EDGE_CURVE('',#12651,#12651,#6328,.T.);
#16098=EDGE_CURVE('',#12649,#12638,#8109,.T.);
#16099=EDGE_CURVE('',#12650,#12644,#8110,.T.);
#16100=EDGE_CURVE('',#12652,#12652,#6329,.T.);
#16101=EDGE_CURVE('',#12634,#12652,#8111,.T.);
#16102=EDGE_CURVE('',#12636,#12632,#6330,.T.);
#16103=EDGE_CURVE('',#12653,#12653,#6331,.T.);
#16104=EDGE_CURVE('',#12651,#12653,#8112,.T.);
#16105=EDGE_CURVE('',#12654,#12655,#8113,.T.);
#16106=EDGE_CURVE('',#12654,#12656,#814,.T.);
#16107=EDGE_CURVE('',#12656,#12657,#6332,.T.);
#16108=EDGE_CURVE('',#12657,#12655,#815,.T.);
#16109=EDGE_CURVE('',#12658,#12659,#8114,.T.);
#16110=EDGE_CURVE('',#12658,#12654,#816,.T.);
#16111=EDGE_CURVE('',#12655,#12659,#817,.T.);
#16112=EDGE_CURVE('',#12660,#12661,#8115,.T.);
#16113=EDGE_CURVE('',#12660,#12658,#818,.T.);
#16114=EDGE_CURVE('',#12659,#12661,#819,.T.);
#16115=EDGE_CURVE('',#12662,#12663,#8116,.T.);
#16116=EDGE_CURVE('',#12662,#12660,#820,.T.);
#16117=EDGE_CURVE('',#12661,#12663,#821,.T.);
#16118=EDGE_CURVE('',#12664,#12665,#8117,.T.);
#16119=EDGE_CURVE('',#12664,#12662,#822,.T.);
#16120=EDGE_CURVE('',#12663,#12665,#823,.T.);
#16121=EDGE_CURVE('',#12666,#12667,#8118,.T.);
#16122=EDGE_CURVE('',#12666,#12664,#824,.T.);
#16123=EDGE_CURVE('',#12665,#12667,#825,.T.);
#16124=EDGE_CURVE('',#12668,#12669,#8119,.T.);
#16125=EDGE_CURVE('',#12668,#12666,#826,.T.);
#16126=EDGE_CURVE('',#12667,#12669,#827,.T.);
#16127=EDGE_CURVE('',#12670,#12671,#8120,.T.);
#16128=EDGE_CURVE('',#12670,#12668,#828,.T.);
#16129=EDGE_CURVE('',#12669,#12671,#829,.T.);
#16130=EDGE_CURVE('',#12672,#12673,#8121,.T.);
#16131=EDGE_CURVE('',#12672,#12670,#830,.T.);
#16132=EDGE_CURVE('',#12671,#12673,#831,.T.);
#16133=EDGE_CURVE('',#12674,#12675,#8122,.T.);
#16134=EDGE_CURVE('',#12674,#12672,#832,.T.);
#16135=EDGE_CURVE('',#12673,#12675,#833,.T.);
#16136=EDGE_CURVE('',#12676,#12677,#8123,.T.);
#16137=EDGE_CURVE('',#12676,#12674,#834,.T.);
#16138=EDGE_CURVE('',#12675,#12677,#835,.T.);
#16139=EDGE_CURVE('',#12678,#12679,#8124,.T.);
#16140=EDGE_CURVE('',#12678,#12676,#836,.T.);
#16141=EDGE_CURVE('',#12677,#12679,#837,.T.);
#16142=EDGE_CURVE('',#12680,#12681,#8125,.T.);
#16143=EDGE_CURVE('',#12680,#12678,#838,.T.);
#16144=EDGE_CURVE('',#12679,#12681,#839,.T.);
#16145=EDGE_CURVE('',#12682,#12683,#8126,.T.);
#16146=EDGE_CURVE('',#12682,#12680,#840,.T.);
#16147=EDGE_CURVE('',#12681,#12683,#841,.T.);
#16148=EDGE_CURVE('',#12684,#12685,#8127,.T.);
#16149=EDGE_CURVE('',#12684,#12682,#842,.T.);
#16150=EDGE_CURVE('',#12683,#12685,#843,.T.);
#16151=EDGE_CURVE('',#12686,#12687,#8128,.T.);
#16152=EDGE_CURVE('',#12686,#12684,#844,.T.);
#16153=EDGE_CURVE('',#12685,#12687,#845,.T.);
#16154=EDGE_CURVE('',#12688,#12689,#8129,.T.);
#16155=EDGE_CURVE('',#12688,#12686,#846,.T.);
#16156=EDGE_CURVE('',#12687,#12689,#847,.T.);
#16157=EDGE_CURVE('',#12690,#12691,#8130,.T.);
#16158=EDGE_CURVE('',#12690,#12688,#848,.T.);
#16159=EDGE_CURVE('',#12689,#12691,#849,.T.);
#16160=EDGE_CURVE('',#12692,#12693,#8131,.T.);
#16161=EDGE_CURVE('',#12692,#12690,#850,.T.);
#16162=EDGE_CURVE('',#12691,#12693,#851,.T.);
#16163=EDGE_CURVE('',#12694,#12695,#8132,.T.);
#16164=EDGE_CURVE('',#12694,#12692,#852,.T.);
#16165=EDGE_CURVE('',#12693,#12695,#853,.T.);
#16166=EDGE_CURVE('',#12696,#12697,#8133,.T.);
#16167=EDGE_CURVE('',#12696,#12694,#854,.T.);
#16168=EDGE_CURVE('',#12695,#12697,#855,.T.);
#16169=EDGE_CURVE('',#12698,#12699,#8134,.T.);
#16170=EDGE_CURVE('',#12698,#12696,#856,.T.);
#16171=EDGE_CURVE('',#12697,#12699,#857,.T.);
#16172=EDGE_CURVE('',#12700,#12701,#8135,.T.);
#16173=EDGE_CURVE('',#12700,#12698,#858,.T.);
#16174=EDGE_CURVE('',#12699,#12701,#859,.T.);
#16175=EDGE_CURVE('',#12702,#12703,#8136,.T.);
#16176=EDGE_CURVE('',#12702,#12704,#860,.T.);
#16177=EDGE_CURVE('',#12705,#12704,#6333,.T.);
#16178=EDGE_CURVE('',#12703,#12705,#861,.T.);
#16179=EDGE_CURVE('',#12706,#12707,#8137,.T.);
#16180=EDGE_CURVE('',#12706,#12702,#862,.T.);
#16181=EDGE_CURVE('',#12707,#12703,#863,.T.);
#16182=EDGE_CURVE('',#12708,#12709,#8138,.T.);
#16183=EDGE_CURVE('',#12708,#12706,#864,.T.);
#16184=EDGE_CURVE('',#12709,#12707,#865,.T.);
#16185=EDGE_CURVE('',#12710,#12711,#8139,.T.);
#16186=EDGE_CURVE('',#12710,#12708,#866,.T.);
#16187=EDGE_CURVE('',#12711,#12709,#867,.T.);
#16188=EDGE_CURVE('',#12712,#12713,#8140,.T.);
#16189=EDGE_CURVE('',#12712,#12710,#868,.T.);
#16190=EDGE_CURVE('',#12713,#12711,#869,.T.);
#16191=EDGE_CURVE('',#12714,#12715,#8141,.T.);
#16192=EDGE_CURVE('',#12714,#12712,#870,.T.);
#16193=EDGE_CURVE('',#12715,#12713,#871,.T.);
#16194=EDGE_CURVE('',#12716,#12717,#8142,.T.);
#16195=EDGE_CURVE('',#12716,#12714,#872,.T.);
#16196=EDGE_CURVE('',#12717,#12715,#873,.T.);
#16197=EDGE_CURVE('',#12718,#12719,#8143,.T.);
#16198=EDGE_CURVE('',#12718,#12716,#874,.T.);
#16199=EDGE_CURVE('',#12719,#12717,#875,.T.);
#16200=EDGE_CURVE('',#12720,#12721,#8144,.T.);
#16201=EDGE_CURVE('',#12720,#12718,#876,.T.);
#16202=EDGE_CURVE('',#12721,#12719,#877,.T.);
#16203=EDGE_CURVE('',#12722,#12723,#8145,.T.);
#16204=EDGE_CURVE('',#12722,#12720,#878,.T.);
#16205=EDGE_CURVE('',#12723,#12721,#879,.T.);
#16206=EDGE_CURVE('',#12724,#12725,#8146,.T.);
#16207=EDGE_CURVE('',#12724,#12722,#880,.T.);
#16208=EDGE_CURVE('',#12725,#12723,#881,.T.);
#16209=EDGE_CURVE('',#12726,#12727,#8147,.T.);
#16210=EDGE_CURVE('',#12726,#12724,#882,.T.);
#16211=EDGE_CURVE('',#12727,#12725,#883,.T.);
#16212=EDGE_CURVE('',#12728,#12729,#8148,.T.);
#16213=EDGE_CURVE('',#12728,#12726,#884,.T.);
#16214=EDGE_CURVE('',#12729,#12727,#885,.T.);
#16215=EDGE_CURVE('',#12730,#12731,#8149,.T.);
#16216=EDGE_CURVE('',#12730,#12728,#886,.T.);
#16217=EDGE_CURVE('',#12731,#12729,#887,.T.);
#16218=EDGE_CURVE('',#12732,#12733,#8150,.T.);
#16219=EDGE_CURVE('',#12732,#12730,#888,.T.);
#16220=EDGE_CURVE('',#12733,#12731,#889,.T.);
#16221=EDGE_CURVE('',#12734,#12735,#8151,.T.);
#16222=EDGE_CURVE('',#12734,#12732,#890,.T.);
#16223=EDGE_CURVE('',#12735,#12733,#891,.T.);
#16224=EDGE_CURVE('',#12736,#12737,#8152,.T.);
#16225=EDGE_CURVE('',#12736,#12734,#892,.T.);
#16226=EDGE_CURVE('',#12737,#12735,#893,.T.);
#16227=EDGE_CURVE('',#12738,#12739,#8153,.T.);
#16228=EDGE_CURVE('',#12738,#12736,#894,.T.);
#16229=EDGE_CURVE('',#12739,#12737,#895,.T.);
#16230=EDGE_CURVE('',#12740,#12741,#8154,.T.);
#16231=EDGE_CURVE('',#12740,#12738,#896,.T.);
#16232=EDGE_CURVE('',#12741,#12739,#897,.T.);
#16233=EDGE_CURVE('',#12742,#12743,#8155,.T.);
#16234=EDGE_CURVE('',#12742,#12740,#898,.T.);
#16235=EDGE_CURVE('',#12743,#12741,#899,.T.);
#16236=EDGE_CURVE('',#12744,#12745,#8156,.T.);
#16237=EDGE_CURVE('',#12744,#12742,#900,.T.);
#16238=EDGE_CURVE('',#12745,#12743,#901,.T.);
#16239=EDGE_CURVE('',#12746,#12747,#8157,.T.);
#16240=EDGE_CURVE('',#12746,#12744,#902,.T.);
#16241=EDGE_CURVE('',#12747,#12745,#903,.T.);
#16242=EDGE_CURVE('',#12748,#12749,#8158,.T.);
#16243=EDGE_CURVE('',#12748,#12746,#904,.T.);
#16244=EDGE_CURVE('',#12749,#12747,#905,.T.);
#16245=EDGE_CURVE('',#12704,#12750,#906,.T.);
#16246=EDGE_CURVE('',#12751,#12750,#6334,.T.);
#16247=EDGE_CURVE('',#12752,#12751,#6335,.T.);
#16248=EDGE_CURVE('',#12752,#12705,#907,.T.);
#16249=EDGE_CURVE('',#12701,#12752,#908,.T.);
#16250=EDGE_CURVE('',#12753,#12657,#909,.T.);
#16251=EDGE_CURVE('',#12753,#12749,#910,.T.);
#16252=EDGE_CURVE('',#12657,#12754,#6336,.T.);
#16253=EDGE_CURVE('',#12754,#12656,#6337,.T.);
#16254=EDGE_CURVE('',#12656,#12755,#911,.T.);
#16255=EDGE_CURVE('',#12755,#12753,#6338,.T.);
#16256=EDGE_CURVE('',#12755,#12748,#912,.T.);
#16257=EDGE_CURVE('',#12750,#12700,#913,.T.);
#16258=EDGE_CURVE('',#12751,#12756,#6339,.T.);
#16259=EDGE_CURVE('',#12756,#12756,#6340,.T.);
#16260=EDGE_CURVE('',#12750,#12752,#6341,.T.);
#16261=EDGE_CURVE('',#12757,#12757,#6342,.T.);
#16262=EDGE_CURVE('',#12758,#12759,#8159,.T.);
#16263=EDGE_CURVE('',#12759,#12758,#6343,.T.);
#16264=EDGE_CURVE('',#12759,#12760,#8160,.T.);
#16265=EDGE_CURVE('',#12760,#12759,#6344,.T.);
#16266=EDGE_CURVE('',#12760,#12761,#8161,.T.);
#16267=EDGE_CURVE('',#12761,#12760,#6345,.T.);
#16268=EDGE_CURVE('',#12761,#12762,#8162,.T.);
#16269=EDGE_CURVE('',#12762,#12761,#6346,.T.);
#16270=EDGE_CURVE('',#12762,#12763,#8163,.T.);
#16271=EDGE_CURVE('',#12763,#12762,#6347,.T.);
#16272=EDGE_CURVE('',#12763,#12758,#8164,.T.);
#16273=EDGE_CURVE('',#12758,#12763,#6348,.T.);
#16274=EDGE_CURVE('',#12764,#12762,#8165,.T.);
#16275=EDGE_CURVE('',#12765,#12766,#8166,.T.);
#16276=EDGE_CURVE('',#12765,#12758,#8167,.T.);
#16277=EDGE_CURVE('',#12766,#12759,#8168,.T.);
#16278=EDGE_CURVE('',#12767,#12765,#8169,.T.);
#16279=EDGE_CURVE('',#12767,#12763,#8170,.T.);
#16280=EDGE_CURVE('',#12768,#12767,#8171,.T.);
#16281=EDGE_CURVE('',#12768,#12762,#8172,.T.);
#16282=EDGE_CURVE('',#12769,#12768,#8173,.T.);
#16283=EDGE_CURVE('',#12769,#12761,#8174,.T.);
#16284=EDGE_CURVE('',#12770,#12769,#8175,.T.);
#16285=EDGE_CURVE('',#12770,#12760,#8176,.T.);
#16286=EDGE_CURVE('',#12766,#12770,#8177,.T.);
#16287=EDGE_CURVE('',#12771,#12772,#8178,.T.);
#16288=EDGE_CURVE('',#12771,#12773,#8179,.T.);
#16289=EDGE_CURVE('',#12774,#12773,#8180,.T.);
#16290=EDGE_CURVE('',#12772,#12774,#8181,.T.);
#16291=EDGE_CURVE('',#12772,#12775,#6349,.T.);
#16292=EDGE_CURVE('',#12774,#12775,#8182,.T.);
#16293=EDGE_CURVE('',#12775,#12776,#8183,.T.);
#16294=EDGE_CURVE('',#12773,#12776,#8184,.T.);
#16295=EDGE_CURVE('',#12776,#12771,#6350,.T.);
#16296=EDGE_CURVE('',#12777,#12778,#8185,.T.);
#16297=EDGE_CURVE('',#12777,#12779,#8186,.T.);
#16298=EDGE_CURVE('',#12780,#12779,#8187,.T.);
#16299=EDGE_CURVE('',#12778,#12780,#8188,.T.);
#16300=EDGE_CURVE('',#12778,#12781,#6351,.T.);
#16301=EDGE_CURVE('',#12780,#12781,#8189,.T.);
#16302=EDGE_CURVE('',#12781,#12782,#8190,.T.);
#16303=EDGE_CURVE('',#12779,#12782,#8191,.T.);
#16304=EDGE_CURVE('',#12782,#12777,#6352,.T.);
#16305=EDGE_CURVE('',#12783,#12784,#8192,.T.);
#16306=EDGE_CURVE('',#12783,#12785,#8193,.T.);
#16307=EDGE_CURVE('',#12786,#12785,#8194,.T.);
#16308=EDGE_CURVE('',#12784,#12786,#8195,.T.);
#16309=EDGE_CURVE('',#12784,#12787,#6353,.T.);
#16310=EDGE_CURVE('',#12786,#12787,#8196,.T.);
#16311=EDGE_CURVE('',#12787,#12788,#8197,.T.);
#16312=EDGE_CURVE('',#12785,#12788,#8198,.T.);
#16313=EDGE_CURVE('',#12788,#12783,#6354,.T.);
#16314=EDGE_CURVE('',#12789,#12790,#8199,.T.);
#16315=EDGE_CURVE('',#12789,#12791,#8200,.T.);
#16316=EDGE_CURVE('',#12792,#12791,#8201,.T.);
#16317=EDGE_CURVE('',#12790,#12792,#8202,.T.);
#16318=EDGE_CURVE('',#12790,#12793,#6355,.T.);
#16319=EDGE_CURVE('',#12792,#12793,#8203,.T.);
#16320=EDGE_CURVE('',#12793,#12794,#8204,.T.);
#16321=EDGE_CURVE('',#12791,#12794,#8205,.T.);
#16322=EDGE_CURVE('',#12794,#12789,#6356,.T.);
#16323=EDGE_CURVE('',#12795,#12796,#8206,.T.);
#16324=EDGE_CURVE('',#12795,#12797,#8207,.T.);
#16325=EDGE_CURVE('',#12798,#12797,#8208,.T.);
#16326=EDGE_CURVE('',#12796,#12798,#8209,.T.);
#16327=EDGE_CURVE('',#12796,#12799,#6357,.T.);
#16328=EDGE_CURVE('',#12798,#12799,#8210,.T.);
#16329=EDGE_CURVE('',#12799,#12800,#8211,.T.);
#16330=EDGE_CURVE('',#12797,#12800,#8212,.T.);
#16331=EDGE_CURVE('',#12800,#12795,#6358,.T.);
#16332=EDGE_CURVE('',#12801,#12802,#8213,.T.);
#16333=EDGE_CURVE('',#12801,#12803,#8214,.T.);
#16334=EDGE_CURVE('',#12804,#12803,#8215,.T.);
#16335=EDGE_CURVE('',#12802,#12804,#8216,.T.);
#16336=EDGE_CURVE('',#12802,#12805,#6359,.T.);
#16337=EDGE_CURVE('',#12804,#12805,#8217,.T.);
#16338=EDGE_CURVE('',#12805,#12806,#8218,.T.);
#16339=EDGE_CURVE('',#12803,#12806,#8219,.T.);
#16340=EDGE_CURVE('',#12806,#12801,#6360,.T.);
#16341=EDGE_CURVE('',#12807,#12808,#8220,.T.);
#16342=EDGE_CURVE('',#12807,#12809,#8221,.T.);
#16343=EDGE_CURVE('',#12810,#12809,#8222,.T.);
#16344=EDGE_CURVE('',#12808,#12810,#8223,.T.);
#16345=EDGE_CURVE('',#12808,#12811,#6361,.T.);
#16346=EDGE_CURVE('',#12810,#12811,#8224,.T.);
#16347=EDGE_CURVE('',#12811,#12812,#8225,.T.);
#16348=EDGE_CURVE('',#12809,#12812,#8226,.T.);
#16349=EDGE_CURVE('',#12812,#12807,#6362,.T.);
#16350=EDGE_CURVE('',#12813,#12814,#8227,.T.);
#16351=EDGE_CURVE('',#12813,#12815,#8228,.T.);
#16352=EDGE_CURVE('',#12816,#12815,#8229,.T.);
#16353=EDGE_CURVE('',#12814,#12816,#8230,.T.);
#16354=EDGE_CURVE('',#12814,#12817,#6363,.T.);
#16355=EDGE_CURVE('',#12816,#12817,#8231,.T.);
#16356=EDGE_CURVE('',#12817,#12818,#8232,.T.);
#16357=EDGE_CURVE('',#12815,#12818,#8233,.T.);
#16358=EDGE_CURVE('',#12818,#12813,#6364,.T.);
#16359=EDGE_CURVE('',#12819,#12820,#8234,.T.);
#16360=EDGE_CURVE('',#12819,#12821,#8235,.T.);
#16361=EDGE_CURVE('',#12822,#12821,#8236,.T.);
#16362=EDGE_CURVE('',#12820,#12822,#8237,.T.);
#16363=EDGE_CURVE('',#12820,#12823,#6365,.T.);
#16364=EDGE_CURVE('',#12822,#12824,#8238,.T.);
#16365=EDGE_CURVE('',#12823,#12824,#6366,.T.);
#16366=EDGE_CURVE('',#12824,#12825,#8239,.T.);
#16367=EDGE_CURVE('',#12821,#12825,#8240,.T.);
#16368=EDGE_CURVE('',#12825,#12826,#6367,.T.);
#16369=EDGE_CURVE('',#12826,#12819,#6368,.T.);
#16370=EDGE_CURVE('',#12827,#12828,#8241,.T.);
#16371=EDGE_CURVE('',#12827,#12829,#8242,.T.);
#16372=EDGE_CURVE('',#12830,#12829,#8243,.T.);
#16373=EDGE_CURVE('',#12828,#12830,#8244,.T.);
#16374=EDGE_CURVE('',#12828,#12831,#6369,.T.);
#16375=EDGE_CURVE('',#12830,#12831,#8245,.T.);
#16376=EDGE_CURVE('',#12831,#12832,#8246,.T.);
#16377=EDGE_CURVE('',#12829,#12832,#8247,.T.);
#16378=EDGE_CURVE('',#12832,#12827,#6370,.T.);
#16379=EDGE_CURVE('',#12833,#12834,#8248,.T.);
#16380=EDGE_CURVE('',#12833,#12835,#8249,.T.);
#16381=EDGE_CURVE('',#12836,#12835,#8250,.T.);
#16382=EDGE_CURVE('',#12834,#12836,#8251,.T.);
#16383=EDGE_CURVE('',#12834,#12837,#6371,.T.);
#16384=EDGE_CURVE('',#12836,#12837,#8252,.T.);
#16385=EDGE_CURVE('',#12837,#12838,#8253,.T.);
#16386=EDGE_CURVE('',#12835,#12838,#8254,.T.);
#16387=EDGE_CURVE('',#12838,#12833,#6372,.T.);
#16388=EDGE_CURVE('',#12839,#12840,#8255,.T.);
#16389=EDGE_CURVE('',#12839,#12841,#8256,.T.);
#16390=EDGE_CURVE('',#12842,#12841,#8257,.T.);
#16391=EDGE_CURVE('',#12840,#12842,#8258,.T.);
#16392=EDGE_CURVE('',#12840,#12843,#6373,.T.);
#16393=EDGE_CURVE('',#12842,#12843,#8259,.T.);
#16394=EDGE_CURVE('',#12843,#12844,#8260,.T.);
#16395=EDGE_CURVE('',#12841,#12844,#8261,.T.);
#16396=EDGE_CURVE('',#12844,#12839,#6374,.T.);
#16397=EDGE_CURVE('',#12845,#12846,#8262,.T.);
#16398=EDGE_CURVE('',#12845,#12847,#8263,.T.);
#16399=EDGE_CURVE('',#12848,#12847,#8264,.T.);
#16400=EDGE_CURVE('',#12846,#12848,#8265,.T.);
#16401=EDGE_CURVE('',#12846,#12849,#6375,.T.);
#16402=EDGE_CURVE('',#12848,#12849,#8266,.T.);
#16403=EDGE_CURVE('',#12849,#12850,#8267,.T.);
#16404=EDGE_CURVE('',#12847,#12850,#8268,.T.);
#16405=EDGE_CURVE('',#12850,#12845,#6376,.T.);
#16406=EDGE_CURVE('',#12851,#12852,#8269,.T.);
#16407=EDGE_CURVE('',#12851,#12853,#8270,.T.);
#16408=EDGE_CURVE('',#12854,#12853,#8271,.T.);
#16409=EDGE_CURVE('',#12852,#12854,#8272,.T.);
#16410=EDGE_CURVE('',#12852,#12855,#6377,.T.);
#16411=EDGE_CURVE('',#12854,#12855,#8273,.T.);
#16412=EDGE_CURVE('',#12855,#12856,#8274,.T.);
#16413=EDGE_CURVE('',#12853,#12856,#8275,.T.);
#16414=EDGE_CURVE('',#12856,#12851,#6378,.T.);
#16415=EDGE_CURVE('',#12857,#12858,#8276,.T.);
#16416=EDGE_CURVE('',#12857,#12859,#8277,.T.);
#16417=EDGE_CURVE('',#12860,#12859,#8278,.T.);
#16418=EDGE_CURVE('',#12858,#12860,#8279,.T.);
#16419=EDGE_CURVE('',#12858,#12861,#6379,.T.);
#16420=EDGE_CURVE('',#12860,#12861,#8280,.T.);
#16421=EDGE_CURVE('',#12861,#12862,#8281,.T.);
#16422=EDGE_CURVE('',#12859,#12862,#8282,.T.);
#16423=EDGE_CURVE('',#12862,#12857,#6380,.T.);
#16424=EDGE_CURVE('',#12863,#12864,#8283,.T.);
#16425=EDGE_CURVE('',#12863,#12865,#8284,.T.);
#16426=EDGE_CURVE('',#12866,#12865,#8285,.T.);
#16427=EDGE_CURVE('',#12864,#12866,#8286,.T.);
#16428=EDGE_CURVE('',#12864,#12867,#6381,.T.);
#16429=EDGE_CURVE('',#12866,#12867,#8287,.T.);
#16430=EDGE_CURVE('',#12867,#12868,#8288,.T.);
#16431=EDGE_CURVE('',#12865,#12868,#8289,.T.);
#16432=EDGE_CURVE('',#12868,#12863,#6382,.T.);
#16433=EDGE_CURVE('',#12869,#12870,#8290,.T.);
#16434=EDGE_CURVE('',#12869,#12871,#8291,.T.);
#16435=EDGE_CURVE('',#12872,#12871,#8292,.T.);
#16436=EDGE_CURVE('',#12870,#12872,#8293,.T.);
#16437=EDGE_CURVE('',#12870,#12873,#6383,.T.);
#16438=EDGE_CURVE('',#12872,#12873,#8294,.T.);
#16439=EDGE_CURVE('',#12873,#12874,#8295,.T.);
#16440=EDGE_CURVE('',#12871,#12874,#8296,.T.);
#16441=EDGE_CURVE('',#12874,#12869,#6384,.T.);
#16442=EDGE_CURVE('',#12875,#12876,#8297,.T.);
#16443=EDGE_CURVE('',#12875,#12877,#8298,.T.);
#16444=EDGE_CURVE('',#12878,#12877,#8299,.T.);
#16445=EDGE_CURVE('',#12876,#12878,#8300,.T.);
#16446=EDGE_CURVE('',#12876,#12879,#6385,.T.);
#16447=EDGE_CURVE('',#12878,#12879,#8301,.T.);
#16448=EDGE_CURVE('',#12879,#12880,#8302,.T.);
#16449=EDGE_CURVE('',#12877,#12880,#8303,.T.);
#16450=EDGE_CURVE('',#12880,#12875,#6386,.T.);
#16451=EDGE_CURVE('',#12881,#12882,#8304,.T.);
#16452=EDGE_CURVE('',#12881,#12883,#8305,.T.);
#16453=EDGE_CURVE('',#12884,#12883,#8306,.T.);
#16454=EDGE_CURVE('',#12882,#12884,#8307,.T.);
#16455=EDGE_CURVE('',#12882,#12885,#6387,.T.);
#16456=EDGE_CURVE('',#12884,#12885,#8308,.T.);
#16457=EDGE_CURVE('',#12885,#12886,#8309,.T.);
#16458=EDGE_CURVE('',#12883,#12886,#8310,.T.);
#16459=EDGE_CURVE('',#12886,#12881,#6388,.T.);
#16460=EDGE_CURVE('',#12887,#12888,#8311,.T.);
#16461=EDGE_CURVE('',#12887,#12889,#8312,.T.);
#16462=EDGE_CURVE('',#12890,#12889,#8313,.T.);
#16463=EDGE_CURVE('',#12888,#12890,#8314,.T.);
#16464=EDGE_CURVE('',#12888,#12891,#6389,.T.);
#16465=EDGE_CURVE('',#12890,#12891,#8315,.T.);
#16466=EDGE_CURVE('',#12891,#12892,#8316,.T.);
#16467=EDGE_CURVE('',#12889,#12892,#8317,.T.);
#16468=EDGE_CURVE('',#12892,#12887,#6390,.T.);
#16469=EDGE_CURVE('',#12893,#12894,#8318,.T.);
#16470=EDGE_CURVE('',#12893,#12895,#8319,.T.);
#16471=EDGE_CURVE('',#12896,#12895,#8320,.T.);
#16472=EDGE_CURVE('',#12894,#12896,#8321,.T.);
#16473=EDGE_CURVE('',#12894,#12897,#6391,.T.);
#16474=EDGE_CURVE('',#12896,#12897,#8322,.T.);
#16475=EDGE_CURVE('',#12897,#12898,#8323,.T.);
#16476=EDGE_CURVE('',#12895,#12898,#8324,.T.);
#16477=EDGE_CURVE('',#12898,#12893,#6392,.T.);
#16478=EDGE_CURVE('',#12899,#12900,#8325,.T.);
#16479=EDGE_CURVE('',#12899,#12901,#8326,.T.);
#16480=EDGE_CURVE('',#12902,#12901,#8327,.T.);
#16481=EDGE_CURVE('',#12900,#12902,#8328,.T.);
#16482=EDGE_CURVE('',#12900,#12903,#6393,.T.);
#16483=EDGE_CURVE('',#12902,#12903,#8329,.T.);
#16484=EDGE_CURVE('',#12903,#12904,#8330,.T.);
#16485=EDGE_CURVE('',#12901,#12904,#8331,.T.);
#16486=EDGE_CURVE('',#12904,#12899,#6394,.T.);
#16487=EDGE_CURVE('',#12905,#12906,#8332,.T.);
#16488=EDGE_CURVE('',#12905,#12907,#8333,.T.);
#16489=EDGE_CURVE('',#12908,#12907,#8334,.T.);
#16490=EDGE_CURVE('',#12906,#12908,#8335,.T.);
#16491=EDGE_CURVE('',#12906,#12909,#6395,.T.);
#16492=EDGE_CURVE('',#12908,#12909,#8336,.T.);
#16493=EDGE_CURVE('',#12909,#12910,#8337,.T.);
#16494=EDGE_CURVE('',#12907,#12910,#8338,.T.);
#16495=EDGE_CURVE('',#12910,#12905,#6396,.T.);
#16496=EDGE_CURVE('',#12911,#12912,#8339,.T.);
#16497=EDGE_CURVE('',#12911,#12913,#8340,.T.);
#16498=EDGE_CURVE('',#12914,#12913,#8341,.T.);
#16499=EDGE_CURVE('',#12912,#12914,#8342,.T.);
#16500=EDGE_CURVE('',#12912,#12915,#6397,.T.);
#16501=EDGE_CURVE('',#12914,#12915,#8343,.T.);
#16502=EDGE_CURVE('',#12915,#12916,#8344,.T.);
#16503=EDGE_CURVE('',#12913,#12916,#8345,.T.);
#16504=EDGE_CURVE('',#12916,#12911,#6398,.T.);
#16505=EDGE_CURVE('',#12917,#12918,#8346,.T.);
#16506=EDGE_CURVE('',#12917,#12919,#8347,.T.);
#16507=EDGE_CURVE('',#12920,#12919,#8348,.T.);
#16508=EDGE_CURVE('',#12918,#12920,#8349,.T.);
#16509=EDGE_CURVE('',#12918,#12921,#6399,.T.);
#16510=EDGE_CURVE('',#12920,#12921,#8350,.T.);
#16511=EDGE_CURVE('',#12921,#12922,#8351,.T.);
#16512=EDGE_CURVE('',#12919,#12922,#8352,.T.);
#16513=EDGE_CURVE('',#12922,#12917,#6400,.T.);
#16514=EDGE_CURVE('',#12923,#12924,#8353,.T.);
#16515=EDGE_CURVE('',#12923,#12925,#8354,.T.);
#16516=EDGE_CURVE('',#12926,#12925,#8355,.T.);
#16517=EDGE_CURVE('',#12924,#12926,#8356,.T.);
#16518=EDGE_CURVE('',#12924,#12927,#6401,.T.);
#16519=EDGE_CURVE('',#12926,#12927,#8357,.T.);
#16520=EDGE_CURVE('',#12927,#12928,#8358,.T.);
#16521=EDGE_CURVE('',#12925,#12928,#8359,.T.);
#16522=EDGE_CURVE('',#12928,#12923,#6402,.T.);
#16523=EDGE_CURVE('',#12929,#12930,#6403,.T.);
#16524=EDGE_CURVE('',#12929,#12931,#8360,.T.);
#16525=EDGE_CURVE('',#12931,#12930,#8361,.T.);
#16526=EDGE_CURVE('',#12932,#12929,#8362,.T.);
#16527=EDGE_CURVE('',#12932,#12933,#8363,.T.);
#16528=EDGE_CURVE('',#12931,#12933,#8364,.T.);
#16529=EDGE_CURVE('',#12930,#12934,#8365,.T.);
#16530=EDGE_CURVE('',#12933,#12934,#8366,.T.);
#16531=EDGE_CURVE('',#12934,#12932,#6404,.T.);
#16532=EDGE_CURVE('',#12935,#12936,#8367,.T.);
#16533=EDGE_CURVE('',#12935,#12937,#8368,.T.);
#16534=EDGE_CURVE('',#12938,#12937,#8369,.T.);
#16535=EDGE_CURVE('',#12936,#12938,#8370,.T.);
#16536=EDGE_CURVE('',#12936,#12939,#6405,.T.);
#16537=EDGE_CURVE('',#12938,#12939,#8371,.T.);
#16538=EDGE_CURVE('',#12939,#12940,#8372,.T.);
#16539=EDGE_CURVE('',#12937,#12940,#8373,.T.);
#16540=EDGE_CURVE('',#12940,#12935,#6406,.T.);
#16541=EDGE_CURVE('',#12941,#12942,#8374,.T.);
#16542=EDGE_CURVE('',#12941,#12943,#8375,.T.);
#16543=EDGE_CURVE('',#12944,#12943,#8376,.T.);
#16544=EDGE_CURVE('',#12942,#12944,#8377,.T.);
#16545=EDGE_CURVE('',#12942,#12945,#6407,.T.);
#16546=EDGE_CURVE('',#12944,#12945,#8378,.T.);
#16547=EDGE_CURVE('',#12945,#12946,#8379,.T.);
#16548=EDGE_CURVE('',#12943,#12946,#8380,.T.);
#16549=EDGE_CURVE('',#12946,#12941,#6408,.T.);
#16550=EDGE_CURVE('',#12947,#12948,#8381,.T.);
#16551=EDGE_CURVE('',#12947,#12949,#8382,.T.);
#16552=EDGE_CURVE('',#12950,#12949,#8383,.T.);
#16553=EDGE_CURVE('',#12948,#12950,#8384,.T.);
#16554=EDGE_CURVE('',#12948,#12951,#6409,.T.);
#16555=EDGE_CURVE('',#12950,#12951,#8385,.T.);
#16556=EDGE_CURVE('',#12951,#12952,#8386,.T.);
#16557=EDGE_CURVE('',#12949,#12952,#8387,.T.);
#16558=EDGE_CURVE('',#12952,#12947,#6410,.T.);
#16559=EDGE_CURVE('',#12953,#12954,#8388,.T.);
#16560=EDGE_CURVE('',#12953,#12955,#8389,.T.);
#16561=EDGE_CURVE('',#12956,#12955,#8390,.T.);
#16562=EDGE_CURVE('',#12954,#12956,#8391,.T.);
#16563=EDGE_CURVE('',#12954,#12957,#6411,.T.);
#16564=EDGE_CURVE('',#12956,#12957,#8392,.T.);
#16565=EDGE_CURVE('',#12957,#12958,#8393,.T.);
#16566=EDGE_CURVE('',#12955,#12958,#8394,.T.);
#16567=EDGE_CURVE('',#12958,#12953,#6412,.T.);
#16568=EDGE_CURVE('',#12959,#12960,#8395,.T.);
#16569=EDGE_CURVE('',#12959,#12961,#8396,.T.);
#16570=EDGE_CURVE('',#12962,#12961,#8397,.T.);
#16571=EDGE_CURVE('',#12960,#12962,#8398,.T.);
#16572=EDGE_CURVE('',#12960,#12963,#6413,.T.);
#16573=EDGE_CURVE('',#12962,#12963,#8399,.T.);
#16574=EDGE_CURVE('',#12963,#12964,#8400,.T.);
#16575=EDGE_CURVE('',#12961,#12964,#8401,.T.);
#16576=EDGE_CURVE('',#12964,#12959,#6414,.T.);
#16577=EDGE_CURVE('',#12965,#12966,#8402,.T.);
#16578=EDGE_CURVE('',#12965,#12967,#8403,.T.);
#16579=EDGE_CURVE('',#12968,#12967,#8404,.T.);
#16580=EDGE_CURVE('',#12966,#12968,#8405,.T.);
#16581=EDGE_CURVE('',#12966,#12969,#6415,.T.);
#16582=EDGE_CURVE('',#12968,#12969,#8406,.T.);
#16583=EDGE_CURVE('',#12969,#12970,#8407,.T.);
#16584=EDGE_CURVE('',#12967,#12970,#8408,.T.);
#16585=EDGE_CURVE('',#12970,#12965,#6416,.T.);
#16586=EDGE_CURVE('',#12971,#12972,#8409,.T.);
#16587=EDGE_CURVE('',#12971,#12973,#8410,.T.);
#16588=EDGE_CURVE('',#12974,#12973,#8411,.T.);
#16589=EDGE_CURVE('',#12972,#12974,#8412,.T.);
#16590=EDGE_CURVE('',#12972,#12975,#6417,.T.);
#16591=EDGE_CURVE('',#12974,#12975,#8413,.T.);
#16592=EDGE_CURVE('',#12975,#12976,#8414,.T.);
#16593=EDGE_CURVE('',#12973,#12976,#8415,.T.);
#16594=EDGE_CURVE('',#12976,#12971,#6418,.T.);
#16595=EDGE_CURVE('',#12977,#12978,#8416,.T.);
#16596=EDGE_CURVE('',#12977,#12979,#8417,.T.);
#16597=EDGE_CURVE('',#12980,#12979,#8418,.T.);
#16598=EDGE_CURVE('',#12978,#12980,#8419,.T.);
#16599=EDGE_CURVE('',#12978,#12981,#6419,.T.);
#16600=EDGE_CURVE('',#12980,#12981,#8420,.T.);
#16601=EDGE_CURVE('',#12981,#12982,#8421,.T.);
#16602=EDGE_CURVE('',#12979,#12982,#8422,.T.);
#16603=EDGE_CURVE('',#12982,#12977,#6420,.T.);
#16604=EDGE_CURVE('',#12983,#12984,#8423,.T.);
#16605=EDGE_CURVE('',#12983,#12985,#8424,.T.);
#16606=EDGE_CURVE('',#12986,#12985,#8425,.T.);
#16607=EDGE_CURVE('',#12984,#12986,#8426,.T.);
#16608=EDGE_CURVE('',#12984,#12987,#6421,.T.);
#16609=EDGE_CURVE('',#12986,#12987,#8427,.T.);
#16610=EDGE_CURVE('',#12987,#12988,#8428,.T.);
#16611=EDGE_CURVE('',#12985,#12988,#8429,.T.);
#16612=EDGE_CURVE('',#12988,#12983,#6422,.T.);
#16613=EDGE_CURVE('',#12989,#12989,#6423,.T.);
#16614=EDGE_CURVE('',#12754,#12989,#8430,.T.);
#16615=EDGE_CURVE('',#12990,#12990,#6424,.T.);
#16616=EDGE_CURVE('',#12990,#12757,#8431,.T.);
#16617=EDGE_CURVE('',#12981,#12772,#6425,.T.);
#16618=EDGE_CURVE('',#12781,#12978,#6426,.T.);
#16619=EDGE_CURVE('',#12975,#12778,#6427,.T.);
#16620=EDGE_CURVE('',#12787,#12972,#6428,.T.);
#16621=EDGE_CURVE('',#12969,#12784,#6429,.T.);
#16622=EDGE_CURVE('',#12793,#12966,#6430,.T.);
#16623=EDGE_CURVE('',#12963,#12790,#6431,.T.);
#16624=EDGE_CURVE('',#12799,#12960,#6432,.T.);
#16625=EDGE_CURVE('',#12957,#12796,#6433,.T.);
#16626=EDGE_CURVE('',#12805,#12954,#6434,.T.);
#16627=EDGE_CURVE('',#12951,#12802,#6435,.T.);
#16628=EDGE_CURVE('',#12811,#12948,#6436,.T.);
#16629=EDGE_CURVE('',#12945,#12808,#6437,.T.);
#16630=EDGE_CURVE('',#12817,#12942,#6438,.T.);
#16631=EDGE_CURVE('',#12939,#12814,#6439,.T.);
#16632=EDGE_CURVE('',#12824,#12936,#6440,.T.);
#16633=EDGE_CURVE('',#12826,#12990,#8432,.T.);
#16634=EDGE_CURVE('',#12831,#12820,#6441,.T.);
#16635=EDGE_CURVE('',#12927,#12828,#6442,.T.);
#16636=EDGE_CURVE('',#12837,#12924,#6443,.T.);
#16637=EDGE_CURVE('',#12921,#12834,#6444,.T.);
#16638=EDGE_CURVE('',#12843,#12918,#6445,.T.);
#16639=EDGE_CURVE('',#12915,#12840,#6446,.T.);
#16640=EDGE_CURVE('',#12849,#12912,#6447,.T.);
#16641=EDGE_CURVE('',#12909,#12846,#6448,.T.);
#16642=EDGE_CURVE('',#12855,#12906,#6449,.T.);
#16643=EDGE_CURVE('',#12903,#12852,#6450,.T.);
#16644=EDGE_CURVE('',#12861,#12900,#6451,.T.);
#16645=EDGE_CURVE('',#12897,#12858,#6452,.T.);
#16646=EDGE_CURVE('',#12867,#12894,#6453,.T.);
#16647=EDGE_CURVE('',#12891,#12864,#6454,.T.);
#16648=EDGE_CURVE('',#12873,#12888,#6455,.T.);
#16649=EDGE_CURVE('',#12885,#12870,#6456,.T.);
#16650=EDGE_CURVE('',#12879,#12882,#6457,.T.);
#16651=EDGE_CURVE('',#12930,#12876,#6458,.T.);
#16652=EDGE_CURVE('',#12987,#12929,#6459,.T.);
#16653=EDGE_CURVE('',#12775,#12984,#6460,.T.);
#16654=EDGE_CURVE('',#12991,#12991,#6461,.T.);
#16655=EDGE_CURVE('',#12991,#12823,#8433,.T.);
#16656=EDGE_CURVE('',#12992,#12993,#8434,.T.);
#16657=EDGE_CURVE('',#12992,#12994,#914,.T.);
#16658=EDGE_CURVE('',#12994,#12995,#6462,.T.);
#16659=EDGE_CURVE('',#12995,#12993,#915,.T.);
#16660=EDGE_CURVE('',#12996,#12997,#8435,.T.);
#16661=EDGE_CURVE('',#12996,#12992,#916,.T.);
#16662=EDGE_CURVE('',#12993,#12997,#917,.T.);
#16663=EDGE_CURVE('',#12998,#12999,#8436,.T.);
#16664=EDGE_CURVE('',#12998,#12996,#918,.T.);
#16665=EDGE_CURVE('',#12997,#12999,#919,.T.);
#16666=EDGE_CURVE('',#13000,#13001,#8437,.T.);
#16667=EDGE_CURVE('',#13000,#12998,#920,.T.);
#16668=EDGE_CURVE('',#12999,#13001,#921,.T.);
#16669=EDGE_CURVE('',#13002,#13003,#8438,.T.);
#16670=EDGE_CURVE('',#13002,#13000,#922,.T.);
#16671=EDGE_CURVE('',#13001,#13003,#923,.T.);
#16672=EDGE_CURVE('',#13004,#13005,#8439,.T.);
#16673=EDGE_CURVE('',#13004,#13002,#924,.T.);
#16674=EDGE_CURVE('',#13003,#13005,#925,.T.);
#16675=EDGE_CURVE('',#13006,#13007,#8440,.T.);
#16676=EDGE_CURVE('',#13006,#13004,#926,.T.);
#16677=EDGE_CURVE('',#13005,#13007,#927,.T.);
#16678=EDGE_CURVE('',#13008,#13009,#8441,.T.);
#16679=EDGE_CURVE('',#13008,#13006,#928,.T.);
#16680=EDGE_CURVE('',#13007,#13009,#929,.T.);
#16681=EDGE_CURVE('',#13010,#13011,#8442,.T.);
#16682=EDGE_CURVE('',#13010,#13008,#930,.T.);
#16683=EDGE_CURVE('',#13009,#13011,#931,.T.);
#16684=EDGE_CURVE('',#13012,#13013,#8443,.T.);
#16685=EDGE_CURVE('',#13012,#13010,#932,.T.);
#16686=EDGE_CURVE('',#13011,#13013,#933,.T.);
#16687=EDGE_CURVE('',#13014,#13015,#8444,.T.);
#16688=EDGE_CURVE('',#13014,#13012,#934,.T.);
#16689=EDGE_CURVE('',#13013,#13015,#935,.T.);
#16690=EDGE_CURVE('',#13016,#13017,#8445,.T.);
#16691=EDGE_CURVE('',#13016,#13014,#936,.T.);
#16692=EDGE_CURVE('',#13015,#13017,#937,.T.);
#16693=EDGE_CURVE('',#13018,#13019,#8446,.T.);
#16694=EDGE_CURVE('',#13018,#13016,#938,.T.);
#16695=EDGE_CURVE('',#13017,#13019,#939,.T.);
#16696=EDGE_CURVE('',#13020,#13021,#8447,.T.);
#16697=EDGE_CURVE('',#13020,#13018,#940,.T.);
#16698=EDGE_CURVE('',#13019,#13021,#941,.T.);
#16699=EDGE_CURVE('',#13022,#13023,#8448,.T.);
#16700=EDGE_CURVE('',#13022,#13020,#942,.T.);
#16701=EDGE_CURVE('',#13021,#13023,#943,.T.);
#16702=EDGE_CURVE('',#13024,#13025,#8449,.T.);
#16703=EDGE_CURVE('',#13024,#13022,#944,.T.);
#16704=EDGE_CURVE('',#13023,#13025,#945,.T.);
#16705=EDGE_CURVE('',#13026,#13027,#8450,.T.);
#16706=EDGE_CURVE('',#13026,#13024,#946,.T.);
#16707=EDGE_CURVE('',#13025,#13027,#947,.T.);
#16708=EDGE_CURVE('',#13028,#13029,#8451,.T.);
#16709=EDGE_CURVE('',#13028,#13026,#948,.T.);
#16710=EDGE_CURVE('',#13027,#13029,#949,.T.);
#16711=EDGE_CURVE('',#13030,#13031,#8452,.T.);
#16712=EDGE_CURVE('',#13030,#13028,#950,.T.);
#16713=EDGE_CURVE('',#13029,#13031,#951,.T.);
#16714=EDGE_CURVE('',#13032,#13033,#8453,.T.);
#16715=EDGE_CURVE('',#13034,#13032,#6463,.T.);
#16716=EDGE_CURVE('',#13034,#13030,#952,.T.);
#16717=EDGE_CURVE('',#13031,#13033,#953,.T.);
#16718=EDGE_CURVE('',#13035,#13036,#8454,.T.);
#16719=EDGE_CURVE('',#13035,#13037,#954,.T.);
#16720=EDGE_CURVE('',#13038,#13037,#6464,.T.);
#16721=EDGE_CURVE('',#13036,#13038,#955,.T.);
#16722=EDGE_CURVE('',#13039,#13040,#8455,.T.);
#16723=EDGE_CURVE('',#13039,#13035,#956,.T.);
#16724=EDGE_CURVE('',#13040,#13036,#957,.T.);
#16725=EDGE_CURVE('',#13041,#13042,#8456,.T.);
#16726=EDGE_CURVE('',#13041,#13039,#958,.T.);
#16727=EDGE_CURVE('',#13042,#13040,#959,.T.);
#16728=EDGE_CURVE('',#13043,#13044,#8457,.T.);
#16729=EDGE_CURVE('',#13043,#13041,#960,.T.);
#16730=EDGE_CURVE('',#13044,#13042,#961,.T.);
#16731=EDGE_CURVE('',#13045,#13046,#8458,.T.);
#16732=EDGE_CURVE('',#13045,#13043,#962,.T.);
#16733=EDGE_CURVE('',#13046,#13044,#963,.T.);
#16734=EDGE_CURVE('',#13047,#13048,#8459,.T.);
#16735=EDGE_CURVE('',#13047,#13045,#964,.T.);
#16736=EDGE_CURVE('',#13048,#13046,#965,.T.);
#16737=EDGE_CURVE('',#13049,#13050,#8460,.T.);
#16738=EDGE_CURVE('',#13049,#13047,#966,.T.);
#16739=EDGE_CURVE('',#13050,#13048,#967,.T.);
#16740=EDGE_CURVE('',#13051,#13052,#8461,.T.);
#16741=EDGE_CURVE('',#13051,#13049,#968,.T.);
#16742=EDGE_CURVE('',#13052,#13050,#969,.T.);
#16743=EDGE_CURVE('',#13053,#13054,#8462,.T.);
#16744=EDGE_CURVE('',#13053,#13051,#970,.T.);
#16745=EDGE_CURVE('',#13054,#13052,#971,.T.);
#16746=EDGE_CURVE('',#13055,#13056,#8463,.T.);
#16747=EDGE_CURVE('',#13055,#13053,#972,.T.);
#16748=EDGE_CURVE('',#13056,#13054,#973,.T.);
#16749=EDGE_CURVE('',#13057,#13058,#8464,.T.);
#16750=EDGE_CURVE('',#13057,#13055,#974,.T.);
#16751=EDGE_CURVE('',#13058,#13056,#975,.T.);
#16752=EDGE_CURVE('',#13059,#13060,#8465,.T.);
#16753=EDGE_CURVE('',#13059,#13057,#976,.T.);
#16754=EDGE_CURVE('',#13060,#13058,#977,.T.);
#16755=EDGE_CURVE('',#13061,#13062,#8466,.T.);
#16756=EDGE_CURVE('',#13061,#13059,#978,.T.);
#16757=EDGE_CURVE('',#13062,#13060,#979,.T.);
#16758=EDGE_CURVE('',#13063,#13064,#8467,.T.);
#16759=EDGE_CURVE('',#13063,#13061,#980,.T.);
#16760=EDGE_CURVE('',#13064,#13062,#981,.T.);
#16761=EDGE_CURVE('',#13065,#13066,#8468,.T.);
#16762=EDGE_CURVE('',#13065,#13063,#982,.T.);
#16763=EDGE_CURVE('',#13066,#13064,#983,.T.);
#16764=EDGE_CURVE('',#13067,#13068,#8469,.T.);
#16765=EDGE_CURVE('',#13067,#13065,#984,.T.);
#16766=EDGE_CURVE('',#13068,#13066,#985,.T.);
#16767=EDGE_CURVE('',#13069,#13070,#8470,.T.);
#16768=EDGE_CURVE('',#13069,#13067,#986,.T.);
#16769=EDGE_CURVE('',#13070,#13068,#987,.T.);
#16770=EDGE_CURVE('',#13071,#13072,#8471,.T.);
#16771=EDGE_CURVE('',#13071,#13069,#988,.T.);
#16772=EDGE_CURVE('',#13072,#13070,#989,.T.);
#16773=EDGE_CURVE('',#13073,#13074,#8472,.T.);
#16774=EDGE_CURVE('',#13073,#13071,#990,.T.);
#16775=EDGE_CURVE('',#13074,#13072,#991,.T.);
#16776=EDGE_CURVE('',#13037,#13034,#992,.T.);
#16777=EDGE_CURVE('',#13075,#13034,#6465,.T.);
#16778=EDGE_CURVE('',#13075,#13038,#993,.T.);
#16779=EDGE_CURVE('',#13033,#13075,#994,.T.);
#16780=EDGE_CURVE('',#13076,#12995,#995,.T.);
#16781=EDGE_CURVE('',#13076,#13074,#996,.T.);
#16782=EDGE_CURVE('',#12995,#13077,#6466,.T.);
#16783=EDGE_CURVE('',#13077,#12994,#6467,.T.);
#16784=EDGE_CURVE('',#12994,#13078,#997,.T.);
#16785=EDGE_CURVE('',#13078,#13076,#6468,.T.);
#16786=EDGE_CURVE('',#13078,#13073,#998,.T.);
#16787=EDGE_CURVE('',#13032,#13079,#6469,.T.);
#16788=EDGE_CURVE('',#13079,#13079,#6470,.T.);
#16789=EDGE_CURVE('',#13032,#13075,#6471,.T.);
#16790=EDGE_CURVE('',#13080,#13080,#6472,.T.);
#16791=EDGE_CURVE('',#13081,#13082,#8473,.T.);
#16792=EDGE_CURVE('',#13082,#13081,#6473,.T.);
#16793=EDGE_CURVE('',#13082,#13083,#8474,.T.);
#16794=EDGE_CURVE('',#13083,#13082,#6474,.T.);
#16795=EDGE_CURVE('',#13083,#13084,#8475,.T.);
#16796=EDGE_CURVE('',#13084,#13083,#6475,.T.);
#16797=EDGE_CURVE('',#13084,#13085,#8476,.T.);
#16798=EDGE_CURVE('',#13085,#13084,#6476,.T.);
#16799=EDGE_CURVE('',#13085,#13086,#8477,.T.);
#16800=EDGE_CURVE('',#13086,#13085,#6477,.T.);
#16801=EDGE_CURVE('',#13086,#13081,#8478,.T.);
#16802=EDGE_CURVE('',#13081,#13086,#6478,.T.);
#16803=EDGE_CURVE('',#13087,#13085,#8479,.T.);
#16804=EDGE_CURVE('',#13088,#13089,#8480,.T.);
#16805=EDGE_CURVE('',#13088,#13081,#8481,.T.);
#16806=EDGE_CURVE('',#13089,#13082,#8482,.T.);
#16807=EDGE_CURVE('',#13090,#13088,#8483,.T.);
#16808=EDGE_CURVE('',#13090,#13086,#8484,.T.);
#16809=EDGE_CURVE('',#13091,#13090,#8485,.T.);
#16810=EDGE_CURVE('',#13091,#13085,#8486,.T.);
#16811=EDGE_CURVE('',#13092,#13091,#8487,.T.);
#16812=EDGE_CURVE('',#13092,#13084,#8488,.T.);
#16813=EDGE_CURVE('',#13093,#13092,#8489,.T.);
#16814=EDGE_CURVE('',#13093,#13083,#8490,.T.);
#16815=EDGE_CURVE('',#13089,#13093,#8491,.T.);
#16816=EDGE_CURVE('',#13094,#13095,#8492,.T.);
#16817=EDGE_CURVE('',#13094,#13096,#8493,.T.);
#16818=EDGE_CURVE('',#13097,#13096,#8494,.T.);
#16819=EDGE_CURVE('',#13095,#13097,#8495,.T.);
#16820=EDGE_CURVE('',#13095,#13098,#6479,.T.);
#16821=EDGE_CURVE('',#13097,#13098,#8496,.T.);
#16822=EDGE_CURVE('',#13098,#13099,#8497,.T.);
#16823=EDGE_CURVE('',#13096,#13099,#8498,.T.);
#16824=EDGE_CURVE('',#13099,#13094,#6480,.T.);
#16825=EDGE_CURVE('',#13100,#13101,#8499,.T.);
#16826=EDGE_CURVE('',#13100,#13102,#8500,.T.);
#16827=EDGE_CURVE('',#13103,#13102,#8501,.T.);
#16828=EDGE_CURVE('',#13101,#13103,#8502,.T.);
#16829=EDGE_CURVE('',#13101,#13104,#6481,.T.);
#16830=EDGE_CURVE('',#13103,#13104,#8503,.T.);
#16831=EDGE_CURVE('',#13104,#13105,#8504,.T.);
#16832=EDGE_CURVE('',#13102,#13105,#8505,.T.);
#16833=EDGE_CURVE('',#13105,#13100,#6482,.T.);
#16834=EDGE_CURVE('',#13106,#13107,#8506,.T.);
#16835=EDGE_CURVE('',#13106,#13108,#8507,.T.);
#16836=EDGE_CURVE('',#13109,#13108,#8508,.T.);
#16837=EDGE_CURVE('',#13107,#13109,#8509,.T.);
#16838=EDGE_CURVE('',#13107,#13110,#6483,.T.);
#16839=EDGE_CURVE('',#13109,#13110,#8510,.T.);
#16840=EDGE_CURVE('',#13110,#13111,#8511,.T.);
#16841=EDGE_CURVE('',#13108,#13111,#8512,.T.);
#16842=EDGE_CURVE('',#13111,#13106,#6484,.T.);
#16843=EDGE_CURVE('',#13112,#13113,#8513,.T.);
#16844=EDGE_CURVE('',#13112,#13114,#8514,.T.);
#16845=EDGE_CURVE('',#13115,#13114,#8515,.T.);
#16846=EDGE_CURVE('',#13113,#13115,#8516,.T.);
#16847=EDGE_CURVE('',#13113,#13116,#6485,.T.);
#16848=EDGE_CURVE('',#13115,#13116,#8517,.T.);
#16849=EDGE_CURVE('',#13116,#13117,#8518,.T.);
#16850=EDGE_CURVE('',#13114,#13117,#8519,.T.);
#16851=EDGE_CURVE('',#13117,#13112,#6486,.T.);
#16852=EDGE_CURVE('',#13118,#13119,#8520,.T.);
#16853=EDGE_CURVE('',#13118,#13120,#8521,.T.);
#16854=EDGE_CURVE('',#13121,#13120,#8522,.T.);
#16855=EDGE_CURVE('',#13119,#13121,#8523,.T.);
#16856=EDGE_CURVE('',#13119,#13122,#6487,.T.);
#16857=EDGE_CURVE('',#13121,#13122,#8524,.T.);
#16858=EDGE_CURVE('',#13122,#13123,#8525,.T.);
#16859=EDGE_CURVE('',#13120,#13123,#8526,.T.);
#16860=EDGE_CURVE('',#13123,#13118,#6488,.T.);
#16861=EDGE_CURVE('',#13124,#13125,#8527,.T.);
#16862=EDGE_CURVE('',#13124,#13126,#8528,.T.);
#16863=EDGE_CURVE('',#13127,#13126,#8529,.T.);
#16864=EDGE_CURVE('',#13125,#13127,#8530,.T.);
#16865=EDGE_CURVE('',#13125,#13128,#6489,.T.);
#16866=EDGE_CURVE('',#13127,#13128,#8531,.T.);
#16867=EDGE_CURVE('',#13128,#13129,#8532,.T.);
#16868=EDGE_CURVE('',#13126,#13129,#8533,.T.);
#16869=EDGE_CURVE('',#13129,#13124,#6490,.T.);
#16870=EDGE_CURVE('',#13130,#13131,#8534,.T.);
#16871=EDGE_CURVE('',#13130,#13132,#8535,.T.);
#16872=EDGE_CURVE('',#13133,#13132,#8536,.T.);
#16873=EDGE_CURVE('',#13131,#13133,#8537,.T.);
#16874=EDGE_CURVE('',#13131,#13134,#6491,.T.);
#16875=EDGE_CURVE('',#13133,#13134,#8538,.T.);
#16876=EDGE_CURVE('',#13134,#13135,#8539,.T.);
#16877=EDGE_CURVE('',#13132,#13135,#8540,.T.);
#16878=EDGE_CURVE('',#13135,#13130,#6492,.T.);
#16879=EDGE_CURVE('',#13136,#13137,#8541,.T.);
#16880=EDGE_CURVE('',#13136,#13138,#8542,.T.);
#16881=EDGE_CURVE('',#13139,#13138,#8543,.T.);
#16882=EDGE_CURVE('',#13137,#13139,#8544,.T.);
#16883=EDGE_CURVE('',#13137,#13140,#6493,.T.);
#16884=EDGE_CURVE('',#13139,#13140,#8545,.T.);
#16885=EDGE_CURVE('',#13140,#13141,#8546,.T.);
#16886=EDGE_CURVE('',#13138,#13141,#8547,.T.);
#16887=EDGE_CURVE('',#13141,#13136,#6494,.T.);
#16888=EDGE_CURVE('',#13142,#13143,#8548,.T.);
#16889=EDGE_CURVE('',#13142,#13144,#8549,.T.);
#16890=EDGE_CURVE('',#13145,#13144,#8550,.T.);
#16891=EDGE_CURVE('',#13143,#13145,#8551,.T.);
#16892=EDGE_CURVE('',#13143,#13146,#6495,.T.);
#16893=EDGE_CURVE('',#13145,#13147,#8552,.T.);
#16894=EDGE_CURVE('',#13146,#13147,#6496,.T.);
#16895=EDGE_CURVE('',#13147,#13148,#8553,.T.);
#16896=EDGE_CURVE('',#13144,#13148,#8554,.T.);
#16897=EDGE_CURVE('',#13148,#13149,#6497,.T.);
#16898=EDGE_CURVE('',#13149,#13142,#6498,.T.);
#16899=EDGE_CURVE('',#13150,#13151,#8555,.T.);
#16900=EDGE_CURVE('',#13150,#13152,#8556,.T.);
#16901=EDGE_CURVE('',#13153,#13152,#8557,.T.);
#16902=EDGE_CURVE('',#13151,#13153,#8558,.T.);
#16903=EDGE_CURVE('',#13151,#13154,#6499,.T.);
#16904=EDGE_CURVE('',#13153,#13154,#8559,.T.);
#16905=EDGE_CURVE('',#13154,#13155,#8560,.T.);
#16906=EDGE_CURVE('',#13152,#13155,#8561,.T.);
#16907=EDGE_CURVE('',#13155,#13150,#6500,.T.);
#16908=EDGE_CURVE('',#13156,#13157,#8562,.T.);
#16909=EDGE_CURVE('',#13156,#13158,#8563,.T.);
#16910=EDGE_CURVE('',#13159,#13158,#8564,.T.);
#16911=EDGE_CURVE('',#13157,#13159,#8565,.T.);
#16912=EDGE_CURVE('',#13157,#13160,#6501,.T.);
#16913=EDGE_CURVE('',#13159,#13160,#8566,.T.);
#16914=EDGE_CURVE('',#13160,#13161,#8567,.T.);
#16915=EDGE_CURVE('',#13158,#13161,#8568,.T.);
#16916=EDGE_CURVE('',#13161,#13156,#6502,.T.);
#16917=EDGE_CURVE('',#13162,#13163,#8569,.T.);
#16918=EDGE_CURVE('',#13162,#13164,#8570,.T.);
#16919=EDGE_CURVE('',#13165,#13164,#8571,.T.);
#16920=EDGE_CURVE('',#13163,#13165,#8572,.T.);
#16921=EDGE_CURVE('',#13163,#13166,#6503,.T.);
#16922=EDGE_CURVE('',#13165,#13166,#8573,.T.);
#16923=EDGE_CURVE('',#13166,#13167,#8574,.T.);
#16924=EDGE_CURVE('',#13164,#13167,#8575,.T.);
#16925=EDGE_CURVE('',#13167,#13162,#6504,.T.);
#16926=EDGE_CURVE('',#13168,#13169,#8576,.T.);
#16927=EDGE_CURVE('',#13168,#13170,#8577,.T.);
#16928=EDGE_CURVE('',#13171,#13170,#8578,.T.);
#16929=EDGE_CURVE('',#13169,#13171,#8579,.T.);
#16930=EDGE_CURVE('',#13169,#13172,#6505,.T.);
#16931=EDGE_CURVE('',#13171,#13172,#8580,.T.);
#16932=EDGE_CURVE('',#13172,#13173,#8581,.T.);
#16933=EDGE_CURVE('',#13170,#13173,#8582,.T.);
#16934=EDGE_CURVE('',#13173,#13168,#6506,.T.);
#16935=EDGE_CURVE('',#13174,#13175,#8583,.T.);
#16936=EDGE_CURVE('',#13174,#13176,#8584,.T.);
#16937=EDGE_CURVE('',#13177,#13176,#8585,.T.);
#16938=EDGE_CURVE('',#13175,#13177,#8586,.T.);
#16939=EDGE_CURVE('',#13175,#13178,#6507,.T.);
#16940=EDGE_CURVE('',#13177,#13178,#8587,.T.);
#16941=EDGE_CURVE('',#13178,#13179,#8588,.T.);
#16942=EDGE_CURVE('',#13176,#13179,#8589,.T.);
#16943=EDGE_CURVE('',#13179,#13174,#6508,.T.);
#16944=EDGE_CURVE('',#13180,#13181,#8590,.T.);
#16945=EDGE_CURVE('',#13180,#13182,#8591,.T.);
#16946=EDGE_CURVE('',#13183,#13182,#8592,.T.);
#16947=EDGE_CURVE('',#13181,#13183,#8593,.T.);
#16948=EDGE_CURVE('',#13181,#13184,#6509,.T.);
#16949=EDGE_CURVE('',#13183,#13184,#8594,.T.);
#16950=EDGE_CURVE('',#13184,#13185,#8595,.T.);
#16951=EDGE_CURVE('',#13182,#13185,#8596,.T.);
#16952=EDGE_CURVE('',#13185,#13180,#6510,.T.);
#16953=EDGE_CURVE('',#13186,#13187,#8597,.T.);
#16954=EDGE_CURVE('',#13186,#13188,#8598,.T.);
#16955=EDGE_CURVE('',#13189,#13188,#8599,.T.);
#16956=EDGE_CURVE('',#13187,#13189,#8600,.T.);
#16957=EDGE_CURVE('',#13187,#13190,#6511,.T.);
#16958=EDGE_CURVE('',#13189,#13190,#8601,.T.);
#16959=EDGE_CURVE('',#13190,#13191,#8602,.T.);
#16960=EDGE_CURVE('',#13188,#13191,#8603,.T.);
#16961=EDGE_CURVE('',#13191,#13186,#6512,.T.);
#16962=EDGE_CURVE('',#13192,#13193,#8604,.T.);
#16963=EDGE_CURVE('',#13192,#13194,#8605,.T.);
#16964=EDGE_CURVE('',#13195,#13194,#8606,.T.);
#16965=EDGE_CURVE('',#13193,#13195,#8607,.T.);
#16966=EDGE_CURVE('',#13193,#13196,#6513,.T.);
#16967=EDGE_CURVE('',#13195,#13196,#8608,.T.);
#16968=EDGE_CURVE('',#13196,#13197,#8609,.T.);
#16969=EDGE_CURVE('',#13194,#13197,#8610,.T.);
#16970=EDGE_CURVE('',#13197,#13192,#6514,.T.);
#16971=EDGE_CURVE('',#13198,#13199,#8611,.T.);
#16972=EDGE_CURVE('',#13198,#13200,#8612,.T.);
#16973=EDGE_CURVE('',#13201,#13200,#8613,.T.);
#16974=EDGE_CURVE('',#13199,#13201,#8614,.T.);
#16975=EDGE_CURVE('',#13199,#13202,#6515,.T.);
#16976=EDGE_CURVE('',#13201,#13202,#8615,.T.);
#16977=EDGE_CURVE('',#13202,#13203,#8616,.T.);
#16978=EDGE_CURVE('',#13200,#13203,#8617,.T.);
#16979=EDGE_CURVE('',#13203,#13198,#6516,.T.);
#16980=EDGE_CURVE('',#13204,#13205,#8618,.T.);
#16981=EDGE_CURVE('',#13204,#13206,#8619,.T.);
#16982=EDGE_CURVE('',#13207,#13206,#8620,.T.);
#16983=EDGE_CURVE('',#13205,#13207,#8621,.T.);
#16984=EDGE_CURVE('',#13205,#13208,#6517,.T.);
#16985=EDGE_CURVE('',#13207,#13208,#8622,.T.);
#16986=EDGE_CURVE('',#13208,#13209,#8623,.T.);
#16987=EDGE_CURVE('',#13206,#13209,#8624,.T.);
#16988=EDGE_CURVE('',#13209,#13204,#6518,.T.);
#16989=EDGE_CURVE('',#13210,#13211,#8625,.T.);
#16990=EDGE_CURVE('',#13210,#13212,#8626,.T.);
#16991=EDGE_CURVE('',#13213,#13212,#8627,.T.);
#16992=EDGE_CURVE('',#13211,#13213,#8628,.T.);
#16993=EDGE_CURVE('',#13211,#13214,#6519,.T.);
#16994=EDGE_CURVE('',#13213,#13214,#8629,.T.);
#16995=EDGE_CURVE('',#13214,#13215,#8630,.T.);
#16996=EDGE_CURVE('',#13212,#13215,#8631,.T.);
#16997=EDGE_CURVE('',#13215,#13210,#6520,.T.);
#16998=EDGE_CURVE('',#13216,#13217,#8632,.T.);
#16999=EDGE_CURVE('',#13216,#13218,#8633,.T.);
#17000=EDGE_CURVE('',#13219,#13218,#8634,.T.);
#17001=EDGE_CURVE('',#13217,#13219,#8635,.T.);
#17002=EDGE_CURVE('',#13217,#13220,#6521,.T.);
#17003=EDGE_CURVE('',#13219,#13220,#8636,.T.);
#17004=EDGE_CURVE('',#13220,#13221,#8637,.T.);
#17005=EDGE_CURVE('',#13218,#13221,#8638,.T.);
#17006=EDGE_CURVE('',#13221,#13216,#6522,.T.);
#17007=EDGE_CURVE('',#13222,#13223,#8639,.T.);
#17008=EDGE_CURVE('',#13222,#13224,#8640,.T.);
#17009=EDGE_CURVE('',#13225,#13224,#8641,.T.);
#17010=EDGE_CURVE('',#13223,#13225,#8642,.T.);
#17011=EDGE_CURVE('',#13223,#13226,#6523,.T.);
#17012=EDGE_CURVE('',#13225,#13226,#8643,.T.);
#17013=EDGE_CURVE('',#13226,#13227,#8644,.T.);
#17014=EDGE_CURVE('',#13224,#13227,#8645,.T.);
#17015=EDGE_CURVE('',#13227,#13222,#6524,.T.);
#17016=EDGE_CURVE('',#13228,#13229,#8646,.T.);
#17017=EDGE_CURVE('',#13228,#13230,#8647,.T.);
#17018=EDGE_CURVE('',#13231,#13230,#8648,.T.);
#17019=EDGE_CURVE('',#13229,#13231,#8649,.T.);
#17020=EDGE_CURVE('',#13229,#13232,#6525,.T.);
#17021=EDGE_CURVE('',#13231,#13232,#8650,.T.);
#17022=EDGE_CURVE('',#13232,#13233,#8651,.T.);
#17023=EDGE_CURVE('',#13230,#13233,#8652,.T.);
#17024=EDGE_CURVE('',#13233,#13228,#6526,.T.);
#17025=EDGE_CURVE('',#13234,#13235,#8653,.T.);
#17026=EDGE_CURVE('',#13234,#13236,#8654,.T.);
#17027=EDGE_CURVE('',#13237,#13236,#8655,.T.);
#17028=EDGE_CURVE('',#13235,#13237,#8656,.T.);
#17029=EDGE_CURVE('',#13235,#13238,#6527,.T.);
#17030=EDGE_CURVE('',#13237,#13238,#8657,.T.);
#17031=EDGE_CURVE('',#13238,#13239,#8658,.T.);
#17032=EDGE_CURVE('',#13236,#13239,#8659,.T.);
#17033=EDGE_CURVE('',#13239,#13234,#6528,.T.);
#17034=EDGE_CURVE('',#13240,#13241,#8660,.T.);
#17035=EDGE_CURVE('',#13240,#13242,#8661,.T.);
#17036=EDGE_CURVE('',#13243,#13242,#8662,.T.);
#17037=EDGE_CURVE('',#13241,#13243,#8663,.T.);
#17038=EDGE_CURVE('',#13241,#13244,#6529,.T.);
#17039=EDGE_CURVE('',#13243,#13244,#8664,.T.);
#17040=EDGE_CURVE('',#13244,#13245,#8665,.T.);
#17041=EDGE_CURVE('',#13242,#13245,#8666,.T.);
#17042=EDGE_CURVE('',#13245,#13240,#6530,.T.);
#17043=EDGE_CURVE('',#13246,#13247,#8667,.T.);
#17044=EDGE_CURVE('',#13246,#13248,#8668,.T.);
#17045=EDGE_CURVE('',#13249,#13248,#8669,.T.);
#17046=EDGE_CURVE('',#13247,#13249,#8670,.T.);
#17047=EDGE_CURVE('',#13247,#13250,#6531,.T.);
#17048=EDGE_CURVE('',#13249,#13250,#8671,.T.);
#17049=EDGE_CURVE('',#13250,#13251,#8672,.T.);
#17050=EDGE_CURVE('',#13248,#13251,#8673,.T.);
#17051=EDGE_CURVE('',#13251,#13246,#6532,.T.);
#17052=EDGE_CURVE('',#13252,#13253,#6533,.T.);
#17053=EDGE_CURVE('',#13252,#13254,#8674,.T.);
#17054=EDGE_CURVE('',#13254,#13253,#8675,.T.);
#17055=EDGE_CURVE('',#13255,#13252,#8676,.T.);
#17056=EDGE_CURVE('',#13255,#13256,#8677,.T.);
#17057=EDGE_CURVE('',#13254,#13256,#8678,.T.);
#17058=EDGE_CURVE('',#13253,#13257,#8679,.T.);
#17059=EDGE_CURVE('',#13256,#13257,#8680,.T.);
#17060=EDGE_CURVE('',#13257,#13255,#6534,.T.);
#17061=EDGE_CURVE('',#13258,#13259,#8681,.T.);
#17062=EDGE_CURVE('',#13258,#13260,#8682,.T.);
#17063=EDGE_CURVE('',#13261,#13260,#8683,.T.);
#17064=EDGE_CURVE('',#13259,#13261,#8684,.T.);
#17065=EDGE_CURVE('',#13259,#13262,#6535,.T.);
#17066=EDGE_CURVE('',#13261,#13262,#8685,.T.);
#17067=EDGE_CURVE('',#13262,#13263,#8686,.T.);
#17068=EDGE_CURVE('',#13260,#13263,#8687,.T.);
#17069=EDGE_CURVE('',#13263,#13258,#6536,.T.);
#17070=EDGE_CURVE('',#13264,#13265,#8688,.T.);
#17071=EDGE_CURVE('',#13264,#13266,#8689,.T.);
#17072=EDGE_CURVE('',#13267,#13266,#8690,.T.);
#17073=EDGE_CURVE('',#13265,#13267,#8691,.T.);
#17074=EDGE_CURVE('',#13265,#13268,#6537,.T.);
#17075=EDGE_CURVE('',#13267,#13268,#8692,.T.);
#17076=EDGE_CURVE('',#13268,#13269,#8693,.T.);
#17077=EDGE_CURVE('',#13266,#13269,#8694,.T.);
#17078=EDGE_CURVE('',#13269,#13264,#6538,.T.);
#17079=EDGE_CURVE('',#13270,#13271,#8695,.T.);
#17080=EDGE_CURVE('',#13270,#13272,#8696,.T.);
#17081=EDGE_CURVE('',#13273,#13272,#8697,.T.);
#17082=EDGE_CURVE('',#13271,#13273,#8698,.T.);
#17083=EDGE_CURVE('',#13271,#13274,#6539,.T.);
#17084=EDGE_CURVE('',#13273,#13274,#8699,.T.);
#17085=EDGE_CURVE('',#13274,#13275,#8700,.T.);
#17086=EDGE_CURVE('',#13272,#13275,#8701,.T.);
#17087=EDGE_CURVE('',#13275,#13270,#6540,.T.);
#17088=EDGE_CURVE('',#13276,#13277,#8702,.T.);
#17089=EDGE_CURVE('',#13276,#13278,#8703,.T.);
#17090=EDGE_CURVE('',#13279,#13278,#8704,.T.);
#17091=EDGE_CURVE('',#13277,#13279,#8705,.T.);
#17092=EDGE_CURVE('',#13277,#13280,#6541,.T.);
#17093=EDGE_CURVE('',#13279,#13280,#8706,.T.);
#17094=EDGE_CURVE('',#13280,#13281,#8707,.T.);
#17095=EDGE_CURVE('',#13278,#13281,#8708,.T.);
#17096=EDGE_CURVE('',#13281,#13276,#6542,.T.);
#17097=EDGE_CURVE('',#13282,#13283,#8709,.T.);
#17098=EDGE_CURVE('',#13282,#13284,#8710,.T.);
#17099=EDGE_CURVE('',#13285,#13284,#8711,.T.);
#17100=EDGE_CURVE('',#13283,#13285,#8712,.T.);
#17101=EDGE_CURVE('',#13283,#13286,#6543,.T.);
#17102=EDGE_CURVE('',#13285,#13286,#8713,.T.);
#17103=EDGE_CURVE('',#13286,#13287,#8714,.T.);
#17104=EDGE_CURVE('',#13284,#13287,#8715,.T.);
#17105=EDGE_CURVE('',#13287,#13282,#6544,.T.);
#17106=EDGE_CURVE('',#13288,#13289,#8716,.T.);
#17107=EDGE_CURVE('',#13288,#13290,#8717,.T.);
#17108=EDGE_CURVE('',#13291,#13290,#8718,.T.);
#17109=EDGE_CURVE('',#13289,#13291,#8719,.T.);
#17110=EDGE_CURVE('',#13289,#13292,#6545,.T.);
#17111=EDGE_CURVE('',#13291,#13292,#8720,.T.);
#17112=EDGE_CURVE('',#13292,#13293,#8721,.T.);
#17113=EDGE_CURVE('',#13290,#13293,#8722,.T.);
#17114=EDGE_CURVE('',#13293,#13288,#6546,.T.);
#17115=EDGE_CURVE('',#13294,#13295,#8723,.T.);
#17116=EDGE_CURVE('',#13294,#13296,#8724,.T.);
#17117=EDGE_CURVE('',#13297,#13296,#8725,.T.);
#17118=EDGE_CURVE('',#13295,#13297,#8726,.T.);
#17119=EDGE_CURVE('',#13295,#13298,#6547,.T.);
#17120=EDGE_CURVE('',#13297,#13298,#8727,.T.);
#17121=EDGE_CURVE('',#13298,#13299,#8728,.T.);
#17122=EDGE_CURVE('',#13296,#13299,#8729,.T.);
#17123=EDGE_CURVE('',#13299,#13294,#6548,.T.);
#17124=EDGE_CURVE('',#13300,#13301,#8730,.T.);
#17125=EDGE_CURVE('',#13300,#13302,#8731,.T.);
#17126=EDGE_CURVE('',#13303,#13302,#8732,.T.);
#17127=EDGE_CURVE('',#13301,#13303,#8733,.T.);
#17128=EDGE_CURVE('',#13301,#13304,#6549,.T.);
#17129=EDGE_CURVE('',#13303,#13304,#8734,.T.);
#17130=EDGE_CURVE('',#13304,#13305,#8735,.T.);
#17131=EDGE_CURVE('',#13302,#13305,#8736,.T.);
#17132=EDGE_CURVE('',#13305,#13300,#6550,.T.);
#17133=EDGE_CURVE('',#13306,#13307,#8737,.T.);
#17134=EDGE_CURVE('',#13306,#13308,#8738,.T.);
#17135=EDGE_CURVE('',#13309,#13308,#8739,.T.);
#17136=EDGE_CURVE('',#13307,#13309,#8740,.T.);
#17137=EDGE_CURVE('',#13307,#13310,#6551,.T.);
#17138=EDGE_CURVE('',#13309,#13310,#8741,.T.);
#17139=EDGE_CURVE('',#13310,#13311,#8742,.T.);
#17140=EDGE_CURVE('',#13308,#13311,#8743,.T.);
#17141=EDGE_CURVE('',#13311,#13306,#6552,.T.);
#17142=EDGE_CURVE('',#13312,#13312,#6553,.T.);
#17143=EDGE_CURVE('',#13077,#13312,#8744,.T.);
#17144=EDGE_CURVE('',#13313,#13313,#6554,.T.);
#17145=EDGE_CURVE('',#13313,#13080,#8745,.T.);
#17146=EDGE_CURVE('',#13304,#13095,#6555,.T.);
#17147=EDGE_CURVE('',#13104,#13301,#6556,.T.);
#17148=EDGE_CURVE('',#13298,#13101,#6557,.T.);
#17149=EDGE_CURVE('',#13110,#13295,#6558,.T.);
#17150=EDGE_CURVE('',#13292,#13107,#6559,.T.);
#17151=EDGE_CURVE('',#13116,#13289,#6560,.T.);
#17152=EDGE_CURVE('',#13286,#13113,#6561,.T.);
#17153=EDGE_CURVE('',#13122,#13283,#6562,.T.);
#17154=EDGE_CURVE('',#13280,#13119,#6563,.T.);
#17155=EDGE_CURVE('',#13128,#13277,#6564,.T.);
#17156=EDGE_CURVE('',#13274,#13125,#6565,.T.);
#17157=EDGE_CURVE('',#13134,#13271,#6566,.T.);
#17158=EDGE_CURVE('',#13268,#13131,#6567,.T.);
#17159=EDGE_CURVE('',#13140,#13265,#6568,.T.);
#17160=EDGE_CURVE('',#13262,#13137,#6569,.T.);
#17161=EDGE_CURVE('',#13147,#13259,#6570,.T.);
#17162=EDGE_CURVE('',#13149,#13313,#8746,.T.);
#17163=EDGE_CURVE('',#13154,#13143,#6571,.T.);
#17164=EDGE_CURVE('',#13250,#13151,#6572,.T.);
#17165=EDGE_CURVE('',#13160,#13247,#6573,.T.);
#17166=EDGE_CURVE('',#13244,#13157,#6574,.T.);
#17167=EDGE_CURVE('',#13166,#13241,#6575,.T.);
#17168=EDGE_CURVE('',#13238,#13163,#6576,.T.);
#17169=EDGE_CURVE('',#13172,#13235,#6577,.T.);
#17170=EDGE_CURVE('',#13232,#13169,#6578,.T.);
#17171=EDGE_CURVE('',#13178,#13229,#6579,.T.);
#17172=EDGE_CURVE('',#13226,#13175,#6580,.T.);
#17173=EDGE_CURVE('',#13184,#13223,#6581,.T.);
#17174=EDGE_CURVE('',#13220,#13181,#6582,.T.);
#17175=EDGE_CURVE('',#13190,#13217,#6583,.T.);
#17176=EDGE_CURVE('',#13214,#13187,#6584,.T.);
#17177=EDGE_CURVE('',#13196,#13211,#6585,.T.);
#17178=EDGE_CURVE('',#13208,#13193,#6586,.T.);
#17179=EDGE_CURVE('',#13202,#13205,#6587,.T.);
#17180=EDGE_CURVE('',#13253,#13199,#6588,.T.);
#17181=EDGE_CURVE('',#13310,#13252,#6589,.T.);
#17182=EDGE_CURVE('',#13098,#13307,#6590,.T.);
#17183=EDGE_CURVE('',#13314,#13314,#6591,.T.);
#17184=EDGE_CURVE('',#13314,#13146,#8747,.T.);
#17185=ORIENTED_EDGE('',*,*,#13315,.T.);
#17186=ORIENTED_EDGE('',*,*,#13316,.T.);
#17187=ORIENTED_EDGE('',*,*,#13317,.T.);
#17188=ORIENTED_EDGE('',*,*,#13318,.T.);
#17189=ORIENTED_EDGE('',*,*,#13319,.T.);
#17190=ORIENTED_EDGE('',*,*,#13320,.T.);
#17191=ORIENTED_EDGE('',*,*,#13315,.F.);
#17192=ORIENTED_EDGE('',*,*,#13321,.T.);
#17193=ORIENTED_EDGE('',*,*,#13322,.T.);
#17194=ORIENTED_EDGE('',*,*,#13323,.T.);
#17195=ORIENTED_EDGE('',*,*,#13319,.F.);
#17196=ORIENTED_EDGE('',*,*,#13324,.T.);
#17197=ORIENTED_EDGE('',*,*,#13325,.T.);
#17198=ORIENTED_EDGE('',*,*,#13326,.T.);
#17199=ORIENTED_EDGE('',*,*,#13322,.F.);
#17200=ORIENTED_EDGE('',*,*,#13327,.T.);
#17201=ORIENTED_EDGE('',*,*,#13328,.T.);
#17202=ORIENTED_EDGE('',*,*,#13329,.T.);
#17203=ORIENTED_EDGE('',*,*,#13325,.F.);
#17204=ORIENTED_EDGE('',*,*,#13330,.T.);
#17205=ORIENTED_EDGE('',*,*,#13331,.T.);
#17206=ORIENTED_EDGE('',*,*,#13332,.T.);
#17207=ORIENTED_EDGE('',*,*,#13328,.F.);
#17208=ORIENTED_EDGE('',*,*,#13333,.T.);
#17209=ORIENTED_EDGE('',*,*,#13334,.T.);
#17210=ORIENTED_EDGE('',*,*,#13335,.T.);
#17211=ORIENTED_EDGE('',*,*,#13331,.F.);
#17212=ORIENTED_EDGE('',*,*,#13336,.T.);
#17213=ORIENTED_EDGE('',*,*,#13317,.F.);
#17214=ORIENTED_EDGE('',*,*,#13337,.T.);
#17215=ORIENTED_EDGE('',*,*,#13334,.F.);
#17216=ORIENTED_EDGE('',*,*,#13338,.T.);
#17217=ORIENTED_EDGE('',*,*,#13332,.F.);
#17218=ORIENTED_EDGE('',*,*,#13339,.T.);
#17219=ORIENTED_EDGE('',*,*,#13340,.F.);
#17220=ORIENTED_EDGE('',*,*,#13341,.T.);
#17221=ORIENTED_EDGE('',*,*,#13335,.F.);
#17222=ORIENTED_EDGE('',*,*,#13342,.F.);
#17223=ORIENTED_EDGE('',*,*,#13343,.F.);
#17224=ORIENTED_EDGE('',*,*,#13339,.F.);
#17225=ORIENTED_EDGE('',*,*,#13337,.F.);
#17226=ORIENTED_EDGE('',*,*,#13344,.F.);
#17227=ORIENTED_EDGE('',*,*,#13345,.F.);
#17228=ORIENTED_EDGE('',*,*,#13342,.T.);
#17229=ORIENTED_EDGE('',*,*,#13316,.F.);
#17230=ORIENTED_EDGE('',*,*,#13346,.F.);
#17231=ORIENTED_EDGE('',*,*,#13347,.F.);
#17232=ORIENTED_EDGE('',*,*,#13344,.T.);
#17233=ORIENTED_EDGE('',*,*,#13348,.F.);
#17234=ORIENTED_EDGE('',*,*,#13349,.F.);
#17235=ORIENTED_EDGE('',*,*,#13350,.F.);
#17236=ORIENTED_EDGE('',*,*,#13351,.F.);
#17237=ORIENTED_EDGE('',*,*,#13352,.F.);
#17238=ORIENTED_EDGE('',*,*,#13353,.F.);
#17239=ORIENTED_EDGE('',*,*,#13354,.F.);
#17240=ORIENTED_EDGE('',*,*,#13355,.F.);
#17241=ORIENTED_EDGE('',*,*,#13318,.F.);
#17242=ORIENTED_EDGE('',*,*,#13338,.F.);
#17243=ORIENTED_EDGE('',*,*,#13336,.F.);
#17244=ORIENTED_EDGE('',*,*,#13333,.F.);
#17245=ORIENTED_EDGE('',*,*,#13330,.F.);
#17246=ORIENTED_EDGE('',*,*,#13327,.F.);
#17247=ORIENTED_EDGE('',*,*,#13324,.F.);
#17248=ORIENTED_EDGE('',*,*,#13321,.F.);
#17249=ORIENTED_EDGE('',*,*,#13356,.T.);
#17250=ORIENTED_EDGE('',*,*,#13357,.T.);
#17251=ORIENTED_EDGE('',*,*,#13358,.T.);
#17252=ORIENTED_EDGE('',*,*,#13357,.F.);
#17253=ORIENTED_EDGE('',*,*,#13359,.F.);
#17254=ORIENTED_EDGE('',*,*,#13360,.F.);
#17255=ORIENTED_EDGE('',*,*,#13361,.F.);
#17256=ORIENTED_EDGE('',*,*,#13362,.F.);
#17257=ORIENTED_EDGE('',*,*,#13363,.F.);
#17258=ORIENTED_EDGE('',*,*,#13364,.F.);
#17259=ORIENTED_EDGE('',*,*,#13365,.F.);
#17260=ORIENTED_EDGE('',*,*,#13366,.F.);
#17261=ORIENTED_EDGE('',*,*,#13367,.F.);
#17262=ORIENTED_EDGE('',*,*,#13368,.F.);
#17263=ORIENTED_EDGE('',*,*,#13369,.T.);
#17264=ORIENTED_EDGE('',*,*,#13370,.F.);
#17265=ORIENTED_EDGE('',*,*,#13371,.F.);
#17266=ORIENTED_EDGE('',*,*,#13372,.F.);
#17267=ORIENTED_EDGE('',*,*,#13373,.F.);
#17268=ORIENTED_EDGE('',*,*,#13374,.F.);
#17269=ORIENTED_EDGE('',*,*,#13356,.F.);
#17270=ORIENTED_EDGE('',*,*,#13375,.F.);
#17271=ORIENTED_EDGE('',*,*,#13376,.T.);
#17272=ORIENTED_EDGE('',*,*,#13358,.F.);
#17273=ORIENTED_EDGE('',*,*,#13376,.F.);
#17274=ORIENTED_EDGE('',*,*,#13367,.T.);
#17275=ORIENTED_EDGE('',*,*,#13377,.T.);
#17276=ORIENTED_EDGE('',*,*,#13378,.T.);
#17277=ORIENTED_EDGE('',*,*,#13377,.F.);
#17278=ORIENTED_EDGE('',*,*,#13379,.F.);
#17279=ORIENTED_EDGE('',*,*,#13380,.T.);
#17280=ORIENTED_EDGE('',*,*,#13378,.F.);
#17281=ORIENTED_EDGE('',*,*,#13380,.F.);
#17282=ORIENTED_EDGE('',*,*,#13374,.T.);
#17283=ORIENTED_EDGE('',*,*,#13381,.T.);
#17284=ORIENTED_EDGE('',*,*,#13382,.T.);
#17285=ORIENTED_EDGE('',*,*,#13381,.F.);
#17286=ORIENTED_EDGE('',*,*,#13383,.F.);
#17287=ORIENTED_EDGE('',*,*,#13384,.T.);
#17288=ORIENTED_EDGE('',*,*,#13382,.F.);
#17289=ORIENTED_EDGE('',*,*,#13384,.F.);
#17290=ORIENTED_EDGE('',*,*,#13368,.T.);
#17291=ORIENTED_EDGE('',*,*,#13385,.T.);
#17292=ORIENTED_EDGE('',*,*,#13386,.T.);
#17293=ORIENTED_EDGE('',*,*,#13385,.F.);
#17294=ORIENTED_EDGE('',*,*,#13387,.F.);
#17295=ORIENTED_EDGE('',*,*,#13388,.T.);
#17296=ORIENTED_EDGE('',*,*,#13386,.F.);
#17297=ORIENTED_EDGE('',*,*,#13388,.F.);
#17298=ORIENTED_EDGE('',*,*,#13372,.T.);
#17299=ORIENTED_EDGE('',*,*,#13389,.T.);
#17300=ORIENTED_EDGE('',*,*,#13390,.T.);
#17301=ORIENTED_EDGE('',*,*,#13391,.F.);
#17302=ORIENTED_EDGE('',*,*,#13370,.T.);
#17303=ORIENTED_EDGE('',*,*,#13392,.T.);
#17304=ORIENTED_EDGE('',*,*,#13393,.T.);
#17305=ORIENTED_EDGE('',*,*,#13394,.T.);
#17306=ORIENTED_EDGE('',*,*,#13395,.T.);
#17307=ORIENTED_EDGE('',*,*,#13392,.F.);
#17308=ORIENTED_EDGE('',*,*,#13373,.T.);
#17309=ORIENTED_EDGE('',*,*,#13391,.T.);
#17310=ORIENTED_EDGE('',*,*,#13371,.T.);
#17311=ORIENTED_EDGE('',*,*,#13394,.F.);
#17312=ORIENTED_EDGE('',*,*,#13396,.T.);
#17313=ORIENTED_EDGE('',*,*,#13389,.F.);
#17314=ORIENTED_EDGE('',*,*,#13396,.F.);
#17315=ORIENTED_EDGE('',*,*,#13397,.T.);
#17316=ORIENTED_EDGE('',*,*,#13398,.T.);
#17317=ORIENTED_EDGE('',*,*,#13399,.F.);
#17318=ORIENTED_EDGE('',*,*,#13393,.F.);
#17319=ORIENTED_EDGE('',*,*,#13400,.T.);
#17320=ORIENTED_EDGE('',*,*,#13401,.T.);
#17321=ORIENTED_EDGE('',*,*,#13397,.F.);
#17322=ORIENTED_EDGE('',*,*,#13402,.T.);
#17323=ORIENTED_EDGE('',*,*,#13403,.T.);
#17324=ORIENTED_EDGE('',*,*,#13404,.T.);
#17325=ORIENTED_EDGE('',*,*,#13340,.T.);
#17326=ORIENTED_EDGE('',*,*,#13405,.T.);
#17327=ORIENTED_EDGE('',*,*,#13406,.T.);
#17328=ORIENTED_EDGE('',*,*,#13407,.T.);
#17329=ORIENTED_EDGE('',*,*,#13408,.T.);
#17330=ORIENTED_EDGE('',*,*,#13404,.F.);
#17331=ORIENTED_EDGE('',*,*,#13409,.T.);
#17332=ORIENTED_EDGE('',*,*,#13410,.T.);
#17333=ORIENTED_EDGE('',*,*,#13411,.T.);
#17334=ORIENTED_EDGE('',*,*,#13407,.F.);
#17335=ORIENTED_EDGE('',*,*,#13412,.T.);
#17336=ORIENTED_EDGE('',*,*,#13413,.T.);
#17337=ORIENTED_EDGE('',*,*,#13414,.T.);
#17338=ORIENTED_EDGE('',*,*,#13410,.F.);
#17339=ORIENTED_EDGE('',*,*,#13415,.T.);
#17340=ORIENTED_EDGE('',*,*,#13416,.T.);
#17341=ORIENTED_EDGE('',*,*,#13417,.T.);
#17342=ORIENTED_EDGE('',*,*,#13418,.T.);
#17343=ORIENTED_EDGE('',*,*,#13419,.T.);
#17344=ORIENTED_EDGE('',*,*,#13413,.F.);
#17345=ORIENTED_EDGE('',*,*,#13420,.T.);
#17346=ORIENTED_EDGE('',*,*,#13421,.T.);
#17347=ORIENTED_EDGE('',*,*,#13347,.T.);
#17348=ORIENTED_EDGE('',*,*,#13418,.F.);
#17349=ORIENTED_EDGE('',*,*,#13422,.T.);
#17350=ORIENTED_EDGE('',*,*,#13423,.T.);
#17351=ORIENTED_EDGE('',*,*,#13345,.T.);
#17352=ORIENTED_EDGE('',*,*,#13421,.F.);
#17353=ORIENTED_EDGE('',*,*,#13424,.T.);
#17354=ORIENTED_EDGE('',*,*,#13405,.F.);
#17355=ORIENTED_EDGE('',*,*,#13343,.T.);
#17356=ORIENTED_EDGE('',*,*,#13423,.F.);
#17357=ORIENTED_EDGE('',*,*,#13425,.T.);
#17358=ORIENTED_EDGE('',*,*,#13406,.F.);
#17359=ORIENTED_EDGE('',*,*,#13426,.T.);
#17360=ORIENTED_EDGE('',*,*,#13427,.F.);
#17361=ORIENTED_EDGE('',*,*,#13428,.F.);
#17362=ORIENTED_EDGE('',*,*,#13403,.F.);
#17363=ORIENTED_EDGE('',*,*,#13429,.T.);
#17364=ORIENTED_EDGE('',*,*,#13430,.T.);
#17365=ORIENTED_EDGE('',*,*,#13425,.F.);
#17366=ORIENTED_EDGE('',*,*,#13431,.T.);
#17367=ORIENTED_EDGE('',*,*,#13432,.F.);
#17368=ORIENTED_EDGE('',*,*,#13426,.F.);
#17369=ORIENTED_EDGE('',*,*,#13424,.F.);
#17370=ORIENTED_EDGE('',*,*,#13433,.T.);
#17371=ORIENTED_EDGE('',*,*,#13434,.F.);
#17372=ORIENTED_EDGE('',*,*,#13431,.F.);
#17373=ORIENTED_EDGE('',*,*,#13422,.F.);
#17374=ORIENTED_EDGE('',*,*,#13435,.T.);
#17375=ORIENTED_EDGE('',*,*,#13436,.F.);
#17376=ORIENTED_EDGE('',*,*,#13433,.F.);
#17377=ORIENTED_EDGE('',*,*,#13417,.F.);
#17378=ORIENTED_EDGE('',*,*,#13437,.T.);
#17379=ORIENTED_EDGE('',*,*,#13438,.T.);
#17380=ORIENTED_EDGE('',*,*,#13420,.F.);
#17381=ORIENTED_EDGE('',*,*,#13439,.T.);
#17382=ORIENTED_EDGE('',*,*,#13440,.F.);
#17383=ORIENTED_EDGE('',*,*,#13435,.F.);
#17384=ORIENTED_EDGE('',*,*,#13416,.F.);
#17385=ORIENTED_EDGE('',*,*,#13438,.F.);
#17386=ORIENTED_EDGE('',*,*,#13441,.T.);
#17387=ORIENTED_EDGE('',*,*,#13442,.F.);
#17388=ORIENTED_EDGE('',*,*,#13443,.F.);
#17389=ORIENTED_EDGE('',*,*,#13444,.F.);
#17390=ORIENTED_EDGE('',*,*,#13441,.F.);
#17391=ORIENTED_EDGE('',*,*,#13437,.F.);
#17392=ORIENTED_EDGE('',*,*,#13445,.T.);
#17393=ORIENTED_EDGE('',*,*,#13446,.T.);
#17394=ORIENTED_EDGE('',*,*,#13447,.T.);
#17395=ORIENTED_EDGE('',*,*,#13448,.T.);
#17396=ORIENTED_EDGE('',*,*,#13449,.T.);
#17397=ORIENTED_EDGE('',*,*,#13450,.T.);
#17398=ORIENTED_EDGE('',*,*,#13451,.T.);
#17399=ORIENTED_EDGE('',*,*,#13452,.T.);
#17400=ORIENTED_EDGE('',*,*,#13449,.F.);
#17401=ORIENTED_EDGE('',*,*,#13446,.F.);
#17402=ORIENTED_EDGE('',*,*,#13453,.T.);
#17403=ORIENTED_EDGE('',*,*,#13454,.T.);
#17404=ORIENTED_EDGE('',*,*,#13455,.T.);
#17405=ORIENTED_EDGE('',*,*,#13456,.F.);
#17406=ORIENTED_EDGE('',*,*,#13445,.F.);
#17407=ORIENTED_EDGE('',*,*,#13452,.F.);
#17408=ORIENTED_EDGE('',*,*,#13457,.F.);
#17409=ORIENTED_EDGE('',*,*,#13458,.F.);
#17410=ORIENTED_EDGE('',*,*,#13459,.T.);
#17411=ORIENTED_EDGE('',*,*,#13460,.F.);
#17412=ORIENTED_EDGE('',*,*,#13461,.F.);
#17413=ORIENTED_EDGE('',*,*,#13453,.F.);
#17414=ORIENTED_EDGE('',*,*,#13447,.F.);
#17415=ORIENTED_EDGE('',*,*,#13456,.T.);
#17416=ORIENTED_EDGE('',*,*,#13462,.T.);
#17417=ORIENTED_EDGE('',*,*,#13463,.T.);
#17418=ORIENTED_EDGE('',*,*,#13464,.T.);
#17419=ORIENTED_EDGE('',*,*,#13465,.T.);
#17420=ORIENTED_EDGE('',*,*,#13464,.F.);
#17421=ORIENTED_EDGE('',*,*,#13466,.F.);
#17422=ORIENTED_EDGE('',*,*,#13467,.T.);
#17423=ORIENTED_EDGE('',*,*,#13468,.T.);
#17424=ORIENTED_EDGE('',*,*,#13469,.T.);
#17425=ORIENTED_EDGE('',*,*,#13463,.F.);
#17426=ORIENTED_EDGE('',*,*,#13470,.T.);
#17427=ORIENTED_EDGE('',*,*,#13471,.F.);
#17428=ORIENTED_EDGE('',*,*,#13472,.T.);
#17429=ORIENTED_EDGE('',*,*,#13466,.T.);
#17430=ORIENTED_EDGE('',*,*,#13462,.F.);
#17431=ORIENTED_EDGE('',*,*,#13473,.F.);
#17432=ORIENTED_EDGE('',*,*,#13474,.F.);
#17433=ORIENTED_EDGE('',*,*,#13475,.F.);
#17434=ORIENTED_EDGE('',*,*,#13476,.T.);
#17435=ORIENTED_EDGE('',*,*,#13474,.T.);
#17436=ORIENTED_EDGE('',*,*,#13477,.T.);
#17437=ORIENTED_EDGE('',*,*,#13478,.T.);
#17438=ORIENTED_EDGE('',*,*,#13476,.F.);
#17439=ORIENTED_EDGE('',*,*,#13479,.T.);
#17440=ORIENTED_EDGE('',*,*,#13480,.T.);
#17441=ORIENTED_EDGE('',*,*,#13470,.F.);
#17442=ORIENTED_EDGE('',*,*,#13475,.T.);
#17443=ORIENTED_EDGE('',*,*,#13481,.T.);
#17444=ORIENTED_EDGE('',*,*,#13482,.T.);
#17445=ORIENTED_EDGE('',*,*,#13483,.T.);
#17446=ORIENTED_EDGE('',*,*,#13348,.T.);
#17447=ORIENTED_EDGE('',*,*,#13484,.T.);
#17448=ORIENTED_EDGE('',*,*,#13485,.T.);
#17449=ORIENTED_EDGE('',*,*,#13481,.F.);
#17450=ORIENTED_EDGE('',*,*,#13355,.T.);
#17451=ORIENTED_EDGE('',*,*,#13486,.T.);
#17452=ORIENTED_EDGE('',*,*,#13487,.T.);
#17453=ORIENTED_EDGE('',*,*,#13484,.F.);
#17454=ORIENTED_EDGE('',*,*,#13354,.T.);
#17455=ORIENTED_EDGE('',*,*,#13488,.T.);
#17456=ORIENTED_EDGE('',*,*,#13489,.T.);
#17457=ORIENTED_EDGE('',*,*,#13486,.F.);
#17458=ORIENTED_EDGE('',*,*,#13353,.T.);
#17459=ORIENTED_EDGE('',*,*,#13490,.T.);
#17460=ORIENTED_EDGE('',*,*,#13491,.T.);
#17461=ORIENTED_EDGE('',*,*,#13488,.F.);
#17462=ORIENTED_EDGE('',*,*,#13352,.T.);
#17463=ORIENTED_EDGE('',*,*,#13492,.T.);
#17464=ORIENTED_EDGE('',*,*,#13493,.T.);
#17465=ORIENTED_EDGE('',*,*,#13490,.F.);
#17466=ORIENTED_EDGE('',*,*,#13351,.T.);
#17467=ORIENTED_EDGE('',*,*,#13494,.T.);
#17468=ORIENTED_EDGE('',*,*,#13495,.T.);
#17469=ORIENTED_EDGE('',*,*,#13492,.F.);
#17470=ORIENTED_EDGE('',*,*,#13350,.T.);
#17471=ORIENTED_EDGE('',*,*,#13483,.F.);
#17472=ORIENTED_EDGE('',*,*,#13496,.T.);
#17473=ORIENTED_EDGE('',*,*,#13494,.F.);
#17474=ORIENTED_EDGE('',*,*,#13349,.T.);
#17475=ORIENTED_EDGE('',*,*,#13493,.F.);
#17476=ORIENTED_EDGE('',*,*,#13497,.T.);
#17477=ORIENTED_EDGE('',*,*,#13498,.F.);
#17478=ORIENTED_EDGE('',*,*,#13499,.T.);
#17479=ORIENTED_EDGE('',*,*,#13495,.F.);
#17480=ORIENTED_EDGE('',*,*,#13500,.F.);
#17481=ORIENTED_EDGE('',*,*,#13501,.F.);
#17482=ORIENTED_EDGE('',*,*,#13497,.F.);
#17483=ORIENTED_EDGE('',*,*,#13496,.F.);
#17484=ORIENTED_EDGE('',*,*,#13502,.F.);
#17485=ORIENTED_EDGE('',*,*,#13503,.F.);
#17486=ORIENTED_EDGE('',*,*,#13500,.T.);
#17487=ORIENTED_EDGE('',*,*,#13482,.F.);
#17488=ORIENTED_EDGE('',*,*,#13504,.F.);
#17489=ORIENTED_EDGE('',*,*,#13505,.F.);
#17490=ORIENTED_EDGE('',*,*,#13502,.T.);
#17491=ORIENTED_EDGE('',*,*,#13506,.T.);
#17492=ORIENTED_EDGE('',*,*,#13498,.T.);
#17493=ORIENTED_EDGE('',*,*,#13507,.T.);
#17494=ORIENTED_EDGE('',*,*,#13508,.T.);
#17495=ORIENTED_EDGE('',*,*,#13509,.T.);
#17496=ORIENTED_EDGE('',*,*,#13510,.T.);
#17497=ORIENTED_EDGE('',*,*,#13506,.F.);
#17498=ORIENTED_EDGE('',*,*,#13511,.T.);
#17499=ORIENTED_EDGE('',*,*,#13512,.T.);
#17500=ORIENTED_EDGE('',*,*,#13513,.T.);
#17501=ORIENTED_EDGE('',*,*,#13514,.T.);
#17502=ORIENTED_EDGE('',*,*,#13515,.T.);
#17503=ORIENTED_EDGE('',*,*,#13509,.F.);
#17504=ORIENTED_EDGE('',*,*,#13516,.T.);
#17505=ORIENTED_EDGE('',*,*,#13517,.T.);
#17506=ORIENTED_EDGE('',*,*,#13518,.T.);
#17507=ORIENTED_EDGE('',*,*,#13514,.F.);
#17508=ORIENTED_EDGE('',*,*,#13519,.T.);
#17509=ORIENTED_EDGE('',*,*,#13520,.T.);
#17510=ORIENTED_EDGE('',*,*,#13521,.T.);
#17511=ORIENTED_EDGE('',*,*,#13517,.F.);
#17512=ORIENTED_EDGE('',*,*,#13460,.T.);
#17513=ORIENTED_EDGE('',*,*,#13522,.T.);
#17514=ORIENTED_EDGE('',*,*,#13505,.T.);
#17515=ORIENTED_EDGE('',*,*,#13520,.F.);
#17516=ORIENTED_EDGE('',*,*,#13523,.T.);
#17517=ORIENTED_EDGE('',*,*,#13443,.T.);
#17518=ORIENTED_EDGE('',*,*,#13524,.T.);
#17519=ORIENTED_EDGE('',*,*,#13525,.T.);
#17520=ORIENTED_EDGE('',*,*,#13503,.T.);
#17521=ORIENTED_EDGE('',*,*,#13522,.F.);
#17522=ORIENTED_EDGE('',*,*,#13526,.T.);
#17523=ORIENTED_EDGE('',*,*,#13507,.F.);
#17524=ORIENTED_EDGE('',*,*,#13501,.T.);
#17525=ORIENTED_EDGE('',*,*,#13525,.F.);
#17526=ORIENTED_EDGE('',*,*,#13527,.T.);
#17527=ORIENTED_EDGE('',*,*,#13516,.F.);
#17528=ORIENTED_EDGE('',*,*,#13528,.F.);
#17529=ORIENTED_EDGE('',*,*,#13529,.F.);
#17530=ORIENTED_EDGE('',*,*,#13530,.T.);
#17531=ORIENTED_EDGE('',*,*,#13513,.F.);
#17532=ORIENTED_EDGE('',*,*,#13531,.T.);
#17533=ORIENTED_EDGE('',*,*,#13532,.T.);
#17534=ORIENTED_EDGE('',*,*,#13511,.F.);
#17535=ORIENTED_EDGE('',*,*,#13533,.F.);
#17536=ORIENTED_EDGE('',*,*,#13534,.F.);
#17537=ORIENTED_EDGE('',*,*,#13528,.T.);
#17538=ORIENTED_EDGE('',*,*,#13508,.F.);
#17539=ORIENTED_EDGE('',*,*,#13535,.F.);
#17540=ORIENTED_EDGE('',*,*,#13536,.F.);
#17541=ORIENTED_EDGE('',*,*,#13537,.F.);
#17542=ORIENTED_EDGE('',*,*,#13538,.F.);
#17543=ORIENTED_EDGE('',*,*,#13467,.F.);
#17544=ORIENTED_EDGE('',*,*,#13472,.F.);
#17545=ORIENTED_EDGE('',*,*,#13533,.T.);
#17546=ORIENTED_EDGE('',*,*,#13527,.F.);
#17547=ORIENTED_EDGE('',*,*,#13539,.F.);
#17548=ORIENTED_EDGE('',*,*,#13540,.F.);
#17549=ORIENTED_EDGE('',*,*,#13535,.T.);
#17550=ORIENTED_EDGE('',*,*,#13524,.F.);
#17551=ORIENTED_EDGE('',*,*,#13442,.T.);
#17552=ORIENTED_EDGE('',*,*,#13444,.T.);
#17553=ORIENTED_EDGE('',*,*,#13526,.F.);
#17554=ORIENTED_EDGE('',*,*,#13541,.F.);
#17555=ORIENTED_EDGE('',*,*,#13542,.F.);
#17556=ORIENTED_EDGE('',*,*,#13539,.T.);
#17557=ORIENTED_EDGE('',*,*,#13543,.T.);
#17558=ORIENTED_EDGE('',*,*,#13544,.T.);
#17559=ORIENTED_EDGE('',*,*,#13454,.F.);
#17560=ORIENTED_EDGE('',*,*,#13545,.T.);
#17561=ORIENTED_EDGE('',*,*,#13546,.T.);
#17562=ORIENTED_EDGE('',*,*,#13547,.T.);
#17563=ORIENTED_EDGE('',*,*,#13543,.F.);
#17564=ORIENTED_EDGE('',*,*,#13529,.T.);
#17565=ORIENTED_EDGE('',*,*,#13471,.T.);
#17566=ORIENTED_EDGE('',*,*,#13548,.T.);
#17567=ORIENTED_EDGE('',*,*,#13546,.F.);
#17568=ORIENTED_EDGE('',*,*,#13534,.T.);
#17569=ORIENTED_EDGE('',*,*,#13477,.F.);
#17570=ORIENTED_EDGE('',*,*,#13473,.T.);
#17571=ORIENTED_EDGE('',*,*,#13455,.F.);
#17572=ORIENTED_EDGE('',*,*,#13549,.F.);
#17573=ORIENTED_EDGE('',*,*,#13550,.T.);
#17574=ORIENTED_EDGE('',*,*,#13544,.F.);
#17575=ORIENTED_EDGE('',*,*,#13551,.F.);
#17576=ORIENTED_EDGE('',*,*,#13552,.T.);
#17577=ORIENTED_EDGE('',*,*,#13549,.T.);
#17578=ORIENTED_EDGE('',*,*,#13547,.F.);
#17579=ORIENTED_EDGE('',*,*,#13553,.F.);
#17580=ORIENTED_EDGE('',*,*,#13554,.T.);
#17581=ORIENTED_EDGE('',*,*,#13551,.T.);
#17582=ORIENTED_EDGE('',*,*,#13548,.F.);
#17583=ORIENTED_EDGE('',*,*,#13480,.F.);
#17584=ORIENTED_EDGE('',*,*,#13555,.T.);
#17585=ORIENTED_EDGE('',*,*,#13553,.T.);
#17586=ORIENTED_EDGE('',*,*,#13556,.F.);
#17587=ORIENTED_EDGE('',*,*,#13557,.F.);
#17588=ORIENTED_EDGE('',*,*,#13558,.F.);
#17589=ORIENTED_EDGE('',*,*,#13559,.F.);
#17590=ORIENTED_EDGE('',*,*,#13560,.F.);
#17591=ORIENTED_EDGE('',*,*,#13561,.F.);
#17592=ORIENTED_EDGE('',*,*,#13562,.T.);
#17593=ORIENTED_EDGE('',*,*,#13563,.T.);
#17594=ORIENTED_EDGE('',*,*,#13557,.T.);
#17595=ORIENTED_EDGE('',*,*,#13564,.T.);
#17596=ORIENTED_EDGE('',*,*,#13565,.T.);
#17597=ORIENTED_EDGE('',*,*,#13566,.T.);
#17598=ORIENTED_EDGE('',*,*,#13562,.F.);
#17599=ORIENTED_EDGE('',*,*,#13567,.T.);
#17600=ORIENTED_EDGE('',*,*,#13568,.T.);
#17601=ORIENTED_EDGE('',*,*,#13569,.T.);
#17602=ORIENTED_EDGE('',*,*,#13565,.F.);
#17603=ORIENTED_EDGE('',*,*,#13570,.T.);
#17604=ORIENTED_EDGE('',*,*,#13571,.T.);
#17605=ORIENTED_EDGE('',*,*,#13572,.T.);
#17606=ORIENTED_EDGE('',*,*,#13568,.F.);
#17607=ORIENTED_EDGE('',*,*,#13573,.T.);
#17608=ORIENTED_EDGE('',*,*,#13571,.F.);
#17609=ORIENTED_EDGE('',*,*,#13574,.T.);
#17610=ORIENTED_EDGE('',*,*,#13560,.T.);
#17611=ORIENTED_EDGE('',*,*,#13575,.T.);
#17612=ORIENTED_EDGE('',*,*,#13556,.T.);
#17613=ORIENTED_EDGE('',*,*,#13576,.T.);
#17614=ORIENTED_EDGE('',*,*,#13561,.T.);
#17615=ORIENTED_EDGE('',*,*,#13577,.T.);
#17616=ORIENTED_EDGE('',*,*,#13578,.F.);
#17617=ORIENTED_EDGE('',*,*,#13579,.F.);
#17618=ORIENTED_EDGE('',*,*,#13580,.F.);
#17619=ORIENTED_EDGE('',*,*,#13581,.F.);
#17620=ORIENTED_EDGE('',*,*,#13582,.F.);
#17621=ORIENTED_EDGE('',*,*,#13583,.F.);
#17622=ORIENTED_EDGE('',*,*,#13584,.F.);
#17623=ORIENTED_EDGE('',*,*,#13585,.F.);
#17624=ORIENTED_EDGE('',*,*,#13537,.T.);
#17625=ORIENTED_EDGE('',*,*,#13583,.T.);
#17626=ORIENTED_EDGE('',*,*,#13586,.T.);
#17627=ORIENTED_EDGE('',*,*,#13587,.T.);
#17628=ORIENTED_EDGE('',*,*,#13588,.T.);
#17629=ORIENTED_EDGE('',*,*,#13468,.F.);
#17630=ORIENTED_EDGE('',*,*,#13538,.T.);
#17631=ORIENTED_EDGE('',*,*,#13587,.F.);
#17632=ORIENTED_EDGE('',*,*,#13589,.T.);
#17633=ORIENTED_EDGE('',*,*,#13590,.T.);
#17634=ORIENTED_EDGE('',*,*,#13584,.T.);
#17635=ORIENTED_EDGE('',*,*,#13536,.T.);
#17636=ORIENTED_EDGE('',*,*,#13591,.T.);
#17637=ORIENTED_EDGE('',*,*,#13592,.T.);
#17638=ORIENTED_EDGE('',*,*,#13589,.F.);
#17639=ORIENTED_EDGE('',*,*,#13540,.T.);
#17640=ORIENTED_EDGE('',*,*,#13593,.T.);
#17641=ORIENTED_EDGE('',*,*,#13594,.T.);
#17642=ORIENTED_EDGE('',*,*,#13591,.F.);
#17643=ORIENTED_EDGE('',*,*,#13542,.T.);
#17644=ORIENTED_EDGE('',*,*,#13595,.T.);
#17645=ORIENTED_EDGE('',*,*,#13596,.T.);
#17646=ORIENTED_EDGE('',*,*,#13593,.F.);
#17647=ORIENTED_EDGE('',*,*,#13597,.T.);
#17648=ORIENTED_EDGE('',*,*,#13595,.F.);
#17649=ORIENTED_EDGE('',*,*,#13458,.T.);
#17650=ORIENTED_EDGE('',*,*,#13579,.T.);
#17651=ORIENTED_EDGE('',*,*,#13598,.T.);
#17652=ORIENTED_EDGE('',*,*,#13559,.T.);
#17653=ORIENTED_EDGE('',*,*,#13599,.T.);
#17654=ORIENTED_EDGE('',*,*,#13585,.T.);
#17655=ORIENTED_EDGE('',*,*,#13600,.T.);
#17656=ORIENTED_EDGE('',*,*,#13582,.T.);
#17657=ORIENTED_EDGE('',*,*,#13601,.T.);
#17658=ORIENTED_EDGE('',*,*,#13581,.T.);
#17659=ORIENTED_EDGE('',*,*,#13602,.T.);
#17660=ORIENTED_EDGE('',*,*,#13603,.T.);
#17661=ORIENTED_EDGE('',*,*,#13580,.T.);
#17662=ORIENTED_EDGE('',*,*,#13457,.T.);
#17663=ORIENTED_EDGE('',*,*,#13451,.F.);
#17664=ORIENTED_EDGE('',*,*,#13558,.T.);
#17665=ORIENTED_EDGE('',*,*,#13604,.T.);
#17666=ORIENTED_EDGE('',*,*,#13578,.T.);
#17667=ORIENTED_EDGE('',*,*,#13605,.T.);
#17668=ORIENTED_EDGE('',*,*,#13566,.F.);
#17669=ORIENTED_EDGE('',*,*,#13606,.T.);
#17670=ORIENTED_EDGE('',*,*,#13596,.F.);
#17671=ORIENTED_EDGE('',*,*,#13607,.F.);
#17672=ORIENTED_EDGE('',*,*,#13575,.F.);
#17673=ORIENTED_EDGE('',*,*,#13600,.F.);
#17674=ORIENTED_EDGE('',*,*,#13590,.F.);
#17675=ORIENTED_EDGE('',*,*,#13608,.F.);
#17676=ORIENTED_EDGE('',*,*,#13569,.F.);
#17677=ORIENTED_EDGE('',*,*,#13609,.T.);
#17678=ORIENTED_EDGE('',*,*,#13594,.F.);
#17679=ORIENTED_EDGE('',*,*,#13606,.F.);
#17680=ORIENTED_EDGE('',*,*,#13572,.F.);
#17681=ORIENTED_EDGE('',*,*,#13608,.T.);
#17682=ORIENTED_EDGE('',*,*,#13592,.F.);
#17683=ORIENTED_EDGE('',*,*,#13609,.F.);
#17684=ORIENTED_EDGE('',*,*,#13448,.F.);
#17685=ORIENTED_EDGE('',*,*,#13465,.F.);
#17686=ORIENTED_EDGE('',*,*,#13469,.F.);
#17687=ORIENTED_EDGE('',*,*,#13610,.T.);
#17688=ORIENTED_EDGE('',*,*,#13450,.F.);
#17689=ORIENTED_EDGE('',*,*,#13610,.F.);
#17690=ORIENTED_EDGE('',*,*,#13588,.F.);
#17691=ORIENTED_EDGE('',*,*,#13611,.F.);
#17692=ORIENTED_EDGE('',*,*,#13612,.T.);
#17693=ORIENTED_EDGE('',*,*,#13586,.F.);
#17694=ORIENTED_EDGE('',*,*,#13602,.F.);
#17695=ORIENTED_EDGE('',*,*,#13603,.F.);
#17696=ORIENTED_EDGE('',*,*,#13611,.T.);
#17697=ORIENTED_EDGE('',*,*,#13564,.F.);
#17698=ORIENTED_EDGE('',*,*,#13577,.F.);
#17699=ORIENTED_EDGE('',*,*,#13574,.F.);
#17700=ORIENTED_EDGE('',*,*,#13573,.F.);
#17701=ORIENTED_EDGE('',*,*,#13570,.F.);
#17702=ORIENTED_EDGE('',*,*,#13567,.F.);
#17703=ORIENTED_EDGE('',*,*,#13576,.F.);
#17704=ORIENTED_EDGE('',*,*,#13605,.F.);
#17705=ORIENTED_EDGE('',*,*,#13601,.F.);
#17706=ORIENTED_EDGE('',*,*,#13599,.F.);
#17707=ORIENTED_EDGE('',*,*,#13563,.F.);
#17708=ORIENTED_EDGE('',*,*,#13607,.T.);
#17709=ORIENTED_EDGE('',*,*,#13598,.F.);
#17710=ORIENTED_EDGE('',*,*,#13604,.F.);
#17711=ORIENTED_EDGE('',*,*,#13478,.F.);
#17712=ORIENTED_EDGE('',*,*,#13550,.F.);
#17713=ORIENTED_EDGE('',*,*,#13552,.F.);
#17714=ORIENTED_EDGE('',*,*,#13554,.F.);
#17715=ORIENTED_EDGE('',*,*,#13555,.F.);
#17716=ORIENTED_EDGE('',*,*,#13479,.F.);
#17717=ORIENTED_EDGE('',*,*,#13613,.T.);
#17718=ORIENTED_EDGE('',*,*,#13359,.T.);
#17719=ORIENTED_EDGE('',*,*,#13614,.T.);
#17720=ORIENTED_EDGE('',*,*,#13615,.T.);
#17721=ORIENTED_EDGE('',*,*,#13616,.T.);
#17722=ORIENTED_EDGE('',*,*,#13440,.T.);
#17723=ORIENTED_EDGE('',*,*,#13614,.F.);
#17724=ORIENTED_EDGE('',*,*,#13366,.T.);
#17725=ORIENTED_EDGE('',*,*,#13617,.T.);
#17726=ORIENTED_EDGE('',*,*,#13436,.T.);
#17727=ORIENTED_EDGE('',*,*,#13616,.F.);
#17728=ORIENTED_EDGE('',*,*,#13365,.T.);
#17729=ORIENTED_EDGE('',*,*,#13618,.T.);
#17730=ORIENTED_EDGE('',*,*,#13434,.T.);
#17731=ORIENTED_EDGE('',*,*,#13617,.F.);
#17732=ORIENTED_EDGE('',*,*,#13364,.T.);
#17733=ORIENTED_EDGE('',*,*,#13619,.T.);
#17734=ORIENTED_EDGE('',*,*,#13432,.T.);
#17735=ORIENTED_EDGE('',*,*,#13618,.F.);
#17736=ORIENTED_EDGE('',*,*,#13363,.T.);
#17737=ORIENTED_EDGE('',*,*,#13620,.T.);
#17738=ORIENTED_EDGE('',*,*,#13427,.T.);
#17739=ORIENTED_EDGE('',*,*,#13619,.F.);
#17740=ORIENTED_EDGE('',*,*,#13362,.T.);
#17741=ORIENTED_EDGE('',*,*,#13621,.T.);
#17742=ORIENTED_EDGE('',*,*,#13622,.T.);
#17743=ORIENTED_EDGE('',*,*,#13620,.F.);
#17744=ORIENTED_EDGE('',*,*,#13361,.T.);
#17745=ORIENTED_EDGE('',*,*,#13613,.F.);
#17746=ORIENTED_EDGE('',*,*,#13623,.T.);
#17747=ORIENTED_EDGE('',*,*,#13621,.F.);
#17748=ORIENTED_EDGE('',*,*,#13360,.T.);
#17749=ORIENTED_EDGE('',*,*,#13409,.F.);
#17750=ORIENTED_EDGE('',*,*,#13428,.T.);
#17751=ORIENTED_EDGE('',*,*,#13622,.F.);
#17752=ORIENTED_EDGE('',*,*,#13624,.F.);
#17753=ORIENTED_EDGE('',*,*,#13412,.F.);
#17754=ORIENTED_EDGE('',*,*,#13624,.T.);
#17755=ORIENTED_EDGE('',*,*,#13623,.F.);
#17756=ORIENTED_EDGE('',*,*,#13625,.F.);
#17757=ORIENTED_EDGE('',*,*,#13415,.F.);
#17758=ORIENTED_EDGE('',*,*,#13625,.T.);
#17759=ORIENTED_EDGE('',*,*,#13615,.F.);
#17760=ORIENTED_EDGE('',*,*,#13439,.F.);
#17761=ORIENTED_EDGE('',*,*,#13329,.F.);
#17762=ORIENTED_EDGE('',*,*,#13341,.F.);
#17763=ORIENTED_EDGE('',*,*,#13408,.F.);
#17764=ORIENTED_EDGE('',*,*,#13626,.T.);
#17765=ORIENTED_EDGE('',*,*,#13326,.F.);
#17766=ORIENTED_EDGE('',*,*,#13626,.F.);
#17767=ORIENTED_EDGE('',*,*,#13411,.F.);
#17768=ORIENTED_EDGE('',*,*,#13627,.T.);
#17769=ORIENTED_EDGE('',*,*,#13323,.F.);
#17770=ORIENTED_EDGE('',*,*,#13627,.F.);
#17771=ORIENTED_EDGE('',*,*,#13414,.F.);
#17772=ORIENTED_EDGE('',*,*,#13628,.T.);
#17773=ORIENTED_EDGE('',*,*,#13320,.F.);
#17774=ORIENTED_EDGE('',*,*,#13628,.F.);
#17775=ORIENTED_EDGE('',*,*,#13419,.F.);
#17776=ORIENTED_EDGE('',*,*,#13346,.T.);
#17777=ORIENTED_EDGE('',*,*,#13491,.F.);
#17778=ORIENTED_EDGE('',*,*,#13499,.F.);
#17779=ORIENTED_EDGE('',*,*,#13510,.F.);
#17780=ORIENTED_EDGE('',*,*,#13629,.T.);
#17781=ORIENTED_EDGE('',*,*,#13489,.F.);
#17782=ORIENTED_EDGE('',*,*,#13629,.F.);
#17783=ORIENTED_EDGE('',*,*,#13515,.F.);
#17784=ORIENTED_EDGE('',*,*,#13630,.T.);
#17785=ORIENTED_EDGE('',*,*,#13487,.F.);
#17786=ORIENTED_EDGE('',*,*,#13630,.F.);
#17787=ORIENTED_EDGE('',*,*,#13518,.F.);
#17788=ORIENTED_EDGE('',*,*,#13631,.T.);
#17789=ORIENTED_EDGE('',*,*,#13485,.F.);
#17790=ORIENTED_EDGE('',*,*,#13631,.F.);
#17791=ORIENTED_EDGE('',*,*,#13521,.F.);
#17792=ORIENTED_EDGE('',*,*,#13504,.T.);
#17793=ORIENTED_EDGE('',*,*,#13519,.F.);
#17794=ORIENTED_EDGE('',*,*,#13530,.F.);
#17795=ORIENTED_EDGE('',*,*,#13545,.F.);
#17796=ORIENTED_EDGE('',*,*,#13461,.T.);
#17797=ORIENTED_EDGE('',*,*,#13512,.F.);
#17798=ORIENTED_EDGE('',*,*,#13532,.F.);
#17799=ORIENTED_EDGE('',*,*,#13632,.T.);
#17800=ORIENTED_EDGE('',*,*,#13429,.F.);
#17801=ORIENTED_EDGE('',*,*,#13402,.F.);
#17802=ORIENTED_EDGE('',*,*,#13430,.F.);
#17803=ORIENTED_EDGE('',*,*,#13632,.F.);
#17804=ORIENTED_EDGE('',*,*,#13531,.F.);
#17805=ORIENTED_EDGE('',*,*,#13612,.F.);
#17806=ORIENTED_EDGE('',*,*,#13633,.T.);
#17807=ORIENTED_EDGE('',*,*,#13369,.F.);
#17808=ORIENTED_EDGE('',*,*,#13633,.F.);
#17809=ORIENTED_EDGE('',*,*,#13634,.T.);
#17810=ORIENTED_EDGE('',*,*,#13375,.T.);
#17811=ORIENTED_EDGE('',*,*,#13634,.F.);
#17812=ORIENTED_EDGE('',*,*,#13635,.T.);
#17813=ORIENTED_EDGE('',*,*,#13379,.T.);
#17814=ORIENTED_EDGE('',*,*,#13635,.F.);
#17815=ORIENTED_EDGE('',*,*,#13636,.T.);
#17816=ORIENTED_EDGE('',*,*,#13383,.T.);
#17817=ORIENTED_EDGE('',*,*,#13636,.F.);
#17818=ORIENTED_EDGE('',*,*,#13637,.T.);
#17819=ORIENTED_EDGE('',*,*,#13387,.T.);
#17820=ORIENTED_EDGE('',*,*,#13637,.F.);
#17821=ORIENTED_EDGE('',*,*,#13395,.F.);
#17822=ORIENTED_EDGE('',*,*,#13638,.T.);
#17823=ORIENTED_EDGE('',*,*,#13639,.T.);
#17824=ORIENTED_EDGE('',*,*,#13400,.F.);
#17825=ORIENTED_EDGE('',*,*,#13390,.F.);
#17826=ORIENTED_EDGE('',*,*,#13399,.T.);
#17827=ORIENTED_EDGE('',*,*,#13640,.T.);
#17828=ORIENTED_EDGE('',*,*,#13638,.F.);
#17829=ORIENTED_EDGE('',*,*,#13398,.F.);
#17830=ORIENTED_EDGE('',*,*,#13401,.F.);
#17831=ORIENTED_EDGE('',*,*,#13639,.F.);
#17832=ORIENTED_EDGE('',*,*,#13640,.F.);
#17833=ORIENTED_EDGE('',*,*,#13523,.F.);
#17834=ORIENTED_EDGE('',*,*,#13459,.F.);
#17835=ORIENTED_EDGE('',*,*,#13597,.F.);
#17836=ORIENTED_EDGE('',*,*,#13541,.T.);
#17837=ORIENTED_EDGE('',*,*,#13641,.T.);
#17838=ORIENTED_EDGE('',*,*,#13642,.T.);
#17839=ORIENTED_EDGE('',*,*,#13643,.T.);
#17840=ORIENTED_EDGE('',*,*,#13644,.T.);
#17841=ORIENTED_EDGE('',*,*,#13642,.F.);
#17842=ORIENTED_EDGE('',*,*,#13643,.F.);
#17843=ORIENTED_EDGE('',*,*,#13644,.F.);
#17844=ORIENTED_EDGE('',*,*,#13645,.T.);
#17845=ORIENTED_EDGE('',*,*,#13646,.F.);
#17846=ORIENTED_EDGE('',*,*,#13647,.F.);
#17847=ORIENTED_EDGE('',*,*,#13645,.F.);
#17848=ORIENTED_EDGE('',*,*,#13641,.F.);
#17849=ORIENTED_EDGE('',*,*,#13648,.T.);
#17850=ORIENTED_EDGE('',*,*,#13646,.T.);
#17851=ORIENTED_EDGE('',*,*,#13647,.T.);
#17852=ORIENTED_EDGE('',*,*,#13649,.T.);
#17853=ORIENTED_EDGE('',*,*,#13650,.T.);
#17854=ORIENTED_EDGE('',*,*,#13651,.T.);
#17855=ORIENTED_EDGE('',*,*,#13649,.F.);
#17856=ORIENTED_EDGE('',*,*,#13650,.F.);
#17857=ORIENTED_EDGE('',*,*,#13651,.F.);
#17858=ORIENTED_EDGE('',*,*,#13652,.T.);
#17859=ORIENTED_EDGE('',*,*,#13653,.F.);
#17860=ORIENTED_EDGE('',*,*,#13654,.F.);
#17861=ORIENTED_EDGE('',*,*,#13652,.F.);
#17862=ORIENTED_EDGE('',*,*,#13655,.T.);
#17863=ORIENTED_EDGE('',*,*,#13656,.T.);
#17864=ORIENTED_EDGE('',*,*,#13657,.T.);
#17865=ORIENTED_EDGE('',*,*,#13658,.T.);
#17866=ORIENTED_EDGE('',*,*,#13659,.T.);
#17867=ORIENTED_EDGE('',*,*,#13657,.F.);
#17868=ORIENTED_EDGE('',*,*,#13660,.T.);
#17869=ORIENTED_EDGE('',*,*,#13661,.T.);
#17870=ORIENTED_EDGE('',*,*,#13662,.T.);
#17871=ORIENTED_EDGE('',*,*,#13663,.T.);
#17872=ORIENTED_EDGE('',*,*,#13664,.T.);
#17873=ORIENTED_EDGE('',*,*,#13655,.F.);
#17874=ORIENTED_EDGE('',*,*,#13665,.T.);
#17875=ORIENTED_EDGE('',*,*,#13666,.F.);
#17876=ORIENTED_EDGE('',*,*,#13667,.T.);
#17877=ORIENTED_EDGE('',*,*,#13668,.F.);
#17878=ORIENTED_EDGE('',*,*,#13669,.T.);
#17879=ORIENTED_EDGE('',*,*,#13670,.F.);
#17880=ORIENTED_EDGE('',*,*,#13671,.T.);
#17881=ORIENTED_EDGE('',*,*,#13663,.F.);
#17882=ORIENTED_EDGE('',*,*,#13672,.F.);
#17883=ORIENTED_EDGE('',*,*,#13673,.T.);
#17884=ORIENTED_EDGE('',*,*,#13658,.F.);
#17885=ORIENTED_EDGE('',*,*,#13659,.F.);
#17886=ORIENTED_EDGE('',*,*,#13673,.F.);
#17887=ORIENTED_EDGE('',*,*,#13670,.T.);
#17888=ORIENTED_EDGE('',*,*,#13674,.T.);
#17889=ORIENTED_EDGE('',*,*,#13675,.T.);
#17890=ORIENTED_EDGE('',*,*,#13676,.T.);
#17891=ORIENTED_EDGE('',*,*,#13675,.F.);
#17892=ORIENTED_EDGE('',*,*,#13677,.T.);
#17893=ORIENTED_EDGE('',*,*,#13678,.F.);
#17894=ORIENTED_EDGE('',*,*,#13679,.T.);
#17895=ORIENTED_EDGE('',*,*,#13676,.F.);
#17896=ORIENTED_EDGE('',*,*,#13679,.F.);
#17897=ORIENTED_EDGE('',*,*,#13680,.T.);
#17898=ORIENTED_EDGE('',*,*,#13681,.T.);
#17899=ORIENTED_EDGE('',*,*,#13682,.T.);
#17900=ORIENTED_EDGE('',*,*,#13683,.T.);
#17901=ORIENTED_EDGE('',*,*,#13684,.T.);
#17902=ORIENTED_EDGE('',*,*,#13685,.T.);
#17903=ORIENTED_EDGE('',*,*,#13681,.F.);
#17904=ORIENTED_EDGE('',*,*,#13686,.F.);
#17905=ORIENTED_EDGE('',*,*,#13687,.F.);
#17906=ORIENTED_EDGE('',*,*,#13688,.F.);
#17907=ORIENTED_EDGE('',*,*,#13689,.F.);
#17908=ORIENTED_EDGE('',*,*,#13690,.F.);
#17909=ORIENTED_EDGE('',*,*,#13691,.F.);
#17910=ORIENTED_EDGE('',*,*,#13692,.F.);
#17911=ORIENTED_EDGE('',*,*,#13693,.F.);
#17912=ORIENTED_EDGE('',*,*,#13694,.F.);
#17913=ORIENTED_EDGE('',*,*,#13695,.F.);
#17914=ORIENTED_EDGE('',*,*,#13696,.F.);
#17915=ORIENTED_EDGE('',*,*,#13697,.F.);
#17916=ORIENTED_EDGE('',*,*,#13698,.F.);
#17917=ORIENTED_EDGE('',*,*,#13699,.F.);
#17918=ORIENTED_EDGE('',*,*,#13700,.F.);
#17919=ORIENTED_EDGE('',*,*,#13680,.F.);
#17920=ORIENTED_EDGE('',*,*,#13701,.F.);
#17921=ORIENTED_EDGE('',*,*,#13702,.T.);
#17922=ORIENTED_EDGE('',*,*,#13703,.T.);
#17923=ORIENTED_EDGE('',*,*,#13686,.T.);
#17924=ORIENTED_EDGE('',*,*,#13685,.F.);
#17925=ORIENTED_EDGE('',*,*,#13704,.T.);
#17926=ORIENTED_EDGE('',*,*,#13705,.T.);
#17927=ORIENTED_EDGE('',*,*,#13706,.T.);
#17928=ORIENTED_EDGE('',*,*,#13701,.T.);
#17929=ORIENTED_EDGE('',*,*,#13707,.T.);
#17930=ORIENTED_EDGE('',*,*,#13708,.T.);
#17931=ORIENTED_EDGE('',*,*,#13709,.T.);
#17932=ORIENTED_EDGE('',*,*,#13708,.F.);
#17933=ORIENTED_EDGE('',*,*,#13707,.F.);
#17934=ORIENTED_EDGE('',*,*,#13710,.T.);
#17935=ORIENTED_EDGE('',*,*,#13711,.F.);
#17936=ORIENTED_EDGE('',*,*,#13710,.F.);
#17937=ORIENTED_EDGE('',*,*,#13709,.F.);
#17938=ORIENTED_EDGE('',*,*,#13712,.T.);
#17939=ORIENTED_EDGE('',*,*,#13713,.T.);
#17940=ORIENTED_EDGE('',*,*,#13714,.T.);
#17941=ORIENTED_EDGE('',*,*,#13715,.T.);
#17942=ORIENTED_EDGE('',*,*,#13713,.F.);
#17943=ORIENTED_EDGE('',*,*,#13716,.T.);
#17944=ORIENTED_EDGE('',*,*,#13717,.F.);
#17945=ORIENTED_EDGE('',*,*,#13718,.F.);
#17946=ORIENTED_EDGE('',*,*,#13719,.T.);
#17947=ORIENTED_EDGE('',*,*,#13661,.F.);
#17948=ORIENTED_EDGE('',*,*,#13662,.F.);
#17949=ORIENTED_EDGE('',*,*,#13719,.F.);
#17950=ORIENTED_EDGE('',*,*,#13720,.T.);
#17951=ORIENTED_EDGE('',*,*,#13721,.F.);
#17952=ORIENTED_EDGE('',*,*,#13722,.T.);
#17953=ORIENTED_EDGE('',*,*,#13723,.F.);
#17954=ORIENTED_EDGE('',*,*,#13724,.T.);
#17955=ORIENTED_EDGE('',*,*,#13725,.F.);
#17956=ORIENTED_EDGE('',*,*,#13726,.F.);
#17957=ORIENTED_EDGE('',*,*,#13727,.F.);
#17958=ORIENTED_EDGE('',*,*,#13653,.T.);
#17959=ORIENTED_EDGE('',*,*,#13654,.T.);
#17960=ORIENTED_EDGE('',*,*,#13716,.F.);
#17961=ORIENTED_EDGE('',*,*,#13714,.F.);
#17962=ORIENTED_EDGE('',*,*,#13715,.F.);
#17963=ORIENTED_EDGE('',*,*,#13728,.T.);
#17964=ORIENTED_EDGE('',*,*,#13729,.T.);
#17965=ORIENTED_EDGE('',*,*,#13728,.F.);
#17966=ORIENTED_EDGE('',*,*,#13711,.T.);
#17967=ORIENTED_EDGE('',*,*,#13730,.T.);
#17968=ORIENTED_EDGE('',*,*,#13717,.T.);
#17969=ORIENTED_EDGE('',*,*,#13718,.T.);
#17970=ORIENTED_EDGE('',*,*,#13730,.F.);
#17971=ORIENTED_EDGE('',*,*,#13731,.T.);
#17972=ORIENTED_EDGE('',*,*,#13732,.T.);
#17973=ORIENTED_EDGE('',*,*,#13733,.T.);
#17974=ORIENTED_EDGE('',*,*,#13734,.T.);
#17975=ORIENTED_EDGE('',*,*,#13732,.F.);
#17976=ORIENTED_EDGE('',*,*,#13735,.T.);
#17977=ORIENTED_EDGE('',*,*,#13736,.F.);
#17978=ORIENTED_EDGE('',*,*,#13737,.T.);
#17979=ORIENTED_EDGE('',*,*,#13731,.F.);
#17980=ORIENTED_EDGE('',*,*,#13738,.T.);
#17981=ORIENTED_EDGE('',*,*,#13739,.T.);
#17982=ORIENTED_EDGE('',*,*,#13740,.T.);
#17983=ORIENTED_EDGE('',*,*,#13741,.T.);
#17984=ORIENTED_EDGE('',*,*,#13742,.F.);
#17985=ORIENTED_EDGE('',*,*,#13743,.T.);
#17986=ORIENTED_EDGE('',*,*,#13744,.T.);
#17987=ORIENTED_EDGE('',*,*,#13745,.T.);
#17988=ORIENTED_EDGE('',*,*,#13746,.F.);
#17989=ORIENTED_EDGE('',*,*,#13747,.T.);
#17990=ORIENTED_EDGE('',*,*,#13748,.T.);
#17991=ORIENTED_EDGE('',*,*,#13746,.T.);
#17992=ORIENTED_EDGE('',*,*,#13749,.T.);
#17993=ORIENTED_EDGE('',*,*,#13750,.T.);
#17994=ORIENTED_EDGE('',*,*,#13751,.T.);
#17995=ORIENTED_EDGE('',*,*,#13682,.F.);
#17996=ORIENTED_EDGE('',*,*,#13692,.T.);
#17997=ORIENTED_EDGE('',*,*,#13752,.T.);
#17998=ORIENTED_EDGE('',*,*,#13753,.T.);
#17999=ORIENTED_EDGE('',*,*,#13754,.T.);
#18000=ORIENTED_EDGE('',*,*,#13683,.F.);
#18001=ORIENTED_EDGE('',*,*,#13754,.F.);
#18002=ORIENTED_EDGE('',*,*,#13755,.T.);
#18003=ORIENTED_EDGE('',*,*,#13756,.T.);
#18004=ORIENTED_EDGE('',*,*,#13757,.T.);
#18005=ORIENTED_EDGE('',*,*,#13758,.F.);
#18006=ORIENTED_EDGE('',*,*,#13759,.F.);
#18007=ORIENTED_EDGE('',*,*,#13760,.F.);
#18008=ORIENTED_EDGE('',*,*,#13761,.T.);
#18009=ORIENTED_EDGE('',*,*,#13759,.T.);
#18010=ORIENTED_EDGE('',*,*,#13762,.T.);
#18011=ORIENTED_EDGE('',*,*,#13763,.T.);
#18012=ORIENTED_EDGE('',*,*,#13764,.F.);
#18013=ORIENTED_EDGE('',*,*,#13765,.F.);
#18014=ORIENTED_EDGE('',*,*,#13766,.F.);
#18015=ORIENTED_EDGE('',*,*,#13767,.T.);
#18016=ORIENTED_EDGE('',*,*,#13768,.T.);
#18017=ORIENTED_EDGE('',*,*,#13765,.T.);
#18018=ORIENTED_EDGE('',*,*,#13769,.T.);
#18019=ORIENTED_EDGE('',*,*,#13770,.T.);
#18020=ORIENTED_EDGE('',*,*,#13771,.T.);
#18021=ORIENTED_EDGE('',*,*,#13767,.F.);
#18022=ORIENTED_EDGE('',*,*,#13772,.T.);
#18023=ORIENTED_EDGE('',*,*,#13773,.T.);
#18024=ORIENTED_EDGE('',*,*,#13774,.T.);
#18025=ORIENTED_EDGE('',*,*,#13770,.F.);
#18026=ORIENTED_EDGE('',*,*,#13775,.T.);
#18027=ORIENTED_EDGE('',*,*,#13776,.T.);
#18028=ORIENTED_EDGE('',*,*,#13777,.T.);
#18029=ORIENTED_EDGE('',*,*,#13773,.F.);
#18030=ORIENTED_EDGE('',*,*,#13778,.T.);
#18031=ORIENTED_EDGE('',*,*,#13776,.F.);
#18032=ORIENTED_EDGE('',*,*,#13779,.T.);
#18033=ORIENTED_EDGE('',*,*,#13760,.T.);
#18034=ORIENTED_EDGE('',*,*,#13780,.T.);
#18035=ORIENTED_EDGE('',*,*,#13781,.T.);
#18036=ORIENTED_EDGE('',*,*,#13766,.T.);
#18037=ORIENTED_EDGE('',*,*,#13782,.T.);
#18038=ORIENTED_EDGE('',*,*,#13783,.T.);
#18039=ORIENTED_EDGE('',*,*,#13758,.T.);
#18040=ORIENTED_EDGE('',*,*,#13784,.T.);
#18041=ORIENTED_EDGE('',*,*,#13764,.T.);
#18042=ORIENTED_EDGE('',*,*,#13785,.T.);
#18043=ORIENTED_EDGE('',*,*,#13786,.T.);
#18044=ORIENTED_EDGE('',*,*,#13783,.F.);
#18045=ORIENTED_EDGE('',*,*,#13787,.T.);
#18046=ORIENTED_EDGE('',*,*,#13705,.F.);
#18047=ORIENTED_EDGE('',*,*,#13788,.T.);
#18048=ORIENTED_EDGE('',*,*,#13763,.F.);
#18049=ORIENTED_EDGE('',*,*,#13789,.T.);
#18050=ORIENTED_EDGE('',*,*,#13756,.F.);
#18051=ORIENTED_EDGE('',*,*,#13703,.F.);
#18052=ORIENTED_EDGE('',*,*,#13790,.T.);
#18053=ORIENTED_EDGE('',*,*,#13791,.T.);
#18054=ORIENTED_EDGE('',*,*,#13687,.T.);
#18055=ORIENTED_EDGE('',*,*,#13792,.T.);
#18056=ORIENTED_EDGE('',*,*,#13793,.T.);
#18057=ORIENTED_EDGE('',*,*,#13752,.F.);
#18058=ORIENTED_EDGE('',*,*,#13691,.T.);
#18059=ORIENTED_EDGE('',*,*,#13791,.F.);
#18060=ORIENTED_EDGE('',*,*,#13794,.T.);
#18061=ORIENTED_EDGE('',*,*,#13750,.F.);
#18062=ORIENTED_EDGE('',*,*,#13688,.T.);
#18063=ORIENTED_EDGE('',*,*,#13742,.T.);
#18064=ORIENTED_EDGE('',*,*,#13795,.T.);
#18065=ORIENTED_EDGE('',*,*,#13796,.T.);
#18066=ORIENTED_EDGE('',*,*,#13797,.T.);
#18067=ORIENTED_EDGE('',*,*,#13796,.F.);
#18068=ORIENTED_EDGE('',*,*,#13798,.T.);
#18069=ORIENTED_EDGE('',*,*,#13792,.F.);
#18070=ORIENTED_EDGE('',*,*,#13690,.T.);
#18071=ORIENTED_EDGE('',*,*,#13780,.F.);
#18072=ORIENTED_EDGE('',*,*,#13761,.F.);
#18073=ORIENTED_EDGE('',*,*,#13788,.F.);
#18074=ORIENTED_EDGE('',*,*,#13755,.F.);
#18075=ORIENTED_EDGE('',*,*,#13753,.F.);
#18076=ORIENTED_EDGE('',*,*,#13799,.T.);
#18077=ORIENTED_EDGE('',*,*,#13800,.F.);
#18078=ORIENTED_EDGE('',*,*,#13801,.F.);
#18079=ORIENTED_EDGE('',*,*,#13793,.F.);
#18080=ORIENTED_EDGE('',*,*,#13798,.F.);
#18081=ORIENTED_EDGE('',*,*,#13795,.F.);
#18082=ORIENTED_EDGE('',*,*,#13741,.F.);
#18083=ORIENTED_EDGE('',*,*,#13802,.T.);
#18084=ORIENTED_EDGE('',*,*,#13803,.F.);
#18085=ORIENTED_EDGE('',*,*,#13804,.F.);
#18086=ORIENTED_EDGE('',*,*,#13805,.F.);
#18087=ORIENTED_EDGE('',*,*,#13806,.F.);
#18088=ORIENTED_EDGE('',*,*,#13799,.F.);
#18089=ORIENTED_EDGE('',*,*,#13744,.F.);
#18090=ORIENTED_EDGE('',*,*,#13807,.F.);
#18091=ORIENTED_EDGE('',*,*,#13748,.F.);
#18092=ORIENTED_EDGE('',*,*,#13808,.T.);
#18093=ORIENTED_EDGE('',*,*,#13809,.F.);
#18094=ORIENTED_EDGE('',*,*,#13810,.F.);
#18095=ORIENTED_EDGE('',*,*,#13811,.F.);
#18096=ORIENTED_EDGE('',*,*,#13812,.F.);
#18097=ORIENTED_EDGE('',*,*,#13813,.F.);
#18098=ORIENTED_EDGE('',*,*,#13814,.F.);
#18099=ORIENTED_EDGE('',*,*,#13815,.F.);
#18100=ORIENTED_EDGE('',*,*,#13802,.F.);
#18101=ORIENTED_EDGE('',*,*,#13816,.F.);
#18102=ORIENTED_EDGE('',*,*,#13817,.F.);
#18103=ORIENTED_EDGE('',*,*,#13818,.F.);
#18104=ORIENTED_EDGE('',*,*,#13819,.F.);
#18105=ORIENTED_EDGE('',*,*,#13743,.F.);
#18106=ORIENTED_EDGE('',*,*,#13797,.F.);
#18107=ORIENTED_EDGE('',*,*,#13689,.T.);
#18108=ORIENTED_EDGE('',*,*,#13749,.F.);
#18109=ORIENTED_EDGE('',*,*,#13745,.F.);
#18110=ORIENTED_EDGE('',*,*,#13807,.T.);
#18111=ORIENTED_EDGE('',*,*,#13762,.F.);
#18112=ORIENTED_EDGE('',*,*,#13785,.F.);
#18113=ORIENTED_EDGE('',*,*,#13781,.F.);
#18114=ORIENTED_EDGE('',*,*,#13820,.T.);
#18115=ORIENTED_EDGE('',*,*,#13684,.F.);
#18116=ORIENTED_EDGE('',*,*,#13757,.F.);
#18117=ORIENTED_EDGE('',*,*,#13821,.T.);
#18118=ORIENTED_EDGE('',*,*,#13704,.F.);
#18119=ORIENTED_EDGE('',*,*,#13789,.F.);
#18120=ORIENTED_EDGE('',*,*,#13820,.F.);
#18121=ORIENTED_EDGE('',*,*,#13786,.F.);
#18122=ORIENTED_EDGE('',*,*,#13821,.F.);
#18123=ORIENTED_EDGE('',*,*,#13769,.F.);
#18124=ORIENTED_EDGE('',*,*,#13784,.F.);
#18125=ORIENTED_EDGE('',*,*,#13779,.F.);
#18126=ORIENTED_EDGE('',*,*,#13778,.F.);
#18127=ORIENTED_EDGE('',*,*,#13775,.F.);
#18128=ORIENTED_EDGE('',*,*,#13772,.F.);
#18129=ORIENTED_EDGE('',*,*,#13822,.F.);
#18130=ORIENTED_EDGE('',*,*,#13823,.F.);
#18131=ORIENTED_EDGE('',*,*,#13824,.F.);
#18132=ORIENTED_EDGE('',*,*,#13825,.F.);
#18133=ORIENTED_EDGE('',*,*,#13826,.F.);
#18134=ORIENTED_EDGE('',*,*,#13827,.F.);
#18135=ORIENTED_EDGE('',*,*,#13828,.F.);
#18136=ORIENTED_EDGE('',*,*,#13829,.F.);
#18137=ORIENTED_EDGE('',*,*,#13830,.T.);
#18138=ORIENTED_EDGE('',*,*,#13697,.T.);
#18139=ORIENTED_EDGE('',*,*,#13831,.T.);
#18140=ORIENTED_EDGE('',*,*,#13832,.T.);
#18141=ORIENTED_EDGE('',*,*,#13833,.T.);
#18142=ORIENTED_EDGE('',*,*,#13698,.T.);
#18143=ORIENTED_EDGE('',*,*,#13830,.F.);
#18144=ORIENTED_EDGE('',*,*,#13834,.T.);
#18145=ORIENTED_EDGE('',*,*,#13835,.T.);
#18146=ORIENTED_EDGE('',*,*,#13699,.T.);
#18147=ORIENTED_EDGE('',*,*,#13833,.F.);
#18148=ORIENTED_EDGE('',*,*,#13836,.T.);
#18149=ORIENTED_EDGE('',*,*,#13831,.F.);
#18150=ORIENTED_EDGE('',*,*,#13700,.T.);
#18151=ORIENTED_EDGE('',*,*,#13835,.F.);
#18152=ORIENTED_EDGE('',*,*,#13837,.T.);
#18153=ORIENTED_EDGE('',*,*,#13834,.F.);
#18154=ORIENTED_EDGE('',*,*,#13838,.F.);
#18155=ORIENTED_EDGE('',*,*,#13839,.F.);
#18156=ORIENTED_EDGE('',*,*,#13840,.T.);
#18157=ORIENTED_EDGE('',*,*,#13832,.F.);
#18158=ORIENTED_EDGE('',*,*,#13841,.F.);
#18159=ORIENTED_EDGE('',*,*,#13842,.F.);
#18160=ORIENTED_EDGE('',*,*,#13838,.T.);
#18161=ORIENTED_EDGE('',*,*,#13843,.T.);
#18162=ORIENTED_EDGE('',*,*,#13822,.T.);
#18163=ORIENTED_EDGE('',*,*,#13844,.T.);
#18164=ORIENTED_EDGE('',*,*,#13845,.T.);
#18165=ORIENTED_EDGE('',*,*,#13846,.T.);
#18166=ORIENTED_EDGE('',*,*,#13823,.T.);
#18167=ORIENTED_EDGE('',*,*,#13843,.F.);
#18168=ORIENTED_EDGE('',*,*,#13847,.T.);
#18169=ORIENTED_EDGE('',*,*,#13848,.T.);
#18170=ORIENTED_EDGE('',*,*,#13824,.T.);
#18171=ORIENTED_EDGE('',*,*,#13846,.F.);
#18172=ORIENTED_EDGE('',*,*,#13849,.T.);
#18173=ORIENTED_EDGE('',*,*,#13844,.F.);
#18174=ORIENTED_EDGE('',*,*,#13825,.T.);
#18175=ORIENTED_EDGE('',*,*,#13848,.F.);
#18176=ORIENTED_EDGE('',*,*,#13850,.T.);
#18177=ORIENTED_EDGE('',*,*,#13847,.F.);
#18178=ORIENTED_EDGE('',*,*,#13851,.F.);
#18179=ORIENTED_EDGE('',*,*,#13852,.F.);
#18180=ORIENTED_EDGE('',*,*,#13853,.T.);
#18181=ORIENTED_EDGE('',*,*,#13845,.F.);
#18182=ORIENTED_EDGE('',*,*,#13854,.F.);
#18183=ORIENTED_EDGE('',*,*,#13855,.F.);
#18184=ORIENTED_EDGE('',*,*,#13851,.T.);
#18185=ORIENTED_EDGE('',*,*,#13856,.T.);
#18186=ORIENTED_EDGE('',*,*,#13826,.T.);
#18187=ORIENTED_EDGE('',*,*,#13857,.T.);
#18188=ORIENTED_EDGE('',*,*,#13858,.T.);
#18189=ORIENTED_EDGE('',*,*,#13859,.T.);
#18190=ORIENTED_EDGE('',*,*,#13827,.T.);
#18191=ORIENTED_EDGE('',*,*,#13856,.F.);
#18192=ORIENTED_EDGE('',*,*,#13860,.T.);
#18193=ORIENTED_EDGE('',*,*,#13861,.T.);
#18194=ORIENTED_EDGE('',*,*,#13828,.T.);
#18195=ORIENTED_EDGE('',*,*,#13859,.F.);
#18196=ORIENTED_EDGE('',*,*,#13862,.T.);
#18197=ORIENTED_EDGE('',*,*,#13857,.F.);
#18198=ORIENTED_EDGE('',*,*,#13829,.T.);
#18199=ORIENTED_EDGE('',*,*,#13861,.F.);
#18200=ORIENTED_EDGE('',*,*,#13863,.T.);
#18201=ORIENTED_EDGE('',*,*,#13860,.F.);
#18202=ORIENTED_EDGE('',*,*,#13864,.F.);
#18203=ORIENTED_EDGE('',*,*,#13865,.F.);
#18204=ORIENTED_EDGE('',*,*,#13866,.T.);
#18205=ORIENTED_EDGE('',*,*,#13858,.F.);
#18206=ORIENTED_EDGE('',*,*,#13867,.F.);
#18207=ORIENTED_EDGE('',*,*,#13868,.F.);
#18208=ORIENTED_EDGE('',*,*,#13864,.T.);
#18209=ORIENTED_EDGE('',*,*,#13869,.T.);
#18210=ORIENTED_EDGE('',*,*,#13693,.T.);
#18211=ORIENTED_EDGE('',*,*,#13870,.T.);
#18212=ORIENTED_EDGE('',*,*,#13871,.T.);
#18213=ORIENTED_EDGE('',*,*,#13872,.T.);
#18214=ORIENTED_EDGE('',*,*,#13694,.T.);
#18215=ORIENTED_EDGE('',*,*,#13869,.F.);
#18216=ORIENTED_EDGE('',*,*,#13873,.T.);
#18217=ORIENTED_EDGE('',*,*,#13874,.T.);
#18218=ORIENTED_EDGE('',*,*,#13695,.T.);
#18219=ORIENTED_EDGE('',*,*,#13872,.F.);
#18220=ORIENTED_EDGE('',*,*,#13875,.T.);
#18221=ORIENTED_EDGE('',*,*,#13870,.F.);
#18222=ORIENTED_EDGE('',*,*,#13696,.T.);
#18223=ORIENTED_EDGE('',*,*,#13874,.F.);
#18224=ORIENTED_EDGE('',*,*,#13876,.T.);
#18225=ORIENTED_EDGE('',*,*,#13873,.F.);
#18226=ORIENTED_EDGE('',*,*,#13877,.F.);
#18227=ORIENTED_EDGE('',*,*,#13878,.F.);
#18228=ORIENTED_EDGE('',*,*,#13879,.T.);
#18229=ORIENTED_EDGE('',*,*,#13871,.F.);
#18230=ORIENTED_EDGE('',*,*,#13880,.F.);
#18231=ORIENTED_EDGE('',*,*,#13881,.F.);
#18232=ORIENTED_EDGE('',*,*,#13877,.T.);
#18233=ORIENTED_EDGE('',*,*,#13666,.T.);
#18234=ORIENTED_EDGE('',*,*,#13882,.T.);
#18235=ORIENTED_EDGE('',*,*,#13883,.T.);
#18236=ORIENTED_EDGE('',*,*,#13884,.T.);
#18237=ORIENTED_EDGE('',*,*,#13885,.T.);
#18238=ORIENTED_EDGE('',*,*,#13883,.F.);
#18239=ORIENTED_EDGE('',*,*,#13886,.T.);
#18240=ORIENTED_EDGE('',*,*,#13887,.F.);
#18241=ORIENTED_EDGE('',*,*,#13888,.T.);
#18242=ORIENTED_EDGE('',*,*,#13884,.F.);
#18243=ORIENTED_EDGE('',*,*,#13885,.F.);
#18244=ORIENTED_EDGE('',*,*,#13888,.F.);
#18245=ORIENTED_EDGE('',*,*,#13668,.T.);
#18246=ORIENTED_EDGE('',*,*,#13889,.T.);
#18247=ORIENTED_EDGE('',*,*,#13890,.T.);
#18248=ORIENTED_EDGE('',*,*,#13891,.T.);
#18249=ORIENTED_EDGE('',*,*,#13890,.F.);
#18250=ORIENTED_EDGE('',*,*,#13892,.T.);
#18251=ORIENTED_EDGE('',*,*,#13893,.F.);
#18252=ORIENTED_EDGE('',*,*,#13894,.T.);
#18253=ORIENTED_EDGE('',*,*,#13891,.F.);
#18254=ORIENTED_EDGE('',*,*,#13894,.F.);
#18255=ORIENTED_EDGE('',*,*,#13895,.T.);
#18256=ORIENTED_EDGE('',*,*,#13896,.T.);
#18257=ORIENTED_EDGE('',*,*,#13897,.T.);
#18258=ORIENTED_EDGE('',*,*,#13881,.T.);
#18259=ORIENTED_EDGE('',*,*,#13898,.T.);
#18260=ORIENTED_EDGE('',*,*,#13899,.T.);
#18261=ORIENTED_EDGE('',*,*,#13895,.F.);
#18262=ORIENTED_EDGE('',*,*,#13900,.T.);
#18263=ORIENTED_EDGE('',*,*,#13901,.T.);
#18264=ORIENTED_EDGE('',*,*,#13902,.T.);
#18265=ORIENTED_EDGE('',*,*,#13898,.F.);
#18266=ORIENTED_EDGE('',*,*,#13903,.T.);
#18267=ORIENTED_EDGE('',*,*,#13897,.F.);
#18268=ORIENTED_EDGE('',*,*,#13904,.T.);
#18269=ORIENTED_EDGE('',*,*,#13901,.F.);
#18270=ORIENTED_EDGE('',*,*,#13878,.T.);
#18271=ORIENTED_EDGE('',*,*,#13876,.F.);
#18272=ORIENTED_EDGE('',*,*,#13905,.F.);
#18273=ORIENTED_EDGE('',*,*,#13900,.F.);
#18274=ORIENTED_EDGE('',*,*,#13880,.T.);
#18275=ORIENTED_EDGE('',*,*,#13906,.F.);
#18276=ORIENTED_EDGE('',*,*,#13907,.F.);
#18277=ORIENTED_EDGE('',*,*,#13908,.F.);
#18278=ORIENTED_EDGE('',*,*,#13909,.F.);
#18279=ORIENTED_EDGE('',*,*,#13910,.F.);
#18280=ORIENTED_EDGE('',*,*,#13911,.F.);
#18281=ORIENTED_EDGE('',*,*,#13912,.T.);
#18282=ORIENTED_EDGE('',*,*,#13913,.F.);
#18283=ORIENTED_EDGE('',*,*,#13914,.F.);
#18284=ORIENTED_EDGE('',*,*,#13733,.F.);
#18285=ORIENTED_EDGE('',*,*,#13737,.F.);
#18286=ORIENTED_EDGE('',*,*,#13915,.F.);
#18287=ORIENTED_EDGE('',*,*,#13916,.T.);
#18288=ORIENTED_EDGE('',*,*,#13917,.F.);
#18289=ORIENTED_EDGE('',*,*,#13918,.F.);
#18290=ORIENTED_EDGE('',*,*,#13919,.F.);
#18291=ORIENTED_EDGE('',*,*,#13920,.F.);
#18292=ORIENTED_EDGE('',*,*,#13921,.F.);
#18293=ORIENTED_EDGE('',*,*,#13922,.F.);
#18294=ORIENTED_EDGE('',*,*,#13923,.F.);
#18295=ORIENTED_EDGE('',*,*,#13924,.F.);
#18296=ORIENTED_EDGE('',*,*,#13925,.F.);
#18297=ORIENTED_EDGE('',*,*,#13926,.F.);
#18298=ORIENTED_EDGE('',*,*,#13927,.F.);
#18299=ORIENTED_EDGE('',*,*,#13928,.F.);
#18300=ORIENTED_EDGE('',*,*,#13929,.F.);
#18301=ORIENTED_EDGE('',*,*,#13930,.F.);
#18302=ORIENTED_EDGE('',*,*,#13931,.F.);
#18303=ORIENTED_EDGE('',*,*,#13932,.F.);
#18304=ORIENTED_EDGE('',*,*,#13933,.F.);
#18305=ORIENTED_EDGE('',*,*,#13934,.F.);
#18306=ORIENTED_EDGE('',*,*,#13935,.F.);
#18307=ORIENTED_EDGE('',*,*,#13936,.F.);
#18308=ORIENTED_EDGE('',*,*,#13937,.F.);
#18309=ORIENTED_EDGE('',*,*,#13896,.F.);
#18310=ORIENTED_EDGE('',*,*,#13899,.F.);
#18311=ORIENTED_EDGE('',*,*,#13902,.F.);
#18312=ORIENTED_EDGE('',*,*,#13904,.F.);
#18313=ORIENTED_EDGE('',*,*,#13938,.T.);
#18314=ORIENTED_EDGE('',*,*,#13926,.T.);
#18315=ORIENTED_EDGE('',*,*,#13939,.T.);
#18316=ORIENTED_EDGE('',*,*,#13868,.T.);
#18317=ORIENTED_EDGE('',*,*,#13940,.T.);
#18318=ORIENTED_EDGE('',*,*,#13927,.T.);
#18319=ORIENTED_EDGE('',*,*,#13938,.F.);
#18320=ORIENTED_EDGE('',*,*,#13941,.T.);
#18321=ORIENTED_EDGE('',*,*,#13942,.T.);
#18322=ORIENTED_EDGE('',*,*,#13928,.T.);
#18323=ORIENTED_EDGE('',*,*,#13940,.F.);
#18324=ORIENTED_EDGE('',*,*,#13943,.T.);
#18325=ORIENTED_EDGE('',*,*,#13939,.F.);
#18326=ORIENTED_EDGE('',*,*,#13929,.T.);
#18327=ORIENTED_EDGE('',*,*,#13942,.F.);
#18328=ORIENTED_EDGE('',*,*,#13865,.T.);
#18329=ORIENTED_EDGE('',*,*,#13863,.F.);
#18330=ORIENTED_EDGE('',*,*,#13944,.F.);
#18331=ORIENTED_EDGE('',*,*,#13941,.F.);
#18332=ORIENTED_EDGE('',*,*,#13867,.T.);
#18333=ORIENTED_EDGE('',*,*,#13945,.T.);
#18334=ORIENTED_EDGE('',*,*,#13934,.T.);
#18335=ORIENTED_EDGE('',*,*,#13946,.T.);
#18336=ORIENTED_EDGE('',*,*,#13855,.T.);
#18337=ORIENTED_EDGE('',*,*,#13947,.T.);
#18338=ORIENTED_EDGE('',*,*,#13935,.T.);
#18339=ORIENTED_EDGE('',*,*,#13945,.F.);
#18340=ORIENTED_EDGE('',*,*,#13948,.T.);
#18341=ORIENTED_EDGE('',*,*,#13949,.T.);
#18342=ORIENTED_EDGE('',*,*,#13936,.T.);
#18343=ORIENTED_EDGE('',*,*,#13947,.F.);
#18344=ORIENTED_EDGE('',*,*,#13950,.T.);
#18345=ORIENTED_EDGE('',*,*,#13946,.F.);
#18346=ORIENTED_EDGE('',*,*,#13937,.T.);
#18347=ORIENTED_EDGE('',*,*,#13949,.F.);
#18348=ORIENTED_EDGE('',*,*,#13852,.T.);
#18349=ORIENTED_EDGE('',*,*,#13850,.F.);
#18350=ORIENTED_EDGE('',*,*,#13951,.F.);
#18351=ORIENTED_EDGE('',*,*,#13948,.F.);
#18352=ORIENTED_EDGE('',*,*,#13854,.T.);
#18353=ORIENTED_EDGE('',*,*,#13952,.T.);
#18354=ORIENTED_EDGE('',*,*,#13930,.T.);
#18355=ORIENTED_EDGE('',*,*,#13953,.T.);
#18356=ORIENTED_EDGE('',*,*,#13842,.T.);
#18357=ORIENTED_EDGE('',*,*,#13954,.T.);
#18358=ORIENTED_EDGE('',*,*,#13931,.T.);
#18359=ORIENTED_EDGE('',*,*,#13952,.F.);
#18360=ORIENTED_EDGE('',*,*,#13955,.T.);
#18361=ORIENTED_EDGE('',*,*,#13956,.T.);
#18362=ORIENTED_EDGE('',*,*,#13932,.T.);
#18363=ORIENTED_EDGE('',*,*,#13954,.F.);
#18364=ORIENTED_EDGE('',*,*,#13957,.T.);
#18365=ORIENTED_EDGE('',*,*,#13953,.F.);
#18366=ORIENTED_EDGE('',*,*,#13933,.T.);
#18367=ORIENTED_EDGE('',*,*,#13956,.F.);
#18368=ORIENTED_EDGE('',*,*,#13839,.T.);
#18369=ORIENTED_EDGE('',*,*,#13837,.F.);
#18370=ORIENTED_EDGE('',*,*,#13958,.F.);
#18371=ORIENTED_EDGE('',*,*,#13955,.F.);
#18372=ORIENTED_EDGE('',*,*,#13841,.T.);
#18373=ORIENTED_EDGE('',*,*,#13959,.T.);
#18374=ORIENTED_EDGE('',*,*,#13960,.F.);
#18375=ORIENTED_EDGE('',*,*,#13803,.T.);
#18376=ORIENTED_EDGE('',*,*,#13815,.T.);
#18377=ORIENTED_EDGE('',*,*,#13961,.T.);
#18378=ORIENTED_EDGE('',*,*,#13962,.F.);
#18379=ORIENTED_EDGE('',*,*,#13963,.T.);
#18380=ORIENTED_EDGE('',*,*,#13809,.T.);
#18381=ORIENTED_EDGE('',*,*,#13962,.T.);
#18382=ORIENTED_EDGE('',*,*,#13964,.T.);
#18383=ORIENTED_EDGE('',*,*,#13965,.T.);
#18384=ORIENTED_EDGE('',*,*,#13966,.T.);
#18385=ORIENTED_EDGE('',*,*,#13967,.T.);
#18386=ORIENTED_EDGE('',*,*,#13919,.T.);
#18387=ORIENTED_EDGE('',*,*,#13968,.T.);
#18388=ORIENTED_EDGE('',*,*,#13969,.T.);
#18389=ORIENTED_EDGE('',*,*,#13970,.T.);
#18390=ORIENTED_EDGE('',*,*,#13920,.T.);
#18391=ORIENTED_EDGE('',*,*,#13967,.F.);
#18392=ORIENTED_EDGE('',*,*,#13971,.T.);
#18393=ORIENTED_EDGE('',*,*,#13972,.T.);
#18394=ORIENTED_EDGE('',*,*,#13921,.T.);
#18395=ORIENTED_EDGE('',*,*,#13970,.F.);
#18396=ORIENTED_EDGE('',*,*,#13973,.T.);
#18397=ORIENTED_EDGE('',*,*,#13974,.T.);
#18398=ORIENTED_EDGE('',*,*,#13922,.T.);
#18399=ORIENTED_EDGE('',*,*,#13972,.F.);
#18400=ORIENTED_EDGE('',*,*,#13975,.T.);
#18401=ORIENTED_EDGE('',*,*,#13976,.T.);
#18402=ORIENTED_EDGE('',*,*,#13923,.T.);
#18403=ORIENTED_EDGE('',*,*,#13974,.F.);
#18404=ORIENTED_EDGE('',*,*,#13977,.T.);
#18405=ORIENTED_EDGE('',*,*,#13978,.T.);
#18406=ORIENTED_EDGE('',*,*,#13924,.T.);
#18407=ORIENTED_EDGE('',*,*,#13976,.F.);
#18408=ORIENTED_EDGE('',*,*,#13800,.T.);
#18409=ORIENTED_EDGE('',*,*,#13979,.T.);
#18410=ORIENTED_EDGE('',*,*,#13925,.T.);
#18411=ORIENTED_EDGE('',*,*,#13978,.F.);
#18412=ORIENTED_EDGE('',*,*,#13806,.T.);
#18413=ORIENTED_EDGE('',*,*,#13968,.F.);
#18414=ORIENTED_EDGE('',*,*,#13918,.T.);
#18415=ORIENTED_EDGE('',*,*,#13965,.F.);
#18416=ORIENTED_EDGE('',*,*,#13980,.T.);
#18417=ORIENTED_EDGE('',*,*,#13960,.T.);
#18418=ORIENTED_EDGE('',*,*,#13981,.T.);
#18419=ORIENTED_EDGE('',*,*,#13982,.T.);
#18420=ORIENTED_EDGE('',*,*,#13804,.T.);
#18421=ORIENTED_EDGE('',*,*,#13982,.F.);
#18422=ORIENTED_EDGE('',*,*,#13906,.T.);
#18423=ORIENTED_EDGE('',*,*,#13979,.F.);
#18424=ORIENTED_EDGE('',*,*,#13805,.T.);
#18425=ORIENTED_EDGE('',*,*,#13981,.F.);
#18426=ORIENTED_EDGE('',*,*,#13959,.F.);
#18427=ORIENTED_EDGE('',*,*,#13814,.T.);
#18428=ORIENTED_EDGE('',*,*,#13983,.F.);
#18429=ORIENTED_EDGE('',*,*,#13907,.T.);
#18430=ORIENTED_EDGE('',*,*,#13777,.F.);
#18431=ORIENTED_EDGE('',*,*,#13801,.T.);
#18432=ORIENTED_EDGE('',*,*,#13977,.F.);
#18433=ORIENTED_EDGE('',*,*,#13984,.F.);
#18434=ORIENTED_EDGE('',*,*,#13774,.F.);
#18435=ORIENTED_EDGE('',*,*,#13984,.T.);
#18436=ORIENTED_EDGE('',*,*,#13975,.F.);
#18437=ORIENTED_EDGE('',*,*,#13985,.F.);
#18438=ORIENTED_EDGE('',*,*,#13771,.F.);
#18439=ORIENTED_EDGE('',*,*,#13985,.T.);
#18440=ORIENTED_EDGE('',*,*,#13973,.F.);
#18441=ORIENTED_EDGE('',*,*,#13986,.F.);
#18442=ORIENTED_EDGE('',*,*,#13768,.F.);
#18443=ORIENTED_EDGE('',*,*,#13986,.T.);
#18444=ORIENTED_EDGE('',*,*,#13971,.F.);
#18445=ORIENTED_EDGE('',*,*,#13987,.F.);
#18446=ORIENTED_EDGE('',*,*,#13702,.F.);
#18447=ORIENTED_EDGE('',*,*,#13706,.F.);
#18448=ORIENTED_EDGE('',*,*,#13787,.F.);
#18449=ORIENTED_EDGE('',*,*,#13782,.F.);
#18450=ORIENTED_EDGE('',*,*,#13988,.T.);
#18451=ORIENTED_EDGE('',*,*,#13911,.T.);
#18452=ORIENTED_EDGE('',*,*,#13989,.T.);
#18453=ORIENTED_EDGE('',*,*,#13990,.T.);
#18454=ORIENTED_EDGE('',*,*,#13991,.T.);
#18455=ORIENTED_EDGE('',*,*,#13992,.T.);
#18456=ORIENTED_EDGE('',*,*,#13993,.T.);
#18457=ORIENTED_EDGE('',*,*,#13990,.F.);
#18458=ORIENTED_EDGE('',*,*,#13994,.T.);
#18459=ORIENTED_EDGE('',*,*,#13995,.T.);
#18460=ORIENTED_EDGE('',*,*,#13996,.T.);
#18461=ORIENTED_EDGE('',*,*,#13997,.T.);
#18462=ORIENTED_EDGE('',*,*,#13994,.F.);
#18463=ORIENTED_EDGE('',*,*,#13998,.T.);
#18464=ORIENTED_EDGE('',*,*,#13992,.F.);
#18465=ORIENTED_EDGE('',*,*,#13999,.T.);
#18466=ORIENTED_EDGE('',*,*,#13739,.F.);
#18467=ORIENTED_EDGE('',*,*,#14000,.T.);
#18468=ORIENTED_EDGE('',*,*,#13996,.F.);
#18469=ORIENTED_EDGE('',*,*,#14001,.T.);
#18470=ORIENTED_EDGE('',*,*,#13988,.F.);
#18471=ORIENTED_EDGE('',*,*,#13993,.F.);
#18472=ORIENTED_EDGE('',*,*,#13998,.F.);
#18473=ORIENTED_EDGE('',*,*,#14002,.T.);
#18474=ORIENTED_EDGE('',*,*,#14003,.F.);
#18475=ORIENTED_EDGE('',*,*,#13912,.F.);
#18476=ORIENTED_EDGE('',*,*,#13997,.F.);
#18477=ORIENTED_EDGE('',*,*,#14004,.T.);
#18478=ORIENTED_EDGE('',*,*,#14005,.F.);
#18479=ORIENTED_EDGE('',*,*,#14002,.F.);
#18480=ORIENTED_EDGE('',*,*,#13734,.F.);
#18481=ORIENTED_EDGE('',*,*,#13914,.T.);
#18482=ORIENTED_EDGE('',*,*,#14006,.F.);
#18483=ORIENTED_EDGE('',*,*,#14004,.F.);
#18484=ORIENTED_EDGE('',*,*,#14000,.F.);
#18485=ORIENTED_EDGE('',*,*,#13738,.F.);
#18486=ORIENTED_EDGE('',*,*,#14007,.T.);
#18487=ORIENTED_EDGE('',*,*,#13909,.T.);
#18488=ORIENTED_EDGE('',*,*,#14008,.T.);
#18489=ORIENTED_EDGE('',*,*,#14009,.T.);
#18490=ORIENTED_EDGE('',*,*,#14010,.T.);
#18491=ORIENTED_EDGE('',*,*,#14011,.T.);
#18492=ORIENTED_EDGE('',*,*,#13723,.T.);
#18493=ORIENTED_EDGE('',*,*,#14012,.T.);
#18494=ORIENTED_EDGE('',*,*,#14009,.F.);
#18495=ORIENTED_EDGE('',*,*,#13989,.F.);
#18496=ORIENTED_EDGE('',*,*,#13910,.T.);
#18497=ORIENTED_EDGE('',*,*,#14007,.F.);
#18498=ORIENTED_EDGE('',*,*,#14013,.T.);
#18499=ORIENTED_EDGE('',*,*,#13991,.F.);
#18500=ORIENTED_EDGE('',*,*,#14013,.F.);
#18501=ORIENTED_EDGE('',*,*,#14010,.F.);
#18502=ORIENTED_EDGE('',*,*,#14012,.F.);
#18503=ORIENTED_EDGE('',*,*,#13722,.F.);
#18504=ORIENTED_EDGE('',*,*,#14014,.F.);
#18505=ORIENTED_EDGE('',*,*,#14015,.F.);
#18506=ORIENTED_EDGE('',*,*,#13735,.F.);
#18507=ORIENTED_EDGE('',*,*,#13740,.F.);
#18508=ORIENTED_EDGE('',*,*,#14001,.F.);
#18509=ORIENTED_EDGE('',*,*,#13995,.F.);
#18510=ORIENTED_EDGE('',*,*,#13999,.F.);
#18511=ORIENTED_EDGE('',*,*,#14016,.T.);
#18512=ORIENTED_EDGE('',*,*,#13915,.T.);
#18513=ORIENTED_EDGE('',*,*,#13736,.T.);
#18514=ORIENTED_EDGE('',*,*,#14015,.T.);
#18515=ORIENTED_EDGE('',*,*,#14017,.T.);
#18516=ORIENTED_EDGE('',*,*,#14014,.T.);
#18517=ORIENTED_EDGE('',*,*,#13721,.T.);
#18518=ORIENTED_EDGE('',*,*,#14018,.T.);
#18519=ORIENTED_EDGE('',*,*,#14017,.F.);
#18520=ORIENTED_EDGE('',*,*,#14016,.F.);
#18521=ORIENTED_EDGE('',*,*,#14018,.F.);
#18522=ORIENTED_EDGE('',*,*,#13720,.F.);
#18523=ORIENTED_EDGE('',*,*,#14019,.F.);
#18524=ORIENTED_EDGE('',*,*,#14020,.F.);
#18525=ORIENTED_EDGE('',*,*,#13916,.F.);
#18526=ORIENTED_EDGE('',*,*,#14021,.T.);
#18527=ORIENTED_EDGE('',*,*,#13811,.T.);
#18528=ORIENTED_EDGE('',*,*,#14022,.T.);
#18529=ORIENTED_EDGE('',*,*,#14020,.T.);
#18530=ORIENTED_EDGE('',*,*,#13727,.T.);
#18531=ORIENTED_EDGE('',*,*,#14023,.T.);
#18532=ORIENTED_EDGE('',*,*,#14021,.F.);
#18533=ORIENTED_EDGE('',*,*,#14019,.T.);
#18534=ORIENTED_EDGE('',*,*,#14024,.T.);
#18535=ORIENTED_EDGE('',*,*,#14025,.T.);
#18536=ORIENTED_EDGE('',*,*,#13725,.T.);
#18537=ORIENTED_EDGE('',*,*,#14026,.T.);
#18538=ORIENTED_EDGE('',*,*,#13983,.T.);
#18539=ORIENTED_EDGE('',*,*,#13813,.T.);
#18540=ORIENTED_EDGE('',*,*,#14024,.F.);
#18541=ORIENTED_EDGE('',*,*,#14027,.T.);
#18542=ORIENTED_EDGE('',*,*,#14008,.F.);
#18543=ORIENTED_EDGE('',*,*,#13908,.T.);
#18544=ORIENTED_EDGE('',*,*,#14027,.F.);
#18545=ORIENTED_EDGE('',*,*,#14026,.F.);
#18546=ORIENTED_EDGE('',*,*,#13724,.F.);
#18547=ORIENTED_EDGE('',*,*,#14011,.F.);
#18548=ORIENTED_EDGE('',*,*,#14003,.T.);
#18549=ORIENTED_EDGE('',*,*,#14028,.T.);
#18550=ORIENTED_EDGE('',*,*,#13816,.T.);
#18551=ORIENTED_EDGE('',*,*,#14029,.T.);
#18552=ORIENTED_EDGE('',*,*,#13913,.T.);
#18553=ORIENTED_EDGE('',*,*,#14029,.F.);
#18554=ORIENTED_EDGE('',*,*,#13819,.T.);
#18555=ORIENTED_EDGE('',*,*,#14030,.T.);
#18556=ORIENTED_EDGE('',*,*,#14031,.T.);
#18557=ORIENTED_EDGE('',*,*,#13817,.T.);
#18558=ORIENTED_EDGE('',*,*,#14028,.F.);
#18559=ORIENTED_EDGE('',*,*,#14005,.T.);
#18560=ORIENTED_EDGE('',*,*,#13818,.T.);
#18561=ORIENTED_EDGE('',*,*,#14031,.F.);
#18562=ORIENTED_EDGE('',*,*,#14006,.T.);
#18563=ORIENTED_EDGE('',*,*,#14030,.F.);
#18564=ORIENTED_EDGE('',*,*,#13966,.F.);
#18565=ORIENTED_EDGE('',*,*,#13917,.T.);
#18566=ORIENTED_EDGE('',*,*,#14022,.F.);
#18567=ORIENTED_EDGE('',*,*,#13810,.T.);
#18568=ORIENTED_EDGE('',*,*,#13963,.F.);
#18569=ORIENTED_EDGE('',*,*,#13790,.F.);
#18570=ORIENTED_EDGE('',*,*,#13987,.T.);
#18571=ORIENTED_EDGE('',*,*,#13969,.F.);
#18572=ORIENTED_EDGE('',*,*,#13980,.F.);
#18573=ORIENTED_EDGE('',*,*,#13964,.F.);
#18574=ORIENTED_EDGE('',*,*,#13961,.F.);
#18575=ORIENTED_EDGE('',*,*,#13808,.F.);
#18576=ORIENTED_EDGE('',*,*,#13747,.F.);
#18577=ORIENTED_EDGE('',*,*,#13751,.F.);
#18578=ORIENTED_EDGE('',*,*,#13794,.F.);
#18579=ORIENTED_EDGE('',*,*,#14023,.F.);
#18580=ORIENTED_EDGE('',*,*,#13726,.T.);
#18581=ORIENTED_EDGE('',*,*,#14025,.F.);
#18582=ORIENTED_EDGE('',*,*,#13812,.T.);
#18583=ORIENTED_EDGE('',*,*,#13875,.F.);
#18584=ORIENTED_EDGE('',*,*,#13879,.F.);
#18585=ORIENTED_EDGE('',*,*,#13903,.F.);
#18586=ORIENTED_EDGE('',*,*,#13905,.T.);
#18587=ORIENTED_EDGE('',*,*,#13862,.F.);
#18588=ORIENTED_EDGE('',*,*,#13866,.F.);
#18589=ORIENTED_EDGE('',*,*,#13943,.F.);
#18590=ORIENTED_EDGE('',*,*,#13944,.T.);
#18591=ORIENTED_EDGE('',*,*,#13849,.F.);
#18592=ORIENTED_EDGE('',*,*,#13853,.F.);
#18593=ORIENTED_EDGE('',*,*,#13950,.F.);
#18594=ORIENTED_EDGE('',*,*,#13951,.T.);
#18595=ORIENTED_EDGE('',*,*,#13836,.F.);
#18596=ORIENTED_EDGE('',*,*,#13840,.F.);
#18597=ORIENTED_EDGE('',*,*,#13957,.F.);
#18598=ORIENTED_EDGE('',*,*,#13958,.T.);
#18599=ORIENTED_EDGE('',*,*,#14032,.T.);
#18600=ORIENTED_EDGE('',*,*,#13678,.T.);
#18601=ORIENTED_EDGE('',*,*,#14032,.F.);
#18602=ORIENTED_EDGE('',*,*,#14033,.T.);
#18603=ORIENTED_EDGE('',*,*,#13893,.T.);
#18604=ORIENTED_EDGE('',*,*,#14033,.F.);
#18605=ORIENTED_EDGE('',*,*,#14034,.T.);
#18606=ORIENTED_EDGE('',*,*,#13887,.T.);
#18607=ORIENTED_EDGE('',*,*,#14034,.F.);
#18608=ORIENTED_EDGE('',*,*,#14035,.T.);
#18609=ORIENTED_EDGE('',*,*,#13672,.T.);
#18610=ORIENTED_EDGE('',*,*,#14035,.F.);
#18611=ORIENTED_EDGE('',*,*,#13729,.F.);
#18612=ORIENTED_EDGE('',*,*,#14036,.T.);
#18613=ORIENTED_EDGE('',*,*,#14036,.F.);
#18614=ORIENTED_EDGE('',*,*,#14037,.T.);
#18615=ORIENTED_EDGE('',*,*,#14038,.F.);
#18616=ORIENTED_EDGE('',*,*,#14039,.F.);
#18617=ORIENTED_EDGE('',*,*,#14037,.F.);
#18618=ORIENTED_EDGE('',*,*,#14040,.F.);
#18619=ORIENTED_EDGE('',*,*,#14041,.F.);
#18620=ORIENTED_EDGE('',*,*,#14042,.T.);
#18621=ORIENTED_EDGE('',*,*,#14043,.T.);
#18622=ORIENTED_EDGE('',*,*,#14042,.F.);
#18623=ORIENTED_EDGE('',*,*,#14043,.F.);
#18624=ORIENTED_EDGE('',*,*,#14044,.T.);
#18625=ORIENTED_EDGE('',*,*,#14044,.F.);
#18626=ORIENTED_EDGE('',*,*,#14045,.T.);
#18627=ORIENTED_EDGE('',*,*,#13648,.F.);
#18628=ORIENTED_EDGE('',*,*,#14045,.F.);
#18629=ORIENTED_EDGE('',*,*,#14046,.F.);
#18630=ORIENTED_EDGE('',*,*,#14047,.T.);
#18631=ORIENTED_EDGE('',*,*,#13712,.F.);
#18632=ORIENTED_EDGE('',*,*,#14047,.F.);
#18633=ORIENTED_EDGE('',*,*,#14038,.T.);
#18634=ORIENTED_EDGE('',*,*,#14039,.T.);
#18635=ORIENTED_EDGE('',*,*,#14040,.T.);
#18636=ORIENTED_EDGE('',*,*,#14041,.T.);
#18637=ORIENTED_EDGE('',*,*,#13656,.F.);
#18638=ORIENTED_EDGE('',*,*,#13664,.F.);
#18639=ORIENTED_EDGE('',*,*,#13671,.F.);
#18640=ORIENTED_EDGE('',*,*,#13677,.F.);
#18641=ORIENTED_EDGE('',*,*,#13674,.F.);
#18642=ORIENTED_EDGE('',*,*,#13669,.F.);
#18643=ORIENTED_EDGE('',*,*,#13892,.F.);
#18644=ORIENTED_EDGE('',*,*,#13889,.F.);
#18645=ORIENTED_EDGE('',*,*,#13667,.F.);
#18646=ORIENTED_EDGE('',*,*,#13886,.F.);
#18647=ORIENTED_EDGE('',*,*,#13882,.F.);
#18648=ORIENTED_EDGE('',*,*,#13665,.F.);
#18649=ORIENTED_EDGE('',*,*,#13660,.F.);
#18650=ORIENTED_EDGE('',*,*,#14046,.T.);
#18651=ORIENTED_EDGE('',*,*,#14048,.T.);
#18652=ORIENTED_EDGE('',*,*,#14049,.T.);
#18653=ORIENTED_EDGE('',*,*,#14050,.T.);
#18654=ORIENTED_EDGE('',*,*,#14051,.T.);
#18655=ORIENTED_EDGE('',*,*,#14049,.F.);
#18656=ORIENTED_EDGE('',*,*,#14050,.F.);
#18657=ORIENTED_EDGE('',*,*,#14051,.F.);
#18658=ORIENTED_EDGE('',*,*,#14052,.T.);
#18659=ORIENTED_EDGE('',*,*,#14053,.T.);
#18660=ORIENTED_EDGE('',*,*,#14052,.F.);
#18661=ORIENTED_EDGE('',*,*,#14048,.F.);
#18662=ORIENTED_EDGE('',*,*,#14054,.F.);
#18663=ORIENTED_EDGE('',*,*,#14055,.F.);
#18664=ORIENTED_EDGE('',*,*,#14056,.T.);
#18665=ORIENTED_EDGE('',*,*,#14057,.T.);
#18666=ORIENTED_EDGE('',*,*,#14058,.F.);
#18667=ORIENTED_EDGE('',*,*,#14059,.F.);
#18668=ORIENTED_EDGE('',*,*,#14058,.T.);
#18669=ORIENTED_EDGE('',*,*,#14060,.T.);
#18670=ORIENTED_EDGE('',*,*,#14061,.F.);
#18671=ORIENTED_EDGE('',*,*,#14062,.F.);
#18672=ORIENTED_EDGE('',*,*,#14061,.T.);
#18673=ORIENTED_EDGE('',*,*,#14063,.T.);
#18674=ORIENTED_EDGE('',*,*,#14064,.F.);
#18675=ORIENTED_EDGE('',*,*,#14065,.F.);
#18676=ORIENTED_EDGE('',*,*,#14064,.T.);
#18677=ORIENTED_EDGE('',*,*,#14066,.T.);
#18678=ORIENTED_EDGE('',*,*,#14056,.F.);
#18679=ORIENTED_EDGE('',*,*,#14066,.F.);
#18680=ORIENTED_EDGE('',*,*,#14063,.F.);
#18681=ORIENTED_EDGE('',*,*,#14060,.F.);
#18682=ORIENTED_EDGE('',*,*,#14057,.F.);
#18683=ORIENTED_EDGE('',*,*,#14067,.F.);
#18684=ORIENTED_EDGE('',*,*,#14068,.T.);
#18685=ORIENTED_EDGE('',*,*,#14069,.T.);
#18686=ORIENTED_EDGE('',*,*,#14070,.F.);
#18687=ORIENTED_EDGE('',*,*,#14071,.F.);
#18688=ORIENTED_EDGE('',*,*,#14070,.T.);
#18689=ORIENTED_EDGE('',*,*,#14072,.T.);
#18690=ORIENTED_EDGE('',*,*,#14073,.F.);
#18691=ORIENTED_EDGE('',*,*,#14074,.F.);
#18692=ORIENTED_EDGE('',*,*,#14073,.T.);
#18693=ORIENTED_EDGE('',*,*,#14075,.T.);
#18694=ORIENTED_EDGE('',*,*,#14076,.F.);
#18695=ORIENTED_EDGE('',*,*,#14077,.F.);
#18696=ORIENTED_EDGE('',*,*,#14076,.T.);
#18697=ORIENTED_EDGE('',*,*,#14078,.T.);
#18698=ORIENTED_EDGE('',*,*,#14068,.F.);
#18699=ORIENTED_EDGE('',*,*,#14078,.F.);
#18700=ORIENTED_EDGE('',*,*,#14075,.F.);
#18701=ORIENTED_EDGE('',*,*,#14072,.F.);
#18702=ORIENTED_EDGE('',*,*,#14069,.F.);
#18703=ORIENTED_EDGE('',*,*,#14079,.F.);
#18704=ORIENTED_EDGE('',*,*,#14080,.T.);
#18705=ORIENTED_EDGE('',*,*,#14081,.T.);
#18706=ORIENTED_EDGE('',*,*,#14082,.F.);
#18707=ORIENTED_EDGE('',*,*,#14083,.F.);
#18708=ORIENTED_EDGE('',*,*,#14082,.T.);
#18709=ORIENTED_EDGE('',*,*,#14084,.T.);
#18710=ORIENTED_EDGE('',*,*,#14085,.F.);
#18711=ORIENTED_EDGE('',*,*,#14086,.F.);
#18712=ORIENTED_EDGE('',*,*,#14085,.T.);
#18713=ORIENTED_EDGE('',*,*,#14087,.T.);
#18714=ORIENTED_EDGE('',*,*,#14088,.F.);
#18715=ORIENTED_EDGE('',*,*,#14089,.F.);
#18716=ORIENTED_EDGE('',*,*,#14088,.T.);
#18717=ORIENTED_EDGE('',*,*,#14090,.T.);
#18718=ORIENTED_EDGE('',*,*,#14080,.F.);
#18719=ORIENTED_EDGE('',*,*,#14090,.F.);
#18720=ORIENTED_EDGE('',*,*,#14087,.F.);
#18721=ORIENTED_EDGE('',*,*,#14084,.F.);
#18722=ORIENTED_EDGE('',*,*,#14081,.F.);
#18723=ORIENTED_EDGE('',*,*,#14091,.F.);
#18724=ORIENTED_EDGE('',*,*,#14092,.T.);
#18725=ORIENTED_EDGE('',*,*,#14093,.T.);
#18726=ORIENTED_EDGE('',*,*,#14094,.F.);
#18727=ORIENTED_EDGE('',*,*,#14095,.F.);
#18728=ORIENTED_EDGE('',*,*,#14094,.T.);
#18729=ORIENTED_EDGE('',*,*,#14096,.T.);
#18730=ORIENTED_EDGE('',*,*,#14097,.F.);
#18731=ORIENTED_EDGE('',*,*,#14098,.F.);
#18732=ORIENTED_EDGE('',*,*,#14097,.T.);
#18733=ORIENTED_EDGE('',*,*,#14099,.T.);
#18734=ORIENTED_EDGE('',*,*,#14100,.F.);
#18735=ORIENTED_EDGE('',*,*,#14101,.F.);
#18736=ORIENTED_EDGE('',*,*,#14100,.T.);
#18737=ORIENTED_EDGE('',*,*,#14102,.T.);
#18738=ORIENTED_EDGE('',*,*,#14092,.F.);
#18739=ORIENTED_EDGE('',*,*,#14102,.F.);
#18740=ORIENTED_EDGE('',*,*,#14099,.F.);
#18741=ORIENTED_EDGE('',*,*,#14096,.F.);
#18742=ORIENTED_EDGE('',*,*,#14093,.F.);
#18743=ORIENTED_EDGE('',*,*,#14103,.F.);
#18744=ORIENTED_EDGE('',*,*,#14104,.T.);
#18745=ORIENTED_EDGE('',*,*,#14105,.T.);
#18746=ORIENTED_EDGE('',*,*,#14106,.F.);
#18747=ORIENTED_EDGE('',*,*,#14107,.F.);
#18748=ORIENTED_EDGE('',*,*,#14106,.T.);
#18749=ORIENTED_EDGE('',*,*,#14108,.T.);
#18750=ORIENTED_EDGE('',*,*,#14109,.F.);
#18751=ORIENTED_EDGE('',*,*,#14110,.F.);
#18752=ORIENTED_EDGE('',*,*,#14109,.T.);
#18753=ORIENTED_EDGE('',*,*,#14111,.T.);
#18754=ORIENTED_EDGE('',*,*,#14112,.F.);
#18755=ORIENTED_EDGE('',*,*,#14113,.F.);
#18756=ORIENTED_EDGE('',*,*,#14112,.T.);
#18757=ORIENTED_EDGE('',*,*,#14114,.T.);
#18758=ORIENTED_EDGE('',*,*,#14104,.F.);
#18759=ORIENTED_EDGE('',*,*,#14114,.F.);
#18760=ORIENTED_EDGE('',*,*,#14111,.F.);
#18761=ORIENTED_EDGE('',*,*,#14108,.F.);
#18762=ORIENTED_EDGE('',*,*,#14105,.F.);
#18763=ORIENTED_EDGE('',*,*,#14115,.F.);
#18764=ORIENTED_EDGE('',*,*,#14116,.T.);
#18765=ORIENTED_EDGE('',*,*,#14117,.T.);
#18766=ORIENTED_EDGE('',*,*,#14118,.F.);
#18767=ORIENTED_EDGE('',*,*,#14119,.F.);
#18768=ORIENTED_EDGE('',*,*,#14118,.T.);
#18769=ORIENTED_EDGE('',*,*,#14120,.T.);
#18770=ORIENTED_EDGE('',*,*,#14121,.F.);
#18771=ORIENTED_EDGE('',*,*,#14122,.F.);
#18772=ORIENTED_EDGE('',*,*,#14121,.T.);
#18773=ORIENTED_EDGE('',*,*,#14123,.T.);
#18774=ORIENTED_EDGE('',*,*,#14124,.F.);
#18775=ORIENTED_EDGE('',*,*,#14125,.F.);
#18776=ORIENTED_EDGE('',*,*,#14124,.T.);
#18777=ORIENTED_EDGE('',*,*,#14126,.T.);
#18778=ORIENTED_EDGE('',*,*,#14116,.F.);
#18779=ORIENTED_EDGE('',*,*,#14126,.F.);
#18780=ORIENTED_EDGE('',*,*,#14123,.F.);
#18781=ORIENTED_EDGE('',*,*,#14120,.F.);
#18782=ORIENTED_EDGE('',*,*,#14117,.F.);
#18783=ORIENTED_EDGE('',*,*,#14127,.F.);
#18784=ORIENTED_EDGE('',*,*,#14128,.T.);
#18785=ORIENTED_EDGE('',*,*,#14129,.T.);
#18786=ORIENTED_EDGE('',*,*,#14130,.F.);
#18787=ORIENTED_EDGE('',*,*,#14131,.F.);
#18788=ORIENTED_EDGE('',*,*,#14130,.T.);
#18789=ORIENTED_EDGE('',*,*,#14132,.T.);
#18790=ORIENTED_EDGE('',*,*,#14133,.F.);
#18791=ORIENTED_EDGE('',*,*,#14134,.F.);
#18792=ORIENTED_EDGE('',*,*,#14133,.T.);
#18793=ORIENTED_EDGE('',*,*,#14135,.T.);
#18794=ORIENTED_EDGE('',*,*,#14136,.F.);
#18795=ORIENTED_EDGE('',*,*,#14137,.F.);
#18796=ORIENTED_EDGE('',*,*,#14136,.T.);
#18797=ORIENTED_EDGE('',*,*,#14138,.T.);
#18798=ORIENTED_EDGE('',*,*,#14128,.F.);
#18799=ORIENTED_EDGE('',*,*,#14138,.F.);
#18800=ORIENTED_EDGE('',*,*,#14135,.F.);
#18801=ORIENTED_EDGE('',*,*,#14132,.F.);
#18802=ORIENTED_EDGE('',*,*,#14129,.F.);
#18803=ORIENTED_EDGE('',*,*,#14139,.F.);
#18804=ORIENTED_EDGE('',*,*,#14140,.T.);
#18805=ORIENTED_EDGE('',*,*,#14141,.T.);
#18806=ORIENTED_EDGE('',*,*,#14142,.F.);
#18807=ORIENTED_EDGE('',*,*,#14143,.F.);
#18808=ORIENTED_EDGE('',*,*,#14142,.T.);
#18809=ORIENTED_EDGE('',*,*,#14144,.T.);
#18810=ORIENTED_EDGE('',*,*,#14145,.F.);
#18811=ORIENTED_EDGE('',*,*,#14146,.F.);
#18812=ORIENTED_EDGE('',*,*,#14145,.T.);
#18813=ORIENTED_EDGE('',*,*,#14147,.T.);
#18814=ORIENTED_EDGE('',*,*,#14148,.F.);
#18815=ORIENTED_EDGE('',*,*,#14149,.F.);
#18816=ORIENTED_EDGE('',*,*,#14148,.T.);
#18817=ORIENTED_EDGE('',*,*,#14150,.T.);
#18818=ORIENTED_EDGE('',*,*,#14140,.F.);
#18819=ORIENTED_EDGE('',*,*,#14150,.F.);
#18820=ORIENTED_EDGE('',*,*,#14147,.F.);
#18821=ORIENTED_EDGE('',*,*,#14144,.F.);
#18822=ORIENTED_EDGE('',*,*,#14141,.F.);
#18823=ORIENTED_EDGE('',*,*,#14151,.F.);
#18824=ORIENTED_EDGE('',*,*,#14152,.T.);
#18825=ORIENTED_EDGE('',*,*,#14153,.T.);
#18826=ORIENTED_EDGE('',*,*,#14154,.F.);
#18827=ORIENTED_EDGE('',*,*,#14155,.F.);
#18828=ORIENTED_EDGE('',*,*,#14154,.T.);
#18829=ORIENTED_EDGE('',*,*,#14156,.T.);
#18830=ORIENTED_EDGE('',*,*,#14157,.F.);
#18831=ORIENTED_EDGE('',*,*,#14158,.F.);
#18832=ORIENTED_EDGE('',*,*,#14157,.T.);
#18833=ORIENTED_EDGE('',*,*,#14159,.T.);
#18834=ORIENTED_EDGE('',*,*,#14160,.F.);
#18835=ORIENTED_EDGE('',*,*,#14161,.F.);
#18836=ORIENTED_EDGE('',*,*,#14160,.T.);
#18837=ORIENTED_EDGE('',*,*,#14162,.T.);
#18838=ORIENTED_EDGE('',*,*,#14152,.F.);
#18839=ORIENTED_EDGE('',*,*,#14162,.F.);
#18840=ORIENTED_EDGE('',*,*,#14159,.F.);
#18841=ORIENTED_EDGE('',*,*,#14156,.F.);
#18842=ORIENTED_EDGE('',*,*,#14153,.F.);
#18843=ORIENTED_EDGE('',*,*,#14163,.F.);
#18844=ORIENTED_EDGE('',*,*,#14164,.T.);
#18845=ORIENTED_EDGE('',*,*,#14165,.T.);
#18846=ORIENTED_EDGE('',*,*,#14166,.F.);
#18847=ORIENTED_EDGE('',*,*,#14167,.F.);
#18848=ORIENTED_EDGE('',*,*,#14166,.T.);
#18849=ORIENTED_EDGE('',*,*,#14168,.T.);
#18850=ORIENTED_EDGE('',*,*,#14169,.F.);
#18851=ORIENTED_EDGE('',*,*,#14170,.F.);
#18852=ORIENTED_EDGE('',*,*,#14169,.T.);
#18853=ORIENTED_EDGE('',*,*,#14171,.T.);
#18854=ORIENTED_EDGE('',*,*,#14172,.F.);
#18855=ORIENTED_EDGE('',*,*,#14173,.F.);
#18856=ORIENTED_EDGE('',*,*,#14172,.T.);
#18857=ORIENTED_EDGE('',*,*,#14174,.T.);
#18858=ORIENTED_EDGE('',*,*,#14164,.F.);
#18859=ORIENTED_EDGE('',*,*,#14174,.F.);
#18860=ORIENTED_EDGE('',*,*,#14171,.F.);
#18861=ORIENTED_EDGE('',*,*,#14168,.F.);
#18862=ORIENTED_EDGE('',*,*,#14165,.F.);
#18863=ORIENTED_EDGE('',*,*,#14175,.F.);
#18864=ORIENTED_EDGE('',*,*,#14176,.T.);
#18865=ORIENTED_EDGE('',*,*,#14177,.T.);
#18866=ORIENTED_EDGE('',*,*,#14178,.F.);
#18867=ORIENTED_EDGE('',*,*,#14179,.F.);
#18868=ORIENTED_EDGE('',*,*,#14178,.T.);
#18869=ORIENTED_EDGE('',*,*,#14180,.T.);
#18870=ORIENTED_EDGE('',*,*,#14181,.F.);
#18871=ORIENTED_EDGE('',*,*,#14182,.F.);
#18872=ORIENTED_EDGE('',*,*,#14181,.T.);
#18873=ORIENTED_EDGE('',*,*,#14183,.T.);
#18874=ORIENTED_EDGE('',*,*,#14184,.F.);
#18875=ORIENTED_EDGE('',*,*,#14185,.F.);
#18876=ORIENTED_EDGE('',*,*,#14184,.T.);
#18877=ORIENTED_EDGE('',*,*,#14186,.T.);
#18878=ORIENTED_EDGE('',*,*,#14176,.F.);
#18879=ORIENTED_EDGE('',*,*,#14186,.F.);
#18880=ORIENTED_EDGE('',*,*,#14183,.F.);
#18881=ORIENTED_EDGE('',*,*,#14180,.F.);
#18882=ORIENTED_EDGE('',*,*,#14177,.F.);
#18883=ORIENTED_EDGE('',*,*,#14187,.F.);
#18884=ORIENTED_EDGE('',*,*,#14188,.T.);
#18885=ORIENTED_EDGE('',*,*,#14189,.T.);
#18886=ORIENTED_EDGE('',*,*,#14190,.F.);
#18887=ORIENTED_EDGE('',*,*,#14191,.F.);
#18888=ORIENTED_EDGE('',*,*,#14190,.T.);
#18889=ORIENTED_EDGE('',*,*,#14192,.T.);
#18890=ORIENTED_EDGE('',*,*,#14193,.F.);
#18891=ORIENTED_EDGE('',*,*,#14194,.F.);
#18892=ORIENTED_EDGE('',*,*,#14193,.T.);
#18893=ORIENTED_EDGE('',*,*,#14195,.T.);
#18894=ORIENTED_EDGE('',*,*,#14196,.F.);
#18895=ORIENTED_EDGE('',*,*,#14197,.F.);
#18896=ORIENTED_EDGE('',*,*,#14196,.T.);
#18897=ORIENTED_EDGE('',*,*,#14198,.T.);
#18898=ORIENTED_EDGE('',*,*,#14188,.F.);
#18899=ORIENTED_EDGE('',*,*,#14198,.F.);
#18900=ORIENTED_EDGE('',*,*,#14195,.F.);
#18901=ORIENTED_EDGE('',*,*,#14192,.F.);
#18902=ORIENTED_EDGE('',*,*,#14189,.F.);
#18903=ORIENTED_EDGE('',*,*,#14199,.F.);
#18904=ORIENTED_EDGE('',*,*,#14200,.T.);
#18905=ORIENTED_EDGE('',*,*,#14201,.T.);
#18906=ORIENTED_EDGE('',*,*,#14202,.F.);
#18907=ORIENTED_EDGE('',*,*,#14203,.F.);
#18908=ORIENTED_EDGE('',*,*,#14202,.T.);
#18909=ORIENTED_EDGE('',*,*,#14204,.T.);
#18910=ORIENTED_EDGE('',*,*,#14205,.F.);
#18911=ORIENTED_EDGE('',*,*,#14206,.F.);
#18912=ORIENTED_EDGE('',*,*,#14205,.T.);
#18913=ORIENTED_EDGE('',*,*,#14207,.T.);
#18914=ORIENTED_EDGE('',*,*,#14208,.F.);
#18915=ORIENTED_EDGE('',*,*,#14209,.F.);
#18916=ORIENTED_EDGE('',*,*,#14208,.T.);
#18917=ORIENTED_EDGE('',*,*,#14210,.T.);
#18918=ORIENTED_EDGE('',*,*,#14200,.F.);
#18919=ORIENTED_EDGE('',*,*,#14210,.F.);
#18920=ORIENTED_EDGE('',*,*,#14207,.F.);
#18921=ORIENTED_EDGE('',*,*,#14204,.F.);
#18922=ORIENTED_EDGE('',*,*,#14201,.F.);
#18923=ORIENTED_EDGE('',*,*,#14211,.F.);
#18924=ORIENTED_EDGE('',*,*,#14212,.T.);
#18925=ORIENTED_EDGE('',*,*,#14213,.T.);
#18926=ORIENTED_EDGE('',*,*,#14214,.F.);
#18927=ORIENTED_EDGE('',*,*,#14215,.F.);
#18928=ORIENTED_EDGE('',*,*,#14214,.T.);
#18929=ORIENTED_EDGE('',*,*,#14216,.T.);
#18930=ORIENTED_EDGE('',*,*,#14217,.F.);
#18931=ORIENTED_EDGE('',*,*,#14218,.F.);
#18932=ORIENTED_EDGE('',*,*,#14217,.T.);
#18933=ORIENTED_EDGE('',*,*,#14219,.T.);
#18934=ORIENTED_EDGE('',*,*,#14220,.F.);
#18935=ORIENTED_EDGE('',*,*,#14221,.F.);
#18936=ORIENTED_EDGE('',*,*,#14220,.T.);
#18937=ORIENTED_EDGE('',*,*,#14222,.T.);
#18938=ORIENTED_EDGE('',*,*,#14212,.F.);
#18939=ORIENTED_EDGE('',*,*,#14222,.F.);
#18940=ORIENTED_EDGE('',*,*,#14219,.F.);
#18941=ORIENTED_EDGE('',*,*,#14216,.F.);
#18942=ORIENTED_EDGE('',*,*,#14213,.F.);
#18943=ORIENTED_EDGE('',*,*,#14223,.F.);
#18944=ORIENTED_EDGE('',*,*,#14224,.T.);
#18945=ORIENTED_EDGE('',*,*,#14225,.T.);
#18946=ORIENTED_EDGE('',*,*,#14226,.F.);
#18947=ORIENTED_EDGE('',*,*,#14227,.F.);
#18948=ORIENTED_EDGE('',*,*,#14226,.T.);
#18949=ORIENTED_EDGE('',*,*,#14228,.T.);
#18950=ORIENTED_EDGE('',*,*,#14229,.F.);
#18951=ORIENTED_EDGE('',*,*,#14230,.F.);
#18952=ORIENTED_EDGE('',*,*,#14229,.T.);
#18953=ORIENTED_EDGE('',*,*,#14231,.T.);
#18954=ORIENTED_EDGE('',*,*,#14232,.F.);
#18955=ORIENTED_EDGE('',*,*,#14233,.F.);
#18956=ORIENTED_EDGE('',*,*,#14232,.T.);
#18957=ORIENTED_EDGE('',*,*,#14234,.T.);
#18958=ORIENTED_EDGE('',*,*,#14224,.F.);
#18959=ORIENTED_EDGE('',*,*,#14234,.F.);
#18960=ORIENTED_EDGE('',*,*,#14231,.F.);
#18961=ORIENTED_EDGE('',*,*,#14228,.F.);
#18962=ORIENTED_EDGE('',*,*,#14225,.F.);
#18963=ORIENTED_EDGE('',*,*,#14235,.F.);
#18964=ORIENTED_EDGE('',*,*,#14236,.T.);
#18965=ORIENTED_EDGE('',*,*,#14237,.T.);
#18966=ORIENTED_EDGE('',*,*,#14238,.F.);
#18967=ORIENTED_EDGE('',*,*,#14239,.F.);
#18968=ORIENTED_EDGE('',*,*,#14238,.T.);
#18969=ORIENTED_EDGE('',*,*,#14240,.T.);
#18970=ORIENTED_EDGE('',*,*,#14241,.F.);
#18971=ORIENTED_EDGE('',*,*,#14242,.F.);
#18972=ORIENTED_EDGE('',*,*,#14241,.T.);
#18973=ORIENTED_EDGE('',*,*,#14243,.T.);
#18974=ORIENTED_EDGE('',*,*,#14244,.F.);
#18975=ORIENTED_EDGE('',*,*,#14245,.F.);
#18976=ORIENTED_EDGE('',*,*,#14244,.T.);
#18977=ORIENTED_EDGE('',*,*,#14246,.T.);
#18978=ORIENTED_EDGE('',*,*,#14236,.F.);
#18979=ORIENTED_EDGE('',*,*,#14246,.F.);
#18980=ORIENTED_EDGE('',*,*,#14243,.F.);
#18981=ORIENTED_EDGE('',*,*,#14240,.F.);
#18982=ORIENTED_EDGE('',*,*,#14237,.F.);
#18983=ORIENTED_EDGE('',*,*,#14247,.F.);
#18984=ORIENTED_EDGE('',*,*,#14248,.T.);
#18985=ORIENTED_EDGE('',*,*,#14249,.T.);
#18986=ORIENTED_EDGE('',*,*,#14250,.F.);
#18987=ORIENTED_EDGE('',*,*,#14251,.F.);
#18988=ORIENTED_EDGE('',*,*,#14250,.T.);
#18989=ORIENTED_EDGE('',*,*,#14252,.T.);
#18990=ORIENTED_EDGE('',*,*,#14253,.F.);
#18991=ORIENTED_EDGE('',*,*,#14254,.F.);
#18992=ORIENTED_EDGE('',*,*,#14253,.T.);
#18993=ORIENTED_EDGE('',*,*,#14255,.T.);
#18994=ORIENTED_EDGE('',*,*,#14256,.F.);
#18995=ORIENTED_EDGE('',*,*,#14257,.F.);
#18996=ORIENTED_EDGE('',*,*,#14256,.T.);
#18997=ORIENTED_EDGE('',*,*,#14258,.T.);
#18998=ORIENTED_EDGE('',*,*,#14248,.F.);
#18999=ORIENTED_EDGE('',*,*,#14258,.F.);
#19000=ORIENTED_EDGE('',*,*,#14255,.F.);
#19001=ORIENTED_EDGE('',*,*,#14252,.F.);
#19002=ORIENTED_EDGE('',*,*,#14249,.F.);
#19003=ORIENTED_EDGE('',*,*,#14259,.F.);
#19004=ORIENTED_EDGE('',*,*,#14260,.T.);
#19005=ORIENTED_EDGE('',*,*,#14261,.T.);
#19006=ORIENTED_EDGE('',*,*,#14262,.F.);
#19007=ORIENTED_EDGE('',*,*,#14263,.F.);
#19008=ORIENTED_EDGE('',*,*,#14262,.T.);
#19009=ORIENTED_EDGE('',*,*,#14264,.T.);
#19010=ORIENTED_EDGE('',*,*,#14265,.F.);
#19011=ORIENTED_EDGE('',*,*,#14266,.F.);
#19012=ORIENTED_EDGE('',*,*,#14265,.T.);
#19013=ORIENTED_EDGE('',*,*,#14267,.T.);
#19014=ORIENTED_EDGE('',*,*,#14268,.F.);
#19015=ORIENTED_EDGE('',*,*,#14269,.F.);
#19016=ORIENTED_EDGE('',*,*,#14268,.T.);
#19017=ORIENTED_EDGE('',*,*,#14270,.T.);
#19018=ORIENTED_EDGE('',*,*,#14260,.F.);
#19019=ORIENTED_EDGE('',*,*,#14270,.F.);
#19020=ORIENTED_EDGE('',*,*,#14267,.F.);
#19021=ORIENTED_EDGE('',*,*,#14264,.F.);
#19022=ORIENTED_EDGE('',*,*,#14261,.F.);
#19023=ORIENTED_EDGE('',*,*,#14271,.F.);
#19024=ORIENTED_EDGE('',*,*,#14272,.T.);
#19025=ORIENTED_EDGE('',*,*,#14273,.T.);
#19026=ORIENTED_EDGE('',*,*,#14274,.F.);
#19027=ORIENTED_EDGE('',*,*,#14275,.F.);
#19028=ORIENTED_EDGE('',*,*,#14274,.T.);
#19029=ORIENTED_EDGE('',*,*,#14276,.T.);
#19030=ORIENTED_EDGE('',*,*,#14277,.F.);
#19031=ORIENTED_EDGE('',*,*,#14278,.F.);
#19032=ORIENTED_EDGE('',*,*,#14277,.T.);
#19033=ORIENTED_EDGE('',*,*,#14279,.T.);
#19034=ORIENTED_EDGE('',*,*,#14280,.F.);
#19035=ORIENTED_EDGE('',*,*,#14281,.F.);
#19036=ORIENTED_EDGE('',*,*,#14280,.T.);
#19037=ORIENTED_EDGE('',*,*,#14282,.T.);
#19038=ORIENTED_EDGE('',*,*,#14272,.F.);
#19039=ORIENTED_EDGE('',*,*,#14282,.F.);
#19040=ORIENTED_EDGE('',*,*,#14279,.F.);
#19041=ORIENTED_EDGE('',*,*,#14276,.F.);
#19042=ORIENTED_EDGE('',*,*,#14273,.F.);
#19043=ORIENTED_EDGE('',*,*,#14283,.F.);
#19044=ORIENTED_EDGE('',*,*,#14284,.T.);
#19045=ORIENTED_EDGE('',*,*,#14285,.T.);
#19046=ORIENTED_EDGE('',*,*,#14286,.F.);
#19047=ORIENTED_EDGE('',*,*,#14287,.F.);
#19048=ORIENTED_EDGE('',*,*,#14286,.T.);
#19049=ORIENTED_EDGE('',*,*,#14288,.T.);
#19050=ORIENTED_EDGE('',*,*,#14289,.F.);
#19051=ORIENTED_EDGE('',*,*,#14290,.F.);
#19052=ORIENTED_EDGE('',*,*,#14289,.T.);
#19053=ORIENTED_EDGE('',*,*,#14291,.T.);
#19054=ORIENTED_EDGE('',*,*,#14292,.F.);
#19055=ORIENTED_EDGE('',*,*,#14293,.F.);
#19056=ORIENTED_EDGE('',*,*,#14292,.T.);
#19057=ORIENTED_EDGE('',*,*,#14294,.T.);
#19058=ORIENTED_EDGE('',*,*,#14284,.F.);
#19059=ORIENTED_EDGE('',*,*,#14294,.F.);
#19060=ORIENTED_EDGE('',*,*,#14291,.F.);
#19061=ORIENTED_EDGE('',*,*,#14288,.F.);
#19062=ORIENTED_EDGE('',*,*,#14285,.F.);
#19063=ORIENTED_EDGE('',*,*,#14295,.F.);
#19064=ORIENTED_EDGE('',*,*,#14296,.T.);
#19065=ORIENTED_EDGE('',*,*,#14297,.T.);
#19066=ORIENTED_EDGE('',*,*,#14298,.F.);
#19067=ORIENTED_EDGE('',*,*,#14299,.F.);
#19068=ORIENTED_EDGE('',*,*,#14298,.T.);
#19069=ORIENTED_EDGE('',*,*,#14300,.T.);
#19070=ORIENTED_EDGE('',*,*,#14301,.F.);
#19071=ORIENTED_EDGE('',*,*,#14302,.F.);
#19072=ORIENTED_EDGE('',*,*,#14301,.T.);
#19073=ORIENTED_EDGE('',*,*,#14303,.T.);
#19074=ORIENTED_EDGE('',*,*,#14304,.F.);
#19075=ORIENTED_EDGE('',*,*,#14305,.F.);
#19076=ORIENTED_EDGE('',*,*,#14304,.T.);
#19077=ORIENTED_EDGE('',*,*,#14306,.T.);
#19078=ORIENTED_EDGE('',*,*,#14296,.F.);
#19079=ORIENTED_EDGE('',*,*,#14306,.F.);
#19080=ORIENTED_EDGE('',*,*,#14303,.F.);
#19081=ORIENTED_EDGE('',*,*,#14300,.F.);
#19082=ORIENTED_EDGE('',*,*,#14297,.F.);
#19083=ORIENTED_EDGE('',*,*,#14307,.F.);
#19084=ORIENTED_EDGE('',*,*,#14308,.F.);
#19085=ORIENTED_EDGE('',*,*,#14309,.T.);
#19086=ORIENTED_EDGE('',*,*,#14310,.T.);
#19087=ORIENTED_EDGE('',*,*,#14311,.F.);
#19088=ORIENTED_EDGE('',*,*,#14310,.F.);
#19089=ORIENTED_EDGE('',*,*,#14312,.T.);
#19090=ORIENTED_EDGE('',*,*,#14313,.T.);
#19091=ORIENTED_EDGE('',*,*,#14314,.F.);
#19092=ORIENTED_EDGE('',*,*,#14313,.F.);
#19093=ORIENTED_EDGE('',*,*,#14315,.T.);
#19094=ORIENTED_EDGE('',*,*,#14316,.T.);
#19095=ORIENTED_EDGE('',*,*,#14317,.F.);
#19096=ORIENTED_EDGE('',*,*,#14316,.F.);
#19097=ORIENTED_EDGE('',*,*,#14318,.T.);
#19098=ORIENTED_EDGE('',*,*,#14308,.T.);
#19099=ORIENTED_EDGE('',*,*,#14312,.F.);
#19100=ORIENTED_EDGE('',*,*,#14309,.F.);
#19101=ORIENTED_EDGE('',*,*,#14318,.F.);
#19102=ORIENTED_EDGE('',*,*,#14315,.F.);
#19103=ORIENTED_EDGE('',*,*,#14319,.T.);
#19104=ORIENTED_EDGE('',*,*,#14320,.T.);
#19105=ORIENTED_EDGE('',*,*,#14321,.F.);
#19106=ORIENTED_EDGE('',*,*,#14320,.F.);
#19107=ORIENTED_EDGE('',*,*,#14322,.F.);
#19108=ORIENTED_EDGE('',*,*,#14321,.T.);
#19109=ORIENTED_EDGE('',*,*,#14323,.F.);
#19110=ORIENTED_EDGE('',*,*,#14324,.T.);
#19111=ORIENTED_EDGE('',*,*,#14322,.T.);
#19112=ORIENTED_EDGE('',*,*,#14324,.F.);
#19113=ORIENTED_EDGE('',*,*,#14053,.F.);
#19114=ORIENTED_EDGE('',*,*,#14325,.T.);
#19115=ORIENTED_EDGE('',*,*,#14323,.T.);
#19116=ORIENTED_EDGE('',*,*,#14325,.F.);
#19117=ORIENTED_EDGE('',*,*,#14062,.T.);
#19118=ORIENTED_EDGE('',*,*,#14065,.T.);
#19119=ORIENTED_EDGE('',*,*,#14055,.T.);
#19120=ORIENTED_EDGE('',*,*,#14059,.T.);
#19121=ORIENTED_EDGE('',*,*,#14074,.T.);
#19122=ORIENTED_EDGE('',*,*,#14077,.T.);
#19123=ORIENTED_EDGE('',*,*,#14067,.T.);
#19124=ORIENTED_EDGE('',*,*,#14071,.T.);
#19125=ORIENTED_EDGE('',*,*,#14086,.T.);
#19126=ORIENTED_EDGE('',*,*,#14089,.T.);
#19127=ORIENTED_EDGE('',*,*,#14079,.T.);
#19128=ORIENTED_EDGE('',*,*,#14083,.T.);
#19129=ORIENTED_EDGE('',*,*,#14098,.T.);
#19130=ORIENTED_EDGE('',*,*,#14101,.T.);
#19131=ORIENTED_EDGE('',*,*,#14091,.T.);
#19132=ORIENTED_EDGE('',*,*,#14095,.T.);
#19133=ORIENTED_EDGE('',*,*,#14110,.T.);
#19134=ORIENTED_EDGE('',*,*,#14113,.T.);
#19135=ORIENTED_EDGE('',*,*,#14103,.T.);
#19136=ORIENTED_EDGE('',*,*,#14107,.T.);
#19137=ORIENTED_EDGE('',*,*,#14122,.T.);
#19138=ORIENTED_EDGE('',*,*,#14125,.T.);
#19139=ORIENTED_EDGE('',*,*,#14115,.T.);
#19140=ORIENTED_EDGE('',*,*,#14119,.T.);
#19141=ORIENTED_EDGE('',*,*,#14134,.T.);
#19142=ORIENTED_EDGE('',*,*,#14137,.T.);
#19143=ORIENTED_EDGE('',*,*,#14127,.T.);
#19144=ORIENTED_EDGE('',*,*,#14131,.T.);
#19145=ORIENTED_EDGE('',*,*,#14146,.T.);
#19146=ORIENTED_EDGE('',*,*,#14149,.T.);
#19147=ORIENTED_EDGE('',*,*,#14139,.T.);
#19148=ORIENTED_EDGE('',*,*,#14143,.T.);
#19149=ORIENTED_EDGE('',*,*,#14158,.T.);
#19150=ORIENTED_EDGE('',*,*,#14161,.T.);
#19151=ORIENTED_EDGE('',*,*,#14151,.T.);
#19152=ORIENTED_EDGE('',*,*,#14155,.T.);
#19153=ORIENTED_EDGE('',*,*,#14170,.T.);
#19154=ORIENTED_EDGE('',*,*,#14173,.T.);
#19155=ORIENTED_EDGE('',*,*,#14163,.T.);
#19156=ORIENTED_EDGE('',*,*,#14167,.T.);
#19157=ORIENTED_EDGE('',*,*,#14182,.T.);
#19158=ORIENTED_EDGE('',*,*,#14185,.T.);
#19159=ORIENTED_EDGE('',*,*,#14175,.T.);
#19160=ORIENTED_EDGE('',*,*,#14179,.T.);
#19161=ORIENTED_EDGE('',*,*,#14194,.T.);
#19162=ORIENTED_EDGE('',*,*,#14197,.T.);
#19163=ORIENTED_EDGE('',*,*,#14187,.T.);
#19164=ORIENTED_EDGE('',*,*,#14191,.T.);
#19165=ORIENTED_EDGE('',*,*,#14206,.T.);
#19166=ORIENTED_EDGE('',*,*,#14209,.T.);
#19167=ORIENTED_EDGE('',*,*,#14199,.T.);
#19168=ORIENTED_EDGE('',*,*,#14203,.T.);
#19169=ORIENTED_EDGE('',*,*,#14218,.T.);
#19170=ORIENTED_EDGE('',*,*,#14221,.T.);
#19171=ORIENTED_EDGE('',*,*,#14211,.T.);
#19172=ORIENTED_EDGE('',*,*,#14215,.T.);
#19173=ORIENTED_EDGE('',*,*,#14230,.T.);
#19174=ORIENTED_EDGE('',*,*,#14233,.T.);
#19175=ORIENTED_EDGE('',*,*,#14223,.T.);
#19176=ORIENTED_EDGE('',*,*,#14227,.T.);
#19177=ORIENTED_EDGE('',*,*,#14242,.T.);
#19178=ORIENTED_EDGE('',*,*,#14245,.T.);
#19179=ORIENTED_EDGE('',*,*,#14235,.T.);
#19180=ORIENTED_EDGE('',*,*,#14239,.T.);
#19181=ORIENTED_EDGE('',*,*,#14254,.T.);
#19182=ORIENTED_EDGE('',*,*,#14257,.T.);
#19183=ORIENTED_EDGE('',*,*,#14247,.T.);
#19184=ORIENTED_EDGE('',*,*,#14251,.T.);
#19185=ORIENTED_EDGE('',*,*,#14266,.T.);
#19186=ORIENTED_EDGE('',*,*,#14269,.T.);
#19187=ORIENTED_EDGE('',*,*,#14259,.T.);
#19188=ORIENTED_EDGE('',*,*,#14263,.T.);
#19189=ORIENTED_EDGE('',*,*,#14278,.T.);
#19190=ORIENTED_EDGE('',*,*,#14281,.T.);
#19191=ORIENTED_EDGE('',*,*,#14271,.T.);
#19192=ORIENTED_EDGE('',*,*,#14275,.T.);
#19193=ORIENTED_EDGE('',*,*,#14290,.T.);
#19194=ORIENTED_EDGE('',*,*,#14293,.T.);
#19195=ORIENTED_EDGE('',*,*,#14283,.T.);
#19196=ORIENTED_EDGE('',*,*,#14287,.T.);
#19197=ORIENTED_EDGE('',*,*,#14302,.T.);
#19198=ORIENTED_EDGE('',*,*,#14305,.T.);
#19199=ORIENTED_EDGE('',*,*,#14295,.T.);
#19200=ORIENTED_EDGE('',*,*,#14299,.T.);
#19201=ORIENTED_EDGE('',*,*,#14314,.T.);
#19202=ORIENTED_EDGE('',*,*,#14317,.T.);
#19203=ORIENTED_EDGE('',*,*,#14307,.T.);
#19204=ORIENTED_EDGE('',*,*,#14311,.T.);
#19205=ORIENTED_EDGE('',*,*,#14054,.T.);
#19206=ORIENTED_EDGE('',*,*,#14326,.T.);
#19207=ORIENTED_EDGE('',*,*,#14327,.F.);
#19208=ORIENTED_EDGE('',*,*,#14326,.F.);
#19209=ORIENTED_EDGE('',*,*,#14327,.T.);
#19210=ORIENTED_EDGE('',*,*,#14328,.T.);
#19211=ORIENTED_EDGE('',*,*,#14329,.F.);
#19212=ORIENTED_EDGE('',*,*,#14328,.F.);
#19213=ORIENTED_EDGE('',*,*,#14329,.T.);
#19214=ORIENTED_EDGE('',*,*,#14330,.F.);
#19215=ORIENTED_EDGE('',*,*,#14330,.T.);
#19216=ORIENTED_EDGE('',*,*,#14331,.T.);
#19217=ORIENTED_EDGE('',*,*,#14332,.F.);
#19218=ORIENTED_EDGE('',*,*,#14331,.F.);
#19219=ORIENTED_EDGE('',*,*,#14319,.F.);
#19220=ORIENTED_EDGE('',*,*,#14332,.T.);
#19221=ORIENTED_EDGE('',*,*,#14333,.T.);
#19222=ORIENTED_EDGE('',*,*,#14334,.T.);
#19223=ORIENTED_EDGE('',*,*,#14335,.T.);
#19224=ORIENTED_EDGE('',*,*,#14336,.T.);
#19225=ORIENTED_EDGE('',*,*,#14337,.T.);
#19226=ORIENTED_EDGE('',*,*,#14335,.F.);
#19227=ORIENTED_EDGE('',*,*,#14336,.F.);
#19228=ORIENTED_EDGE('',*,*,#14337,.F.);
#19229=ORIENTED_EDGE('',*,*,#14338,.T.);
#19230=ORIENTED_EDGE('',*,*,#14339,.T.);
#19231=ORIENTED_EDGE('',*,*,#14338,.F.);
#19232=ORIENTED_EDGE('',*,*,#14340,.T.);
#19233=ORIENTED_EDGE('',*,*,#14333,.F.);
#19234=ORIENTED_EDGE('',*,*,#14334,.F.);
#19235=ORIENTED_EDGE('',*,*,#14340,.F.);
#19236=ORIENTED_EDGE('',*,*,#14341,.F.);
#19237=ORIENTED_EDGE('',*,*,#14342,.F.);
#19238=ORIENTED_EDGE('',*,*,#14343,.T.);
#19239=ORIENTED_EDGE('',*,*,#14341,.T.);
#19240=ORIENTED_EDGE('',*,*,#14343,.F.);
#19241=ORIENTED_EDGE('',*,*,#14339,.F.);
#19242=ORIENTED_EDGE('',*,*,#14344,.T.);
#19243=ORIENTED_EDGE('',*,*,#14342,.T.);
#19244=ORIENTED_EDGE('',*,*,#14344,.F.);
#19245=ORIENTED_EDGE('',*,*,#14345,.F.);
#19246=ORIENTED_EDGE('',*,*,#14346,.T.);
#19247=ORIENTED_EDGE('',*,*,#14347,.T.);
#19248=ORIENTED_EDGE('',*,*,#14348,.T.);
#19249=ORIENTED_EDGE('',*,*,#14349,.F.);
#19250=ORIENTED_EDGE('',*,*,#14350,.T.);
#19251=ORIENTED_EDGE('',*,*,#14345,.T.);
#19252=ORIENTED_EDGE('',*,*,#14351,.T.);
#19253=ORIENTED_EDGE('',*,*,#14352,.F.);
#19254=ORIENTED_EDGE('',*,*,#14353,.T.);
#19255=ORIENTED_EDGE('',*,*,#14349,.T.);
#19256=ORIENTED_EDGE('',*,*,#14354,.T.);
#19257=ORIENTED_EDGE('',*,*,#14355,.F.);
#19258=ORIENTED_EDGE('',*,*,#14356,.T.);
#19259=ORIENTED_EDGE('',*,*,#14352,.T.);
#19260=ORIENTED_EDGE('',*,*,#14357,.T.);
#19261=ORIENTED_EDGE('',*,*,#14358,.F.);
#19262=ORIENTED_EDGE('',*,*,#14359,.T.);
#19263=ORIENTED_EDGE('',*,*,#14355,.T.);
#19264=ORIENTED_EDGE('',*,*,#14360,.T.);
#19265=ORIENTED_EDGE('',*,*,#14361,.F.);
#19266=ORIENTED_EDGE('',*,*,#14362,.T.);
#19267=ORIENTED_EDGE('',*,*,#14358,.T.);
#19268=ORIENTED_EDGE('',*,*,#14363,.T.);
#19269=ORIENTED_EDGE('',*,*,#14364,.F.);
#19270=ORIENTED_EDGE('',*,*,#14365,.T.);
#19271=ORIENTED_EDGE('',*,*,#14361,.T.);
#19272=ORIENTED_EDGE('',*,*,#14366,.T.);
#19273=ORIENTED_EDGE('',*,*,#14367,.F.);
#19274=ORIENTED_EDGE('',*,*,#14368,.T.);
#19275=ORIENTED_EDGE('',*,*,#14364,.T.);
#19276=ORIENTED_EDGE('',*,*,#14369,.T.);
#19277=ORIENTED_EDGE('',*,*,#14370,.F.);
#19278=ORIENTED_EDGE('',*,*,#14371,.T.);
#19279=ORIENTED_EDGE('',*,*,#14367,.T.);
#19280=ORIENTED_EDGE('',*,*,#14372,.T.);
#19281=ORIENTED_EDGE('',*,*,#14373,.F.);
#19282=ORIENTED_EDGE('',*,*,#14374,.T.);
#19283=ORIENTED_EDGE('',*,*,#14370,.T.);
#19284=ORIENTED_EDGE('',*,*,#14375,.T.);
#19285=ORIENTED_EDGE('',*,*,#14376,.F.);
#19286=ORIENTED_EDGE('',*,*,#14377,.T.);
#19287=ORIENTED_EDGE('',*,*,#14373,.T.);
#19288=ORIENTED_EDGE('',*,*,#14378,.T.);
#19289=ORIENTED_EDGE('',*,*,#14379,.F.);
#19290=ORIENTED_EDGE('',*,*,#14380,.T.);
#19291=ORIENTED_EDGE('',*,*,#14376,.T.);
#19292=ORIENTED_EDGE('',*,*,#14381,.T.);
#19293=ORIENTED_EDGE('',*,*,#14382,.F.);
#19294=ORIENTED_EDGE('',*,*,#14383,.T.);
#19295=ORIENTED_EDGE('',*,*,#14379,.T.);
#19296=ORIENTED_EDGE('',*,*,#14384,.T.);
#19297=ORIENTED_EDGE('',*,*,#14385,.F.);
#19298=ORIENTED_EDGE('',*,*,#14386,.T.);
#19299=ORIENTED_EDGE('',*,*,#14382,.T.);
#19300=ORIENTED_EDGE('',*,*,#14387,.T.);
#19301=ORIENTED_EDGE('',*,*,#14388,.F.);
#19302=ORIENTED_EDGE('',*,*,#14389,.T.);
#19303=ORIENTED_EDGE('',*,*,#14385,.T.);
#19304=ORIENTED_EDGE('',*,*,#14390,.T.);
#19305=ORIENTED_EDGE('',*,*,#14391,.F.);
#19306=ORIENTED_EDGE('',*,*,#14392,.T.);
#19307=ORIENTED_EDGE('',*,*,#14388,.T.);
#19308=ORIENTED_EDGE('',*,*,#14393,.T.);
#19309=ORIENTED_EDGE('',*,*,#14394,.F.);
#19310=ORIENTED_EDGE('',*,*,#14395,.T.);
#19311=ORIENTED_EDGE('',*,*,#14391,.T.);
#19312=ORIENTED_EDGE('',*,*,#14396,.T.);
#19313=ORIENTED_EDGE('',*,*,#14397,.F.);
#19314=ORIENTED_EDGE('',*,*,#14398,.T.);
#19315=ORIENTED_EDGE('',*,*,#14394,.T.);
#19316=ORIENTED_EDGE('',*,*,#14399,.T.);
#19317=ORIENTED_EDGE('',*,*,#14400,.F.);
#19318=ORIENTED_EDGE('',*,*,#14401,.T.);
#19319=ORIENTED_EDGE('',*,*,#14397,.T.);
#19320=ORIENTED_EDGE('',*,*,#14402,.T.);
#19321=ORIENTED_EDGE('',*,*,#14403,.F.);
#19322=ORIENTED_EDGE('',*,*,#14404,.T.);
#19323=ORIENTED_EDGE('',*,*,#14400,.T.);
#19324=ORIENTED_EDGE('',*,*,#14405,.T.);
#19325=ORIENTED_EDGE('',*,*,#14406,.F.);
#19326=ORIENTED_EDGE('',*,*,#14407,.T.);
#19327=ORIENTED_EDGE('',*,*,#14403,.T.);
#19328=ORIENTED_EDGE('',*,*,#14408,.T.);
#19329=ORIENTED_EDGE('',*,*,#14409,.F.);
#19330=ORIENTED_EDGE('',*,*,#14410,.T.);
#19331=ORIENTED_EDGE('',*,*,#14406,.T.);
#19332=ORIENTED_EDGE('',*,*,#14411,.T.);
#19333=ORIENTED_EDGE('',*,*,#14412,.F.);
#19334=ORIENTED_EDGE('',*,*,#14413,.T.);
#19335=ORIENTED_EDGE('',*,*,#14409,.T.);
#19336=ORIENTED_EDGE('',*,*,#14414,.T.);
#19337=ORIENTED_EDGE('',*,*,#14415,.F.);
#19338=ORIENTED_EDGE('',*,*,#14416,.T.);
#19339=ORIENTED_EDGE('',*,*,#14412,.T.);
#19340=ORIENTED_EDGE('',*,*,#14417,.T.);
#19341=ORIENTED_EDGE('',*,*,#14418,.F.);
#19342=ORIENTED_EDGE('',*,*,#14419,.T.);
#19343=ORIENTED_EDGE('',*,*,#14415,.T.);
#19344=ORIENTED_EDGE('',*,*,#14420,.T.);
#19345=ORIENTED_EDGE('',*,*,#14421,.F.);
#19346=ORIENTED_EDGE('',*,*,#14422,.T.);
#19347=ORIENTED_EDGE('',*,*,#14418,.T.);
#19348=ORIENTED_EDGE('',*,*,#14423,.T.);
#19349=ORIENTED_EDGE('',*,*,#14424,.F.);
#19350=ORIENTED_EDGE('',*,*,#14425,.T.);
#19351=ORIENTED_EDGE('',*,*,#14421,.T.);
#19352=ORIENTED_EDGE('',*,*,#14426,.T.);
#19353=ORIENTED_EDGE('',*,*,#14427,.F.);
#19354=ORIENTED_EDGE('',*,*,#14428,.T.);
#19355=ORIENTED_EDGE('',*,*,#14424,.T.);
#19356=ORIENTED_EDGE('',*,*,#14429,.T.);
#19357=ORIENTED_EDGE('',*,*,#14430,.F.);
#19358=ORIENTED_EDGE('',*,*,#14431,.T.);
#19359=ORIENTED_EDGE('',*,*,#14427,.T.);
#19360=ORIENTED_EDGE('',*,*,#14432,.T.);
#19361=ORIENTED_EDGE('',*,*,#14433,.F.);
#19362=ORIENTED_EDGE('',*,*,#14434,.T.);
#19363=ORIENTED_EDGE('',*,*,#14430,.T.);
#19364=ORIENTED_EDGE('',*,*,#14435,.T.);
#19365=ORIENTED_EDGE('',*,*,#14436,.F.);
#19366=ORIENTED_EDGE('',*,*,#14437,.T.);
#19367=ORIENTED_EDGE('',*,*,#14433,.T.);
#19368=ORIENTED_EDGE('',*,*,#14438,.T.);
#19369=ORIENTED_EDGE('',*,*,#14439,.F.);
#19370=ORIENTED_EDGE('',*,*,#14440,.T.);
#19371=ORIENTED_EDGE('',*,*,#14436,.T.);
#19372=ORIENTED_EDGE('',*,*,#14441,.T.);
#19373=ORIENTED_EDGE('',*,*,#14442,.F.);
#19374=ORIENTED_EDGE('',*,*,#14443,.T.);
#19375=ORIENTED_EDGE('',*,*,#14439,.T.);
#19376=ORIENTED_EDGE('',*,*,#14444,.T.);
#19377=ORIENTED_EDGE('',*,*,#14445,.F.);
#19378=ORIENTED_EDGE('',*,*,#14446,.T.);
#19379=ORIENTED_EDGE('',*,*,#14442,.T.);
#19380=ORIENTED_EDGE('',*,*,#14447,.T.);
#19381=ORIENTED_EDGE('',*,*,#14448,.F.);
#19382=ORIENTED_EDGE('',*,*,#14449,.T.);
#19383=ORIENTED_EDGE('',*,*,#14445,.T.);
#19384=ORIENTED_EDGE('',*,*,#14450,.T.);
#19385=ORIENTED_EDGE('',*,*,#14451,.F.);
#19386=ORIENTED_EDGE('',*,*,#14452,.T.);
#19387=ORIENTED_EDGE('',*,*,#14448,.T.);
#19388=ORIENTED_EDGE('',*,*,#14453,.T.);
#19389=ORIENTED_EDGE('',*,*,#14454,.F.);
#19390=ORIENTED_EDGE('',*,*,#14455,.T.);
#19391=ORIENTED_EDGE('',*,*,#14451,.T.);
#19392=ORIENTED_EDGE('',*,*,#14456,.T.);
#19393=ORIENTED_EDGE('',*,*,#14457,.F.);
#19394=ORIENTED_EDGE('',*,*,#14458,.T.);
#19395=ORIENTED_EDGE('',*,*,#14454,.T.);
#19396=ORIENTED_EDGE('',*,*,#14459,.T.);
#19397=ORIENTED_EDGE('',*,*,#14460,.F.);
#19398=ORIENTED_EDGE('',*,*,#14461,.T.);
#19399=ORIENTED_EDGE('',*,*,#14457,.T.);
#19400=ORIENTED_EDGE('',*,*,#14462,.T.);
#19401=ORIENTED_EDGE('',*,*,#14463,.F.);
#19402=ORIENTED_EDGE('',*,*,#14464,.T.);
#19403=ORIENTED_EDGE('',*,*,#14460,.T.);
#19404=ORIENTED_EDGE('',*,*,#14465,.T.);
#19405=ORIENTED_EDGE('',*,*,#14466,.F.);
#19406=ORIENTED_EDGE('',*,*,#14467,.T.);
#19407=ORIENTED_EDGE('',*,*,#14463,.T.);
#19408=ORIENTED_EDGE('',*,*,#14468,.T.);
#19409=ORIENTED_EDGE('',*,*,#14469,.F.);
#19410=ORIENTED_EDGE('',*,*,#14470,.T.);
#19411=ORIENTED_EDGE('',*,*,#14466,.T.);
#19412=ORIENTED_EDGE('',*,*,#14471,.T.);
#19413=ORIENTED_EDGE('',*,*,#14472,.F.);
#19414=ORIENTED_EDGE('',*,*,#14473,.T.);
#19415=ORIENTED_EDGE('',*,*,#14474,.F.);
#19416=ORIENTED_EDGE('',*,*,#14475,.F.);
#19417=ORIENTED_EDGE('',*,*,#14476,.F.);
#19418=ORIENTED_EDGE('',*,*,#14477,.T.);
#19419=ORIENTED_EDGE('',*,*,#14472,.T.);
#19420=ORIENTED_EDGE('',*,*,#14478,.F.);
#19421=ORIENTED_EDGE('',*,*,#14479,.F.);
#19422=ORIENTED_EDGE('',*,*,#14480,.T.);
#19423=ORIENTED_EDGE('',*,*,#14476,.T.);
#19424=ORIENTED_EDGE('',*,*,#14481,.F.);
#19425=ORIENTED_EDGE('',*,*,#14482,.F.);
#19426=ORIENTED_EDGE('',*,*,#14483,.T.);
#19427=ORIENTED_EDGE('',*,*,#14479,.T.);
#19428=ORIENTED_EDGE('',*,*,#14484,.F.);
#19429=ORIENTED_EDGE('',*,*,#14485,.F.);
#19430=ORIENTED_EDGE('',*,*,#14486,.T.);
#19431=ORIENTED_EDGE('',*,*,#14482,.T.);
#19432=ORIENTED_EDGE('',*,*,#14487,.F.);
#19433=ORIENTED_EDGE('',*,*,#14488,.F.);
#19434=ORIENTED_EDGE('',*,*,#14489,.T.);
#19435=ORIENTED_EDGE('',*,*,#14485,.T.);
#19436=ORIENTED_EDGE('',*,*,#14490,.F.);
#19437=ORIENTED_EDGE('',*,*,#14491,.F.);
#19438=ORIENTED_EDGE('',*,*,#14492,.T.);
#19439=ORIENTED_EDGE('',*,*,#14488,.T.);
#19440=ORIENTED_EDGE('',*,*,#14493,.F.);
#19441=ORIENTED_EDGE('',*,*,#14494,.F.);
#19442=ORIENTED_EDGE('',*,*,#14495,.T.);
#19443=ORIENTED_EDGE('',*,*,#14491,.T.);
#19444=ORIENTED_EDGE('',*,*,#14496,.F.);
#19445=ORIENTED_EDGE('',*,*,#14497,.F.);
#19446=ORIENTED_EDGE('',*,*,#14498,.T.);
#19447=ORIENTED_EDGE('',*,*,#14494,.T.);
#19448=ORIENTED_EDGE('',*,*,#14499,.F.);
#19449=ORIENTED_EDGE('',*,*,#14500,.F.);
#19450=ORIENTED_EDGE('',*,*,#14501,.T.);
#19451=ORIENTED_EDGE('',*,*,#14497,.T.);
#19452=ORIENTED_EDGE('',*,*,#14502,.F.);
#19453=ORIENTED_EDGE('',*,*,#14503,.F.);
#19454=ORIENTED_EDGE('',*,*,#14504,.T.);
#19455=ORIENTED_EDGE('',*,*,#14500,.T.);
#19456=ORIENTED_EDGE('',*,*,#14505,.F.);
#19457=ORIENTED_EDGE('',*,*,#14506,.F.);
#19458=ORIENTED_EDGE('',*,*,#14507,.T.);
#19459=ORIENTED_EDGE('',*,*,#14503,.T.);
#19460=ORIENTED_EDGE('',*,*,#14508,.F.);
#19461=ORIENTED_EDGE('',*,*,#14509,.F.);
#19462=ORIENTED_EDGE('',*,*,#14510,.T.);
#19463=ORIENTED_EDGE('',*,*,#14506,.T.);
#19464=ORIENTED_EDGE('',*,*,#14511,.F.);
#19465=ORIENTED_EDGE('',*,*,#14512,.F.);
#19466=ORIENTED_EDGE('',*,*,#14513,.T.);
#19467=ORIENTED_EDGE('',*,*,#14509,.T.);
#19468=ORIENTED_EDGE('',*,*,#14514,.F.);
#19469=ORIENTED_EDGE('',*,*,#14515,.F.);
#19470=ORIENTED_EDGE('',*,*,#14516,.T.);
#19471=ORIENTED_EDGE('',*,*,#14512,.T.);
#19472=ORIENTED_EDGE('',*,*,#14517,.F.);
#19473=ORIENTED_EDGE('',*,*,#14518,.F.);
#19474=ORIENTED_EDGE('',*,*,#14519,.T.);
#19475=ORIENTED_EDGE('',*,*,#14515,.T.);
#19476=ORIENTED_EDGE('',*,*,#14520,.F.);
#19477=ORIENTED_EDGE('',*,*,#14521,.F.);
#19478=ORIENTED_EDGE('',*,*,#14522,.T.);
#19479=ORIENTED_EDGE('',*,*,#14518,.T.);
#19480=ORIENTED_EDGE('',*,*,#14523,.F.);
#19481=ORIENTED_EDGE('',*,*,#14524,.F.);
#19482=ORIENTED_EDGE('',*,*,#14525,.T.);
#19483=ORIENTED_EDGE('',*,*,#14521,.T.);
#19484=ORIENTED_EDGE('',*,*,#14526,.F.);
#19485=ORIENTED_EDGE('',*,*,#14527,.F.);
#19486=ORIENTED_EDGE('',*,*,#14528,.T.);
#19487=ORIENTED_EDGE('',*,*,#14524,.T.);
#19488=ORIENTED_EDGE('',*,*,#14529,.F.);
#19489=ORIENTED_EDGE('',*,*,#14530,.F.);
#19490=ORIENTED_EDGE('',*,*,#14531,.T.);
#19491=ORIENTED_EDGE('',*,*,#14527,.T.);
#19492=ORIENTED_EDGE('',*,*,#14532,.F.);
#19493=ORIENTED_EDGE('',*,*,#14533,.F.);
#19494=ORIENTED_EDGE('',*,*,#14534,.T.);
#19495=ORIENTED_EDGE('',*,*,#14530,.T.);
#19496=ORIENTED_EDGE('',*,*,#14535,.F.);
#19497=ORIENTED_EDGE('',*,*,#14536,.F.);
#19498=ORIENTED_EDGE('',*,*,#14537,.T.);
#19499=ORIENTED_EDGE('',*,*,#14533,.T.);
#19500=ORIENTED_EDGE('',*,*,#14538,.F.);
#19501=ORIENTED_EDGE('',*,*,#14539,.F.);
#19502=ORIENTED_EDGE('',*,*,#14540,.T.);
#19503=ORIENTED_EDGE('',*,*,#14536,.T.);
#19504=ORIENTED_EDGE('',*,*,#14541,.F.);
#19505=ORIENTED_EDGE('',*,*,#14542,.F.);
#19506=ORIENTED_EDGE('',*,*,#14543,.T.);
#19507=ORIENTED_EDGE('',*,*,#14539,.T.);
#19508=ORIENTED_EDGE('',*,*,#14544,.F.);
#19509=ORIENTED_EDGE('',*,*,#14545,.F.);
#19510=ORIENTED_EDGE('',*,*,#14546,.T.);
#19511=ORIENTED_EDGE('',*,*,#14542,.T.);
#19512=ORIENTED_EDGE('',*,*,#14547,.F.);
#19513=ORIENTED_EDGE('',*,*,#14548,.F.);
#19514=ORIENTED_EDGE('',*,*,#14549,.T.);
#19515=ORIENTED_EDGE('',*,*,#14545,.T.);
#19516=ORIENTED_EDGE('',*,*,#14550,.F.);
#19517=ORIENTED_EDGE('',*,*,#14551,.F.);
#19518=ORIENTED_EDGE('',*,*,#14552,.T.);
#19519=ORIENTED_EDGE('',*,*,#14548,.T.);
#19520=ORIENTED_EDGE('',*,*,#14553,.F.);
#19521=ORIENTED_EDGE('',*,*,#14554,.F.);
#19522=ORIENTED_EDGE('',*,*,#14555,.T.);
#19523=ORIENTED_EDGE('',*,*,#14551,.T.);
#19524=ORIENTED_EDGE('',*,*,#14556,.F.);
#19525=ORIENTED_EDGE('',*,*,#14557,.F.);
#19526=ORIENTED_EDGE('',*,*,#14558,.T.);
#19527=ORIENTED_EDGE('',*,*,#14554,.T.);
#19528=ORIENTED_EDGE('',*,*,#14559,.F.);
#19529=ORIENTED_EDGE('',*,*,#14560,.F.);
#19530=ORIENTED_EDGE('',*,*,#14561,.T.);
#19531=ORIENTED_EDGE('',*,*,#14557,.T.);
#19532=ORIENTED_EDGE('',*,*,#14562,.F.);
#19533=ORIENTED_EDGE('',*,*,#14563,.F.);
#19534=ORIENTED_EDGE('',*,*,#14564,.T.);
#19535=ORIENTED_EDGE('',*,*,#14560,.T.);
#19536=ORIENTED_EDGE('',*,*,#14565,.F.);
#19537=ORIENTED_EDGE('',*,*,#14566,.F.);
#19538=ORIENTED_EDGE('',*,*,#14567,.T.);
#19539=ORIENTED_EDGE('',*,*,#14563,.T.);
#19540=ORIENTED_EDGE('',*,*,#14568,.F.);
#19541=ORIENTED_EDGE('',*,*,#14569,.F.);
#19542=ORIENTED_EDGE('',*,*,#14570,.T.);
#19543=ORIENTED_EDGE('',*,*,#14566,.T.);
#19544=ORIENTED_EDGE('',*,*,#14571,.F.);
#19545=ORIENTED_EDGE('',*,*,#14572,.F.);
#19546=ORIENTED_EDGE('',*,*,#14573,.T.);
#19547=ORIENTED_EDGE('',*,*,#14569,.T.);
#19548=ORIENTED_EDGE('',*,*,#14574,.F.);
#19549=ORIENTED_EDGE('',*,*,#14575,.F.);
#19550=ORIENTED_EDGE('',*,*,#14576,.T.);
#19551=ORIENTED_EDGE('',*,*,#14572,.T.);
#19552=ORIENTED_EDGE('',*,*,#14577,.F.);
#19553=ORIENTED_EDGE('',*,*,#14578,.F.);
#19554=ORIENTED_EDGE('',*,*,#14579,.T.);
#19555=ORIENTED_EDGE('',*,*,#14575,.T.);
#19556=ORIENTED_EDGE('',*,*,#14580,.F.);
#19557=ORIENTED_EDGE('',*,*,#14581,.F.);
#19558=ORIENTED_EDGE('',*,*,#14582,.T.);
#19559=ORIENTED_EDGE('',*,*,#14578,.T.);
#19560=ORIENTED_EDGE('',*,*,#14583,.F.);
#19561=ORIENTED_EDGE('',*,*,#14584,.F.);
#19562=ORIENTED_EDGE('',*,*,#14585,.T.);
#19563=ORIENTED_EDGE('',*,*,#14581,.T.);
#19564=ORIENTED_EDGE('',*,*,#14586,.F.);
#19565=ORIENTED_EDGE('',*,*,#14587,.F.);
#19566=ORIENTED_EDGE('',*,*,#14588,.T.);
#19567=ORIENTED_EDGE('',*,*,#14584,.T.);
#19568=ORIENTED_EDGE('',*,*,#14589,.F.);
#19569=ORIENTED_EDGE('',*,*,#14590,.F.);
#19570=ORIENTED_EDGE('',*,*,#14591,.T.);
#19571=ORIENTED_EDGE('',*,*,#14587,.T.);
#19572=ORIENTED_EDGE('',*,*,#14592,.F.);
#19573=ORIENTED_EDGE('',*,*,#14593,.F.);
#19574=ORIENTED_EDGE('',*,*,#14594,.T.);
#19575=ORIENTED_EDGE('',*,*,#14590,.T.);
#19576=ORIENTED_EDGE('',*,*,#14595,.F.);
#19577=ORIENTED_EDGE('',*,*,#14596,.F.);
#19578=ORIENTED_EDGE('',*,*,#14597,.T.);
#19579=ORIENTED_EDGE('',*,*,#14593,.T.);
#19580=ORIENTED_EDGE('',*,*,#14598,.F.);
#19581=ORIENTED_EDGE('',*,*,#14599,.T.);
#19582=ORIENTED_EDGE('',*,*,#14600,.T.);
#19583=ORIENTED_EDGE('',*,*,#14601,.T.);
#19584=ORIENTED_EDGE('',*,*,#14602,.T.);
#19585=ORIENTED_EDGE('',*,*,#14600,.F.);
#19586=ORIENTED_EDGE('',*,*,#14601,.F.);
#19587=ORIENTED_EDGE('',*,*,#14602,.F.);
#19588=ORIENTED_EDGE('',*,*,#14603,.T.);
#19589=ORIENTED_EDGE('',*,*,#14604,.F.);
#19590=ORIENTED_EDGE('',*,*,#14605,.F.);
#19591=ORIENTED_EDGE('',*,*,#14606,.F.);
#19592=ORIENTED_EDGE('',*,*,#14603,.F.);
#19593=ORIENTED_EDGE('',*,*,#14599,.F.);
#19594=ORIENTED_EDGE('',*,*,#14607,.T.);
#19595=ORIENTED_EDGE('',*,*,#14608,.T.);
#19596=ORIENTED_EDGE('',*,*,#14609,.T.);
#19597=ORIENTED_EDGE('',*,*,#14608,.F.);
#19598=ORIENTED_EDGE('',*,*,#14610,.F.);
#19599=ORIENTED_EDGE('',*,*,#14611,.T.);
#19600=ORIENTED_EDGE('',*,*,#14609,.F.);
#19601=ORIENTED_EDGE('',*,*,#14611,.F.);
#19602=ORIENTED_EDGE('',*,*,#14612,.F.);
#19603=ORIENTED_EDGE('',*,*,#14607,.F.);
#19604=ORIENTED_EDGE('',*,*,#14613,.T.);
#19605=ORIENTED_EDGE('',*,*,#14604,.T.);
#19606=ORIENTED_EDGE('',*,*,#14606,.T.);
#19607=ORIENTED_EDGE('',*,*,#14614,.T.);
#19608=ORIENTED_EDGE('',*,*,#14615,.T.);
#19609=ORIENTED_EDGE('',*,*,#14614,.F.);
#19610=ORIENTED_EDGE('',*,*,#14616,.T.);
#19611=ORIENTED_EDGE('',*,*,#14617,.F.);
#19612=ORIENTED_EDGE('',*,*,#14473,.F.);
#19613=ORIENTED_EDGE('',*,*,#14477,.F.);
#19614=ORIENTED_EDGE('',*,*,#14480,.F.);
#19615=ORIENTED_EDGE('',*,*,#14483,.F.);
#19616=ORIENTED_EDGE('',*,*,#14486,.F.);
#19617=ORIENTED_EDGE('',*,*,#14489,.F.);
#19618=ORIENTED_EDGE('',*,*,#14492,.F.);
#19619=ORIENTED_EDGE('',*,*,#14495,.F.);
#19620=ORIENTED_EDGE('',*,*,#14498,.F.);
#19621=ORIENTED_EDGE('',*,*,#14501,.F.);
#19622=ORIENTED_EDGE('',*,*,#14504,.F.);
#19623=ORIENTED_EDGE('',*,*,#14507,.F.);
#19624=ORIENTED_EDGE('',*,*,#14510,.F.);
#19625=ORIENTED_EDGE('',*,*,#14513,.F.);
#19626=ORIENTED_EDGE('',*,*,#14516,.F.);
#19627=ORIENTED_EDGE('',*,*,#14519,.F.);
#19628=ORIENTED_EDGE('',*,*,#14522,.F.);
#19629=ORIENTED_EDGE('',*,*,#14525,.F.);
#19630=ORIENTED_EDGE('',*,*,#14528,.F.);
#19631=ORIENTED_EDGE('',*,*,#14531,.F.);
#19632=ORIENTED_EDGE('',*,*,#14534,.F.);
#19633=ORIENTED_EDGE('',*,*,#14537,.F.);
#19634=ORIENTED_EDGE('',*,*,#14540,.F.);
#19635=ORIENTED_EDGE('',*,*,#14543,.F.);
#19636=ORIENTED_EDGE('',*,*,#14546,.F.);
#19637=ORIENTED_EDGE('',*,*,#14549,.F.);
#19638=ORIENTED_EDGE('',*,*,#14552,.F.);
#19639=ORIENTED_EDGE('',*,*,#14555,.F.);
#19640=ORIENTED_EDGE('',*,*,#14558,.F.);
#19641=ORIENTED_EDGE('',*,*,#14561,.F.);
#19642=ORIENTED_EDGE('',*,*,#14564,.F.);
#19643=ORIENTED_EDGE('',*,*,#14567,.F.);
#19644=ORIENTED_EDGE('',*,*,#14570,.F.);
#19645=ORIENTED_EDGE('',*,*,#14573,.F.);
#19646=ORIENTED_EDGE('',*,*,#14576,.F.);
#19647=ORIENTED_EDGE('',*,*,#14579,.F.);
#19648=ORIENTED_EDGE('',*,*,#14582,.F.);
#19649=ORIENTED_EDGE('',*,*,#14585,.F.);
#19650=ORIENTED_EDGE('',*,*,#14588,.F.);
#19651=ORIENTED_EDGE('',*,*,#14591,.F.);
#19652=ORIENTED_EDGE('',*,*,#14594,.F.);
#19653=ORIENTED_EDGE('',*,*,#14597,.F.);
#19654=ORIENTED_EDGE('',*,*,#14618,.F.);
#19655=ORIENTED_EDGE('',*,*,#14619,.F.);
#19656=ORIENTED_EDGE('',*,*,#14346,.F.);
#19657=ORIENTED_EDGE('',*,*,#14350,.F.);
#19658=ORIENTED_EDGE('',*,*,#14353,.F.);
#19659=ORIENTED_EDGE('',*,*,#14356,.F.);
#19660=ORIENTED_EDGE('',*,*,#14359,.F.);
#19661=ORIENTED_EDGE('',*,*,#14362,.F.);
#19662=ORIENTED_EDGE('',*,*,#14365,.F.);
#19663=ORIENTED_EDGE('',*,*,#14368,.F.);
#19664=ORIENTED_EDGE('',*,*,#14371,.F.);
#19665=ORIENTED_EDGE('',*,*,#14374,.F.);
#19666=ORIENTED_EDGE('',*,*,#14377,.F.);
#19667=ORIENTED_EDGE('',*,*,#14380,.F.);
#19668=ORIENTED_EDGE('',*,*,#14383,.F.);
#19669=ORIENTED_EDGE('',*,*,#14386,.F.);
#19670=ORIENTED_EDGE('',*,*,#14389,.F.);
#19671=ORIENTED_EDGE('',*,*,#14392,.F.);
#19672=ORIENTED_EDGE('',*,*,#14395,.F.);
#19673=ORIENTED_EDGE('',*,*,#14398,.F.);
#19674=ORIENTED_EDGE('',*,*,#14401,.F.);
#19675=ORIENTED_EDGE('',*,*,#14404,.F.);
#19676=ORIENTED_EDGE('',*,*,#14407,.F.);
#19677=ORIENTED_EDGE('',*,*,#14410,.F.);
#19678=ORIENTED_EDGE('',*,*,#14413,.F.);
#19679=ORIENTED_EDGE('',*,*,#14416,.F.);
#19680=ORIENTED_EDGE('',*,*,#14419,.F.);
#19681=ORIENTED_EDGE('',*,*,#14422,.F.);
#19682=ORIENTED_EDGE('',*,*,#14425,.F.);
#19683=ORIENTED_EDGE('',*,*,#14428,.F.);
#19684=ORIENTED_EDGE('',*,*,#14431,.F.);
#19685=ORIENTED_EDGE('',*,*,#14434,.F.);
#19686=ORIENTED_EDGE('',*,*,#14437,.F.);
#19687=ORIENTED_EDGE('',*,*,#14440,.F.);
#19688=ORIENTED_EDGE('',*,*,#14443,.F.);
#19689=ORIENTED_EDGE('',*,*,#14446,.F.);
#19690=ORIENTED_EDGE('',*,*,#14449,.F.);
#19691=ORIENTED_EDGE('',*,*,#14452,.F.);
#19692=ORIENTED_EDGE('',*,*,#14455,.F.);
#19693=ORIENTED_EDGE('',*,*,#14458,.F.);
#19694=ORIENTED_EDGE('',*,*,#14461,.F.);
#19695=ORIENTED_EDGE('',*,*,#14464,.F.);
#19696=ORIENTED_EDGE('',*,*,#14467,.F.);
#19697=ORIENTED_EDGE('',*,*,#14470,.F.);
#19698=ORIENTED_EDGE('',*,*,#14620,.F.);
#19699=ORIENTED_EDGE('',*,*,#14621,.T.);
#19700=ORIENTED_EDGE('',*,*,#14622,.T.);
#19701=ORIENTED_EDGE('',*,*,#14616,.F.);
#19702=ORIENTED_EDGE('',*,*,#14605,.T.);
#19703=ORIENTED_EDGE('',*,*,#14622,.F.);
#19704=ORIENTED_EDGE('',*,*,#14623,.T.);
#19705=ORIENTED_EDGE('',*,*,#14474,.T.);
#19706=ORIENTED_EDGE('',*,*,#14617,.T.);
#19707=ORIENTED_EDGE('',*,*,#14613,.F.);
#19708=ORIENTED_EDGE('',*,*,#14624,.F.);
#19709=ORIENTED_EDGE('',*,*,#14471,.F.);
#19710=ORIENTED_EDGE('',*,*,#14468,.F.);
#19711=ORIENTED_EDGE('',*,*,#14465,.F.);
#19712=ORIENTED_EDGE('',*,*,#14462,.F.);
#19713=ORIENTED_EDGE('',*,*,#14459,.F.);
#19714=ORIENTED_EDGE('',*,*,#14456,.F.);
#19715=ORIENTED_EDGE('',*,*,#14453,.F.);
#19716=ORIENTED_EDGE('',*,*,#14450,.F.);
#19717=ORIENTED_EDGE('',*,*,#14447,.F.);
#19718=ORIENTED_EDGE('',*,*,#14444,.F.);
#19719=ORIENTED_EDGE('',*,*,#14441,.F.);
#19720=ORIENTED_EDGE('',*,*,#14438,.F.);
#19721=ORIENTED_EDGE('',*,*,#14435,.F.);
#19722=ORIENTED_EDGE('',*,*,#14432,.F.);
#19723=ORIENTED_EDGE('',*,*,#14429,.F.);
#19724=ORIENTED_EDGE('',*,*,#14426,.F.);
#19725=ORIENTED_EDGE('',*,*,#14423,.F.);
#19726=ORIENTED_EDGE('',*,*,#14420,.F.);
#19727=ORIENTED_EDGE('',*,*,#14417,.F.);
#19728=ORIENTED_EDGE('',*,*,#14414,.F.);
#19729=ORIENTED_EDGE('',*,*,#14411,.F.);
#19730=ORIENTED_EDGE('',*,*,#14408,.F.);
#19731=ORIENTED_EDGE('',*,*,#14405,.F.);
#19732=ORIENTED_EDGE('',*,*,#14402,.F.);
#19733=ORIENTED_EDGE('',*,*,#14399,.F.);
#19734=ORIENTED_EDGE('',*,*,#14396,.F.);
#19735=ORIENTED_EDGE('',*,*,#14393,.F.);
#19736=ORIENTED_EDGE('',*,*,#14390,.F.);
#19737=ORIENTED_EDGE('',*,*,#14387,.F.);
#19738=ORIENTED_EDGE('',*,*,#14384,.F.);
#19739=ORIENTED_EDGE('',*,*,#14381,.F.);
#19740=ORIENTED_EDGE('',*,*,#14378,.F.);
#19741=ORIENTED_EDGE('',*,*,#14375,.F.);
#19742=ORIENTED_EDGE('',*,*,#14372,.F.);
#19743=ORIENTED_EDGE('',*,*,#14369,.F.);
#19744=ORIENTED_EDGE('',*,*,#14366,.F.);
#19745=ORIENTED_EDGE('',*,*,#14363,.F.);
#19746=ORIENTED_EDGE('',*,*,#14360,.F.);
#19747=ORIENTED_EDGE('',*,*,#14357,.F.);
#19748=ORIENTED_EDGE('',*,*,#14354,.F.);
#19749=ORIENTED_EDGE('',*,*,#14351,.F.);
#19750=ORIENTED_EDGE('',*,*,#14348,.F.);
#19751=ORIENTED_EDGE('',*,*,#14625,.F.);
#19752=ORIENTED_EDGE('',*,*,#14626,.T.);
#19753=ORIENTED_EDGE('',*,*,#14598,.T.);
#19754=ORIENTED_EDGE('',*,*,#14595,.T.);
#19755=ORIENTED_EDGE('',*,*,#14592,.T.);
#19756=ORIENTED_EDGE('',*,*,#14589,.T.);
#19757=ORIENTED_EDGE('',*,*,#14586,.T.);
#19758=ORIENTED_EDGE('',*,*,#14583,.T.);
#19759=ORIENTED_EDGE('',*,*,#14580,.T.);
#19760=ORIENTED_EDGE('',*,*,#14577,.T.);
#19761=ORIENTED_EDGE('',*,*,#14574,.T.);
#19762=ORIENTED_EDGE('',*,*,#14571,.T.);
#19763=ORIENTED_EDGE('',*,*,#14568,.T.);
#19764=ORIENTED_EDGE('',*,*,#14565,.T.);
#19765=ORIENTED_EDGE('',*,*,#14562,.T.);
#19766=ORIENTED_EDGE('',*,*,#14559,.T.);
#19767=ORIENTED_EDGE('',*,*,#14556,.T.);
#19768=ORIENTED_EDGE('',*,*,#14553,.T.);
#19769=ORIENTED_EDGE('',*,*,#14550,.T.);
#19770=ORIENTED_EDGE('',*,*,#14547,.T.);
#19771=ORIENTED_EDGE('',*,*,#14544,.T.);
#19772=ORIENTED_EDGE('',*,*,#14541,.T.);
#19773=ORIENTED_EDGE('',*,*,#14538,.T.);
#19774=ORIENTED_EDGE('',*,*,#14535,.T.);
#19775=ORIENTED_EDGE('',*,*,#14532,.T.);
#19776=ORIENTED_EDGE('',*,*,#14529,.T.);
#19777=ORIENTED_EDGE('',*,*,#14526,.T.);
#19778=ORIENTED_EDGE('',*,*,#14523,.T.);
#19779=ORIENTED_EDGE('',*,*,#14520,.T.);
#19780=ORIENTED_EDGE('',*,*,#14517,.T.);
#19781=ORIENTED_EDGE('',*,*,#14514,.T.);
#19782=ORIENTED_EDGE('',*,*,#14511,.T.);
#19783=ORIENTED_EDGE('',*,*,#14508,.T.);
#19784=ORIENTED_EDGE('',*,*,#14505,.T.);
#19785=ORIENTED_EDGE('',*,*,#14502,.T.);
#19786=ORIENTED_EDGE('',*,*,#14499,.T.);
#19787=ORIENTED_EDGE('',*,*,#14496,.T.);
#19788=ORIENTED_EDGE('',*,*,#14493,.T.);
#19789=ORIENTED_EDGE('',*,*,#14490,.T.);
#19790=ORIENTED_EDGE('',*,*,#14487,.T.);
#19791=ORIENTED_EDGE('',*,*,#14484,.T.);
#19792=ORIENTED_EDGE('',*,*,#14481,.T.);
#19793=ORIENTED_EDGE('',*,*,#14478,.T.);
#19794=ORIENTED_EDGE('',*,*,#14475,.T.);
#19795=ORIENTED_EDGE('',*,*,#14623,.F.);
#19796=ORIENTED_EDGE('',*,*,#14621,.F.);
#19797=ORIENTED_EDGE('',*,*,#14596,.T.);
#19798=ORIENTED_EDGE('',*,*,#14626,.F.);
#19799=ORIENTED_EDGE('',*,*,#14627,.F.);
#19800=ORIENTED_EDGE('',*,*,#14618,.T.);
#19801=ORIENTED_EDGE('',*,*,#14469,.T.);
#19802=ORIENTED_EDGE('',*,*,#14624,.T.);
#19803=ORIENTED_EDGE('',*,*,#14615,.F.);
#19804=ORIENTED_EDGE('',*,*,#14620,.T.);
#19805=ORIENTED_EDGE('',*,*,#14628,.T.);
#19806=ORIENTED_EDGE('',*,*,#14610,.T.);
#19807=ORIENTED_EDGE('',*,*,#14628,.F.);
#19808=ORIENTED_EDGE('',*,*,#14629,.F.);
#19809=ORIENTED_EDGE('',*,*,#14630,.F.);
#19810=ORIENTED_EDGE('',*,*,#14631,.F.);
#19811=ORIENTED_EDGE('',*,*,#14632,.T.);
#19812=ORIENTED_EDGE('',*,*,#14633,.F.);
#19813=ORIENTED_EDGE('',*,*,#14632,.F.);
#19814=ORIENTED_EDGE('',*,*,#14634,.F.);
#19815=ORIENTED_EDGE('',*,*,#14635,.T.);
#19816=ORIENTED_EDGE('',*,*,#14636,.F.);
#19817=ORIENTED_EDGE('',*,*,#14635,.F.);
#19818=ORIENTED_EDGE('',*,*,#14637,.F.);
#19819=ORIENTED_EDGE('',*,*,#14638,.T.);
#19820=ORIENTED_EDGE('',*,*,#14639,.F.);
#19821=ORIENTED_EDGE('',*,*,#14638,.F.);
#19822=ORIENTED_EDGE('',*,*,#14640,.F.);
#19823=ORIENTED_EDGE('',*,*,#14630,.T.);
#19824=ORIENTED_EDGE('',*,*,#14634,.T.);
#19825=ORIENTED_EDGE('',*,*,#14631,.T.);
#19826=ORIENTED_EDGE('',*,*,#14640,.T.);
#19827=ORIENTED_EDGE('',*,*,#14637,.T.);
#19828=ORIENTED_EDGE('',*,*,#14641,.F.);
#19829=ORIENTED_EDGE('',*,*,#14642,.T.);
#19830=ORIENTED_EDGE('',*,*,#14612,.T.);
#19831=ORIENTED_EDGE('',*,*,#14642,.F.);
#19832=ORIENTED_EDGE('',*,*,#14643,.F.);
#19833=ORIENTED_EDGE('',*,*,#14644,.T.);
#19834=ORIENTED_EDGE('',*,*,#14641,.T.);
#19835=ORIENTED_EDGE('',*,*,#14644,.F.);
#19836=ORIENTED_EDGE('',*,*,#14636,.T.);
#19837=ORIENTED_EDGE('',*,*,#14639,.T.);
#19838=ORIENTED_EDGE('',*,*,#14629,.T.);
#19839=ORIENTED_EDGE('',*,*,#14633,.T.);
#19840=ORIENTED_EDGE('',*,*,#14645,.F.);
#19841=ORIENTED_EDGE('',*,*,#14643,.T.);
#19842=ORIENTED_EDGE('',*,*,#14646,.F.);
#19843=ORIENTED_EDGE('',*,*,#14647,.T.);
#19844=ORIENTED_EDGE('',*,*,#14645,.T.);
#19845=ORIENTED_EDGE('',*,*,#14647,.F.);
#19846=ORIENTED_EDGE('',*,*,#14648,.F.);
#19847=ORIENTED_EDGE('',*,*,#14649,.T.);
#19848=ORIENTED_EDGE('',*,*,#14646,.T.);
#19849=ORIENTED_EDGE('',*,*,#14649,.F.);
#19850=ORIENTED_EDGE('',*,*,#14650,.F.);
#19851=ORIENTED_EDGE('',*,*,#14651,.T.);
#19852=ORIENTED_EDGE('',*,*,#14648,.T.);
#19853=ORIENTED_EDGE('',*,*,#14651,.F.);
#19854=ORIENTED_EDGE('',*,*,#14650,.T.);
#19855=ORIENTED_EDGE('',*,*,#14619,.T.);
#19856=ORIENTED_EDGE('',*,*,#14627,.T.);
#19857=ORIENTED_EDGE('',*,*,#14625,.T.);
#19858=ORIENTED_EDGE('',*,*,#14347,.F.);
#19859=ORIENTED_EDGE('',*,*,#14652,.T.);
#19860=ORIENTED_EDGE('',*,*,#14653,.T.);
#19861=ORIENTED_EDGE('',*,*,#14654,.T.);
#19862=ORIENTED_EDGE('',*,*,#14655,.T.);
#19863=ORIENTED_EDGE('',*,*,#14653,.F.);
#19864=ORIENTED_EDGE('',*,*,#14656,.F.);
#19865=ORIENTED_EDGE('',*,*,#14657,.F.);
#19866=ORIENTED_EDGE('',*,*,#14658,.T.);
#19867=ORIENTED_EDGE('',*,*,#14654,.F.);
#19868=ORIENTED_EDGE('',*,*,#14655,.F.);
#19869=ORIENTED_EDGE('',*,*,#14658,.F.);
#19870=ORIENTED_EDGE('',*,*,#14659,.F.);
#19871=ORIENTED_EDGE('',*,*,#14652,.F.);
#19872=ORIENTED_EDGE('',*,*,#14656,.T.);
#19873=ORIENTED_EDGE('',*,*,#14657,.T.);
#19874=ORIENTED_EDGE('',*,*,#14660,.T.);
#19875=ORIENTED_EDGE('',*,*,#14661,.T.);
#19876=ORIENTED_EDGE('',*,*,#14662,.T.);
#19877=ORIENTED_EDGE('',*,*,#14660,.F.);
#19878=ORIENTED_EDGE('',*,*,#14663,.T.);
#19879=ORIENTED_EDGE('',*,*,#14664,.T.);
#19880=ORIENTED_EDGE('',*,*,#14661,.F.);
#19881=ORIENTED_EDGE('',*,*,#14662,.F.);
#19882=ORIENTED_EDGE('',*,*,#14664,.F.);
#19883=ORIENTED_EDGE('',*,*,#14665,.F.);
#19884=ORIENTED_EDGE('',*,*,#14666,.T.);
#19885=ORIENTED_EDGE('',*,*,#14667,.T.);
#19886=ORIENTED_EDGE('',*,*,#14668,.T.);
#19887=ORIENTED_EDGE('',*,*,#14666,.F.);
#19888=ORIENTED_EDGE('',*,*,#14668,.F.);
#19889=ORIENTED_EDGE('',*,*,#14669,.F.);
#19890=ORIENTED_EDGE('',*,*,#14667,.F.);
#19891=ORIENTED_EDGE('',*,*,#14669,.T.);
#19892=ORIENTED_EDGE('',*,*,#14670,.T.);
#19893=ORIENTED_EDGE('',*,*,#14671,.T.);
#19894=ORIENTED_EDGE('',*,*,#14670,.F.);
#19895=ORIENTED_EDGE('',*,*,#14671,.F.);
#19896=ORIENTED_EDGE('',*,*,#14672,.T.);
#19897=ORIENTED_EDGE('',*,*,#14659,.T.);
#19898=ORIENTED_EDGE('',*,*,#14672,.F.);
#19899=ORIENTED_EDGE('',*,*,#14673,.F.);
#19900=ORIENTED_EDGE('',*,*,#14674,.T.);
#19901=ORIENTED_EDGE('',*,*,#14665,.T.);
#19902=ORIENTED_EDGE('',*,*,#14674,.F.);
#19903=ORIENTED_EDGE('',*,*,#14675,.F.);
#19904=ORIENTED_EDGE('',*,*,#14676,.T.);
#19905=ORIENTED_EDGE('',*,*,#14673,.T.);
#19906=ORIENTED_EDGE('',*,*,#14676,.F.);
#19907=ORIENTED_EDGE('',*,*,#14675,.T.);
#19908=ORIENTED_EDGE('',*,*,#14677,.F.);
#19909=ORIENTED_EDGE('',*,*,#14677,.T.);
#19910=ORIENTED_EDGE('',*,*,#14678,.T.);
#19911=ORIENTED_EDGE('',*,*,#14663,.F.);
#19912=ORIENTED_EDGE('',*,*,#14678,.F.);
#19913=ORIENTED_EDGE('',*,*,#14679,.T.);
#19914=ORIENTED_EDGE('',*,*,#14680,.T.);
#19915=ORIENTED_EDGE('',*,*,#14681,.T.);
#19916=ORIENTED_EDGE('',*,*,#14682,.T.);
#19917=ORIENTED_EDGE('',*,*,#14681,.F.);
#19918=ORIENTED_EDGE('',*,*,#14683,.T.);
#19919=ORIENTED_EDGE('',*,*,#14682,.F.);
#19920=ORIENTED_EDGE('',*,*,#14679,.F.);
#19921=ORIENTED_EDGE('',*,*,#14680,.F.);
#19922=ORIENTED_EDGE('',*,*,#14684,.T.);
#19923=ORIENTED_EDGE('',*,*,#14685,.F.);
#19924=ORIENTED_EDGE('',*,*,#14684,.F.);
#19925=ORIENTED_EDGE('',*,*,#14686,.T.);
#19926=ORIENTED_EDGE('',*,*,#14687,.T.);
#19927=ORIENTED_EDGE('',*,*,#14688,.T.);
#19928=ORIENTED_EDGE('',*,*,#14689,.T.);
#19929=ORIENTED_EDGE('',*,*,#14687,.F.);
#19930=ORIENTED_EDGE('',*,*,#14688,.F.);
#19931=ORIENTED_EDGE('',*,*,#14689,.F.);
#19932=ORIENTED_EDGE('',*,*,#14690,.T.);
#19933=ORIENTED_EDGE('',*,*,#14691,.F.);
#19934=ORIENTED_EDGE('',*,*,#14692,.F.);
#19935=ORIENTED_EDGE('',*,*,#14690,.F.);
#19936=ORIENTED_EDGE('',*,*,#14686,.F.);
#19937=ORIENTED_EDGE('',*,*,#14693,.F.);
#19938=ORIENTED_EDGE('',*,*,#14694,.T.);
#19939=ORIENTED_EDGE('',*,*,#14695,.T.);
#19940=ORIENTED_EDGE('',*,*,#14696,.T.);
#19941=ORIENTED_EDGE('',*,*,#14697,.T.);
#19942=ORIENTED_EDGE('',*,*,#14691,.T.);
#19943=ORIENTED_EDGE('',*,*,#14692,.T.);
#19944=ORIENTED_EDGE('',*,*,#14698,.T.);
#19945=ORIENTED_EDGE('',*,*,#14699,.T.);
#19946=ORIENTED_EDGE('',*,*,#14700,.T.);
#19947=ORIENTED_EDGE('',*,*,#14698,.F.);
#19948=ORIENTED_EDGE('',*,*,#14699,.F.);
#19949=ORIENTED_EDGE('',*,*,#14700,.F.);
#19950=ORIENTED_EDGE('',*,*,#14701,.T.);
#19951=ORIENTED_EDGE('',*,*,#14702,.F.);
#19952=ORIENTED_EDGE('',*,*,#14703,.F.);
#19953=ORIENTED_EDGE('',*,*,#14701,.F.);
#19954=ORIENTED_EDGE('',*,*,#14702,.T.);
#19955=ORIENTED_EDGE('',*,*,#14703,.T.);
#19956=ORIENTED_EDGE('',*,*,#14704,.T.);
#19957=ORIENTED_EDGE('',*,*,#14705,.T.);
#19958=ORIENTED_EDGE('',*,*,#14706,.T.);
#19959=ORIENTED_EDGE('',*,*,#14704,.F.);
#19960=ORIENTED_EDGE('',*,*,#14705,.F.);
#19961=ORIENTED_EDGE('',*,*,#14706,.F.);
#19962=ORIENTED_EDGE('',*,*,#14707,.T.);
#19963=ORIENTED_EDGE('',*,*,#14708,.F.);
#19964=ORIENTED_EDGE('',*,*,#14709,.F.);
#19965=ORIENTED_EDGE('',*,*,#14707,.F.);
#19966=ORIENTED_EDGE('',*,*,#14708,.T.);
#19967=ORIENTED_EDGE('',*,*,#14709,.T.);
#19968=ORIENTED_EDGE('',*,*,#14710,.T.);
#19969=ORIENTED_EDGE('',*,*,#14711,.T.);
#19970=ORIENTED_EDGE('',*,*,#14710,.F.);
#19971=ORIENTED_EDGE('',*,*,#14711,.F.);
#19972=ORIENTED_EDGE('',*,*,#14712,.T.);
#19973=ORIENTED_EDGE('',*,*,#14713,.T.);
#19974=ORIENTED_EDGE('',*,*,#14714,.T.);
#19975=ORIENTED_EDGE('',*,*,#14715,.T.);
#19976=ORIENTED_EDGE('',*,*,#14716,.T.);
#19977=ORIENTED_EDGE('',*,*,#14717,.T.);
#19978=ORIENTED_EDGE('',*,*,#14718,.T.);
#19979=ORIENTED_EDGE('',*,*,#14719,.T.);
#19980=ORIENTED_EDGE('',*,*,#14720,.T.);
#19981=ORIENTED_EDGE('',*,*,#14721,.T.);
#19982=ORIENTED_EDGE('',*,*,#14719,.F.);
#19983=ORIENTED_EDGE('',*,*,#14720,.F.);
#19984=ORIENTED_EDGE('',*,*,#14721,.F.);
#19985=ORIENTED_EDGE('',*,*,#14722,.T.);
#19986=ORIENTED_EDGE('',*,*,#14723,.F.);
#19987=ORIENTED_EDGE('',*,*,#14724,.F.);
#19988=ORIENTED_EDGE('',*,*,#14722,.F.);
#19989=ORIENTED_EDGE('',*,*,#14712,.F.);
#19990=ORIENTED_EDGE('',*,*,#14725,.T.);
#19991=ORIENTED_EDGE('',*,*,#14717,.F.);
#19992=ORIENTED_EDGE('',*,*,#14718,.F.);
#19993=ORIENTED_EDGE('',*,*,#14725,.F.);
#19994=ORIENTED_EDGE('',*,*,#14723,.T.);
#19995=ORIENTED_EDGE('',*,*,#14724,.T.);
#19996=ORIENTED_EDGE('',*,*,#14726,.T.);
#19997=ORIENTED_EDGE('',*,*,#14727,.T.);
#19998=ORIENTED_EDGE('',*,*,#14726,.F.);
#19999=ORIENTED_EDGE('',*,*,#14727,.F.);
#20000=ORIENTED_EDGE('',*,*,#14728,.F.);
#20001=ORIENTED_EDGE('',*,*,#14728,.T.);
#20002=ORIENTED_EDGE('',*,*,#14729,.T.);
#20003=ORIENTED_EDGE('',*,*,#14730,.T.);
#20004=ORIENTED_EDGE('',*,*,#14731,.T.);
#20005=ORIENTED_EDGE('',*,*,#14729,.F.);
#20006=ORIENTED_EDGE('',*,*,#14732,.T.);
#20007=ORIENTED_EDGE('',*,*,#14733,.T.);
#20008=ORIENTED_EDGE('',*,*,#14730,.F.);
#20009=ORIENTED_EDGE('',*,*,#14731,.F.);
#20010=ORIENTED_EDGE('',*,*,#14733,.F.);
#20011=ORIENTED_EDGE('',*,*,#14697,.F.);
#20012=ORIENTED_EDGE('',*,*,#14734,.T.);
#20013=ORIENTED_EDGE('',*,*,#14716,.F.);
#20014=ORIENTED_EDGE('',*,*,#14734,.F.);
#20015=ORIENTED_EDGE('',*,*,#14696,.F.);
#20016=ORIENTED_EDGE('',*,*,#14735,.T.);
#20017=ORIENTED_EDGE('',*,*,#14715,.F.);
#20018=ORIENTED_EDGE('',*,*,#14735,.F.);
#20019=ORIENTED_EDGE('',*,*,#14695,.F.);
#20020=ORIENTED_EDGE('',*,*,#14736,.T.);
#20021=ORIENTED_EDGE('',*,*,#14714,.F.);
#20022=ORIENTED_EDGE('',*,*,#14736,.F.);
#20023=ORIENTED_EDGE('',*,*,#14694,.F.);
#20024=ORIENTED_EDGE('',*,*,#14737,.T.);
#20025=ORIENTED_EDGE('',*,*,#14713,.F.);
#20026=ORIENTED_EDGE('',*,*,#14737,.F.);
#20027=ORIENTED_EDGE('',*,*,#14738,.F.);
#20028=ORIENTED_EDGE('',*,*,#14739,.T.);
#20029=ORIENTED_EDGE('',*,*,#14693,.T.);
#20030=ORIENTED_EDGE('',*,*,#14739,.F.);
#20031=ORIENTED_EDGE('',*,*,#14683,.F.);
#20032=ORIENTED_EDGE('',*,*,#14740,.T.);
#20033=ORIENTED_EDGE('',*,*,#14738,.T.);
#20034=ORIENTED_EDGE('',*,*,#14740,.F.);
#20035=ORIENTED_EDGE('',*,*,#14685,.T.);
#20036=ORIENTED_EDGE('',*,*,#14741,.F.);
#20037=ORIENTED_EDGE('',*,*,#14741,.T.);
#20038=ORIENTED_EDGE('',*,*,#14742,.T.);
#20039=ORIENTED_EDGE('',*,*,#14743,.F.);
#20040=ORIENTED_EDGE('',*,*,#14742,.F.);
#20041=ORIENTED_EDGE('',*,*,#14732,.F.);
#20042=ORIENTED_EDGE('',*,*,#14743,.T.);
#20043=ORIENTED_EDGE('',*,*,#14744,.T.);
#20044=ORIENTED_EDGE('',*,*,#14745,.T.);
#20045=ORIENTED_EDGE('',*,*,#14746,.T.);
#20046=ORIENTED_EDGE('',*,*,#14747,.T.);
#20047=ORIENTED_EDGE('',*,*,#14748,.T.);
#20048=ORIENTED_EDGE('',*,*,#14746,.F.);
#20049=ORIENTED_EDGE('',*,*,#14747,.F.);
#20050=ORIENTED_EDGE('',*,*,#14748,.F.);
#20051=ORIENTED_EDGE('',*,*,#14749,.T.);
#20052=ORIENTED_EDGE('',*,*,#14750,.F.);
#20053=ORIENTED_EDGE('',*,*,#14751,.F.);
#20054=ORIENTED_EDGE('',*,*,#14749,.F.);
#20055=ORIENTED_EDGE('',*,*,#14752,.T.);
#20056=ORIENTED_EDGE('',*,*,#14753,.T.);
#20057=ORIENTED_EDGE('',*,*,#14754,.T.);
#20058=ORIENTED_EDGE('',*,*,#14755,.T.);
#20059=ORIENTED_EDGE('',*,*,#14756,.T.);
#20060=ORIENTED_EDGE('',*,*,#14757,.T.);
#20061=ORIENTED_EDGE('',*,*,#14758,.T.);
#20062=ORIENTED_EDGE('',*,*,#14759,.T.);
#20063=ORIENTED_EDGE('',*,*,#14760,.F.);
#20064=ORIENTED_EDGE('',*,*,#14761,.F.);
#20065=ORIENTED_EDGE('',*,*,#14762,.T.);
#20066=ORIENTED_EDGE('',*,*,#14744,.F.);
#20067=ORIENTED_EDGE('',*,*,#14745,.F.);
#20068=ORIENTED_EDGE('',*,*,#14762,.F.);
#20069=ORIENTED_EDGE('',*,*,#14750,.T.);
#20070=ORIENTED_EDGE('',*,*,#14751,.T.);
#20071=ORIENTED_EDGE('',*,*,#14763,.T.);
#20072=ORIENTED_EDGE('',*,*,#14764,.T.);
#20073=ORIENTED_EDGE('',*,*,#14765,.T.);
#20074=ORIENTED_EDGE('',*,*,#14763,.F.);
#20075=ORIENTED_EDGE('',*,*,#14764,.F.);
#20076=ORIENTED_EDGE('',*,*,#14765,.F.);
#20077=ORIENTED_EDGE('',*,*,#14766,.T.);
#20078=ORIENTED_EDGE('',*,*,#14767,.F.);
#20079=ORIENTED_EDGE('',*,*,#14768,.F.);
#20080=ORIENTED_EDGE('',*,*,#14766,.F.);
#20081=ORIENTED_EDGE('',*,*,#14767,.T.);
#20082=ORIENTED_EDGE('',*,*,#14768,.T.);
#20083=ORIENTED_EDGE('',*,*,#14769,.T.);
#20084=ORIENTED_EDGE('',*,*,#14770,.T.);
#20085=ORIENTED_EDGE('',*,*,#14769,.F.);
#20086=ORIENTED_EDGE('',*,*,#14770,.F.);
#20087=ORIENTED_EDGE('',*,*,#14771,.T.);
#20088=ORIENTED_EDGE('',*,*,#14772,.T.);
#20089=ORIENTED_EDGE('',*,*,#14773,.T.);
#20090=ORIENTED_EDGE('',*,*,#14760,.T.);
#20091=ORIENTED_EDGE('',*,*,#14761,.T.);
#20092=ORIENTED_EDGE('',*,*,#14773,.F.);
#20093=ORIENTED_EDGE('',*,*,#14772,.F.);
#20094=ORIENTED_EDGE('',*,*,#14774,.F.);
#20095=ORIENTED_EDGE('',*,*,#14775,.F.);
#20096=ORIENTED_EDGE('',*,*,#14776,.F.);
#20097=ORIENTED_EDGE('',*,*,#14777,.F.);
#20098=ORIENTED_EDGE('',*,*,#14778,.T.);
#20099=ORIENTED_EDGE('',*,*,#14779,.T.);
#20100=ORIENTED_EDGE('',*,*,#14774,.T.);
#20101=ORIENTED_EDGE('',*,*,#14780,.T.);
#20102=ORIENTED_EDGE('',*,*,#14776,.T.);
#20103=ORIENTED_EDGE('',*,*,#14781,.T.);
#20104=ORIENTED_EDGE('',*,*,#14782,.T.);
#20105=ORIENTED_EDGE('',*,*,#14783,.T.);
#20106=ORIENTED_EDGE('',*,*,#14777,.T.);
#20107=ORIENTED_EDGE('',*,*,#14783,.F.);
#20108=ORIENTED_EDGE('',*,*,#14784,.T.);
#20109=ORIENTED_EDGE('',*,*,#14780,.F.);
#20110=ORIENTED_EDGE('',*,*,#14784,.F.);
#20111=ORIENTED_EDGE('',*,*,#14785,.F.);
#20112=ORIENTED_EDGE('',*,*,#14786,.F.);
#20113=ORIENTED_EDGE('',*,*,#14787,.F.);
#20114=ORIENTED_EDGE('',*,*,#14782,.F.);
#20115=ORIENTED_EDGE('',*,*,#14788,.F.);
#20116=ORIENTED_EDGE('',*,*,#14789,.F.);
#20117=ORIENTED_EDGE('',*,*,#14785,.T.);
#20118=ORIENTED_EDGE('',*,*,#14778,.F.);
#20119=ORIENTED_EDGE('',*,*,#14787,.T.);
#20120=ORIENTED_EDGE('',*,*,#14790,.T.);
#20121=ORIENTED_EDGE('',*,*,#14791,.F.);
#20122=ORIENTED_EDGE('',*,*,#14779,.F.);
#20123=ORIENTED_EDGE('',*,*,#14791,.T.);
#20124=ORIENTED_EDGE('',*,*,#14792,.F.);
#20125=ORIENTED_EDGE('',*,*,#14788,.T.);
#20126=ORIENTED_EDGE('',*,*,#14781,.F.);
#20127=ORIENTED_EDGE('',*,*,#14775,.T.);
#20128=ORIENTED_EDGE('',*,*,#14793,.F.);
#20129=ORIENTED_EDGE('',*,*,#14794,.F.);
#20130=ORIENTED_EDGE('',*,*,#14795,.F.);
#20131=ORIENTED_EDGE('',*,*,#14796,.T.);
#20132=ORIENTED_EDGE('',*,*,#14752,.F.);
#20133=ORIENTED_EDGE('',*,*,#14753,.F.);
#20134=ORIENTED_EDGE('',*,*,#14796,.F.);
#20135=ORIENTED_EDGE('',*,*,#14797,.F.);
#20136=ORIENTED_EDGE('',*,*,#14798,.F.);
#20137=ORIENTED_EDGE('',*,*,#14799,.F.);
#20138=ORIENTED_EDGE('',*,*,#14800,.T.);
#20139=ORIENTED_EDGE('',*,*,#14754,.F.);
#20140=ORIENTED_EDGE('',*,*,#14755,.F.);
#20141=ORIENTED_EDGE('',*,*,#14800,.F.);
#20142=ORIENTED_EDGE('',*,*,#14801,.F.);
#20143=ORIENTED_EDGE('',*,*,#14802,.F.);
#20144=ORIENTED_EDGE('',*,*,#14803,.F.);
#20145=ORIENTED_EDGE('',*,*,#14804,.T.);
#20146=ORIENTED_EDGE('',*,*,#14756,.F.);
#20147=ORIENTED_EDGE('',*,*,#14757,.F.);
#20148=ORIENTED_EDGE('',*,*,#14804,.F.);
#20149=ORIENTED_EDGE('',*,*,#14805,.F.);
#20150=ORIENTED_EDGE('',*,*,#14806,.F.);
#20151=ORIENTED_EDGE('',*,*,#14807,.F.);
#20152=ORIENTED_EDGE('',*,*,#14808,.T.);
#20153=ORIENTED_EDGE('',*,*,#14758,.F.);
#20154=ORIENTED_EDGE('',*,*,#14759,.F.);
#20155=ORIENTED_EDGE('',*,*,#14808,.F.);
#20156=ORIENTED_EDGE('',*,*,#14809,.T.);
#20157=ORIENTED_EDGE('',*,*,#14810,.F.);
#20158=ORIENTED_EDGE('',*,*,#14803,.T.);
#20159=ORIENTED_EDGE('',*,*,#14811,.F.);
#20160=ORIENTED_EDGE('',*,*,#14799,.T.);
#20161=ORIENTED_EDGE('',*,*,#14812,.F.);
#20162=ORIENTED_EDGE('',*,*,#14795,.T.);
#20163=ORIENTED_EDGE('',*,*,#14813,.F.);
#20164=ORIENTED_EDGE('',*,*,#14807,.T.);
#20165=ORIENTED_EDGE('',*,*,#14814,.F.);
#20166=ORIENTED_EDGE('',*,*,#14809,.F.);
#20167=ORIENTED_EDGE('',*,*,#14814,.T.);
#20168=ORIENTED_EDGE('',*,*,#14806,.T.);
#20169=ORIENTED_EDGE('',*,*,#14805,.T.);
#20170=ORIENTED_EDGE('',*,*,#14813,.T.);
#20171=ORIENTED_EDGE('',*,*,#14794,.T.);
#20172=ORIENTED_EDGE('',*,*,#14793,.T.);
#20173=ORIENTED_EDGE('',*,*,#14812,.T.);
#20174=ORIENTED_EDGE('',*,*,#14798,.T.);
#20175=ORIENTED_EDGE('',*,*,#14797,.T.);
#20176=ORIENTED_EDGE('',*,*,#14811,.T.);
#20177=ORIENTED_EDGE('',*,*,#14802,.T.);
#20178=ORIENTED_EDGE('',*,*,#14801,.T.);
#20179=ORIENTED_EDGE('',*,*,#14810,.T.);
#20180=ORIENTED_EDGE('',*,*,#14815,.T.);
#20181=ORIENTED_EDGE('',*,*,#14816,.T.);
#20182=ORIENTED_EDGE('',*,*,#14771,.F.);
#20183=ORIENTED_EDGE('',*,*,#14816,.F.);
#20184=ORIENTED_EDGE('',*,*,#14792,.T.);
#20185=ORIENTED_EDGE('',*,*,#14790,.F.);
#20186=ORIENTED_EDGE('',*,*,#14786,.T.);
#20187=ORIENTED_EDGE('',*,*,#14789,.T.);
#20188=ORIENTED_EDGE('',*,*,#14815,.F.);
#20189=ORIENTED_EDGE('',*,*,#14817,.F.);
#20190=ORIENTED_EDGE('',*,*,#14818,.T.);
#20191=ORIENTED_EDGE('',*,*,#14819,.T.);
#20192=ORIENTED_EDGE('',*,*,#14820,.T.);
#20193=ORIENTED_EDGE('',*,*,#14821,.F.);
#20194=ORIENTED_EDGE('',*,*,#14822,.T.);
#20195=ORIENTED_EDGE('',*,*,#14817,.T.);
#20196=ORIENTED_EDGE('',*,*,#14823,.T.);
#20197=ORIENTED_EDGE('',*,*,#14824,.F.);
#20198=ORIENTED_EDGE('',*,*,#14825,.T.);
#20199=ORIENTED_EDGE('',*,*,#14821,.T.);
#20200=ORIENTED_EDGE('',*,*,#14826,.T.);
#20201=ORIENTED_EDGE('',*,*,#14827,.F.);
#20202=ORIENTED_EDGE('',*,*,#14828,.T.);
#20203=ORIENTED_EDGE('',*,*,#14824,.T.);
#20204=ORIENTED_EDGE('',*,*,#14829,.T.);
#20205=ORIENTED_EDGE('',*,*,#14830,.F.);
#20206=ORIENTED_EDGE('',*,*,#14831,.T.);
#20207=ORIENTED_EDGE('',*,*,#14827,.T.);
#20208=ORIENTED_EDGE('',*,*,#14832,.T.);
#20209=ORIENTED_EDGE('',*,*,#14833,.F.);
#20210=ORIENTED_EDGE('',*,*,#14834,.T.);
#20211=ORIENTED_EDGE('',*,*,#14830,.T.);
#20212=ORIENTED_EDGE('',*,*,#14835,.T.);
#20213=ORIENTED_EDGE('',*,*,#14836,.F.);
#20214=ORIENTED_EDGE('',*,*,#14837,.T.);
#20215=ORIENTED_EDGE('',*,*,#14833,.T.);
#20216=ORIENTED_EDGE('',*,*,#14838,.T.);
#20217=ORIENTED_EDGE('',*,*,#14839,.F.);
#20218=ORIENTED_EDGE('',*,*,#14840,.T.);
#20219=ORIENTED_EDGE('',*,*,#14836,.T.);
#20220=ORIENTED_EDGE('',*,*,#14841,.T.);
#20221=ORIENTED_EDGE('',*,*,#14842,.F.);
#20222=ORIENTED_EDGE('',*,*,#14843,.T.);
#20223=ORIENTED_EDGE('',*,*,#14839,.T.);
#20224=ORIENTED_EDGE('',*,*,#14844,.T.);
#20225=ORIENTED_EDGE('',*,*,#14845,.F.);
#20226=ORIENTED_EDGE('',*,*,#14846,.T.);
#20227=ORIENTED_EDGE('',*,*,#14842,.T.);
#20228=ORIENTED_EDGE('',*,*,#14847,.T.);
#20229=ORIENTED_EDGE('',*,*,#14848,.F.);
#20230=ORIENTED_EDGE('',*,*,#14849,.T.);
#20231=ORIENTED_EDGE('',*,*,#14845,.T.);
#20232=ORIENTED_EDGE('',*,*,#14850,.T.);
#20233=ORIENTED_EDGE('',*,*,#14851,.F.);
#20234=ORIENTED_EDGE('',*,*,#14852,.T.);
#20235=ORIENTED_EDGE('',*,*,#14848,.T.);
#20236=ORIENTED_EDGE('',*,*,#14853,.T.);
#20237=ORIENTED_EDGE('',*,*,#14854,.F.);
#20238=ORIENTED_EDGE('',*,*,#14855,.T.);
#20239=ORIENTED_EDGE('',*,*,#14851,.T.);
#20240=ORIENTED_EDGE('',*,*,#14856,.T.);
#20241=ORIENTED_EDGE('',*,*,#14857,.F.);
#20242=ORIENTED_EDGE('',*,*,#14858,.T.);
#20243=ORIENTED_EDGE('',*,*,#14854,.T.);
#20244=ORIENTED_EDGE('',*,*,#14859,.T.);
#20245=ORIENTED_EDGE('',*,*,#14860,.F.);
#20246=ORIENTED_EDGE('',*,*,#14861,.T.);
#20247=ORIENTED_EDGE('',*,*,#14857,.T.);
#20248=ORIENTED_EDGE('',*,*,#14862,.T.);
#20249=ORIENTED_EDGE('',*,*,#14863,.F.);
#20250=ORIENTED_EDGE('',*,*,#14864,.T.);
#20251=ORIENTED_EDGE('',*,*,#14860,.T.);
#20252=ORIENTED_EDGE('',*,*,#14865,.T.);
#20253=ORIENTED_EDGE('',*,*,#14866,.F.);
#20254=ORIENTED_EDGE('',*,*,#14867,.T.);
#20255=ORIENTED_EDGE('',*,*,#14868,.F.);
#20256=ORIENTED_EDGE('',*,*,#14869,.F.);
#20257=ORIENTED_EDGE('',*,*,#14870,.F.);
#20258=ORIENTED_EDGE('',*,*,#14871,.T.);
#20259=ORIENTED_EDGE('',*,*,#14866,.T.);
#20260=ORIENTED_EDGE('',*,*,#14872,.F.);
#20261=ORIENTED_EDGE('',*,*,#14873,.F.);
#20262=ORIENTED_EDGE('',*,*,#14874,.T.);
#20263=ORIENTED_EDGE('',*,*,#14870,.T.);
#20264=ORIENTED_EDGE('',*,*,#14875,.F.);
#20265=ORIENTED_EDGE('',*,*,#14876,.F.);
#20266=ORIENTED_EDGE('',*,*,#14877,.T.);
#20267=ORIENTED_EDGE('',*,*,#14873,.T.);
#20268=ORIENTED_EDGE('',*,*,#14878,.F.);
#20269=ORIENTED_EDGE('',*,*,#14879,.F.);
#20270=ORIENTED_EDGE('',*,*,#14880,.T.);
#20271=ORIENTED_EDGE('',*,*,#14876,.T.);
#20272=ORIENTED_EDGE('',*,*,#14881,.F.);
#20273=ORIENTED_EDGE('',*,*,#14882,.F.);
#20274=ORIENTED_EDGE('',*,*,#14883,.T.);
#20275=ORIENTED_EDGE('',*,*,#14879,.T.);
#20276=ORIENTED_EDGE('',*,*,#14884,.F.);
#20277=ORIENTED_EDGE('',*,*,#14885,.F.);
#20278=ORIENTED_EDGE('',*,*,#14886,.T.);
#20279=ORIENTED_EDGE('',*,*,#14882,.T.);
#20280=ORIENTED_EDGE('',*,*,#14887,.F.);
#20281=ORIENTED_EDGE('',*,*,#14888,.F.);
#20282=ORIENTED_EDGE('',*,*,#14889,.T.);
#20283=ORIENTED_EDGE('',*,*,#14885,.T.);
#20284=ORIENTED_EDGE('',*,*,#14890,.F.);
#20285=ORIENTED_EDGE('',*,*,#14891,.F.);
#20286=ORIENTED_EDGE('',*,*,#14892,.T.);
#20287=ORIENTED_EDGE('',*,*,#14888,.T.);
#20288=ORIENTED_EDGE('',*,*,#14893,.F.);
#20289=ORIENTED_EDGE('',*,*,#14894,.F.);
#20290=ORIENTED_EDGE('',*,*,#14895,.T.);
#20291=ORIENTED_EDGE('',*,*,#14891,.T.);
#20292=ORIENTED_EDGE('',*,*,#14896,.F.);
#20293=ORIENTED_EDGE('',*,*,#14897,.F.);
#20294=ORIENTED_EDGE('',*,*,#14898,.T.);
#20295=ORIENTED_EDGE('',*,*,#14894,.T.);
#20296=ORIENTED_EDGE('',*,*,#14899,.F.);
#20297=ORIENTED_EDGE('',*,*,#14900,.F.);
#20298=ORIENTED_EDGE('',*,*,#14901,.T.);
#20299=ORIENTED_EDGE('',*,*,#14897,.T.);
#20300=ORIENTED_EDGE('',*,*,#14902,.F.);
#20301=ORIENTED_EDGE('',*,*,#14903,.F.);
#20302=ORIENTED_EDGE('',*,*,#14904,.T.);
#20303=ORIENTED_EDGE('',*,*,#14900,.T.);
#20304=ORIENTED_EDGE('',*,*,#14905,.F.);
#20305=ORIENTED_EDGE('',*,*,#14906,.F.);
#20306=ORIENTED_EDGE('',*,*,#14907,.T.);
#20307=ORIENTED_EDGE('',*,*,#14903,.T.);
#20308=ORIENTED_EDGE('',*,*,#14908,.F.);
#20309=ORIENTED_EDGE('',*,*,#14909,.F.);
#20310=ORIENTED_EDGE('',*,*,#14910,.T.);
#20311=ORIENTED_EDGE('',*,*,#14906,.T.);
#20312=ORIENTED_EDGE('',*,*,#14911,.F.);
#20313=ORIENTED_EDGE('',*,*,#14868,.T.);
#20314=ORIENTED_EDGE('',*,*,#14912,.T.);
#20315=ORIENTED_EDGE('',*,*,#14913,.F.);
#20316=ORIENTED_EDGE('',*,*,#14914,.F.);
#20317=ORIENTED_EDGE('',*,*,#14915,.T.);
#20318=ORIENTED_EDGE('',*,*,#14915,.F.);
#20319=ORIENTED_EDGE('',*,*,#14916,.F.);
#20320=ORIENTED_EDGE('',*,*,#14865,.F.);
#20321=ORIENTED_EDGE('',*,*,#14862,.F.);
#20322=ORIENTED_EDGE('',*,*,#14859,.F.);
#20323=ORIENTED_EDGE('',*,*,#14856,.F.);
#20324=ORIENTED_EDGE('',*,*,#14853,.F.);
#20325=ORIENTED_EDGE('',*,*,#14850,.F.);
#20326=ORIENTED_EDGE('',*,*,#14847,.F.);
#20327=ORIENTED_EDGE('',*,*,#14844,.F.);
#20328=ORIENTED_EDGE('',*,*,#14841,.F.);
#20329=ORIENTED_EDGE('',*,*,#14838,.F.);
#20330=ORIENTED_EDGE('',*,*,#14835,.F.);
#20331=ORIENTED_EDGE('',*,*,#14832,.F.);
#20332=ORIENTED_EDGE('',*,*,#14829,.F.);
#20333=ORIENTED_EDGE('',*,*,#14826,.F.);
#20334=ORIENTED_EDGE('',*,*,#14823,.F.);
#20335=ORIENTED_EDGE('',*,*,#14820,.F.);
#20336=ORIENTED_EDGE('',*,*,#14917,.F.);
#20337=ORIENTED_EDGE('',*,*,#14918,.T.);
#20338=ORIENTED_EDGE('',*,*,#14911,.T.);
#20339=ORIENTED_EDGE('',*,*,#14908,.T.);
#20340=ORIENTED_EDGE('',*,*,#14905,.T.);
#20341=ORIENTED_EDGE('',*,*,#14902,.T.);
#20342=ORIENTED_EDGE('',*,*,#14899,.T.);
#20343=ORIENTED_EDGE('',*,*,#14896,.T.);
#20344=ORIENTED_EDGE('',*,*,#14893,.T.);
#20345=ORIENTED_EDGE('',*,*,#14890,.T.);
#20346=ORIENTED_EDGE('',*,*,#14887,.T.);
#20347=ORIENTED_EDGE('',*,*,#14884,.T.);
#20348=ORIENTED_EDGE('',*,*,#14881,.T.);
#20349=ORIENTED_EDGE('',*,*,#14878,.T.);
#20350=ORIENTED_EDGE('',*,*,#14875,.T.);
#20351=ORIENTED_EDGE('',*,*,#14872,.T.);
#20352=ORIENTED_EDGE('',*,*,#14869,.T.);
#20353=ORIENTED_EDGE('',*,*,#14919,.T.);
#20354=ORIENTED_EDGE('',*,*,#14920,.T.);
#20355=ORIENTED_EDGE('',*,*,#14921,.T.);
#20356=ORIENTED_EDGE('',*,*,#14922,.T.);
#20357=ORIENTED_EDGE('',*,*,#14917,.T.);
#20358=ORIENTED_EDGE('',*,*,#14909,.T.);
#20359=ORIENTED_EDGE('',*,*,#14918,.F.);
#20360=ORIENTED_EDGE('',*,*,#14922,.F.);
#20361=ORIENTED_EDGE('',*,*,#14923,.T.);
#20362=ORIENTED_EDGE('',*,*,#14912,.F.);
#20363=ORIENTED_EDGE('',*,*,#14867,.F.);
#20364=ORIENTED_EDGE('',*,*,#14871,.F.);
#20365=ORIENTED_EDGE('',*,*,#14874,.F.);
#20366=ORIENTED_EDGE('',*,*,#14877,.F.);
#20367=ORIENTED_EDGE('',*,*,#14880,.F.);
#20368=ORIENTED_EDGE('',*,*,#14883,.F.);
#20369=ORIENTED_EDGE('',*,*,#14886,.F.);
#20370=ORIENTED_EDGE('',*,*,#14889,.F.);
#20371=ORIENTED_EDGE('',*,*,#14892,.F.);
#20372=ORIENTED_EDGE('',*,*,#14895,.F.);
#20373=ORIENTED_EDGE('',*,*,#14898,.F.);
#20374=ORIENTED_EDGE('',*,*,#14901,.F.);
#20375=ORIENTED_EDGE('',*,*,#14904,.F.);
#20376=ORIENTED_EDGE('',*,*,#14907,.F.);
#20377=ORIENTED_EDGE('',*,*,#14910,.F.);
#20378=ORIENTED_EDGE('',*,*,#14923,.F.);
#20379=ORIENTED_EDGE('',*,*,#14921,.F.);
#20380=ORIENTED_EDGE('',*,*,#14818,.F.);
#20381=ORIENTED_EDGE('',*,*,#14822,.F.);
#20382=ORIENTED_EDGE('',*,*,#14825,.F.);
#20383=ORIENTED_EDGE('',*,*,#14828,.F.);
#20384=ORIENTED_EDGE('',*,*,#14831,.F.);
#20385=ORIENTED_EDGE('',*,*,#14834,.F.);
#20386=ORIENTED_EDGE('',*,*,#14837,.F.);
#20387=ORIENTED_EDGE('',*,*,#14840,.F.);
#20388=ORIENTED_EDGE('',*,*,#14843,.F.);
#20389=ORIENTED_EDGE('',*,*,#14846,.F.);
#20390=ORIENTED_EDGE('',*,*,#14849,.F.);
#20391=ORIENTED_EDGE('',*,*,#14852,.F.);
#20392=ORIENTED_EDGE('',*,*,#14855,.F.);
#20393=ORIENTED_EDGE('',*,*,#14858,.F.);
#20394=ORIENTED_EDGE('',*,*,#14861,.F.);
#20395=ORIENTED_EDGE('',*,*,#14864,.F.);
#20396=ORIENTED_EDGE('',*,*,#14924,.F.);
#20397=ORIENTED_EDGE('',*,*,#14914,.T.);
#20398=ORIENTED_EDGE('',*,*,#14925,.T.);
#20399=ORIENTED_EDGE('',*,*,#14926,.T.);
#20400=ORIENTED_EDGE('',*,*,#14925,.F.);
#20401=ORIENTED_EDGE('',*,*,#14913,.T.);
#20402=ORIENTED_EDGE('',*,*,#14927,.T.);
#20403=ORIENTED_EDGE('',*,*,#14863,.T.);
#20404=ORIENTED_EDGE('',*,*,#14916,.T.);
#20405=ORIENTED_EDGE('',*,*,#14927,.F.);
#20406=ORIENTED_EDGE('',*,*,#14924,.T.);
#20407=ORIENTED_EDGE('',*,*,#14928,.F.);
#20408=ORIENTED_EDGE('',*,*,#14926,.F.);
#20409=ORIENTED_EDGE('',*,*,#14929,.F.);
#20410=ORIENTED_EDGE('',*,*,#14930,.F.);
#20411=ORIENTED_EDGE('',*,*,#14931,.F.);
#20412=ORIENTED_EDGE('',*,*,#14932,.F.);
#20413=ORIENTED_EDGE('',*,*,#14933,.F.);
#20414=ORIENTED_EDGE('',*,*,#14934,.F.);
#20415=ORIENTED_EDGE('',*,*,#14935,.F.);
#20416=ORIENTED_EDGE('',*,*,#14936,.F.);
#20417=ORIENTED_EDGE('',*,*,#14937,.F.);
#20418=ORIENTED_EDGE('',*,*,#14938,.F.);
#20419=ORIENTED_EDGE('',*,*,#14939,.F.);
#20420=ORIENTED_EDGE('',*,*,#14940,.F.);
#20421=ORIENTED_EDGE('',*,*,#14941,.T.);
#20422=ORIENTED_EDGE('',*,*,#14936,.T.);
#20423=ORIENTED_EDGE('',*,*,#14934,.T.);
#20424=ORIENTED_EDGE('',*,*,#14932,.T.);
#20425=ORIENTED_EDGE('',*,*,#14930,.T.);
#20426=ORIENTED_EDGE('',*,*,#14940,.T.);
#20427=ORIENTED_EDGE('',*,*,#14938,.T.);
#20428=ORIENTED_EDGE('',*,*,#14941,.F.);
#20429=ORIENTED_EDGE('',*,*,#14942,.F.);
#20430=ORIENTED_EDGE('',*,*,#14943,.T.);
#20431=ORIENTED_EDGE('',*,*,#14929,.T.);
#20432=ORIENTED_EDGE('',*,*,#14944,.F.);
#20433=ORIENTED_EDGE('',*,*,#14945,.F.);
#20434=ORIENTED_EDGE('',*,*,#14946,.T.);
#20435=ORIENTED_EDGE('',*,*,#14939,.T.);
#20436=ORIENTED_EDGE('',*,*,#14943,.F.);
#20437=ORIENTED_EDGE('',*,*,#14947,.F.);
#20438=ORIENTED_EDGE('',*,*,#14948,.T.);
#20439=ORIENTED_EDGE('',*,*,#14937,.T.);
#20440=ORIENTED_EDGE('',*,*,#14946,.F.);
#20441=ORIENTED_EDGE('',*,*,#14949,.F.);
#20442=ORIENTED_EDGE('',*,*,#14950,.T.);
#20443=ORIENTED_EDGE('',*,*,#14935,.T.);
#20444=ORIENTED_EDGE('',*,*,#14948,.F.);
#20445=ORIENTED_EDGE('',*,*,#14951,.F.);
#20446=ORIENTED_EDGE('',*,*,#14952,.T.);
#20447=ORIENTED_EDGE('',*,*,#14933,.T.);
#20448=ORIENTED_EDGE('',*,*,#14950,.F.);
#20449=ORIENTED_EDGE('',*,*,#14953,.F.);
#20450=ORIENTED_EDGE('',*,*,#14944,.T.);
#20451=ORIENTED_EDGE('',*,*,#14931,.T.);
#20452=ORIENTED_EDGE('',*,*,#14952,.F.);
#20453=ORIENTED_EDGE('',*,*,#14954,.F.);
#20454=ORIENTED_EDGE('',*,*,#14955,.T.);
#20455=ORIENTED_EDGE('',*,*,#14956,.F.);
#20456=ORIENTED_EDGE('',*,*,#14957,.F.);
#20457=ORIENTED_EDGE('',*,*,#14958,.F.);
#20458=ORIENTED_EDGE('',*,*,#14957,.T.);
#20459=ORIENTED_EDGE('',*,*,#14959,.T.);
#20460=ORIENTED_EDGE('',*,*,#14960,.F.);
#20461=ORIENTED_EDGE('',*,*,#14959,.F.);
#20462=ORIENTED_EDGE('',*,*,#14956,.T.);
#20463=ORIENTED_EDGE('',*,*,#14961,.T.);
#20464=ORIENTED_EDGE('',*,*,#14962,.F.);
#20465=ORIENTED_EDGE('',*,*,#14961,.F.);
#20466=ORIENTED_EDGE('',*,*,#14955,.F.);
#20467=ORIENTED_EDGE('',*,*,#14963,.F.);
#20468=ORIENTED_EDGE('',*,*,#14964,.T.);
#20469=ORIENTED_EDGE('',*,*,#14965,.F.);
#20470=ORIENTED_EDGE('',*,*,#14966,.F.);
#20471=ORIENTED_EDGE('',*,*,#14967,.F.);
#20472=ORIENTED_EDGE('',*,*,#14966,.T.);
#20473=ORIENTED_EDGE('',*,*,#14968,.T.);
#20474=ORIENTED_EDGE('',*,*,#14969,.F.);
#20475=ORIENTED_EDGE('',*,*,#14968,.F.);
#20476=ORIENTED_EDGE('',*,*,#14965,.T.);
#20477=ORIENTED_EDGE('',*,*,#14970,.T.);
#20478=ORIENTED_EDGE('',*,*,#14971,.F.);
#20479=ORIENTED_EDGE('',*,*,#14970,.F.);
#20480=ORIENTED_EDGE('',*,*,#14964,.F.);
#20481=ORIENTED_EDGE('',*,*,#14972,.F.);
#20482=ORIENTED_EDGE('',*,*,#14973,.T.);
#20483=ORIENTED_EDGE('',*,*,#14974,.F.);
#20484=ORIENTED_EDGE('',*,*,#14975,.F.);
#20485=ORIENTED_EDGE('',*,*,#14976,.F.);
#20486=ORIENTED_EDGE('',*,*,#14975,.T.);
#20487=ORIENTED_EDGE('',*,*,#14977,.T.);
#20488=ORIENTED_EDGE('',*,*,#14978,.F.);
#20489=ORIENTED_EDGE('',*,*,#14977,.F.);
#20490=ORIENTED_EDGE('',*,*,#14974,.T.);
#20491=ORIENTED_EDGE('',*,*,#14979,.T.);
#20492=ORIENTED_EDGE('',*,*,#14980,.F.);
#20493=ORIENTED_EDGE('',*,*,#14979,.F.);
#20494=ORIENTED_EDGE('',*,*,#14973,.F.);
#20495=ORIENTED_EDGE('',*,*,#14981,.F.);
#20496=ORIENTED_EDGE('',*,*,#14982,.T.);
#20497=ORIENTED_EDGE('',*,*,#14983,.F.);
#20498=ORIENTED_EDGE('',*,*,#14984,.F.);
#20499=ORIENTED_EDGE('',*,*,#14985,.F.);
#20500=ORIENTED_EDGE('',*,*,#14984,.T.);
#20501=ORIENTED_EDGE('',*,*,#14986,.T.);
#20502=ORIENTED_EDGE('',*,*,#14987,.F.);
#20503=ORIENTED_EDGE('',*,*,#14986,.F.);
#20504=ORIENTED_EDGE('',*,*,#14983,.T.);
#20505=ORIENTED_EDGE('',*,*,#14988,.T.);
#20506=ORIENTED_EDGE('',*,*,#14989,.F.);
#20507=ORIENTED_EDGE('',*,*,#14988,.F.);
#20508=ORIENTED_EDGE('',*,*,#14982,.F.);
#20509=ORIENTED_EDGE('',*,*,#14990,.F.);
#20510=ORIENTED_EDGE('',*,*,#14991,.T.);
#20511=ORIENTED_EDGE('',*,*,#14992,.F.);
#20512=ORIENTED_EDGE('',*,*,#14993,.F.);
#20513=ORIENTED_EDGE('',*,*,#14994,.F.);
#20514=ORIENTED_EDGE('',*,*,#14993,.T.);
#20515=ORIENTED_EDGE('',*,*,#14995,.T.);
#20516=ORIENTED_EDGE('',*,*,#14996,.F.);
#20517=ORIENTED_EDGE('',*,*,#14995,.F.);
#20518=ORIENTED_EDGE('',*,*,#14992,.T.);
#20519=ORIENTED_EDGE('',*,*,#14997,.T.);
#20520=ORIENTED_EDGE('',*,*,#14998,.F.);
#20521=ORIENTED_EDGE('',*,*,#14997,.F.);
#20522=ORIENTED_EDGE('',*,*,#14991,.F.);
#20523=ORIENTED_EDGE('',*,*,#14999,.F.);
#20524=ORIENTED_EDGE('',*,*,#15000,.T.);
#20525=ORIENTED_EDGE('',*,*,#15001,.F.);
#20526=ORIENTED_EDGE('',*,*,#15002,.F.);
#20527=ORIENTED_EDGE('',*,*,#15003,.F.);
#20528=ORIENTED_EDGE('',*,*,#15002,.T.);
#20529=ORIENTED_EDGE('',*,*,#15004,.T.);
#20530=ORIENTED_EDGE('',*,*,#15005,.F.);
#20531=ORIENTED_EDGE('',*,*,#15004,.F.);
#20532=ORIENTED_EDGE('',*,*,#15001,.T.);
#20533=ORIENTED_EDGE('',*,*,#15006,.T.);
#20534=ORIENTED_EDGE('',*,*,#15007,.F.);
#20535=ORIENTED_EDGE('',*,*,#15006,.F.);
#20536=ORIENTED_EDGE('',*,*,#15000,.F.);
#20537=ORIENTED_EDGE('',*,*,#15008,.F.);
#20538=ORIENTED_EDGE('',*,*,#15009,.T.);
#20539=ORIENTED_EDGE('',*,*,#15010,.F.);
#20540=ORIENTED_EDGE('',*,*,#15011,.F.);
#20541=ORIENTED_EDGE('',*,*,#15012,.F.);
#20542=ORIENTED_EDGE('',*,*,#15011,.T.);
#20543=ORIENTED_EDGE('',*,*,#15013,.T.);
#20544=ORIENTED_EDGE('',*,*,#15014,.F.);
#20545=ORIENTED_EDGE('',*,*,#15013,.F.);
#20546=ORIENTED_EDGE('',*,*,#15010,.T.);
#20547=ORIENTED_EDGE('',*,*,#15015,.T.);
#20548=ORIENTED_EDGE('',*,*,#15016,.F.);
#20549=ORIENTED_EDGE('',*,*,#15015,.F.);
#20550=ORIENTED_EDGE('',*,*,#15009,.F.);
#20551=ORIENTED_EDGE('',*,*,#15017,.F.);
#20552=ORIENTED_EDGE('',*,*,#15018,.T.);
#20553=ORIENTED_EDGE('',*,*,#15019,.F.);
#20554=ORIENTED_EDGE('',*,*,#15020,.F.);
#20555=ORIENTED_EDGE('',*,*,#15021,.F.);
#20556=ORIENTED_EDGE('',*,*,#15020,.T.);
#20557=ORIENTED_EDGE('',*,*,#15022,.T.);
#20558=ORIENTED_EDGE('',*,*,#15023,.F.);
#20559=ORIENTED_EDGE('',*,*,#15022,.F.);
#20560=ORIENTED_EDGE('',*,*,#15019,.T.);
#20561=ORIENTED_EDGE('',*,*,#15024,.T.);
#20562=ORIENTED_EDGE('',*,*,#15025,.F.);
#20563=ORIENTED_EDGE('',*,*,#15024,.F.);
#20564=ORIENTED_EDGE('',*,*,#15018,.F.);
#20565=ORIENTED_EDGE('',*,*,#15026,.F.);
#20566=ORIENTED_EDGE('',*,*,#15027,.T.);
#20567=ORIENTED_EDGE('',*,*,#15028,.F.);
#20568=ORIENTED_EDGE('',*,*,#15029,.F.);
#20569=ORIENTED_EDGE('',*,*,#15030,.F.);
#20570=ORIENTED_EDGE('',*,*,#15029,.T.);
#20571=ORIENTED_EDGE('',*,*,#15031,.T.);
#20572=ORIENTED_EDGE('',*,*,#15032,.F.);
#20573=ORIENTED_EDGE('',*,*,#15033,.F.);
#20574=ORIENTED_EDGE('',*,*,#15031,.F.);
#20575=ORIENTED_EDGE('',*,*,#15028,.T.);
#20576=ORIENTED_EDGE('',*,*,#15034,.T.);
#20577=ORIENTED_EDGE('',*,*,#15035,.F.);
#20578=ORIENTED_EDGE('',*,*,#15034,.F.);
#20579=ORIENTED_EDGE('',*,*,#15027,.F.);
#20580=ORIENTED_EDGE('',*,*,#15036,.F.);
#20581=ORIENTED_EDGE('',*,*,#15037,.F.);
#20582=ORIENTED_EDGE('',*,*,#15038,.T.);
#20583=ORIENTED_EDGE('',*,*,#15039,.F.);
#20584=ORIENTED_EDGE('',*,*,#15040,.F.);
#20585=ORIENTED_EDGE('',*,*,#15041,.F.);
#20586=ORIENTED_EDGE('',*,*,#15040,.T.);
#20587=ORIENTED_EDGE('',*,*,#15042,.T.);
#20588=ORIENTED_EDGE('',*,*,#15043,.F.);
#20589=ORIENTED_EDGE('',*,*,#15042,.F.);
#20590=ORIENTED_EDGE('',*,*,#15039,.T.);
#20591=ORIENTED_EDGE('',*,*,#15044,.T.);
#20592=ORIENTED_EDGE('',*,*,#15045,.F.);
#20593=ORIENTED_EDGE('',*,*,#15044,.F.);
#20594=ORIENTED_EDGE('',*,*,#15038,.F.);
#20595=ORIENTED_EDGE('',*,*,#15046,.F.);
#20596=ORIENTED_EDGE('',*,*,#15047,.T.);
#20597=ORIENTED_EDGE('',*,*,#15048,.F.);
#20598=ORIENTED_EDGE('',*,*,#15049,.F.);
#20599=ORIENTED_EDGE('',*,*,#15050,.F.);
#20600=ORIENTED_EDGE('',*,*,#15049,.T.);
#20601=ORIENTED_EDGE('',*,*,#15051,.T.);
#20602=ORIENTED_EDGE('',*,*,#15052,.F.);
#20603=ORIENTED_EDGE('',*,*,#15051,.F.);
#20604=ORIENTED_EDGE('',*,*,#15048,.T.);
#20605=ORIENTED_EDGE('',*,*,#15053,.T.);
#20606=ORIENTED_EDGE('',*,*,#15054,.F.);
#20607=ORIENTED_EDGE('',*,*,#15053,.F.);
#20608=ORIENTED_EDGE('',*,*,#15047,.F.);
#20609=ORIENTED_EDGE('',*,*,#15055,.F.);
#20610=ORIENTED_EDGE('',*,*,#15056,.T.);
#20611=ORIENTED_EDGE('',*,*,#15057,.F.);
#20612=ORIENTED_EDGE('',*,*,#15058,.F.);
#20613=ORIENTED_EDGE('',*,*,#15059,.F.);
#20614=ORIENTED_EDGE('',*,*,#15058,.T.);
#20615=ORIENTED_EDGE('',*,*,#15060,.T.);
#20616=ORIENTED_EDGE('',*,*,#15061,.F.);
#20617=ORIENTED_EDGE('',*,*,#15060,.F.);
#20618=ORIENTED_EDGE('',*,*,#15057,.T.);
#20619=ORIENTED_EDGE('',*,*,#15062,.T.);
#20620=ORIENTED_EDGE('',*,*,#15063,.F.);
#20621=ORIENTED_EDGE('',*,*,#15062,.F.);
#20622=ORIENTED_EDGE('',*,*,#15056,.F.);
#20623=ORIENTED_EDGE('',*,*,#15064,.F.);
#20624=ORIENTED_EDGE('',*,*,#15065,.T.);
#20625=ORIENTED_EDGE('',*,*,#15066,.F.);
#20626=ORIENTED_EDGE('',*,*,#15067,.F.);
#20627=ORIENTED_EDGE('',*,*,#15068,.F.);
#20628=ORIENTED_EDGE('',*,*,#15067,.T.);
#20629=ORIENTED_EDGE('',*,*,#15069,.T.);
#20630=ORIENTED_EDGE('',*,*,#15070,.F.);
#20631=ORIENTED_EDGE('',*,*,#15069,.F.);
#20632=ORIENTED_EDGE('',*,*,#15066,.T.);
#20633=ORIENTED_EDGE('',*,*,#15071,.T.);
#20634=ORIENTED_EDGE('',*,*,#15072,.F.);
#20635=ORIENTED_EDGE('',*,*,#15071,.F.);
#20636=ORIENTED_EDGE('',*,*,#15065,.F.);
#20637=ORIENTED_EDGE('',*,*,#15073,.F.);
#20638=ORIENTED_EDGE('',*,*,#15074,.T.);
#20639=ORIENTED_EDGE('',*,*,#15075,.F.);
#20640=ORIENTED_EDGE('',*,*,#15076,.F.);
#20641=ORIENTED_EDGE('',*,*,#15077,.F.);
#20642=ORIENTED_EDGE('',*,*,#15076,.T.);
#20643=ORIENTED_EDGE('',*,*,#15078,.T.);
#20644=ORIENTED_EDGE('',*,*,#15079,.F.);
#20645=ORIENTED_EDGE('',*,*,#15078,.F.);
#20646=ORIENTED_EDGE('',*,*,#15075,.T.);
#20647=ORIENTED_EDGE('',*,*,#15080,.T.);
#20648=ORIENTED_EDGE('',*,*,#15081,.F.);
#20649=ORIENTED_EDGE('',*,*,#15080,.F.);
#20650=ORIENTED_EDGE('',*,*,#15074,.F.);
#20651=ORIENTED_EDGE('',*,*,#15082,.F.);
#20652=ORIENTED_EDGE('',*,*,#15083,.T.);
#20653=ORIENTED_EDGE('',*,*,#15084,.F.);
#20654=ORIENTED_EDGE('',*,*,#15085,.F.);
#20655=ORIENTED_EDGE('',*,*,#15086,.F.);
#20656=ORIENTED_EDGE('',*,*,#15085,.T.);
#20657=ORIENTED_EDGE('',*,*,#15087,.T.);
#20658=ORIENTED_EDGE('',*,*,#15088,.F.);
#20659=ORIENTED_EDGE('',*,*,#15087,.F.);
#20660=ORIENTED_EDGE('',*,*,#15084,.T.);
#20661=ORIENTED_EDGE('',*,*,#15089,.T.);
#20662=ORIENTED_EDGE('',*,*,#15090,.F.);
#20663=ORIENTED_EDGE('',*,*,#15089,.F.);
#20664=ORIENTED_EDGE('',*,*,#15083,.F.);
#20665=ORIENTED_EDGE('',*,*,#15091,.F.);
#20666=ORIENTED_EDGE('',*,*,#15092,.T.);
#20667=ORIENTED_EDGE('',*,*,#15093,.F.);
#20668=ORIENTED_EDGE('',*,*,#15094,.F.);
#20669=ORIENTED_EDGE('',*,*,#15095,.F.);
#20670=ORIENTED_EDGE('',*,*,#15094,.T.);
#20671=ORIENTED_EDGE('',*,*,#15096,.T.);
#20672=ORIENTED_EDGE('',*,*,#15097,.F.);
#20673=ORIENTED_EDGE('',*,*,#15096,.F.);
#20674=ORIENTED_EDGE('',*,*,#15093,.T.);
#20675=ORIENTED_EDGE('',*,*,#15098,.T.);
#20676=ORIENTED_EDGE('',*,*,#15099,.F.);
#20677=ORIENTED_EDGE('',*,*,#15098,.F.);
#20678=ORIENTED_EDGE('',*,*,#15092,.F.);
#20679=ORIENTED_EDGE('',*,*,#15100,.F.);
#20680=ORIENTED_EDGE('',*,*,#15101,.T.);
#20681=ORIENTED_EDGE('',*,*,#15102,.F.);
#20682=ORIENTED_EDGE('',*,*,#15103,.F.);
#20683=ORIENTED_EDGE('',*,*,#15104,.F.);
#20684=ORIENTED_EDGE('',*,*,#15103,.T.);
#20685=ORIENTED_EDGE('',*,*,#15105,.T.);
#20686=ORIENTED_EDGE('',*,*,#15106,.F.);
#20687=ORIENTED_EDGE('',*,*,#15105,.F.);
#20688=ORIENTED_EDGE('',*,*,#15102,.T.);
#20689=ORIENTED_EDGE('',*,*,#15107,.T.);
#20690=ORIENTED_EDGE('',*,*,#15108,.F.);
#20691=ORIENTED_EDGE('',*,*,#15107,.F.);
#20692=ORIENTED_EDGE('',*,*,#15101,.F.);
#20693=ORIENTED_EDGE('',*,*,#15109,.F.);
#20694=ORIENTED_EDGE('',*,*,#15110,.T.);
#20695=ORIENTED_EDGE('',*,*,#15111,.F.);
#20696=ORIENTED_EDGE('',*,*,#15112,.F.);
#20697=ORIENTED_EDGE('',*,*,#15113,.F.);
#20698=ORIENTED_EDGE('',*,*,#15112,.T.);
#20699=ORIENTED_EDGE('',*,*,#15114,.T.);
#20700=ORIENTED_EDGE('',*,*,#15115,.F.);
#20701=ORIENTED_EDGE('',*,*,#15114,.F.);
#20702=ORIENTED_EDGE('',*,*,#15111,.T.);
#20703=ORIENTED_EDGE('',*,*,#15116,.T.);
#20704=ORIENTED_EDGE('',*,*,#15117,.F.);
#20705=ORIENTED_EDGE('',*,*,#15116,.F.);
#20706=ORIENTED_EDGE('',*,*,#15110,.F.);
#20707=ORIENTED_EDGE('',*,*,#15118,.F.);
#20708=ORIENTED_EDGE('',*,*,#15119,.T.);
#20709=ORIENTED_EDGE('',*,*,#15120,.F.);
#20710=ORIENTED_EDGE('',*,*,#15121,.F.);
#20711=ORIENTED_EDGE('',*,*,#15122,.F.);
#20712=ORIENTED_EDGE('',*,*,#15121,.T.);
#20713=ORIENTED_EDGE('',*,*,#15123,.T.);
#20714=ORIENTED_EDGE('',*,*,#15124,.F.);
#20715=ORIENTED_EDGE('',*,*,#15123,.F.);
#20716=ORIENTED_EDGE('',*,*,#15120,.T.);
#20717=ORIENTED_EDGE('',*,*,#15125,.T.);
#20718=ORIENTED_EDGE('',*,*,#15126,.F.);
#20719=ORIENTED_EDGE('',*,*,#15125,.F.);
#20720=ORIENTED_EDGE('',*,*,#15119,.F.);
#20721=ORIENTED_EDGE('',*,*,#15127,.F.);
#20722=ORIENTED_EDGE('',*,*,#15128,.T.);
#20723=ORIENTED_EDGE('',*,*,#15129,.F.);
#20724=ORIENTED_EDGE('',*,*,#15130,.F.);
#20725=ORIENTED_EDGE('',*,*,#15131,.F.);
#20726=ORIENTED_EDGE('',*,*,#15130,.T.);
#20727=ORIENTED_EDGE('',*,*,#15132,.T.);
#20728=ORIENTED_EDGE('',*,*,#15133,.F.);
#20729=ORIENTED_EDGE('',*,*,#15132,.F.);
#20730=ORIENTED_EDGE('',*,*,#15129,.T.);
#20731=ORIENTED_EDGE('',*,*,#15134,.T.);
#20732=ORIENTED_EDGE('',*,*,#15135,.F.);
#20733=ORIENTED_EDGE('',*,*,#15134,.F.);
#20734=ORIENTED_EDGE('',*,*,#15128,.F.);
#20735=ORIENTED_EDGE('',*,*,#15136,.F.);
#20736=ORIENTED_EDGE('',*,*,#15137,.T.);
#20737=ORIENTED_EDGE('',*,*,#15138,.F.);
#20738=ORIENTED_EDGE('',*,*,#15139,.F.);
#20739=ORIENTED_EDGE('',*,*,#15140,.F.);
#20740=ORIENTED_EDGE('',*,*,#15139,.T.);
#20741=ORIENTED_EDGE('',*,*,#15141,.T.);
#20742=ORIENTED_EDGE('',*,*,#15142,.F.);
#20743=ORIENTED_EDGE('',*,*,#15141,.F.);
#20744=ORIENTED_EDGE('',*,*,#15138,.T.);
#20745=ORIENTED_EDGE('',*,*,#15143,.T.);
#20746=ORIENTED_EDGE('',*,*,#15144,.F.);
#20747=ORIENTED_EDGE('',*,*,#15143,.F.);
#20748=ORIENTED_EDGE('',*,*,#15137,.F.);
#20749=ORIENTED_EDGE('',*,*,#15145,.F.);
#20750=ORIENTED_EDGE('',*,*,#15146,.T.);
#20751=ORIENTED_EDGE('',*,*,#15147,.F.);
#20752=ORIENTED_EDGE('',*,*,#15148,.F.);
#20753=ORIENTED_EDGE('',*,*,#15149,.F.);
#20754=ORIENTED_EDGE('',*,*,#15148,.T.);
#20755=ORIENTED_EDGE('',*,*,#15150,.T.);
#20756=ORIENTED_EDGE('',*,*,#15151,.F.);
#20757=ORIENTED_EDGE('',*,*,#15150,.F.);
#20758=ORIENTED_EDGE('',*,*,#15147,.T.);
#20759=ORIENTED_EDGE('',*,*,#15152,.T.);
#20760=ORIENTED_EDGE('',*,*,#15153,.F.);
#20761=ORIENTED_EDGE('',*,*,#15152,.F.);
#20762=ORIENTED_EDGE('',*,*,#15146,.F.);
#20763=ORIENTED_EDGE('',*,*,#15154,.F.);
#20764=ORIENTED_EDGE('',*,*,#15155,.T.);
#20765=ORIENTED_EDGE('',*,*,#15156,.F.);
#20766=ORIENTED_EDGE('',*,*,#15157,.F.);
#20767=ORIENTED_EDGE('',*,*,#15158,.F.);
#20768=ORIENTED_EDGE('',*,*,#15157,.T.);
#20769=ORIENTED_EDGE('',*,*,#15159,.T.);
#20770=ORIENTED_EDGE('',*,*,#15160,.F.);
#20771=ORIENTED_EDGE('',*,*,#15159,.F.);
#20772=ORIENTED_EDGE('',*,*,#15156,.T.);
#20773=ORIENTED_EDGE('',*,*,#15161,.T.);
#20774=ORIENTED_EDGE('',*,*,#15162,.F.);
#20775=ORIENTED_EDGE('',*,*,#15161,.F.);
#20776=ORIENTED_EDGE('',*,*,#15155,.F.);
#20777=ORIENTED_EDGE('',*,*,#15163,.F.);
#20778=ORIENTED_EDGE('',*,*,#15164,.T.);
#20779=ORIENTED_EDGE('',*,*,#15165,.F.);
#20780=ORIENTED_EDGE('',*,*,#15166,.F.);
#20781=ORIENTED_EDGE('',*,*,#15167,.F.);
#20782=ORIENTED_EDGE('',*,*,#15166,.T.);
#20783=ORIENTED_EDGE('',*,*,#15168,.T.);
#20784=ORIENTED_EDGE('',*,*,#15169,.F.);
#20785=ORIENTED_EDGE('',*,*,#15168,.F.);
#20786=ORIENTED_EDGE('',*,*,#15165,.T.);
#20787=ORIENTED_EDGE('',*,*,#15170,.T.);
#20788=ORIENTED_EDGE('',*,*,#15171,.F.);
#20789=ORIENTED_EDGE('',*,*,#15170,.F.);
#20790=ORIENTED_EDGE('',*,*,#15164,.F.);
#20791=ORIENTED_EDGE('',*,*,#15172,.F.);
#20792=ORIENTED_EDGE('',*,*,#15173,.T.);
#20793=ORIENTED_EDGE('',*,*,#15174,.F.);
#20794=ORIENTED_EDGE('',*,*,#15175,.F.);
#20795=ORIENTED_EDGE('',*,*,#15176,.F.);
#20796=ORIENTED_EDGE('',*,*,#15175,.T.);
#20797=ORIENTED_EDGE('',*,*,#15177,.T.);
#20798=ORIENTED_EDGE('',*,*,#15178,.F.);
#20799=ORIENTED_EDGE('',*,*,#15177,.F.);
#20800=ORIENTED_EDGE('',*,*,#15174,.T.);
#20801=ORIENTED_EDGE('',*,*,#15179,.T.);
#20802=ORIENTED_EDGE('',*,*,#15180,.F.);
#20803=ORIENTED_EDGE('',*,*,#15179,.F.);
#20804=ORIENTED_EDGE('',*,*,#15173,.F.);
#20805=ORIENTED_EDGE('',*,*,#15181,.F.);
#20806=ORIENTED_EDGE('',*,*,#15182,.T.);
#20807=ORIENTED_EDGE('',*,*,#15183,.F.);
#20808=ORIENTED_EDGE('',*,*,#15184,.F.);
#20809=ORIENTED_EDGE('',*,*,#15185,.F.);
#20810=ORIENTED_EDGE('',*,*,#15184,.T.);
#20811=ORIENTED_EDGE('',*,*,#15186,.T.);
#20812=ORIENTED_EDGE('',*,*,#15187,.F.);
#20813=ORIENTED_EDGE('',*,*,#15186,.F.);
#20814=ORIENTED_EDGE('',*,*,#15183,.T.);
#20815=ORIENTED_EDGE('',*,*,#15188,.T.);
#20816=ORIENTED_EDGE('',*,*,#15189,.F.);
#20817=ORIENTED_EDGE('',*,*,#15188,.F.);
#20818=ORIENTED_EDGE('',*,*,#15182,.F.);
#20819=ORIENTED_EDGE('',*,*,#15190,.F.);
#20820=ORIENTED_EDGE('',*,*,#15191,.T.);
#20821=ORIENTED_EDGE('',*,*,#15192,.T.);
#20822=ORIENTED_EDGE('',*,*,#15193,.F.);
#20823=ORIENTED_EDGE('',*,*,#15194,.T.);
#20824=ORIENTED_EDGE('',*,*,#15195,.F.);
#20825=ORIENTED_EDGE('',*,*,#15191,.F.);
#20826=ORIENTED_EDGE('',*,*,#15196,.F.);
#20827=ORIENTED_EDGE('',*,*,#15192,.F.);
#20828=ORIENTED_EDGE('',*,*,#15195,.T.);
#20829=ORIENTED_EDGE('',*,*,#15197,.T.);
#20830=ORIENTED_EDGE('',*,*,#15198,.F.);
#20831=ORIENTED_EDGE('',*,*,#15197,.F.);
#20832=ORIENTED_EDGE('',*,*,#15194,.F.);
#20833=ORIENTED_EDGE('',*,*,#15199,.F.);
#20834=ORIENTED_EDGE('',*,*,#15200,.T.);
#20835=ORIENTED_EDGE('',*,*,#15201,.F.);
#20836=ORIENTED_EDGE('',*,*,#15202,.F.);
#20837=ORIENTED_EDGE('',*,*,#15203,.F.);
#20838=ORIENTED_EDGE('',*,*,#15202,.T.);
#20839=ORIENTED_EDGE('',*,*,#15204,.T.);
#20840=ORIENTED_EDGE('',*,*,#15205,.F.);
#20841=ORIENTED_EDGE('',*,*,#15204,.F.);
#20842=ORIENTED_EDGE('',*,*,#15201,.T.);
#20843=ORIENTED_EDGE('',*,*,#15206,.T.);
#20844=ORIENTED_EDGE('',*,*,#15207,.F.);
#20845=ORIENTED_EDGE('',*,*,#15206,.F.);
#20846=ORIENTED_EDGE('',*,*,#15200,.F.);
#20847=ORIENTED_EDGE('',*,*,#15208,.F.);
#20848=ORIENTED_EDGE('',*,*,#15209,.T.);
#20849=ORIENTED_EDGE('',*,*,#15210,.F.);
#20850=ORIENTED_EDGE('',*,*,#15211,.F.);
#20851=ORIENTED_EDGE('',*,*,#15212,.F.);
#20852=ORIENTED_EDGE('',*,*,#15211,.T.);
#20853=ORIENTED_EDGE('',*,*,#15213,.T.);
#20854=ORIENTED_EDGE('',*,*,#15214,.F.);
#20855=ORIENTED_EDGE('',*,*,#15213,.F.);
#20856=ORIENTED_EDGE('',*,*,#15210,.T.);
#20857=ORIENTED_EDGE('',*,*,#15215,.T.);
#20858=ORIENTED_EDGE('',*,*,#15216,.F.);
#20859=ORIENTED_EDGE('',*,*,#15215,.F.);
#20860=ORIENTED_EDGE('',*,*,#15209,.F.);
#20861=ORIENTED_EDGE('',*,*,#15217,.F.);
#20862=ORIENTED_EDGE('',*,*,#15218,.T.);
#20863=ORIENTED_EDGE('',*,*,#15219,.F.);
#20864=ORIENTED_EDGE('',*,*,#15220,.F.);
#20865=ORIENTED_EDGE('',*,*,#15221,.F.);
#20866=ORIENTED_EDGE('',*,*,#15220,.T.);
#20867=ORIENTED_EDGE('',*,*,#15222,.T.);
#20868=ORIENTED_EDGE('',*,*,#15223,.F.);
#20869=ORIENTED_EDGE('',*,*,#15222,.F.);
#20870=ORIENTED_EDGE('',*,*,#15219,.T.);
#20871=ORIENTED_EDGE('',*,*,#15224,.T.);
#20872=ORIENTED_EDGE('',*,*,#15225,.F.);
#20873=ORIENTED_EDGE('',*,*,#15224,.F.);
#20874=ORIENTED_EDGE('',*,*,#15218,.F.);
#20875=ORIENTED_EDGE('',*,*,#15226,.F.);
#20876=ORIENTED_EDGE('',*,*,#15227,.T.);
#20877=ORIENTED_EDGE('',*,*,#15228,.F.);
#20878=ORIENTED_EDGE('',*,*,#15229,.F.);
#20879=ORIENTED_EDGE('',*,*,#15230,.F.);
#20880=ORIENTED_EDGE('',*,*,#15229,.T.);
#20881=ORIENTED_EDGE('',*,*,#15231,.T.);
#20882=ORIENTED_EDGE('',*,*,#15232,.F.);
#20883=ORIENTED_EDGE('',*,*,#15231,.F.);
#20884=ORIENTED_EDGE('',*,*,#15228,.T.);
#20885=ORIENTED_EDGE('',*,*,#15233,.T.);
#20886=ORIENTED_EDGE('',*,*,#15234,.F.);
#20887=ORIENTED_EDGE('',*,*,#15233,.F.);
#20888=ORIENTED_EDGE('',*,*,#15227,.F.);
#20889=ORIENTED_EDGE('',*,*,#15235,.F.);
#20890=ORIENTED_EDGE('',*,*,#15236,.T.);
#20891=ORIENTED_EDGE('',*,*,#15237,.F.);
#20892=ORIENTED_EDGE('',*,*,#15238,.F.);
#20893=ORIENTED_EDGE('',*,*,#15239,.F.);
#20894=ORIENTED_EDGE('',*,*,#15238,.T.);
#20895=ORIENTED_EDGE('',*,*,#15240,.T.);
#20896=ORIENTED_EDGE('',*,*,#15241,.F.);
#20897=ORIENTED_EDGE('',*,*,#15240,.F.);
#20898=ORIENTED_EDGE('',*,*,#15237,.T.);
#20899=ORIENTED_EDGE('',*,*,#15242,.T.);
#20900=ORIENTED_EDGE('',*,*,#15243,.F.);
#20901=ORIENTED_EDGE('',*,*,#15242,.F.);
#20902=ORIENTED_EDGE('',*,*,#15236,.F.);
#20903=ORIENTED_EDGE('',*,*,#15244,.F.);
#20904=ORIENTED_EDGE('',*,*,#15245,.T.);
#20905=ORIENTED_EDGE('',*,*,#15246,.F.);
#20906=ORIENTED_EDGE('',*,*,#15247,.F.);
#20907=ORIENTED_EDGE('',*,*,#15248,.F.);
#20908=ORIENTED_EDGE('',*,*,#15247,.T.);
#20909=ORIENTED_EDGE('',*,*,#15249,.T.);
#20910=ORIENTED_EDGE('',*,*,#15250,.F.);
#20911=ORIENTED_EDGE('',*,*,#15249,.F.);
#20912=ORIENTED_EDGE('',*,*,#15246,.T.);
#20913=ORIENTED_EDGE('',*,*,#15251,.T.);
#20914=ORIENTED_EDGE('',*,*,#15252,.F.);
#20915=ORIENTED_EDGE('',*,*,#15251,.F.);
#20916=ORIENTED_EDGE('',*,*,#15245,.F.);
#20917=ORIENTED_EDGE('',*,*,#15253,.F.);
#20918=ORIENTED_EDGE('',*,*,#15254,.T.);
#20919=ORIENTED_EDGE('',*,*,#15255,.F.);
#20920=ORIENTED_EDGE('',*,*,#15256,.F.);
#20921=ORIENTED_EDGE('',*,*,#15257,.F.);
#20922=ORIENTED_EDGE('',*,*,#15256,.T.);
#20923=ORIENTED_EDGE('',*,*,#15258,.T.);
#20924=ORIENTED_EDGE('',*,*,#15259,.F.);
#20925=ORIENTED_EDGE('',*,*,#15258,.F.);
#20926=ORIENTED_EDGE('',*,*,#15255,.T.);
#20927=ORIENTED_EDGE('',*,*,#15260,.T.);
#20928=ORIENTED_EDGE('',*,*,#15261,.F.);
#20929=ORIENTED_EDGE('',*,*,#15260,.F.);
#20930=ORIENTED_EDGE('',*,*,#15254,.F.);
#20931=ORIENTED_EDGE('',*,*,#15262,.F.);
#20932=ORIENTED_EDGE('',*,*,#15263,.T.);
#20933=ORIENTED_EDGE('',*,*,#15264,.F.);
#20934=ORIENTED_EDGE('',*,*,#15265,.F.);
#20935=ORIENTED_EDGE('',*,*,#15266,.F.);
#20936=ORIENTED_EDGE('',*,*,#15265,.T.);
#20937=ORIENTED_EDGE('',*,*,#15267,.T.);
#20938=ORIENTED_EDGE('',*,*,#15268,.F.);
#20939=ORIENTED_EDGE('',*,*,#15267,.F.);
#20940=ORIENTED_EDGE('',*,*,#15264,.T.);
#20941=ORIENTED_EDGE('',*,*,#15269,.T.);
#20942=ORIENTED_EDGE('',*,*,#15270,.F.);
#20943=ORIENTED_EDGE('',*,*,#15269,.F.);
#20944=ORIENTED_EDGE('',*,*,#15263,.F.);
#20945=ORIENTED_EDGE('',*,*,#15271,.F.);
#20946=ORIENTED_EDGE('',*,*,#15272,.T.);
#20947=ORIENTED_EDGE('',*,*,#15273,.F.);
#20948=ORIENTED_EDGE('',*,*,#15274,.F.);
#20949=ORIENTED_EDGE('',*,*,#15275,.F.);
#20950=ORIENTED_EDGE('',*,*,#15274,.T.);
#20951=ORIENTED_EDGE('',*,*,#15276,.T.);
#20952=ORIENTED_EDGE('',*,*,#15277,.F.);
#20953=ORIENTED_EDGE('',*,*,#15276,.F.);
#20954=ORIENTED_EDGE('',*,*,#15273,.T.);
#20955=ORIENTED_EDGE('',*,*,#15278,.T.);
#20956=ORIENTED_EDGE('',*,*,#15279,.F.);
#20957=ORIENTED_EDGE('',*,*,#15278,.F.);
#20958=ORIENTED_EDGE('',*,*,#15272,.F.);
#20959=ORIENTED_EDGE('',*,*,#15280,.F.);
#20960=ORIENTED_EDGE('',*,*,#14919,.F.);
#20961=ORIENTED_EDGE('',*,*,#14819,.F.);
#20962=ORIENTED_EDGE('',*,*,#14920,.F.);
#20963=ORIENTED_EDGE('',*,*,#15281,.T.);
#20964=ORIENTED_EDGE('',*,*,#15280,.T.);
#20965=ORIENTED_EDGE('',*,*,#15281,.F.);
#20966=ORIENTED_EDGE('',*,*,#15282,.F.);
#20967=ORIENTED_EDGE('',*,*,#15283,.T.);
#20968=ORIENTED_EDGE('',*,*,#14928,.T.);
#20969=ORIENTED_EDGE('',*,*,#15283,.F.);
#20970=ORIENTED_EDGE('',*,*,#14954,.T.);
#20971=ORIENTED_EDGE('',*,*,#15284,.F.);
#20972=ORIENTED_EDGE('',*,*,#15268,.T.);
#20973=ORIENTED_EDGE('',*,*,#15270,.T.);
#20974=ORIENTED_EDGE('',*,*,#15262,.T.);
#20975=ORIENTED_EDGE('',*,*,#15285,.F.);
#20976=ORIENTED_EDGE('',*,*,#14969,.T.);
#20977=ORIENTED_EDGE('',*,*,#14971,.T.);
#20978=ORIENTED_EDGE('',*,*,#14963,.T.);
#20979=ORIENTED_EDGE('',*,*,#15286,.F.);
#20980=ORIENTED_EDGE('',*,*,#15259,.T.);
#20981=ORIENTED_EDGE('',*,*,#15261,.T.);
#20982=ORIENTED_EDGE('',*,*,#15253,.T.);
#20983=ORIENTED_EDGE('',*,*,#15287,.F.);
#20984=ORIENTED_EDGE('',*,*,#14978,.T.);
#20985=ORIENTED_EDGE('',*,*,#14980,.T.);
#20986=ORIENTED_EDGE('',*,*,#14972,.T.);
#20987=ORIENTED_EDGE('',*,*,#15288,.F.);
#20988=ORIENTED_EDGE('',*,*,#15250,.T.);
#20989=ORIENTED_EDGE('',*,*,#15252,.T.);
#20990=ORIENTED_EDGE('',*,*,#15244,.T.);
#20991=ORIENTED_EDGE('',*,*,#15289,.F.);
#20992=ORIENTED_EDGE('',*,*,#14987,.T.);
#20993=ORIENTED_EDGE('',*,*,#14989,.T.);
#20994=ORIENTED_EDGE('',*,*,#14981,.T.);
#20995=ORIENTED_EDGE('',*,*,#15290,.F.);
#20996=ORIENTED_EDGE('',*,*,#15241,.T.);
#20997=ORIENTED_EDGE('',*,*,#15243,.T.);
#20998=ORIENTED_EDGE('',*,*,#15235,.T.);
#20999=ORIENTED_EDGE('',*,*,#15291,.F.);
#21000=ORIENTED_EDGE('',*,*,#14996,.T.);
#21001=ORIENTED_EDGE('',*,*,#14998,.T.);
#21002=ORIENTED_EDGE('',*,*,#14990,.T.);
#21003=ORIENTED_EDGE('',*,*,#15292,.F.);
#21004=ORIENTED_EDGE('',*,*,#15232,.T.);
#21005=ORIENTED_EDGE('',*,*,#15234,.T.);
#21006=ORIENTED_EDGE('',*,*,#15226,.T.);
#21007=ORIENTED_EDGE('',*,*,#15293,.F.);
#21008=ORIENTED_EDGE('',*,*,#15005,.T.);
#21009=ORIENTED_EDGE('',*,*,#15007,.T.);
#21010=ORIENTED_EDGE('',*,*,#14999,.T.);
#21011=ORIENTED_EDGE('',*,*,#15294,.F.);
#21012=ORIENTED_EDGE('',*,*,#15223,.T.);
#21013=ORIENTED_EDGE('',*,*,#15225,.T.);
#21014=ORIENTED_EDGE('',*,*,#15217,.T.);
#21015=ORIENTED_EDGE('',*,*,#15295,.F.);
#21016=ORIENTED_EDGE('',*,*,#15014,.T.);
#21017=ORIENTED_EDGE('',*,*,#15016,.T.);
#21018=ORIENTED_EDGE('',*,*,#15008,.T.);
#21019=ORIENTED_EDGE('',*,*,#15296,.F.);
#21020=ORIENTED_EDGE('',*,*,#15214,.T.);
#21021=ORIENTED_EDGE('',*,*,#15216,.T.);
#21022=ORIENTED_EDGE('',*,*,#15208,.T.);
#21023=ORIENTED_EDGE('',*,*,#15297,.F.);
#21024=ORIENTED_EDGE('',*,*,#15023,.T.);
#21025=ORIENTED_EDGE('',*,*,#15025,.T.);
#21026=ORIENTED_EDGE('',*,*,#15017,.T.);
#21027=ORIENTED_EDGE('',*,*,#15298,.F.);
#21028=ORIENTED_EDGE('',*,*,#15205,.T.);
#21029=ORIENTED_EDGE('',*,*,#15207,.T.);
#21030=ORIENTED_EDGE('',*,*,#15199,.T.);
#21031=ORIENTED_EDGE('',*,*,#15299,.F.);
#21032=ORIENTED_EDGE('',*,*,#15033,.T.);
#21033=ORIENTED_EDGE('',*,*,#15035,.T.);
#21034=ORIENTED_EDGE('',*,*,#15300,.T.);
#21035=ORIENTED_EDGE('',*,*,#15282,.T.);
#21036=ORIENTED_EDGE('',*,*,#15300,.F.);
#21037=ORIENTED_EDGE('',*,*,#15036,.T.);
#21038=ORIENTED_EDGE('',*,*,#15026,.T.);
#21039=ORIENTED_EDGE('',*,*,#15301,.F.);
#21040=ORIENTED_EDGE('',*,*,#15043,.T.);
#21041=ORIENTED_EDGE('',*,*,#15045,.T.);
#21042=ORIENTED_EDGE('',*,*,#15037,.T.);
#21043=ORIENTED_EDGE('',*,*,#15302,.F.);
#21044=ORIENTED_EDGE('',*,*,#15187,.T.);
#21045=ORIENTED_EDGE('',*,*,#15189,.T.);
#21046=ORIENTED_EDGE('',*,*,#15181,.T.);
#21047=ORIENTED_EDGE('',*,*,#15303,.F.);
#21048=ORIENTED_EDGE('',*,*,#15052,.T.);
#21049=ORIENTED_EDGE('',*,*,#15054,.T.);
#21050=ORIENTED_EDGE('',*,*,#15046,.T.);
#21051=ORIENTED_EDGE('',*,*,#15304,.F.);
#21052=ORIENTED_EDGE('',*,*,#15178,.T.);
#21053=ORIENTED_EDGE('',*,*,#15180,.T.);
#21054=ORIENTED_EDGE('',*,*,#15172,.T.);
#21055=ORIENTED_EDGE('',*,*,#15305,.F.);
#21056=ORIENTED_EDGE('',*,*,#15061,.T.);
#21057=ORIENTED_EDGE('',*,*,#15063,.T.);
#21058=ORIENTED_EDGE('',*,*,#15055,.T.);
#21059=ORIENTED_EDGE('',*,*,#15306,.F.);
#21060=ORIENTED_EDGE('',*,*,#15169,.T.);
#21061=ORIENTED_EDGE('',*,*,#15171,.T.);
#21062=ORIENTED_EDGE('',*,*,#15163,.T.);
#21063=ORIENTED_EDGE('',*,*,#15307,.F.);
#21064=ORIENTED_EDGE('',*,*,#15070,.T.);
#21065=ORIENTED_EDGE('',*,*,#15072,.T.);
#21066=ORIENTED_EDGE('',*,*,#15064,.T.);
#21067=ORIENTED_EDGE('',*,*,#15308,.F.);
#21068=ORIENTED_EDGE('',*,*,#15160,.T.);
#21069=ORIENTED_EDGE('',*,*,#15162,.T.);
#21070=ORIENTED_EDGE('',*,*,#15154,.T.);
#21071=ORIENTED_EDGE('',*,*,#15309,.F.);
#21072=ORIENTED_EDGE('',*,*,#15079,.T.);
#21073=ORIENTED_EDGE('',*,*,#15081,.T.);
#21074=ORIENTED_EDGE('',*,*,#15073,.T.);
#21075=ORIENTED_EDGE('',*,*,#15310,.F.);
#21076=ORIENTED_EDGE('',*,*,#15151,.T.);
#21077=ORIENTED_EDGE('',*,*,#15153,.T.);
#21078=ORIENTED_EDGE('',*,*,#15145,.T.);
#21079=ORIENTED_EDGE('',*,*,#15311,.F.);
#21080=ORIENTED_EDGE('',*,*,#15088,.T.);
#21081=ORIENTED_EDGE('',*,*,#15090,.T.);
#21082=ORIENTED_EDGE('',*,*,#15082,.T.);
#21083=ORIENTED_EDGE('',*,*,#15312,.F.);
#21084=ORIENTED_EDGE('',*,*,#15142,.T.);
#21085=ORIENTED_EDGE('',*,*,#15144,.T.);
#21086=ORIENTED_EDGE('',*,*,#15136,.T.);
#21087=ORIENTED_EDGE('',*,*,#15313,.F.);
#21088=ORIENTED_EDGE('',*,*,#15097,.T.);
#21089=ORIENTED_EDGE('',*,*,#15099,.T.);
#21090=ORIENTED_EDGE('',*,*,#15091,.T.);
#21091=ORIENTED_EDGE('',*,*,#15314,.F.);
#21092=ORIENTED_EDGE('',*,*,#15133,.T.);
#21093=ORIENTED_EDGE('',*,*,#15135,.T.);
#21094=ORIENTED_EDGE('',*,*,#15127,.T.);
#21095=ORIENTED_EDGE('',*,*,#15315,.F.);
#21096=ORIENTED_EDGE('',*,*,#15106,.T.);
#21097=ORIENTED_EDGE('',*,*,#15108,.T.);
#21098=ORIENTED_EDGE('',*,*,#15100,.T.);
#21099=ORIENTED_EDGE('',*,*,#15316,.F.);
#21100=ORIENTED_EDGE('',*,*,#15124,.T.);
#21101=ORIENTED_EDGE('',*,*,#15126,.T.);
#21102=ORIENTED_EDGE('',*,*,#15118,.T.);
#21103=ORIENTED_EDGE('',*,*,#15317,.F.);
#21104=ORIENTED_EDGE('',*,*,#15115,.T.);
#21105=ORIENTED_EDGE('',*,*,#15117,.T.);
#21106=ORIENTED_EDGE('',*,*,#15109,.T.);
#21107=ORIENTED_EDGE('',*,*,#15318,.F.);
#21108=ORIENTED_EDGE('',*,*,#15196,.T.);
#21109=ORIENTED_EDGE('',*,*,#15198,.T.);
#21110=ORIENTED_EDGE('',*,*,#15193,.T.);
#21111=ORIENTED_EDGE('',*,*,#15319,.F.);
#21112=ORIENTED_EDGE('',*,*,#15277,.T.);
#21113=ORIENTED_EDGE('',*,*,#15279,.T.);
#21114=ORIENTED_EDGE('',*,*,#15271,.T.);
#21115=ORIENTED_EDGE('',*,*,#15320,.F.);
#21116=ORIENTED_EDGE('',*,*,#14960,.T.);
#21117=ORIENTED_EDGE('',*,*,#14962,.T.);
#21118=ORIENTED_EDGE('',*,*,#15321,.F.);
#21119=ORIENTED_EDGE('',*,*,#15322,.T.);
#21120=ORIENTED_EDGE('',*,*,#15032,.T.);
#21121=ORIENTED_EDGE('',*,*,#15299,.T.);
#21122=ORIENTED_EDGE('',*,*,#15203,.T.);
#21123=ORIENTED_EDGE('',*,*,#15298,.T.);
#21124=ORIENTED_EDGE('',*,*,#15021,.T.);
#21125=ORIENTED_EDGE('',*,*,#15297,.T.);
#21126=ORIENTED_EDGE('',*,*,#15212,.T.);
#21127=ORIENTED_EDGE('',*,*,#15296,.T.);
#21128=ORIENTED_EDGE('',*,*,#15012,.T.);
#21129=ORIENTED_EDGE('',*,*,#15295,.T.);
#21130=ORIENTED_EDGE('',*,*,#15221,.T.);
#21131=ORIENTED_EDGE('',*,*,#15294,.T.);
#21132=ORIENTED_EDGE('',*,*,#15003,.T.);
#21133=ORIENTED_EDGE('',*,*,#15293,.T.);
#21134=ORIENTED_EDGE('',*,*,#15230,.T.);
#21135=ORIENTED_EDGE('',*,*,#15292,.T.);
#21136=ORIENTED_EDGE('',*,*,#14994,.T.);
#21137=ORIENTED_EDGE('',*,*,#15291,.T.);
#21138=ORIENTED_EDGE('',*,*,#15239,.T.);
#21139=ORIENTED_EDGE('',*,*,#15290,.T.);
#21140=ORIENTED_EDGE('',*,*,#14985,.T.);
#21141=ORIENTED_EDGE('',*,*,#15289,.T.);
#21142=ORIENTED_EDGE('',*,*,#15248,.T.);
#21143=ORIENTED_EDGE('',*,*,#15288,.T.);
#21144=ORIENTED_EDGE('',*,*,#14976,.T.);
#21145=ORIENTED_EDGE('',*,*,#15287,.T.);
#21146=ORIENTED_EDGE('',*,*,#15257,.T.);
#21147=ORIENTED_EDGE('',*,*,#15286,.T.);
#21148=ORIENTED_EDGE('',*,*,#14967,.T.);
#21149=ORIENTED_EDGE('',*,*,#15285,.T.);
#21150=ORIENTED_EDGE('',*,*,#15266,.T.);
#21151=ORIENTED_EDGE('',*,*,#15284,.T.);
#21152=ORIENTED_EDGE('',*,*,#14958,.T.);
#21153=ORIENTED_EDGE('',*,*,#15320,.T.);
#21154=ORIENTED_EDGE('',*,*,#15275,.T.);
#21155=ORIENTED_EDGE('',*,*,#15319,.T.);
#21156=ORIENTED_EDGE('',*,*,#15190,.T.);
#21157=ORIENTED_EDGE('',*,*,#15318,.T.);
#21158=ORIENTED_EDGE('',*,*,#15113,.T.);
#21159=ORIENTED_EDGE('',*,*,#15317,.T.);
#21160=ORIENTED_EDGE('',*,*,#15122,.T.);
#21161=ORIENTED_EDGE('',*,*,#15316,.T.);
#21162=ORIENTED_EDGE('',*,*,#15104,.T.);
#21163=ORIENTED_EDGE('',*,*,#15315,.T.);
#21164=ORIENTED_EDGE('',*,*,#15131,.T.);
#21165=ORIENTED_EDGE('',*,*,#15314,.T.);
#21166=ORIENTED_EDGE('',*,*,#15095,.T.);
#21167=ORIENTED_EDGE('',*,*,#15313,.T.);
#21168=ORIENTED_EDGE('',*,*,#15140,.T.);
#21169=ORIENTED_EDGE('',*,*,#15312,.T.);
#21170=ORIENTED_EDGE('',*,*,#15086,.T.);
#21171=ORIENTED_EDGE('',*,*,#15311,.T.);
#21172=ORIENTED_EDGE('',*,*,#15149,.T.);
#21173=ORIENTED_EDGE('',*,*,#15310,.T.);
#21174=ORIENTED_EDGE('',*,*,#15077,.T.);
#21175=ORIENTED_EDGE('',*,*,#15309,.T.);
#21176=ORIENTED_EDGE('',*,*,#15158,.T.);
#21177=ORIENTED_EDGE('',*,*,#15308,.T.);
#21178=ORIENTED_EDGE('',*,*,#15068,.T.);
#21179=ORIENTED_EDGE('',*,*,#15307,.T.);
#21180=ORIENTED_EDGE('',*,*,#15167,.T.);
#21181=ORIENTED_EDGE('',*,*,#15306,.T.);
#21182=ORIENTED_EDGE('',*,*,#15059,.T.);
#21183=ORIENTED_EDGE('',*,*,#15305,.T.);
#21184=ORIENTED_EDGE('',*,*,#15176,.T.);
#21185=ORIENTED_EDGE('',*,*,#15304,.T.);
#21186=ORIENTED_EDGE('',*,*,#15050,.T.);
#21187=ORIENTED_EDGE('',*,*,#15303,.T.);
#21188=ORIENTED_EDGE('',*,*,#15185,.T.);
#21189=ORIENTED_EDGE('',*,*,#15302,.T.);
#21190=ORIENTED_EDGE('',*,*,#15041,.T.);
#21191=ORIENTED_EDGE('',*,*,#15301,.T.);
#21192=ORIENTED_EDGE('',*,*,#15030,.T.);
#21193=ORIENTED_EDGE('',*,*,#15322,.F.);
#21194=ORIENTED_EDGE('',*,*,#15321,.T.);
#21195=ORIENTED_EDGE('',*,*,#14942,.T.);
#21196=ORIENTED_EDGE('',*,*,#14953,.T.);
#21197=ORIENTED_EDGE('',*,*,#14951,.T.);
#21198=ORIENTED_EDGE('',*,*,#14949,.T.);
#21199=ORIENTED_EDGE('',*,*,#14947,.T.);
#21200=ORIENTED_EDGE('',*,*,#14945,.T.);
#21201=ORIENTED_EDGE('',*,*,#15323,.T.);
#21202=ORIENTED_EDGE('',*,*,#15324,.T.);
#21203=ORIENTED_EDGE('',*,*,#15325,.T.);
#21204=ORIENTED_EDGE('',*,*,#15326,.T.);
#21205=ORIENTED_EDGE('',*,*,#15327,.T.);
#21206=ORIENTED_EDGE('',*,*,#15328,.T.);
#21207=ORIENTED_EDGE('',*,*,#15323,.F.);
#21208=ORIENTED_EDGE('',*,*,#15329,.T.);
#21209=ORIENTED_EDGE('',*,*,#15330,.T.);
#21210=ORIENTED_EDGE('',*,*,#15331,.T.);
#21211=ORIENTED_EDGE('',*,*,#15327,.F.);
#21212=ORIENTED_EDGE('',*,*,#15332,.T.);
#21213=ORIENTED_EDGE('',*,*,#15325,.F.);
#21214=ORIENTED_EDGE('',*,*,#15333,.T.);
#21215=ORIENTED_EDGE('',*,*,#15330,.F.);
#21216=ORIENTED_EDGE('',*,*,#15334,.T.);
#21217=ORIENTED_EDGE('',*,*,#15333,.F.);
#21218=ORIENTED_EDGE('',*,*,#15335,.T.);
#21219=ORIENTED_EDGE('',*,*,#15336,.F.);
#21220=ORIENTED_EDGE('',*,*,#15337,.F.);
#21221=ORIENTED_EDGE('',*,*,#15324,.F.);
#21222=ORIENTED_EDGE('',*,*,#15338,.T.);
#21223=ORIENTED_EDGE('',*,*,#15339,.F.);
#21224=ORIENTED_EDGE('',*,*,#15335,.F.);
#21225=ORIENTED_EDGE('',*,*,#15326,.F.);
#21226=ORIENTED_EDGE('',*,*,#15334,.F.);
#21227=ORIENTED_EDGE('',*,*,#15332,.F.);
#21228=ORIENTED_EDGE('',*,*,#15329,.F.);
#21229=ORIENTED_EDGE('',*,*,#15340,.T.);
#21230=ORIENTED_EDGE('',*,*,#15341,.T.);
#21231=ORIENTED_EDGE('',*,*,#15342,.T.);
#21232=ORIENTED_EDGE('',*,*,#15339,.T.);
#21233=ORIENTED_EDGE('',*,*,#15343,.T.);
#21234=ORIENTED_EDGE('',*,*,#15344,.T.);
#21235=ORIENTED_EDGE('',*,*,#15340,.F.);
#21236=ORIENTED_EDGE('',*,*,#15345,.T.);
#21237=ORIENTED_EDGE('',*,*,#15346,.T.);
#21238=ORIENTED_EDGE('',*,*,#15347,.T.);
#21239=ORIENTED_EDGE('',*,*,#15343,.F.);
#21240=ORIENTED_EDGE('',*,*,#15348,.T.);
#21241=ORIENTED_EDGE('',*,*,#15342,.F.);
#21242=ORIENTED_EDGE('',*,*,#15349,.T.);
#21243=ORIENTED_EDGE('',*,*,#15346,.F.);
#21244=ORIENTED_EDGE('',*,*,#15336,.T.);
#21245=ORIENTED_EDGE('',*,*,#15328,.F.);
#21246=ORIENTED_EDGE('',*,*,#15350,.T.);
#21247=ORIENTED_EDGE('',*,*,#15345,.F.);
#21248=ORIENTED_EDGE('',*,*,#15338,.F.);
#21249=ORIENTED_EDGE('',*,*,#15341,.F.);
#21250=ORIENTED_EDGE('',*,*,#15344,.F.);
#21251=ORIENTED_EDGE('',*,*,#15347,.F.);
#21252=ORIENTED_EDGE('',*,*,#15349,.F.);
#21253=ORIENTED_EDGE('',*,*,#15331,.F.);
#21254=ORIENTED_EDGE('',*,*,#15337,.T.);
#21255=ORIENTED_EDGE('',*,*,#15348,.F.);
#21256=ORIENTED_EDGE('',*,*,#15350,.F.);
#21257=ORIENTED_EDGE('',*,*,#15351,.F.);
#21258=ORIENTED_EDGE('',*,*,#15352,.T.);
#21259=ORIENTED_EDGE('',*,*,#15353,.T.);
#21260=ORIENTED_EDGE('',*,*,#15354,.T.);
#21261=ORIENTED_EDGE('',*,*,#15355,.F.);
#21262=ORIENTED_EDGE('',*,*,#15356,.T.);
#21263=ORIENTED_EDGE('',*,*,#15351,.T.);
#21264=ORIENTED_EDGE('',*,*,#15357,.T.);
#21265=ORIENTED_EDGE('',*,*,#15358,.F.);
#21266=ORIENTED_EDGE('',*,*,#15359,.T.);
#21267=ORIENTED_EDGE('',*,*,#15355,.T.);
#21268=ORIENTED_EDGE('',*,*,#15360,.T.);
#21269=ORIENTED_EDGE('',*,*,#15361,.F.);
#21270=ORIENTED_EDGE('',*,*,#15362,.T.);
#21271=ORIENTED_EDGE('',*,*,#15358,.T.);
#21272=ORIENTED_EDGE('',*,*,#15363,.T.);
#21273=ORIENTED_EDGE('',*,*,#15364,.F.);
#21274=ORIENTED_EDGE('',*,*,#15365,.T.);
#21275=ORIENTED_EDGE('',*,*,#15361,.T.);
#21276=ORIENTED_EDGE('',*,*,#15366,.T.);
#21277=ORIENTED_EDGE('',*,*,#15367,.F.);
#21278=ORIENTED_EDGE('',*,*,#15368,.T.);
#21279=ORIENTED_EDGE('',*,*,#15364,.T.);
#21280=ORIENTED_EDGE('',*,*,#15369,.T.);
#21281=ORIENTED_EDGE('',*,*,#15370,.F.);
#21282=ORIENTED_EDGE('',*,*,#15371,.T.);
#21283=ORIENTED_EDGE('',*,*,#15367,.T.);
#21284=ORIENTED_EDGE('',*,*,#15372,.T.);
#21285=ORIENTED_EDGE('',*,*,#15373,.F.);
#21286=ORIENTED_EDGE('',*,*,#15374,.T.);
#21287=ORIENTED_EDGE('',*,*,#15370,.T.);
#21288=ORIENTED_EDGE('',*,*,#15375,.T.);
#21289=ORIENTED_EDGE('',*,*,#15376,.F.);
#21290=ORIENTED_EDGE('',*,*,#15377,.T.);
#21291=ORIENTED_EDGE('',*,*,#15373,.T.);
#21292=ORIENTED_EDGE('',*,*,#15378,.T.);
#21293=ORIENTED_EDGE('',*,*,#15379,.F.);
#21294=ORIENTED_EDGE('',*,*,#15380,.T.);
#21295=ORIENTED_EDGE('',*,*,#15376,.T.);
#21296=ORIENTED_EDGE('',*,*,#15381,.T.);
#21297=ORIENTED_EDGE('',*,*,#15382,.F.);
#21298=ORIENTED_EDGE('',*,*,#15383,.T.);
#21299=ORIENTED_EDGE('',*,*,#15384,.F.);
#21300=ORIENTED_EDGE('',*,*,#15385,.F.);
#21301=ORIENTED_EDGE('',*,*,#15386,.F.);
#21302=ORIENTED_EDGE('',*,*,#15387,.T.);
#21303=ORIENTED_EDGE('',*,*,#15382,.T.);
#21304=ORIENTED_EDGE('',*,*,#15388,.F.);
#21305=ORIENTED_EDGE('',*,*,#15389,.F.);
#21306=ORIENTED_EDGE('',*,*,#15390,.T.);
#21307=ORIENTED_EDGE('',*,*,#15386,.T.);
#21308=ORIENTED_EDGE('',*,*,#15391,.F.);
#21309=ORIENTED_EDGE('',*,*,#15392,.F.);
#21310=ORIENTED_EDGE('',*,*,#15393,.T.);
#21311=ORIENTED_EDGE('',*,*,#15389,.T.);
#21312=ORIENTED_EDGE('',*,*,#15394,.F.);
#21313=ORIENTED_EDGE('',*,*,#15395,.F.);
#21314=ORIENTED_EDGE('',*,*,#15396,.T.);
#21315=ORIENTED_EDGE('',*,*,#15392,.T.);
#21316=ORIENTED_EDGE('',*,*,#15397,.F.);
#21317=ORIENTED_EDGE('',*,*,#15398,.F.);
#21318=ORIENTED_EDGE('',*,*,#15399,.T.);
#21319=ORIENTED_EDGE('',*,*,#15395,.T.);
#21320=ORIENTED_EDGE('',*,*,#15400,.F.);
#21321=ORIENTED_EDGE('',*,*,#15401,.F.);
#21322=ORIENTED_EDGE('',*,*,#15402,.T.);
#21323=ORIENTED_EDGE('',*,*,#15398,.T.);
#21324=ORIENTED_EDGE('',*,*,#15403,.F.);
#21325=ORIENTED_EDGE('',*,*,#15404,.F.);
#21326=ORIENTED_EDGE('',*,*,#15405,.T.);
#21327=ORIENTED_EDGE('',*,*,#15401,.T.);
#21328=ORIENTED_EDGE('',*,*,#15406,.F.);
#21329=ORIENTED_EDGE('',*,*,#15407,.F.);
#21330=ORIENTED_EDGE('',*,*,#15408,.T.);
#21331=ORIENTED_EDGE('',*,*,#15404,.T.);
#21332=ORIENTED_EDGE('',*,*,#15409,.F.);
#21333=ORIENTED_EDGE('',*,*,#15410,.T.);
#21334=ORIENTED_EDGE('',*,*,#15411,.T.);
#21335=ORIENTED_EDGE('',*,*,#15412,.T.);
#21336=ORIENTED_EDGE('',*,*,#15413,.T.);
#21337=ORIENTED_EDGE('',*,*,#15411,.F.);
#21338=ORIENTED_EDGE('',*,*,#15414,.T.);
#21339=ORIENTED_EDGE('',*,*,#15415,.T.);
#21340=ORIENTED_EDGE('',*,*,#15416,.T.);
#21341=ORIENTED_EDGE('',*,*,#15417,.T.);
#21342=ORIENTED_EDGE('',*,*,#15418,.F.);
#21343=ORIENTED_EDGE('',*,*,#15419,.F.);
#21344=ORIENTED_EDGE('',*,*,#15381,.F.);
#21345=ORIENTED_EDGE('',*,*,#15378,.F.);
#21346=ORIENTED_EDGE('',*,*,#15375,.F.);
#21347=ORIENTED_EDGE('',*,*,#15372,.F.);
#21348=ORIENTED_EDGE('',*,*,#15369,.F.);
#21349=ORIENTED_EDGE('',*,*,#15366,.F.);
#21350=ORIENTED_EDGE('',*,*,#15363,.F.);
#21351=ORIENTED_EDGE('',*,*,#15360,.F.);
#21352=ORIENTED_EDGE('',*,*,#15357,.F.);
#21353=ORIENTED_EDGE('',*,*,#15354,.F.);
#21354=ORIENTED_EDGE('',*,*,#15420,.F.);
#21355=ORIENTED_EDGE('',*,*,#15421,.T.);
#21356=ORIENTED_EDGE('',*,*,#15409,.T.);
#21357=ORIENTED_EDGE('',*,*,#15406,.T.);
#21358=ORIENTED_EDGE('',*,*,#15403,.T.);
#21359=ORIENTED_EDGE('',*,*,#15400,.T.);
#21360=ORIENTED_EDGE('',*,*,#15397,.T.);
#21361=ORIENTED_EDGE('',*,*,#15394,.T.);
#21362=ORIENTED_EDGE('',*,*,#15391,.T.);
#21363=ORIENTED_EDGE('',*,*,#15388,.T.);
#21364=ORIENTED_EDGE('',*,*,#15385,.T.);
#21365=ORIENTED_EDGE('',*,*,#15422,.T.);
#21366=ORIENTED_EDGE('',*,*,#15423,.T.);
#21367=ORIENTED_EDGE('',*,*,#15424,.T.);
#21368=ORIENTED_EDGE('',*,*,#15425,.T.);
#21369=ORIENTED_EDGE('',*,*,#15420,.T.);
#21370=ORIENTED_EDGE('',*,*,#15407,.T.);
#21371=ORIENTED_EDGE('',*,*,#15421,.F.);
#21372=ORIENTED_EDGE('',*,*,#15425,.F.);
#21373=ORIENTED_EDGE('',*,*,#15426,.T.);
#21374=ORIENTED_EDGE('',*,*,#15427,.F.);
#21375=ORIENTED_EDGE('',*,*,#15383,.F.);
#21376=ORIENTED_EDGE('',*,*,#15387,.F.);
#21377=ORIENTED_EDGE('',*,*,#15390,.F.);
#21378=ORIENTED_EDGE('',*,*,#15393,.F.);
#21379=ORIENTED_EDGE('',*,*,#15396,.F.);
#21380=ORIENTED_EDGE('',*,*,#15399,.F.);
#21381=ORIENTED_EDGE('',*,*,#15402,.F.);
#21382=ORIENTED_EDGE('',*,*,#15405,.F.);
#21383=ORIENTED_EDGE('',*,*,#15408,.F.);
#21384=ORIENTED_EDGE('',*,*,#15426,.F.);
#21385=ORIENTED_EDGE('',*,*,#15424,.F.);
#21386=ORIENTED_EDGE('',*,*,#15352,.F.);
#21387=ORIENTED_EDGE('',*,*,#15356,.F.);
#21388=ORIENTED_EDGE('',*,*,#15359,.F.);
#21389=ORIENTED_EDGE('',*,*,#15362,.F.);
#21390=ORIENTED_EDGE('',*,*,#15365,.F.);
#21391=ORIENTED_EDGE('',*,*,#15368,.F.);
#21392=ORIENTED_EDGE('',*,*,#15371,.F.);
#21393=ORIENTED_EDGE('',*,*,#15374,.F.);
#21394=ORIENTED_EDGE('',*,*,#15377,.F.);
#21395=ORIENTED_EDGE('',*,*,#15380,.F.);
#21396=ORIENTED_EDGE('',*,*,#15428,.F.);
#21397=ORIENTED_EDGE('',*,*,#15417,.F.);
#21398=ORIENTED_EDGE('',*,*,#15429,.F.);
#21399=ORIENTED_EDGE('',*,*,#15430,.T.);
#21400=ORIENTED_EDGE('',*,*,#15431,.T.);
#21401=ORIENTED_EDGE('',*,*,#15432,.T.);
#21402=ORIENTED_EDGE('',*,*,#15433,.T.);
#21403=ORIENTED_EDGE('',*,*,#15430,.F.);
#21404=ORIENTED_EDGE('',*,*,#15434,.F.);
#21405=ORIENTED_EDGE('',*,*,#15414,.F.);
#21406=ORIENTED_EDGE('',*,*,#15410,.F.);
#21407=ORIENTED_EDGE('',*,*,#15435,.F.);
#21408=ORIENTED_EDGE('',*,*,#15436,.F.);
#21409=ORIENTED_EDGE('',*,*,#15437,.F.);
#21410=ORIENTED_EDGE('',*,*,#15412,.F.);
#21411=ORIENTED_EDGE('',*,*,#15432,.F.);
#21412=ORIENTED_EDGE('',*,*,#15438,.T.);
#21413=ORIENTED_EDGE('',*,*,#15438,.F.);
#21414=ORIENTED_EDGE('',*,*,#15431,.F.);
#21415=ORIENTED_EDGE('',*,*,#15433,.F.);
#21416=ORIENTED_EDGE('',*,*,#15439,.F.);
#21417=ORIENTED_EDGE('',*,*,#15439,.T.);
#21418=ORIENTED_EDGE('',*,*,#15440,.F.);
#21419=ORIENTED_EDGE('',*,*,#15436,.T.);
#21420=ORIENTED_EDGE('',*,*,#15413,.F.);
#21421=ORIENTED_EDGE('',*,*,#15437,.T.);
#21422=ORIENTED_EDGE('',*,*,#15440,.T.);
#21423=ORIENTED_EDGE('',*,*,#15435,.T.);
#21424=ORIENTED_EDGE('',*,*,#15441,.F.);
#21425=ORIENTED_EDGE('',*,*,#15422,.F.);
#21426=ORIENTED_EDGE('',*,*,#15353,.F.);
#21427=ORIENTED_EDGE('',*,*,#15423,.F.);
#21428=ORIENTED_EDGE('',*,*,#15442,.T.);
#21429=ORIENTED_EDGE('',*,*,#15441,.T.);
#21430=ORIENTED_EDGE('',*,*,#15442,.F.);
#21431=ORIENTED_EDGE('',*,*,#15379,.T.);
#21432=ORIENTED_EDGE('',*,*,#15419,.T.);
#21433=ORIENTED_EDGE('',*,*,#15443,.F.);
#21434=ORIENTED_EDGE('',*,*,#15428,.T.);
#21435=ORIENTED_EDGE('',*,*,#15444,.F.);
#21436=ORIENTED_EDGE('',*,*,#15443,.T.);
#21437=ORIENTED_EDGE('',*,*,#15418,.T.);
#21438=ORIENTED_EDGE('',*,*,#15384,.T.);
#21439=ORIENTED_EDGE('',*,*,#15427,.T.);
#21440=ORIENTED_EDGE('',*,*,#15434,.T.);
#21441=ORIENTED_EDGE('',*,*,#15429,.T.);
#21442=ORIENTED_EDGE('',*,*,#15416,.F.);
#21443=ORIENTED_EDGE('',*,*,#15445,.T.);
#21444=ORIENTED_EDGE('',*,*,#15444,.T.);
#21445=ORIENTED_EDGE('',*,*,#15445,.F.);
#21446=ORIENTED_EDGE('',*,*,#15415,.F.);
#21447=ORIENTED_EDGE('',*,*,#15446,.F.);
#21448=ORIENTED_EDGE('',*,*,#15447,.F.);
#21449=ORIENTED_EDGE('',*,*,#15448,.F.);
#21450=ORIENTED_EDGE('',*,*,#15449,.T.);
#21451=ORIENTED_EDGE('',*,*,#15447,.T.);
#21452=ORIENTED_EDGE('',*,*,#15446,.T.);
#21453=ORIENTED_EDGE('',*,*,#15449,.F.);
#21454=ORIENTED_EDGE('',*,*,#15450,.F.);
#21455=ORIENTED_EDGE('',*,*,#15451,.T.);
#21456=ORIENTED_EDGE('',*,*,#15448,.T.);
#21457=ORIENTED_EDGE('',*,*,#15451,.F.);
#21458=ORIENTED_EDGE('',*,*,#15450,.T.);
#21459=ORIENTED_EDGE('',*,*,#15452,.F.);
#21460=ORIENTED_EDGE('',*,*,#15453,.T.);
#21461=ORIENTED_EDGE('',*,*,#15454,.T.);
#21462=ORIENTED_EDGE('',*,*,#15455,.T.);
#21463=ORIENTED_EDGE('',*,*,#15456,.F.);
#21464=ORIENTED_EDGE('',*,*,#15457,.T.);
#21465=ORIENTED_EDGE('',*,*,#15452,.T.);
#21466=ORIENTED_EDGE('',*,*,#15458,.T.);
#21467=ORIENTED_EDGE('',*,*,#15459,.F.);
#21468=ORIENTED_EDGE('',*,*,#15460,.T.);
#21469=ORIENTED_EDGE('',*,*,#15456,.T.);
#21470=ORIENTED_EDGE('',*,*,#15461,.T.);
#21471=ORIENTED_EDGE('',*,*,#15462,.F.);
#21472=ORIENTED_EDGE('',*,*,#15463,.T.);
#21473=ORIENTED_EDGE('',*,*,#15459,.T.);
#21474=ORIENTED_EDGE('',*,*,#15464,.T.);
#21475=ORIENTED_EDGE('',*,*,#15465,.F.);
#21476=ORIENTED_EDGE('',*,*,#15466,.T.);
#21477=ORIENTED_EDGE('',*,*,#15462,.T.);
#21478=ORIENTED_EDGE('',*,*,#15467,.T.);
#21479=ORIENTED_EDGE('',*,*,#15468,.F.);
#21480=ORIENTED_EDGE('',*,*,#15469,.T.);
#21481=ORIENTED_EDGE('',*,*,#15465,.T.);
#21482=ORIENTED_EDGE('',*,*,#15470,.T.);
#21483=ORIENTED_EDGE('',*,*,#15471,.F.);
#21484=ORIENTED_EDGE('',*,*,#15472,.T.);
#21485=ORIENTED_EDGE('',*,*,#15468,.T.);
#21486=ORIENTED_EDGE('',*,*,#15473,.T.);
#21487=ORIENTED_EDGE('',*,*,#15474,.F.);
#21488=ORIENTED_EDGE('',*,*,#15475,.T.);
#21489=ORIENTED_EDGE('',*,*,#15471,.T.);
#21490=ORIENTED_EDGE('',*,*,#15476,.T.);
#21491=ORIENTED_EDGE('',*,*,#15477,.F.);
#21492=ORIENTED_EDGE('',*,*,#15478,.T.);
#21493=ORIENTED_EDGE('',*,*,#15474,.T.);
#21494=ORIENTED_EDGE('',*,*,#15479,.T.);
#21495=ORIENTED_EDGE('',*,*,#15480,.F.);
#21496=ORIENTED_EDGE('',*,*,#15481,.T.);
#21497=ORIENTED_EDGE('',*,*,#15477,.T.);
#21498=ORIENTED_EDGE('',*,*,#15482,.T.);
#21499=ORIENTED_EDGE('',*,*,#15483,.F.);
#21500=ORIENTED_EDGE('',*,*,#15484,.T.);
#21501=ORIENTED_EDGE('',*,*,#15480,.T.);
#21502=ORIENTED_EDGE('',*,*,#15485,.T.);
#21503=ORIENTED_EDGE('',*,*,#15486,.F.);
#21504=ORIENTED_EDGE('',*,*,#15487,.T.);
#21505=ORIENTED_EDGE('',*,*,#15483,.T.);
#21506=ORIENTED_EDGE('',*,*,#15488,.T.);
#21507=ORIENTED_EDGE('',*,*,#15489,.F.);
#21508=ORIENTED_EDGE('',*,*,#15490,.T.);
#21509=ORIENTED_EDGE('',*,*,#15486,.T.);
#21510=ORIENTED_EDGE('',*,*,#15491,.T.);
#21511=ORIENTED_EDGE('',*,*,#15492,.F.);
#21512=ORIENTED_EDGE('',*,*,#15493,.T.);
#21513=ORIENTED_EDGE('',*,*,#15489,.T.);
#21514=ORIENTED_EDGE('',*,*,#15494,.T.);
#21515=ORIENTED_EDGE('',*,*,#15495,.F.);
#21516=ORIENTED_EDGE('',*,*,#15496,.T.);
#21517=ORIENTED_EDGE('',*,*,#15497,.F.);
#21518=ORIENTED_EDGE('',*,*,#15498,.F.);
#21519=ORIENTED_EDGE('',*,*,#15499,.F.);
#21520=ORIENTED_EDGE('',*,*,#15500,.T.);
#21521=ORIENTED_EDGE('',*,*,#15495,.T.);
#21522=ORIENTED_EDGE('',*,*,#15501,.F.);
#21523=ORIENTED_EDGE('',*,*,#15502,.F.);
#21524=ORIENTED_EDGE('',*,*,#15503,.T.);
#21525=ORIENTED_EDGE('',*,*,#15499,.T.);
#21526=ORIENTED_EDGE('',*,*,#15504,.F.);
#21527=ORIENTED_EDGE('',*,*,#15505,.F.);
#21528=ORIENTED_EDGE('',*,*,#15506,.T.);
#21529=ORIENTED_EDGE('',*,*,#15502,.T.);
#21530=ORIENTED_EDGE('',*,*,#15507,.F.);
#21531=ORIENTED_EDGE('',*,*,#15508,.F.);
#21532=ORIENTED_EDGE('',*,*,#15509,.T.);
#21533=ORIENTED_EDGE('',*,*,#15505,.T.);
#21534=ORIENTED_EDGE('',*,*,#15510,.F.);
#21535=ORIENTED_EDGE('',*,*,#15511,.F.);
#21536=ORIENTED_EDGE('',*,*,#15512,.T.);
#21537=ORIENTED_EDGE('',*,*,#15508,.T.);
#21538=ORIENTED_EDGE('',*,*,#15513,.F.);
#21539=ORIENTED_EDGE('',*,*,#15514,.F.);
#21540=ORIENTED_EDGE('',*,*,#15515,.T.);
#21541=ORIENTED_EDGE('',*,*,#15511,.T.);
#21542=ORIENTED_EDGE('',*,*,#15516,.F.);
#21543=ORIENTED_EDGE('',*,*,#15517,.F.);
#21544=ORIENTED_EDGE('',*,*,#15518,.T.);
#21545=ORIENTED_EDGE('',*,*,#15514,.T.);
#21546=ORIENTED_EDGE('',*,*,#15519,.F.);
#21547=ORIENTED_EDGE('',*,*,#15520,.F.);
#21548=ORIENTED_EDGE('',*,*,#15521,.T.);
#21549=ORIENTED_EDGE('',*,*,#15517,.T.);
#21550=ORIENTED_EDGE('',*,*,#15522,.F.);
#21551=ORIENTED_EDGE('',*,*,#15523,.F.);
#21552=ORIENTED_EDGE('',*,*,#15524,.T.);
#21553=ORIENTED_EDGE('',*,*,#15520,.T.);
#21554=ORIENTED_EDGE('',*,*,#15525,.F.);
#21555=ORIENTED_EDGE('',*,*,#15526,.F.);
#21556=ORIENTED_EDGE('',*,*,#15527,.T.);
#21557=ORIENTED_EDGE('',*,*,#15523,.T.);
#21558=ORIENTED_EDGE('',*,*,#15528,.F.);
#21559=ORIENTED_EDGE('',*,*,#15529,.F.);
#21560=ORIENTED_EDGE('',*,*,#15530,.T.);
#21561=ORIENTED_EDGE('',*,*,#15526,.T.);
#21562=ORIENTED_EDGE('',*,*,#15531,.F.);
#21563=ORIENTED_EDGE('',*,*,#15532,.F.);
#21564=ORIENTED_EDGE('',*,*,#15533,.T.);
#21565=ORIENTED_EDGE('',*,*,#15529,.T.);
#21566=ORIENTED_EDGE('',*,*,#15534,.F.);
#21567=ORIENTED_EDGE('',*,*,#15535,.F.);
#21568=ORIENTED_EDGE('',*,*,#15536,.T.);
#21569=ORIENTED_EDGE('',*,*,#15532,.T.);
#21570=ORIENTED_EDGE('',*,*,#15537,.F.);
#21571=ORIENTED_EDGE('',*,*,#15538,.F.);
#21572=ORIENTED_EDGE('',*,*,#15539,.F.);
#21573=ORIENTED_EDGE('',*,*,#15494,.F.);
#21574=ORIENTED_EDGE('',*,*,#15491,.F.);
#21575=ORIENTED_EDGE('',*,*,#15488,.F.);
#21576=ORIENTED_EDGE('',*,*,#15485,.F.);
#21577=ORIENTED_EDGE('',*,*,#15482,.F.);
#21578=ORIENTED_EDGE('',*,*,#15479,.F.);
#21579=ORIENTED_EDGE('',*,*,#15476,.F.);
#21580=ORIENTED_EDGE('',*,*,#15473,.F.);
#21581=ORIENTED_EDGE('',*,*,#15470,.F.);
#21582=ORIENTED_EDGE('',*,*,#15467,.F.);
#21583=ORIENTED_EDGE('',*,*,#15464,.F.);
#21584=ORIENTED_EDGE('',*,*,#15461,.F.);
#21585=ORIENTED_EDGE('',*,*,#15458,.F.);
#21586=ORIENTED_EDGE('',*,*,#15455,.F.);
#21587=ORIENTED_EDGE('',*,*,#15540,.F.);
#21588=ORIENTED_EDGE('',*,*,#15541,.T.);
#21589=ORIENTED_EDGE('',*,*,#15537,.T.);
#21590=ORIENTED_EDGE('',*,*,#15534,.T.);
#21591=ORIENTED_EDGE('',*,*,#15531,.T.);
#21592=ORIENTED_EDGE('',*,*,#15528,.T.);
#21593=ORIENTED_EDGE('',*,*,#15525,.T.);
#21594=ORIENTED_EDGE('',*,*,#15522,.T.);
#21595=ORIENTED_EDGE('',*,*,#15519,.T.);
#21596=ORIENTED_EDGE('',*,*,#15516,.T.);
#21597=ORIENTED_EDGE('',*,*,#15513,.T.);
#21598=ORIENTED_EDGE('',*,*,#15510,.T.);
#21599=ORIENTED_EDGE('',*,*,#15507,.T.);
#21600=ORIENTED_EDGE('',*,*,#15504,.T.);
#21601=ORIENTED_EDGE('',*,*,#15501,.T.);
#21602=ORIENTED_EDGE('',*,*,#15498,.T.);
#21603=ORIENTED_EDGE('',*,*,#15542,.T.);
#21604=ORIENTED_EDGE('',*,*,#15543,.T.);
#21605=ORIENTED_EDGE('',*,*,#15544,.T.);
#21606=ORIENTED_EDGE('',*,*,#15545,.T.);
#21607=ORIENTED_EDGE('',*,*,#15540,.T.);
#21608=ORIENTED_EDGE('',*,*,#15535,.T.);
#21609=ORIENTED_EDGE('',*,*,#15541,.F.);
#21610=ORIENTED_EDGE('',*,*,#15545,.F.);
#21611=ORIENTED_EDGE('',*,*,#15546,.T.);
#21612=ORIENTED_EDGE('',*,*,#15547,.F.);
#21613=ORIENTED_EDGE('',*,*,#15496,.F.);
#21614=ORIENTED_EDGE('',*,*,#15500,.F.);
#21615=ORIENTED_EDGE('',*,*,#15503,.F.);
#21616=ORIENTED_EDGE('',*,*,#15506,.F.);
#21617=ORIENTED_EDGE('',*,*,#15509,.F.);
#21618=ORIENTED_EDGE('',*,*,#15512,.F.);
#21619=ORIENTED_EDGE('',*,*,#15515,.F.);
#21620=ORIENTED_EDGE('',*,*,#15518,.F.);
#21621=ORIENTED_EDGE('',*,*,#15521,.F.);
#21622=ORIENTED_EDGE('',*,*,#15524,.F.);
#21623=ORIENTED_EDGE('',*,*,#15527,.F.);
#21624=ORIENTED_EDGE('',*,*,#15530,.F.);
#21625=ORIENTED_EDGE('',*,*,#15533,.F.);
#21626=ORIENTED_EDGE('',*,*,#15536,.F.);
#21627=ORIENTED_EDGE('',*,*,#15546,.F.);
#21628=ORIENTED_EDGE('',*,*,#15544,.F.);
#21629=ORIENTED_EDGE('',*,*,#15453,.F.);
#21630=ORIENTED_EDGE('',*,*,#15457,.F.);
#21631=ORIENTED_EDGE('',*,*,#15460,.F.);
#21632=ORIENTED_EDGE('',*,*,#15463,.F.);
#21633=ORIENTED_EDGE('',*,*,#15466,.F.);
#21634=ORIENTED_EDGE('',*,*,#15469,.F.);
#21635=ORIENTED_EDGE('',*,*,#15472,.F.);
#21636=ORIENTED_EDGE('',*,*,#15475,.F.);
#21637=ORIENTED_EDGE('',*,*,#15478,.F.);
#21638=ORIENTED_EDGE('',*,*,#15481,.F.);
#21639=ORIENTED_EDGE('',*,*,#15484,.F.);
#21640=ORIENTED_EDGE('',*,*,#15487,.F.);
#21641=ORIENTED_EDGE('',*,*,#15490,.F.);
#21642=ORIENTED_EDGE('',*,*,#15493,.F.);
#21643=ORIENTED_EDGE('',*,*,#15548,.F.);
#21644=ORIENTED_EDGE('',*,*,#15538,.T.);
#21645=ORIENTED_EDGE('',*,*,#15497,.T.);
#21646=ORIENTED_EDGE('',*,*,#15547,.T.);
#21647=ORIENTED_EDGE('',*,*,#15549,.T.);
#21648=ORIENTED_EDGE('',*,*,#15550,.F.);
#21649=ORIENTED_EDGE('',*,*,#15551,.F.);
#21650=ORIENTED_EDGE('',*,*,#15552,.T.);
#21651=ORIENTED_EDGE('',*,*,#15553,.T.);
#21652=ORIENTED_EDGE('',*,*,#15554,.F.);
#21653=ORIENTED_EDGE('',*,*,#15555,.F.);
#21654=ORIENTED_EDGE('',*,*,#15556,.T.);
#21655=ORIENTED_EDGE('',*,*,#15557,.T.);
#21656=ORIENTED_EDGE('',*,*,#15552,.F.);
#21657=ORIENTED_EDGE('',*,*,#15558,.F.);
#21658=ORIENTED_EDGE('',*,*,#15559,.T.);
#21659=ORIENTED_EDGE('',*,*,#15560,.T.);
#21660=ORIENTED_EDGE('',*,*,#15556,.F.);
#21661=ORIENTED_EDGE('',*,*,#15561,.F.);
#21662=ORIENTED_EDGE('',*,*,#15562,.T.);
#21663=ORIENTED_EDGE('',*,*,#15563,.T.);
#21664=ORIENTED_EDGE('',*,*,#15559,.F.);
#21665=ORIENTED_EDGE('',*,*,#15564,.F.);
#21666=ORIENTED_EDGE('',*,*,#15565,.T.);
#21667=ORIENTED_EDGE('',*,*,#15566,.T.);
#21668=ORIENTED_EDGE('',*,*,#15562,.F.);
#21669=ORIENTED_EDGE('',*,*,#15567,.F.);
#21670=ORIENTED_EDGE('',*,*,#15554,.T.);
#21671=ORIENTED_EDGE('',*,*,#15568,.T.);
#21672=ORIENTED_EDGE('',*,*,#15565,.F.);
#21673=ORIENTED_EDGE('',*,*,#15568,.F.);
#21674=ORIENTED_EDGE('',*,*,#15553,.F.);
#21675=ORIENTED_EDGE('',*,*,#15557,.F.);
#21676=ORIENTED_EDGE('',*,*,#15560,.F.);
#21677=ORIENTED_EDGE('',*,*,#15563,.F.);
#21678=ORIENTED_EDGE('',*,*,#15566,.F.);
#21679=ORIENTED_EDGE('',*,*,#15569,.F.);
#21680=ORIENTED_EDGE('',*,*,#15551,.T.);
#21681=ORIENTED_EDGE('',*,*,#15567,.T.);
#21682=ORIENTED_EDGE('',*,*,#15564,.T.);
#21683=ORIENTED_EDGE('',*,*,#15561,.T.);
#21684=ORIENTED_EDGE('',*,*,#15558,.T.);
#21685=ORIENTED_EDGE('',*,*,#15555,.T.);
#21686=ORIENTED_EDGE('',*,*,#15542,.F.);
#21687=ORIENTED_EDGE('',*,*,#15454,.F.);
#21688=ORIENTED_EDGE('',*,*,#15543,.F.);
#21689=ORIENTED_EDGE('',*,*,#15570,.T.);
#21690=ORIENTED_EDGE('',*,*,#15569,.T.);
#21691=ORIENTED_EDGE('',*,*,#15570,.F.);
#21692=ORIENTED_EDGE('',*,*,#15492,.T.);
#21693=ORIENTED_EDGE('',*,*,#15539,.T.);
#21694=ORIENTED_EDGE('',*,*,#15549,.F.);
#21695=ORIENTED_EDGE('',*,*,#15548,.T.);
#21696=ORIENTED_EDGE('',*,*,#15571,.F.);
#21697=ORIENTED_EDGE('',*,*,#15572,.T.);
#21698=ORIENTED_EDGE('',*,*,#15550,.T.);
#21699=ORIENTED_EDGE('',*,*,#15572,.F.);
#21700=ORIENTED_EDGE('',*,*,#15573,.F.);
#21701=ORIENTED_EDGE('',*,*,#15574,.T.);
#21702=ORIENTED_EDGE('',*,*,#15571,.T.);
#21703=ORIENTED_EDGE('',*,*,#15574,.F.);
#21704=ORIENTED_EDGE('',*,*,#15573,.T.);
#21705=ORIENTED_EDGE('',*,*,#15575,.T.);
#21706=ORIENTED_EDGE('',*,*,#15576,.T.);
#21707=ORIENTED_EDGE('',*,*,#15577,.T.);
#21708=ORIENTED_EDGE('',*,*,#15578,.T.);
#21709=ORIENTED_EDGE('',*,*,#15579,.T.);
#21710=ORIENTED_EDGE('',*,*,#15580,.T.);
#21711=ORIENTED_EDGE('',*,*,#15576,.F.);
#21712=ORIENTED_EDGE('',*,*,#15581,.F.);
#21713=ORIENTED_EDGE('',*,*,#15582,.F.);
#21714=ORIENTED_EDGE('',*,*,#15583,.F.);
#21715=ORIENTED_EDGE('',*,*,#15575,.F.);
#21716=ORIENTED_EDGE('',*,*,#15584,.F.);
#21717=ORIENTED_EDGE('',*,*,#15585,.T.);
#21718=ORIENTED_EDGE('',*,*,#15586,.T.);
#21719=ORIENTED_EDGE('',*,*,#15587,.F.);
#21720=ORIENTED_EDGE('',*,*,#15581,.T.);
#21721=ORIENTED_EDGE('',*,*,#15580,.F.);
#21722=ORIENTED_EDGE('',*,*,#15588,.T.);
#21723=ORIENTED_EDGE('',*,*,#15589,.F.);
#21724=ORIENTED_EDGE('',*,*,#15590,.F.);
#21725=ORIENTED_EDGE('',*,*,#15591,.T.);
#21726=ORIENTED_EDGE('',*,*,#15584,.T.);
#21727=ORIENTED_EDGE('',*,*,#15592,.T.);
#21728=ORIENTED_EDGE('',*,*,#15593,.T.);
#21729=ORIENTED_EDGE('',*,*,#15594,.T.);
#21730=ORIENTED_EDGE('',*,*,#15595,.T.);
#21731=ORIENTED_EDGE('',*,*,#15582,.T.);
#21732=ORIENTED_EDGE('',*,*,#15587,.T.);
#21733=ORIENTED_EDGE('',*,*,#15594,.F.);
#21734=ORIENTED_EDGE('',*,*,#15596,.T.);
#21735=ORIENTED_EDGE('',*,*,#15597,.F.);
#21736=ORIENTED_EDGE('',*,*,#15598,.F.);
#21737=ORIENTED_EDGE('',*,*,#15599,.T.);
#21738=ORIENTED_EDGE('',*,*,#15600,.T.);
#21739=ORIENTED_EDGE('',*,*,#15593,.F.);
#21740=ORIENTED_EDGE('',*,*,#15601,.F.);
#21741=ORIENTED_EDGE('',*,*,#15602,.F.);
#21742=ORIENTED_EDGE('',*,*,#15596,.F.);
#21743=ORIENTED_EDGE('',*,*,#15592,.F.);
#21744=ORIENTED_EDGE('',*,*,#15586,.F.);
#21745=ORIENTED_EDGE('',*,*,#15603,.T.);
#21746=ORIENTED_EDGE('',*,*,#15604,.T.);
#21747=ORIENTED_EDGE('',*,*,#15605,.F.);
#21748=ORIENTED_EDGE('',*,*,#15601,.T.);
#21749=ORIENTED_EDGE('',*,*,#15589,.T.);
#21750=ORIENTED_EDGE('',*,*,#15606,.T.);
#21751=ORIENTED_EDGE('',*,*,#15607,.T.);
#21752=ORIENTED_EDGE('',*,*,#15608,.T.);
#21753=ORIENTED_EDGE('',*,*,#15609,.T.);
#21754=ORIENTED_EDGE('',*,*,#15610,.T.);
#21755=ORIENTED_EDGE('',*,*,#15609,.F.);
#21756=ORIENTED_EDGE('',*,*,#15611,.F.);
#21757=ORIENTED_EDGE('',*,*,#15612,.F.);
#21758=ORIENTED_EDGE('',*,*,#15613,.F.);
#21759=ORIENTED_EDGE('',*,*,#15608,.F.);
#21760=ORIENTED_EDGE('',*,*,#15614,.F.);
#21761=ORIENTED_EDGE('',*,*,#15615,.T.);
#21762=ORIENTED_EDGE('',*,*,#15598,.T.);
#21763=ORIENTED_EDGE('',*,*,#15616,.F.);
#21764=ORIENTED_EDGE('',*,*,#15611,.T.);
#21765=ORIENTED_EDGE('',*,*,#15578,.F.);
#21766=ORIENTED_EDGE('',*,*,#15617,.T.);
#21767=ORIENTED_EDGE('',*,*,#15618,.T.);
#21768=ORIENTED_EDGE('',*,*,#15614,.T.);
#21769=ORIENTED_EDGE('',*,*,#15607,.F.);
#21770=ORIENTED_EDGE('',*,*,#15619,.T.);
#21771=ORIENTED_EDGE('',*,*,#15620,.T.);
#21772=ORIENTED_EDGE('',*,*,#15612,.T.);
#21773=ORIENTED_EDGE('',*,*,#15616,.T.);
#21774=ORIENTED_EDGE('',*,*,#15597,.T.);
#21775=ORIENTED_EDGE('',*,*,#15602,.T.);
#21776=ORIENTED_EDGE('',*,*,#15605,.T.);
#21777=ORIENTED_EDGE('',*,*,#15577,.F.);
#21778=ORIENTED_EDGE('',*,*,#15583,.T.);
#21779=ORIENTED_EDGE('',*,*,#15595,.F.);
#21780=ORIENTED_EDGE('',*,*,#15600,.F.);
#21781=ORIENTED_EDGE('',*,*,#15621,.T.);
#21782=ORIENTED_EDGE('',*,*,#15617,.F.);
#21783=ORIENTED_EDGE('',*,*,#15599,.F.);
#21784=ORIENTED_EDGE('',*,*,#15615,.F.);
#21785=ORIENTED_EDGE('',*,*,#15618,.F.);
#21786=ORIENTED_EDGE('',*,*,#15621,.F.);
#21787=ORIENTED_EDGE('',*,*,#15610,.F.);
#21788=ORIENTED_EDGE('',*,*,#15613,.T.);
#21789=ORIENTED_EDGE('',*,*,#15620,.F.);
#21790=ORIENTED_EDGE('',*,*,#15604,.F.);
#21791=ORIENTED_EDGE('',*,*,#15622,.T.);
#21792=ORIENTED_EDGE('',*,*,#15590,.T.);
#21793=ORIENTED_EDGE('',*,*,#15622,.F.);
#21794=ORIENTED_EDGE('',*,*,#15603,.F.);
#21795=ORIENTED_EDGE('',*,*,#15585,.F.);
#21796=ORIENTED_EDGE('',*,*,#15591,.F.);
#21797=ORIENTED_EDGE('',*,*,#15579,.F.);
#21798=ORIENTED_EDGE('',*,*,#15619,.F.);
#21799=ORIENTED_EDGE('',*,*,#15606,.F.);
#21800=ORIENTED_EDGE('',*,*,#15588,.F.);
#21801=ORIENTED_EDGE('',*,*,#15623,.F.);
#21802=ORIENTED_EDGE('',*,*,#15624,.T.);
#21803=ORIENTED_EDGE('',*,*,#15625,.T.);
#21804=ORIENTED_EDGE('',*,*,#15626,.T.);
#21805=ORIENTED_EDGE('',*,*,#15627,.F.);
#21806=ORIENTED_EDGE('',*,*,#15628,.T.);
#21807=ORIENTED_EDGE('',*,*,#15623,.T.);
#21808=ORIENTED_EDGE('',*,*,#15629,.T.);
#21809=ORIENTED_EDGE('',*,*,#15630,.F.);
#21810=ORIENTED_EDGE('',*,*,#15631,.T.);
#21811=ORIENTED_EDGE('',*,*,#15627,.T.);
#21812=ORIENTED_EDGE('',*,*,#15632,.T.);
#21813=ORIENTED_EDGE('',*,*,#15633,.F.);
#21814=ORIENTED_EDGE('',*,*,#15634,.T.);
#21815=ORIENTED_EDGE('',*,*,#15630,.T.);
#21816=ORIENTED_EDGE('',*,*,#15635,.T.);
#21817=ORIENTED_EDGE('',*,*,#15636,.F.);
#21818=ORIENTED_EDGE('',*,*,#15637,.T.);
#21819=ORIENTED_EDGE('',*,*,#15633,.T.);
#21820=ORIENTED_EDGE('',*,*,#15638,.T.);
#21821=ORIENTED_EDGE('',*,*,#15639,.F.);
#21822=ORIENTED_EDGE('',*,*,#15640,.T.);
#21823=ORIENTED_EDGE('',*,*,#15636,.T.);
#21824=ORIENTED_EDGE('',*,*,#15641,.T.);
#21825=ORIENTED_EDGE('',*,*,#15642,.F.);
#21826=ORIENTED_EDGE('',*,*,#15643,.T.);
#21827=ORIENTED_EDGE('',*,*,#15639,.T.);
#21828=ORIENTED_EDGE('',*,*,#15644,.T.);
#21829=ORIENTED_EDGE('',*,*,#15645,.F.);
#21830=ORIENTED_EDGE('',*,*,#15646,.T.);
#21831=ORIENTED_EDGE('',*,*,#15642,.T.);
#21832=ORIENTED_EDGE('',*,*,#15647,.T.);
#21833=ORIENTED_EDGE('',*,*,#15648,.F.);
#21834=ORIENTED_EDGE('',*,*,#15649,.T.);
#21835=ORIENTED_EDGE('',*,*,#15645,.T.);
#21836=ORIENTED_EDGE('',*,*,#15650,.T.);
#21837=ORIENTED_EDGE('',*,*,#15651,.F.);
#21838=ORIENTED_EDGE('',*,*,#15652,.T.);
#21839=ORIENTED_EDGE('',*,*,#15648,.T.);
#21840=ORIENTED_EDGE('',*,*,#15653,.T.);
#21841=ORIENTED_EDGE('',*,*,#15654,.F.);
#21842=ORIENTED_EDGE('',*,*,#15655,.T.);
#21843=ORIENTED_EDGE('',*,*,#15651,.T.);
#21844=ORIENTED_EDGE('',*,*,#15656,.T.);
#21845=ORIENTED_EDGE('',*,*,#15657,.F.);
#21846=ORIENTED_EDGE('',*,*,#15658,.T.);
#21847=ORIENTED_EDGE('',*,*,#15654,.T.);
#21848=ORIENTED_EDGE('',*,*,#15659,.T.);
#21849=ORIENTED_EDGE('',*,*,#15660,.F.);
#21850=ORIENTED_EDGE('',*,*,#15661,.T.);
#21851=ORIENTED_EDGE('',*,*,#15657,.T.);
#21852=ORIENTED_EDGE('',*,*,#15662,.T.);
#21853=ORIENTED_EDGE('',*,*,#15663,.F.);
#21854=ORIENTED_EDGE('',*,*,#15664,.T.);
#21855=ORIENTED_EDGE('',*,*,#15660,.T.);
#21856=ORIENTED_EDGE('',*,*,#15665,.T.);
#21857=ORIENTED_EDGE('',*,*,#15666,.F.);
#21858=ORIENTED_EDGE('',*,*,#15667,.T.);
#21859=ORIENTED_EDGE('',*,*,#15663,.T.);
#21860=ORIENTED_EDGE('',*,*,#15668,.T.);
#21861=ORIENTED_EDGE('',*,*,#15669,.F.);
#21862=ORIENTED_EDGE('',*,*,#15670,.T.);
#21863=ORIENTED_EDGE('',*,*,#15666,.T.);
#21864=ORIENTED_EDGE('',*,*,#15671,.T.);
#21865=ORIENTED_EDGE('',*,*,#15672,.F.);
#21866=ORIENTED_EDGE('',*,*,#15673,.T.);
#21867=ORIENTED_EDGE('',*,*,#15669,.T.);
#21868=ORIENTED_EDGE('',*,*,#15674,.T.);
#21869=ORIENTED_EDGE('',*,*,#15675,.F.);
#21870=ORIENTED_EDGE('',*,*,#15676,.T.);
#21871=ORIENTED_EDGE('',*,*,#15672,.T.);
#21872=ORIENTED_EDGE('',*,*,#15677,.T.);
#21873=ORIENTED_EDGE('',*,*,#15678,.F.);
#21874=ORIENTED_EDGE('',*,*,#15679,.T.);
#21875=ORIENTED_EDGE('',*,*,#15675,.T.);
#21876=ORIENTED_EDGE('',*,*,#15680,.T.);
#21877=ORIENTED_EDGE('',*,*,#15681,.F.);
#21878=ORIENTED_EDGE('',*,*,#15682,.T.);
#21879=ORIENTED_EDGE('',*,*,#15678,.T.);
#21880=ORIENTED_EDGE('',*,*,#15683,.T.);
#21881=ORIENTED_EDGE('',*,*,#15684,.F.);
#21882=ORIENTED_EDGE('',*,*,#15685,.T.);
#21883=ORIENTED_EDGE('',*,*,#15686,.F.);
#21884=ORIENTED_EDGE('',*,*,#15687,.F.);
#21885=ORIENTED_EDGE('',*,*,#15688,.T.);
#21886=ORIENTED_EDGE('',*,*,#15684,.T.);
#21887=ORIENTED_EDGE('',*,*,#15689,.F.);
#21888=ORIENTED_EDGE('',*,*,#15690,.F.);
#21889=ORIENTED_EDGE('',*,*,#15691,.F.);
#21890=ORIENTED_EDGE('',*,*,#15692,.T.);
#21891=ORIENTED_EDGE('',*,*,#15687,.T.);
#21892=ORIENTED_EDGE('',*,*,#15693,.F.);
#21893=ORIENTED_EDGE('',*,*,#15694,.F.);
#21894=ORIENTED_EDGE('',*,*,#15695,.T.);
#21895=ORIENTED_EDGE('',*,*,#15691,.T.);
#21896=ORIENTED_EDGE('',*,*,#15696,.F.);
#21897=ORIENTED_EDGE('',*,*,#15697,.F.);
#21898=ORIENTED_EDGE('',*,*,#15698,.T.);
#21899=ORIENTED_EDGE('',*,*,#15694,.T.);
#21900=ORIENTED_EDGE('',*,*,#15699,.F.);
#21901=ORIENTED_EDGE('',*,*,#15700,.F.);
#21902=ORIENTED_EDGE('',*,*,#15701,.T.);
#21903=ORIENTED_EDGE('',*,*,#15697,.T.);
#21904=ORIENTED_EDGE('',*,*,#15702,.F.);
#21905=ORIENTED_EDGE('',*,*,#15703,.F.);
#21906=ORIENTED_EDGE('',*,*,#15704,.T.);
#21907=ORIENTED_EDGE('',*,*,#15700,.T.);
#21908=ORIENTED_EDGE('',*,*,#15705,.F.);
#21909=ORIENTED_EDGE('',*,*,#15706,.F.);
#21910=ORIENTED_EDGE('',*,*,#15707,.T.);
#21911=ORIENTED_EDGE('',*,*,#15703,.T.);
#21912=ORIENTED_EDGE('',*,*,#15708,.F.);
#21913=ORIENTED_EDGE('',*,*,#15709,.F.);
#21914=ORIENTED_EDGE('',*,*,#15710,.T.);
#21915=ORIENTED_EDGE('',*,*,#15706,.T.);
#21916=ORIENTED_EDGE('',*,*,#15711,.F.);
#21917=ORIENTED_EDGE('',*,*,#15712,.F.);
#21918=ORIENTED_EDGE('',*,*,#15713,.T.);
#21919=ORIENTED_EDGE('',*,*,#15709,.T.);
#21920=ORIENTED_EDGE('',*,*,#15714,.F.);
#21921=ORIENTED_EDGE('',*,*,#15715,.F.);
#21922=ORIENTED_EDGE('',*,*,#15716,.T.);
#21923=ORIENTED_EDGE('',*,*,#15712,.T.);
#21924=ORIENTED_EDGE('',*,*,#15717,.F.);
#21925=ORIENTED_EDGE('',*,*,#15718,.F.);
#21926=ORIENTED_EDGE('',*,*,#15719,.T.);
#21927=ORIENTED_EDGE('',*,*,#15715,.T.);
#21928=ORIENTED_EDGE('',*,*,#15720,.F.);
#21929=ORIENTED_EDGE('',*,*,#15721,.F.);
#21930=ORIENTED_EDGE('',*,*,#15722,.T.);
#21931=ORIENTED_EDGE('',*,*,#15718,.T.);
#21932=ORIENTED_EDGE('',*,*,#15723,.F.);
#21933=ORIENTED_EDGE('',*,*,#15724,.F.);
#21934=ORIENTED_EDGE('',*,*,#15725,.T.);
#21935=ORIENTED_EDGE('',*,*,#15721,.T.);
#21936=ORIENTED_EDGE('',*,*,#15726,.F.);
#21937=ORIENTED_EDGE('',*,*,#15727,.F.);
#21938=ORIENTED_EDGE('',*,*,#15728,.T.);
#21939=ORIENTED_EDGE('',*,*,#15724,.T.);
#21940=ORIENTED_EDGE('',*,*,#15729,.F.);
#21941=ORIENTED_EDGE('',*,*,#15730,.F.);
#21942=ORIENTED_EDGE('',*,*,#15731,.T.);
#21943=ORIENTED_EDGE('',*,*,#15727,.T.);
#21944=ORIENTED_EDGE('',*,*,#15732,.F.);
#21945=ORIENTED_EDGE('',*,*,#15733,.F.);
#21946=ORIENTED_EDGE('',*,*,#15734,.T.);
#21947=ORIENTED_EDGE('',*,*,#15730,.T.);
#21948=ORIENTED_EDGE('',*,*,#15735,.F.);
#21949=ORIENTED_EDGE('',*,*,#15736,.F.);
#21950=ORIENTED_EDGE('',*,*,#15737,.T.);
#21951=ORIENTED_EDGE('',*,*,#15733,.T.);
#21952=ORIENTED_EDGE('',*,*,#15738,.F.);
#21953=ORIENTED_EDGE('',*,*,#15739,.F.);
#21954=ORIENTED_EDGE('',*,*,#15740,.T.);
#21955=ORIENTED_EDGE('',*,*,#15736,.T.);
#21956=ORIENTED_EDGE('',*,*,#15741,.F.);
#21957=ORIENTED_EDGE('',*,*,#15742,.F.);
#21958=ORIENTED_EDGE('',*,*,#15743,.T.);
#21959=ORIENTED_EDGE('',*,*,#15739,.T.);
#21960=ORIENTED_EDGE('',*,*,#15744,.F.);
#21961=ORIENTED_EDGE('',*,*,#15745,.F.);
#21962=ORIENTED_EDGE('',*,*,#15746,.F.);
#21963=ORIENTED_EDGE('',*,*,#15683,.F.);
#21964=ORIENTED_EDGE('',*,*,#15680,.F.);
#21965=ORIENTED_EDGE('',*,*,#15677,.F.);
#21966=ORIENTED_EDGE('',*,*,#15674,.F.);
#21967=ORIENTED_EDGE('',*,*,#15671,.F.);
#21968=ORIENTED_EDGE('',*,*,#15668,.F.);
#21969=ORIENTED_EDGE('',*,*,#15665,.F.);
#21970=ORIENTED_EDGE('',*,*,#15662,.F.);
#21971=ORIENTED_EDGE('',*,*,#15659,.F.);
#21972=ORIENTED_EDGE('',*,*,#15656,.F.);
#21973=ORIENTED_EDGE('',*,*,#15653,.F.);
#21974=ORIENTED_EDGE('',*,*,#15650,.F.);
#21975=ORIENTED_EDGE('',*,*,#15647,.F.);
#21976=ORIENTED_EDGE('',*,*,#15644,.F.);
#21977=ORIENTED_EDGE('',*,*,#15641,.F.);
#21978=ORIENTED_EDGE('',*,*,#15638,.F.);
#21979=ORIENTED_EDGE('',*,*,#15635,.F.);
#21980=ORIENTED_EDGE('',*,*,#15632,.F.);
#21981=ORIENTED_EDGE('',*,*,#15629,.F.);
#21982=ORIENTED_EDGE('',*,*,#15626,.F.);
#21983=ORIENTED_EDGE('',*,*,#15747,.F.);
#21984=ORIENTED_EDGE('',*,*,#15748,.T.);
#21985=ORIENTED_EDGE('',*,*,#15744,.T.);
#21986=ORIENTED_EDGE('',*,*,#15741,.T.);
#21987=ORIENTED_EDGE('',*,*,#15738,.T.);
#21988=ORIENTED_EDGE('',*,*,#15735,.T.);
#21989=ORIENTED_EDGE('',*,*,#15732,.T.);
#21990=ORIENTED_EDGE('',*,*,#15729,.T.);
#21991=ORIENTED_EDGE('',*,*,#15726,.T.);
#21992=ORIENTED_EDGE('',*,*,#15723,.T.);
#21993=ORIENTED_EDGE('',*,*,#15720,.T.);
#21994=ORIENTED_EDGE('',*,*,#15717,.T.);
#21995=ORIENTED_EDGE('',*,*,#15714,.T.);
#21996=ORIENTED_EDGE('',*,*,#15711,.T.);
#21997=ORIENTED_EDGE('',*,*,#15708,.T.);
#21998=ORIENTED_EDGE('',*,*,#15705,.T.);
#21999=ORIENTED_EDGE('',*,*,#15702,.T.);
#22000=ORIENTED_EDGE('',*,*,#15699,.T.);
#22001=ORIENTED_EDGE('',*,*,#15696,.T.);
#22002=ORIENTED_EDGE('',*,*,#15693,.T.);
#22003=ORIENTED_EDGE('',*,*,#15690,.T.);
#22004=ORIENTED_EDGE('',*,*,#15749,.T.);
#22005=ORIENTED_EDGE('',*,*,#15750,.T.);
#22006=ORIENTED_EDGE('',*,*,#15751,.T.);
#22007=ORIENTED_EDGE('',*,*,#15752,.T.);
#22008=ORIENTED_EDGE('',*,*,#15747,.T.);
#22009=ORIENTED_EDGE('',*,*,#15742,.T.);
#22010=ORIENTED_EDGE('',*,*,#15748,.F.);
#22011=ORIENTED_EDGE('',*,*,#15752,.F.);
#22012=ORIENTED_EDGE('',*,*,#15753,.T.);
#22013=ORIENTED_EDGE('',*,*,#15754,.F.);
#22014=ORIENTED_EDGE('',*,*,#15685,.F.);
#22015=ORIENTED_EDGE('',*,*,#15688,.F.);
#22016=ORIENTED_EDGE('',*,*,#15692,.F.);
#22017=ORIENTED_EDGE('',*,*,#15695,.F.);
#22018=ORIENTED_EDGE('',*,*,#15698,.F.);
#22019=ORIENTED_EDGE('',*,*,#15701,.F.);
#22020=ORIENTED_EDGE('',*,*,#15704,.F.);
#22021=ORIENTED_EDGE('',*,*,#15707,.F.);
#22022=ORIENTED_EDGE('',*,*,#15710,.F.);
#22023=ORIENTED_EDGE('',*,*,#15713,.F.);
#22024=ORIENTED_EDGE('',*,*,#15716,.F.);
#22025=ORIENTED_EDGE('',*,*,#15719,.F.);
#22026=ORIENTED_EDGE('',*,*,#15722,.F.);
#22027=ORIENTED_EDGE('',*,*,#15725,.F.);
#22028=ORIENTED_EDGE('',*,*,#15728,.F.);
#22029=ORIENTED_EDGE('',*,*,#15731,.F.);
#22030=ORIENTED_EDGE('',*,*,#15734,.F.);
#22031=ORIENTED_EDGE('',*,*,#15737,.F.);
#22032=ORIENTED_EDGE('',*,*,#15740,.F.);
#22033=ORIENTED_EDGE('',*,*,#15743,.F.);
#22034=ORIENTED_EDGE('',*,*,#15753,.F.);
#22035=ORIENTED_EDGE('',*,*,#15751,.F.);
#22036=ORIENTED_EDGE('',*,*,#15624,.F.);
#22037=ORIENTED_EDGE('',*,*,#15628,.F.);
#22038=ORIENTED_EDGE('',*,*,#15631,.F.);
#22039=ORIENTED_EDGE('',*,*,#15634,.F.);
#22040=ORIENTED_EDGE('',*,*,#15637,.F.);
#22041=ORIENTED_EDGE('',*,*,#15640,.F.);
#22042=ORIENTED_EDGE('',*,*,#15643,.F.);
#22043=ORIENTED_EDGE('',*,*,#15646,.F.);
#22044=ORIENTED_EDGE('',*,*,#15649,.F.);
#22045=ORIENTED_EDGE('',*,*,#15652,.F.);
#22046=ORIENTED_EDGE('',*,*,#15655,.F.);
#22047=ORIENTED_EDGE('',*,*,#15658,.F.);
#22048=ORIENTED_EDGE('',*,*,#15661,.F.);
#22049=ORIENTED_EDGE('',*,*,#15664,.F.);
#22050=ORIENTED_EDGE('',*,*,#15667,.F.);
#22051=ORIENTED_EDGE('',*,*,#15670,.F.);
#22052=ORIENTED_EDGE('',*,*,#15673,.F.);
#22053=ORIENTED_EDGE('',*,*,#15676,.F.);
#22054=ORIENTED_EDGE('',*,*,#15679,.F.);
#22055=ORIENTED_EDGE('',*,*,#15682,.F.);
#22056=ORIENTED_EDGE('',*,*,#15755,.F.);
#22057=ORIENTED_EDGE('',*,*,#15756,.F.);
#22058=ORIENTED_EDGE('',*,*,#15757,.F.);
#22059=ORIENTED_EDGE('',*,*,#15758,.F.);
#22060=ORIENTED_EDGE('',*,*,#15759,.F.);
#22061=ORIENTED_EDGE('',*,*,#15760,.F.);
#22062=ORIENTED_EDGE('',*,*,#15761,.T.);
#22063=ORIENTED_EDGE('',*,*,#15762,.F.);
#22064=ORIENTED_EDGE('',*,*,#15761,.F.);
#22065=ORIENTED_EDGE('',*,*,#15763,.F.);
#22066=ORIENTED_EDGE('',*,*,#15764,.F.);
#22067=ORIENTED_EDGE('',*,*,#15759,.T.);
#22068=ORIENTED_EDGE('',*,*,#15765,.F.);
#22069=ORIENTED_EDGE('',*,*,#15766,.T.);
#22070=ORIENTED_EDGE('',*,*,#15767,.T.);
#22071=ORIENTED_EDGE('',*,*,#15758,.T.);
#22072=ORIENTED_EDGE('',*,*,#15768,.F.);
#22073=ORIENTED_EDGE('',*,*,#15769,.T.);
#22074=ORIENTED_EDGE('',*,*,#15765,.T.);
#22075=ORIENTED_EDGE('',*,*,#15757,.T.);
#22076=ORIENTED_EDGE('',*,*,#15770,.F.);
#22077=ORIENTED_EDGE('',*,*,#15771,.T.);
#22078=ORIENTED_EDGE('',*,*,#15768,.T.);
#22079=ORIENTED_EDGE('',*,*,#15771,.F.);
#22080=ORIENTED_EDGE('',*,*,#15772,.F.);
#22081=ORIENTED_EDGE('',*,*,#15773,.F.);
#22082=ORIENTED_EDGE('',*,*,#15774,.F.);
#22083=ORIENTED_EDGE('',*,*,#15766,.F.);
#22084=ORIENTED_EDGE('',*,*,#15769,.F.);
#22085=ORIENTED_EDGE('',*,*,#15775,.T.);
#22086=ORIENTED_EDGE('',*,*,#15756,.T.);
#22087=ORIENTED_EDGE('',*,*,#15776,.F.);
#22088=ORIENTED_EDGE('',*,*,#15772,.T.);
#22089=ORIENTED_EDGE('',*,*,#15770,.T.);
#22090=ORIENTED_EDGE('',*,*,#15764,.T.);
#22091=ORIENTED_EDGE('',*,*,#15777,.F.);
#22092=ORIENTED_EDGE('',*,*,#15773,.T.);
#22093=ORIENTED_EDGE('',*,*,#15776,.T.);
#22094=ORIENTED_EDGE('',*,*,#15763,.T.);
#22095=ORIENTED_EDGE('',*,*,#15760,.T.);
#22096=ORIENTED_EDGE('',*,*,#15767,.F.);
#22097=ORIENTED_EDGE('',*,*,#15774,.T.);
#22098=ORIENTED_EDGE('',*,*,#15777,.T.);
#22099=ORIENTED_EDGE('',*,*,#15762,.T.);
#22100=ORIENTED_EDGE('',*,*,#15778,.F.);
#22101=ORIENTED_EDGE('',*,*,#15749,.F.);
#22102=ORIENTED_EDGE('',*,*,#15625,.F.);
#22103=ORIENTED_EDGE('',*,*,#15750,.F.);
#22104=ORIENTED_EDGE('',*,*,#15779,.T.);
#22105=ORIENTED_EDGE('',*,*,#15778,.T.);
#22106=ORIENTED_EDGE('',*,*,#15779,.F.);
#22107=ORIENTED_EDGE('',*,*,#15681,.T.);
#22108=ORIENTED_EDGE('',*,*,#15746,.T.);
#22109=ORIENTED_EDGE('',*,*,#15780,.F.);
#22110=ORIENTED_EDGE('',*,*,#15755,.T.);
#22111=ORIENTED_EDGE('',*,*,#15781,.F.);
#22112=ORIENTED_EDGE('',*,*,#15780,.T.);
#22113=ORIENTED_EDGE('',*,*,#15745,.T.);
#22114=ORIENTED_EDGE('',*,*,#15689,.T.);
#22115=ORIENTED_EDGE('',*,*,#15686,.T.);
#22116=ORIENTED_EDGE('',*,*,#15754,.T.);
#22117=ORIENTED_EDGE('',*,*,#15775,.F.);
#22118=ORIENTED_EDGE('',*,*,#15782,.T.);
#22119=ORIENTED_EDGE('',*,*,#15781,.T.);
#22120=ORIENTED_EDGE('',*,*,#15782,.F.);
#22121=ORIENTED_EDGE('',*,*,#15783,.T.);
#22122=ORIENTED_EDGE('',*,*,#15784,.T.);
#22123=ORIENTED_EDGE('',*,*,#15785,.T.);
#22124=ORIENTED_EDGE('',*,*,#15784,.F.);
#22125=ORIENTED_EDGE('',*,*,#15783,.F.);
#22126=ORIENTED_EDGE('',*,*,#15786,.T.);
#22127=ORIENTED_EDGE('',*,*,#15787,.F.);
#22128=ORIENTED_EDGE('',*,*,#15786,.F.);
#22129=ORIENTED_EDGE('',*,*,#15788,.F.);
#22130=ORIENTED_EDGE('',*,*,#15789,.F.);
#22131=ORIENTED_EDGE('',*,*,#15790,.F.);
#22132=ORIENTED_EDGE('',*,*,#15791,.F.);
#22133=ORIENTED_EDGE('',*,*,#15792,.F.);
#22134=ORIENTED_EDGE('',*,*,#15793,.F.);
#22135=ORIENTED_EDGE('',*,*,#15794,.F.);
#22136=ORIENTED_EDGE('',*,*,#15795,.F.);
#22137=ORIENTED_EDGE('',*,*,#15785,.F.);
#22138=ORIENTED_EDGE('',*,*,#15787,.T.);
#22139=ORIENTED_EDGE('',*,*,#15796,.T.);
#22140=ORIENTED_EDGE('',*,*,#15797,.T.);
#22141=ORIENTED_EDGE('',*,*,#15796,.F.);
#22142=ORIENTED_EDGE('',*,*,#15798,.F.);
#22143=ORIENTED_EDGE('',*,*,#15799,.T.);
#22144=ORIENTED_EDGE('',*,*,#15797,.F.);
#22145=ORIENTED_EDGE('',*,*,#15799,.F.);
#22146=ORIENTED_EDGE('',*,*,#15800,.T.);
#22147=ORIENTED_EDGE('',*,*,#15801,.T.);
#22148=ORIENTED_EDGE('',*,*,#15798,.T.);
#22149=ORIENTED_EDGE('',*,*,#15801,.F.);
#22150=ORIENTED_EDGE('',*,*,#15802,.F.);
#22151=ORIENTED_EDGE('',*,*,#15803,.T.);
#22152=ORIENTED_EDGE('',*,*,#15800,.F.);
#22153=ORIENTED_EDGE('',*,*,#15803,.F.);
#22154=ORIENTED_EDGE('',*,*,#15802,.T.);
#22155=ORIENTED_EDGE('',*,*,#15804,.T.);
#22156=ORIENTED_EDGE('',*,*,#15805,.T.);
#22157=ORIENTED_EDGE('',*,*,#15804,.F.);
#22158=ORIENTED_EDGE('',*,*,#15806,.F.);
#22159=ORIENTED_EDGE('',*,*,#15807,.F.);
#22160=ORIENTED_EDGE('',*,*,#15808,.F.);
#22161=ORIENTED_EDGE('',*,*,#15809,.F.);
#22162=ORIENTED_EDGE('',*,*,#15810,.F.);
#22163=ORIENTED_EDGE('',*,*,#15811,.F.);
#22164=ORIENTED_EDGE('',*,*,#15812,.F.);
#22165=ORIENTED_EDGE('',*,*,#15813,.F.);
#22166=ORIENTED_EDGE('',*,*,#15805,.F.);
#22167=ORIENTED_EDGE('',*,*,#15814,.T.);
#22168=ORIENTED_EDGE('',*,*,#15815,.T.);
#22169=ORIENTED_EDGE('',*,*,#15816,.T.);
#22170=ORIENTED_EDGE('',*,*,#15817,.T.);
#22171=ORIENTED_EDGE('',*,*,#15818,.T.);
#22172=ORIENTED_EDGE('',*,*,#15819,.T.);
#22173=ORIENTED_EDGE('',*,*,#15814,.F.);
#22174=ORIENTED_EDGE('',*,*,#15820,.T.);
#22175=ORIENTED_EDGE('',*,*,#15821,.T.);
#22176=ORIENTED_EDGE('',*,*,#15822,.T.);
#22177=ORIENTED_EDGE('',*,*,#15818,.F.);
#22178=ORIENTED_EDGE('',*,*,#15823,.T.);
#22179=ORIENTED_EDGE('',*,*,#15824,.T.);
#22180=ORIENTED_EDGE('',*,*,#15825,.T.);
#22181=ORIENTED_EDGE('',*,*,#15821,.F.);
#22182=ORIENTED_EDGE('',*,*,#15826,.T.);
#22183=ORIENTED_EDGE('',*,*,#15827,.T.);
#22184=ORIENTED_EDGE('',*,*,#15828,.T.);
#22185=ORIENTED_EDGE('',*,*,#15824,.F.);
#22186=ORIENTED_EDGE('',*,*,#15829,.T.);
#22187=ORIENTED_EDGE('',*,*,#15830,.T.);
#22188=ORIENTED_EDGE('',*,*,#15831,.T.);
#22189=ORIENTED_EDGE('',*,*,#15827,.F.);
#22190=ORIENTED_EDGE('',*,*,#15832,.T.);
#22191=ORIENTED_EDGE('',*,*,#15833,.T.);
#22192=ORIENTED_EDGE('',*,*,#15834,.T.);
#22193=ORIENTED_EDGE('',*,*,#15830,.F.);
#22194=ORIENTED_EDGE('',*,*,#15835,.T.);
#22195=ORIENTED_EDGE('',*,*,#15816,.F.);
#22196=ORIENTED_EDGE('',*,*,#15836,.T.);
#22197=ORIENTED_EDGE('',*,*,#15833,.F.);
#22198=ORIENTED_EDGE('',*,*,#15837,.T.);
#22199=ORIENTED_EDGE('',*,*,#15826,.F.);
#22200=ORIENTED_EDGE('',*,*,#15838,.F.);
#22201=ORIENTED_EDGE('',*,*,#15839,.F.);
#22202=ORIENTED_EDGE('',*,*,#15840,.T.);
#22203=ORIENTED_EDGE('',*,*,#15823,.F.);
#22204=ORIENTED_EDGE('',*,*,#15841,.F.);
#22205=ORIENTED_EDGE('',*,*,#15842,.F.);
#22206=ORIENTED_EDGE('',*,*,#15838,.T.);
#22207=ORIENTED_EDGE('',*,*,#15820,.F.);
#22208=ORIENTED_EDGE('',*,*,#15843,.F.);
#22209=ORIENTED_EDGE('',*,*,#15844,.F.);
#22210=ORIENTED_EDGE('',*,*,#15841,.T.);
#22211=ORIENTED_EDGE('',*,*,#15817,.F.);
#22212=ORIENTED_EDGE('',*,*,#15845,.F.);
#22213=ORIENTED_EDGE('',*,*,#15846,.F.);
#22214=ORIENTED_EDGE('',*,*,#15843,.T.);
#22215=ORIENTED_EDGE('',*,*,#15831,.F.);
#22216=ORIENTED_EDGE('',*,*,#15847,.T.);
#22217=ORIENTED_EDGE('',*,*,#15790,.T.);
#22218=ORIENTED_EDGE('',*,*,#15848,.F.);
#22219=ORIENTED_EDGE('',*,*,#15834,.F.);
#22220=ORIENTED_EDGE('',*,*,#15849,.T.);
#22221=ORIENTED_EDGE('',*,*,#15791,.T.);
#22222=ORIENTED_EDGE('',*,*,#15847,.F.);
#22223=ORIENTED_EDGE('',*,*,#15836,.F.);
#22224=ORIENTED_EDGE('',*,*,#15850,.T.);
#22225=ORIENTED_EDGE('',*,*,#15792,.T.);
#22226=ORIENTED_EDGE('',*,*,#15849,.F.);
#22227=ORIENTED_EDGE('',*,*,#15815,.F.);
#22228=ORIENTED_EDGE('',*,*,#15851,.T.);
#22229=ORIENTED_EDGE('',*,*,#15793,.T.);
#22230=ORIENTED_EDGE('',*,*,#15850,.F.);
#22231=ORIENTED_EDGE('',*,*,#15852,.T.);
#22232=ORIENTED_EDGE('',*,*,#15853,.T.);
#22233=ORIENTED_EDGE('',*,*,#15854,.T.);
#22234=ORIENTED_EDGE('',*,*,#15806,.T.);
#22235=ORIENTED_EDGE('',*,*,#15855,.T.);
#22236=ORIENTED_EDGE('',*,*,#15856,.T.);
#22237=ORIENTED_EDGE('',*,*,#15852,.F.);
#22238=ORIENTED_EDGE('',*,*,#15813,.T.);
#22239=ORIENTED_EDGE('',*,*,#15857,.T.);
#22240=ORIENTED_EDGE('',*,*,#15858,.T.);
#22241=ORIENTED_EDGE('',*,*,#15855,.F.);
#22242=ORIENTED_EDGE('',*,*,#15812,.T.);
#22243=ORIENTED_EDGE('',*,*,#15859,.T.);
#22244=ORIENTED_EDGE('',*,*,#15860,.T.);
#22245=ORIENTED_EDGE('',*,*,#15857,.F.);
#22246=ORIENTED_EDGE('',*,*,#15811,.T.);
#22247=ORIENTED_EDGE('',*,*,#15861,.T.);
#22248=ORIENTED_EDGE('',*,*,#15862,.T.);
#22249=ORIENTED_EDGE('',*,*,#15859,.F.);
#22250=ORIENTED_EDGE('',*,*,#15810,.T.);
#22251=ORIENTED_EDGE('',*,*,#15863,.T.);
#22252=ORIENTED_EDGE('',*,*,#15864,.T.);
#22253=ORIENTED_EDGE('',*,*,#15861,.F.);
#22254=ORIENTED_EDGE('',*,*,#15809,.T.);
#22255=ORIENTED_EDGE('',*,*,#15865,.T.);
#22256=ORIENTED_EDGE('',*,*,#15866,.T.);
#22257=ORIENTED_EDGE('',*,*,#15863,.F.);
#22258=ORIENTED_EDGE('',*,*,#15808,.T.);
#22259=ORIENTED_EDGE('',*,*,#15854,.F.);
#22260=ORIENTED_EDGE('',*,*,#15867,.T.);
#22261=ORIENTED_EDGE('',*,*,#15865,.F.);
#22262=ORIENTED_EDGE('',*,*,#15807,.T.);
#22263=ORIENTED_EDGE('',*,*,#15864,.F.);
#22264=ORIENTED_EDGE('',*,*,#15868,.T.);
#22265=ORIENTED_EDGE('',*,*,#15869,.F.);
#22266=ORIENTED_EDGE('',*,*,#15870,.F.);
#22267=ORIENTED_EDGE('',*,*,#15866,.F.);
#22268=ORIENTED_EDGE('',*,*,#15871,.T.);
#22269=ORIENTED_EDGE('',*,*,#15872,.F.);
#22270=ORIENTED_EDGE('',*,*,#15868,.F.);
#22271=ORIENTED_EDGE('',*,*,#15867,.F.);
#22272=ORIENTED_EDGE('',*,*,#15873,.F.);
#22273=ORIENTED_EDGE('',*,*,#15874,.F.);
#22274=ORIENTED_EDGE('',*,*,#15871,.F.);
#22275=ORIENTED_EDGE('',*,*,#15853,.F.);
#22276=ORIENTED_EDGE('',*,*,#15875,.T.);
#22277=ORIENTED_EDGE('',*,*,#15876,.F.);
#22278=ORIENTED_EDGE('',*,*,#15873,.T.);
#22279=ORIENTED_EDGE('',*,*,#15877,.T.);
#22280=ORIENTED_EDGE('',*,*,#15876,.T.);
#22281=ORIENTED_EDGE('',*,*,#15878,.T.);
#22282=ORIENTED_EDGE('',*,*,#15839,.T.);
#22283=ORIENTED_EDGE('',*,*,#15879,.T.);
#22284=ORIENTED_EDGE('',*,*,#15874,.T.);
#22285=ORIENTED_EDGE('',*,*,#15877,.F.);
#22286=ORIENTED_EDGE('',*,*,#15842,.T.);
#22287=ORIENTED_EDGE('',*,*,#15880,.T.);
#22288=ORIENTED_EDGE('',*,*,#15872,.T.);
#22289=ORIENTED_EDGE('',*,*,#15879,.F.);
#22290=ORIENTED_EDGE('',*,*,#15844,.T.);
#22291=ORIENTED_EDGE('',*,*,#15881,.T.);
#22292=ORIENTED_EDGE('',*,*,#15869,.T.);
#22293=ORIENTED_EDGE('',*,*,#15880,.F.);
#22294=ORIENTED_EDGE('',*,*,#15846,.T.);
#22295=ORIENTED_EDGE('',*,*,#15882,.T.);
#22296=ORIENTED_EDGE('',*,*,#15883,.T.);
#22297=ORIENTED_EDGE('',*,*,#15881,.F.);
#22298=ORIENTED_EDGE('',*,*,#15884,.T.);
#22299=ORIENTED_EDGE('',*,*,#15885,.T.);
#22300=ORIENTED_EDGE('',*,*,#15886,.T.);
#22301=ORIENTED_EDGE('',*,*,#15882,.F.);
#22302=ORIENTED_EDGE('',*,*,#15887,.T.);
#22303=ORIENTED_EDGE('',*,*,#15888,.T.);
#22304=ORIENTED_EDGE('',*,*,#15889,.T.);
#22305=ORIENTED_EDGE('',*,*,#15885,.F.);
#22306=ORIENTED_EDGE('',*,*,#15890,.T.);
#22307=ORIENTED_EDGE('',*,*,#15878,.F.);
#22308=ORIENTED_EDGE('',*,*,#15891,.T.);
#22309=ORIENTED_EDGE('',*,*,#15888,.F.);
#22310=ORIENTED_EDGE('',*,*,#15892,.T.);
#22311=ORIENTED_EDGE('',*,*,#15860,.F.);
#22312=ORIENTED_EDGE('',*,*,#15893,.T.);
#22313=ORIENTED_EDGE('',*,*,#15886,.F.);
#22314=ORIENTED_EDGE('',*,*,#15894,.F.);
#22315=ORIENTED_EDGE('',*,*,#15858,.F.);
#22316=ORIENTED_EDGE('',*,*,#15894,.T.);
#22317=ORIENTED_EDGE('',*,*,#15889,.F.);
#22318=ORIENTED_EDGE('',*,*,#15895,.F.);
#22319=ORIENTED_EDGE('',*,*,#15856,.F.);
#22320=ORIENTED_EDGE('',*,*,#15895,.T.);
#22321=ORIENTED_EDGE('',*,*,#15891,.F.);
#22322=ORIENTED_EDGE('',*,*,#15875,.F.);
#22323=ORIENTED_EDGE('',*,*,#15862,.F.);
#22324=ORIENTED_EDGE('',*,*,#15870,.T.);
#22325=ORIENTED_EDGE('',*,*,#15883,.F.);
#22326=ORIENTED_EDGE('',*,*,#15893,.F.);
#22327=ORIENTED_EDGE('',*,*,#15825,.F.);
#22328=ORIENTED_EDGE('',*,*,#15896,.T.);
#22329=ORIENTED_EDGE('',*,*,#15788,.T.);
#22330=ORIENTED_EDGE('',*,*,#15897,.T.);
#22331=ORIENTED_EDGE('',*,*,#15828,.F.);
#22332=ORIENTED_EDGE('',*,*,#15848,.T.);
#22333=ORIENTED_EDGE('',*,*,#15789,.T.);
#22334=ORIENTED_EDGE('',*,*,#15896,.F.);
#22335=ORIENTED_EDGE('',*,*,#15819,.F.);
#22336=ORIENTED_EDGE('',*,*,#15898,.T.);
#22337=ORIENTED_EDGE('',*,*,#15794,.T.);
#22338=ORIENTED_EDGE('',*,*,#15851,.F.);
#22339=ORIENTED_EDGE('',*,*,#15822,.F.);
#22340=ORIENTED_EDGE('',*,*,#15897,.F.);
#22341=ORIENTED_EDGE('',*,*,#15795,.T.);
#22342=ORIENTED_EDGE('',*,*,#15898,.F.);
#22343=ORIENTED_EDGE('',*,*,#15835,.F.);
#22344=ORIENTED_EDGE('',*,*,#15899,.F.);
#22345=ORIENTED_EDGE('',*,*,#15887,.F.);
#22346=ORIENTED_EDGE('',*,*,#15900,.T.);
#22347=ORIENTED_EDGE('',*,*,#15832,.F.);
#22348=ORIENTED_EDGE('',*,*,#15901,.F.);
#22349=ORIENTED_EDGE('',*,*,#15890,.F.);
#22350=ORIENTED_EDGE('',*,*,#15899,.T.);
#22351=ORIENTED_EDGE('',*,*,#15829,.F.);
#22352=ORIENTED_EDGE('',*,*,#15840,.F.);
#22353=ORIENTED_EDGE('',*,*,#15892,.F.);
#22354=ORIENTED_EDGE('',*,*,#15901,.T.);
#22355=ORIENTED_EDGE('',*,*,#15837,.F.);
#22356=ORIENTED_EDGE('',*,*,#15900,.F.);
#22357=ORIENTED_EDGE('',*,*,#15884,.F.);
#22358=ORIENTED_EDGE('',*,*,#15845,.T.);
#22359=ORIENTED_EDGE('',*,*,#15902,.T.);
#22360=ORIENTED_EDGE('',*,*,#15903,.T.);
#22361=ORIENTED_EDGE('',*,*,#15904,.F.);
#22362=ORIENTED_EDGE('',*,*,#15903,.F.);
#22363=ORIENTED_EDGE('',*,*,#15905,.F.);
#22364=ORIENTED_EDGE('',*,*,#15906,.T.);
#22365=ORIENTED_EDGE('',*,*,#15902,.F.);
#22366=ORIENTED_EDGE('',*,*,#15906,.F.);
#22367=ORIENTED_EDGE('',*,*,#15905,.T.);
#22368=ORIENTED_EDGE('',*,*,#15907,.T.);
#22369=ORIENTED_EDGE('',*,*,#15908,.T.);
#22370=ORIENTED_EDGE('',*,*,#15907,.F.);
#22371=ORIENTED_EDGE('',*,*,#15909,.T.);
#22372=ORIENTED_EDGE('',*,*,#15910,.T.);
#22373=ORIENTED_EDGE('',*,*,#15911,.F.);
#22374=ORIENTED_EDGE('',*,*,#15910,.F.);
#22375=ORIENTED_EDGE('',*,*,#15912,.F.);
#22376=ORIENTED_EDGE('',*,*,#15911,.T.);
#22377=ORIENTED_EDGE('',*,*,#15913,.F.);
#22378=ORIENTED_EDGE('',*,*,#15914,.T.);
#22379=ORIENTED_EDGE('',*,*,#15912,.T.);
#22380=ORIENTED_EDGE('',*,*,#15914,.F.);
#22381=ORIENTED_EDGE('',*,*,#15915,.F.);
#22382=ORIENTED_EDGE('',*,*,#15916,.T.);
#22383=ORIENTED_EDGE('',*,*,#15913,.T.);
#22384=ORIENTED_EDGE('',*,*,#15916,.F.);
#22385=ORIENTED_EDGE('',*,*,#15915,.T.);
#22386=ORIENTED_EDGE('',*,*,#15908,.F.);
#22387=ORIENTED_EDGE('',*,*,#15917,.F.);
#22388=ORIENTED_EDGE('',*,*,#15918,.T.);
#22389=ORIENTED_EDGE('',*,*,#15904,.T.);
#22390=ORIENTED_EDGE('',*,*,#15918,.F.);
#22391=ORIENTED_EDGE('',*,*,#15919,.F.);
#22392=ORIENTED_EDGE('',*,*,#15917,.T.);
#22393=ORIENTED_EDGE('',*,*,#15920,.F.);
#22394=ORIENTED_EDGE('',*,*,#15921,.T.);
#22395=ORIENTED_EDGE('',*,*,#15919,.T.);
#22396=ORIENTED_EDGE('',*,*,#15921,.F.);
#22397=ORIENTED_EDGE('',*,*,#15922,.F.);
#22398=ORIENTED_EDGE('',*,*,#15923,.T.);
#22399=ORIENTED_EDGE('',*,*,#15920,.T.);
#22400=ORIENTED_EDGE('',*,*,#15923,.F.);
#22401=ORIENTED_EDGE('',*,*,#15922,.T.);
#22402=ORIENTED_EDGE('',*,*,#15924,.F.);
#22403=ORIENTED_EDGE('',*,*,#15924,.T.);
#22404=ORIENTED_EDGE('',*,*,#15925,.T.);
#22405=ORIENTED_EDGE('',*,*,#15926,.F.);
#22406=ORIENTED_EDGE('',*,*,#15925,.F.);
#22407=ORIENTED_EDGE('',*,*,#15927,.F.);
#22408=ORIENTED_EDGE('',*,*,#15926,.T.);
#22409=ORIENTED_EDGE('',*,*,#15927,.T.);
#22410=ORIENTED_EDGE('',*,*,#15928,.T.);
#22411=ORIENTED_EDGE('',*,*,#15929,.F.);
#22412=ORIENTED_EDGE('',*,*,#15928,.F.);
#22413=ORIENTED_EDGE('',*,*,#15929,.T.);
#22414=ORIENTED_EDGE('',*,*,#15909,.F.);
#22415=ORIENTED_EDGE('',*,*,#15930,.F.);
#22416=ORIENTED_EDGE('',*,*,#15931,.T.);
#22417=ORIENTED_EDGE('',*,*,#15932,.T.);
#22418=ORIENTED_EDGE('',*,*,#15933,.T.);
#22419=ORIENTED_EDGE('',*,*,#15934,.F.);
#22420=ORIENTED_EDGE('',*,*,#15935,.T.);
#22421=ORIENTED_EDGE('',*,*,#15930,.T.);
#22422=ORIENTED_EDGE('',*,*,#15936,.T.);
#22423=ORIENTED_EDGE('',*,*,#15937,.F.);
#22424=ORIENTED_EDGE('',*,*,#15938,.T.);
#22425=ORIENTED_EDGE('',*,*,#15934,.T.);
#22426=ORIENTED_EDGE('',*,*,#15939,.T.);
#22427=ORIENTED_EDGE('',*,*,#15940,.F.);
#22428=ORIENTED_EDGE('',*,*,#15941,.T.);
#22429=ORIENTED_EDGE('',*,*,#15937,.T.);
#22430=ORIENTED_EDGE('',*,*,#15942,.T.);
#22431=ORIENTED_EDGE('',*,*,#15943,.F.);
#22432=ORIENTED_EDGE('',*,*,#15944,.T.);
#22433=ORIENTED_EDGE('',*,*,#15940,.T.);
#22434=ORIENTED_EDGE('',*,*,#15945,.T.);
#22435=ORIENTED_EDGE('',*,*,#15946,.F.);
#22436=ORIENTED_EDGE('',*,*,#15947,.T.);
#22437=ORIENTED_EDGE('',*,*,#15943,.T.);
#22438=ORIENTED_EDGE('',*,*,#15948,.T.);
#22439=ORIENTED_EDGE('',*,*,#15949,.F.);
#22440=ORIENTED_EDGE('',*,*,#15950,.T.);
#22441=ORIENTED_EDGE('',*,*,#15946,.T.);
#22442=ORIENTED_EDGE('',*,*,#15951,.T.);
#22443=ORIENTED_EDGE('',*,*,#15952,.F.);
#22444=ORIENTED_EDGE('',*,*,#15953,.T.);
#22445=ORIENTED_EDGE('',*,*,#15949,.T.);
#22446=ORIENTED_EDGE('',*,*,#15954,.T.);
#22447=ORIENTED_EDGE('',*,*,#15955,.F.);
#22448=ORIENTED_EDGE('',*,*,#15956,.T.);
#22449=ORIENTED_EDGE('',*,*,#15952,.T.);
#22450=ORIENTED_EDGE('',*,*,#15957,.T.);
#22451=ORIENTED_EDGE('',*,*,#15958,.F.);
#22452=ORIENTED_EDGE('',*,*,#15959,.T.);
#22453=ORIENTED_EDGE('',*,*,#15955,.T.);
#22454=ORIENTED_EDGE('',*,*,#15960,.T.);
#22455=ORIENTED_EDGE('',*,*,#15961,.F.);
#22456=ORIENTED_EDGE('',*,*,#15962,.T.);
#22457=ORIENTED_EDGE('',*,*,#15958,.T.);
#22458=ORIENTED_EDGE('',*,*,#15963,.T.);
#22459=ORIENTED_EDGE('',*,*,#15964,.F.);
#22460=ORIENTED_EDGE('',*,*,#15965,.T.);
#22461=ORIENTED_EDGE('',*,*,#15961,.T.);
#22462=ORIENTED_EDGE('',*,*,#15966,.T.);
#22463=ORIENTED_EDGE('',*,*,#15967,.F.);
#22464=ORIENTED_EDGE('',*,*,#15968,.T.);
#22465=ORIENTED_EDGE('',*,*,#15964,.T.);
#22466=ORIENTED_EDGE('',*,*,#15969,.T.);
#22467=ORIENTED_EDGE('',*,*,#15970,.F.);
#22468=ORIENTED_EDGE('',*,*,#15971,.T.);
#22469=ORIENTED_EDGE('',*,*,#15967,.T.);
#22470=ORIENTED_EDGE('',*,*,#15972,.T.);
#22471=ORIENTED_EDGE('',*,*,#15973,.F.);
#22472=ORIENTED_EDGE('',*,*,#15974,.T.);
#22473=ORIENTED_EDGE('',*,*,#15970,.T.);
#22474=ORIENTED_EDGE('',*,*,#15975,.T.);
#22475=ORIENTED_EDGE('',*,*,#15976,.F.);
#22476=ORIENTED_EDGE('',*,*,#15977,.T.);
#22477=ORIENTED_EDGE('',*,*,#15973,.T.);
#22478=ORIENTED_EDGE('',*,*,#15978,.T.);
#22479=ORIENTED_EDGE('',*,*,#15979,.F.);
#22480=ORIENTED_EDGE('',*,*,#15980,.T.);
#22481=ORIENTED_EDGE('',*,*,#15976,.T.);
#22482=ORIENTED_EDGE('',*,*,#15981,.T.);
#22483=ORIENTED_EDGE('',*,*,#15982,.F.);
#22484=ORIENTED_EDGE('',*,*,#15983,.T.);
#22485=ORIENTED_EDGE('',*,*,#15979,.T.);
#22486=ORIENTED_EDGE('',*,*,#15984,.T.);
#22487=ORIENTED_EDGE('',*,*,#15985,.F.);
#22488=ORIENTED_EDGE('',*,*,#15986,.T.);
#22489=ORIENTED_EDGE('',*,*,#15982,.T.);
#22490=ORIENTED_EDGE('',*,*,#15987,.T.);
#22491=ORIENTED_EDGE('',*,*,#15988,.F.);
#22492=ORIENTED_EDGE('',*,*,#15989,.T.);
#22493=ORIENTED_EDGE('',*,*,#15985,.T.);
#22494=ORIENTED_EDGE('',*,*,#15990,.T.);
#22495=ORIENTED_EDGE('',*,*,#15991,.F.);
#22496=ORIENTED_EDGE('',*,*,#15992,.T.);
#22497=ORIENTED_EDGE('',*,*,#15988,.T.);
#22498=ORIENTED_EDGE('',*,*,#15993,.T.);
#22499=ORIENTED_EDGE('',*,*,#15994,.F.);
#22500=ORIENTED_EDGE('',*,*,#15995,.T.);
#22501=ORIENTED_EDGE('',*,*,#15991,.T.);
#22502=ORIENTED_EDGE('',*,*,#15996,.T.);
#22503=ORIENTED_EDGE('',*,*,#15997,.F.);
#22504=ORIENTED_EDGE('',*,*,#15998,.T.);
#22505=ORIENTED_EDGE('',*,*,#15994,.T.);
#22506=ORIENTED_EDGE('',*,*,#15999,.T.);
#22507=ORIENTED_EDGE('',*,*,#16000,.F.);
#22508=ORIENTED_EDGE('',*,*,#16001,.T.);
#22509=ORIENTED_EDGE('',*,*,#16002,.F.);
#22510=ORIENTED_EDGE('',*,*,#16003,.F.);
#22511=ORIENTED_EDGE('',*,*,#16004,.F.);
#22512=ORIENTED_EDGE('',*,*,#16005,.T.);
#22513=ORIENTED_EDGE('',*,*,#16000,.T.);
#22514=ORIENTED_EDGE('',*,*,#16006,.F.);
#22515=ORIENTED_EDGE('',*,*,#16007,.F.);
#22516=ORIENTED_EDGE('',*,*,#16008,.T.);
#22517=ORIENTED_EDGE('',*,*,#16004,.T.);
#22518=ORIENTED_EDGE('',*,*,#16009,.F.);
#22519=ORIENTED_EDGE('',*,*,#16010,.F.);
#22520=ORIENTED_EDGE('',*,*,#16011,.T.);
#22521=ORIENTED_EDGE('',*,*,#16007,.T.);
#22522=ORIENTED_EDGE('',*,*,#16012,.F.);
#22523=ORIENTED_EDGE('',*,*,#16013,.F.);
#22524=ORIENTED_EDGE('',*,*,#16014,.T.);
#22525=ORIENTED_EDGE('',*,*,#16010,.T.);
#22526=ORIENTED_EDGE('',*,*,#16015,.F.);
#22527=ORIENTED_EDGE('',*,*,#16016,.F.);
#22528=ORIENTED_EDGE('',*,*,#16017,.T.);
#22529=ORIENTED_EDGE('',*,*,#16013,.T.);
#22530=ORIENTED_EDGE('',*,*,#16018,.F.);
#22531=ORIENTED_EDGE('',*,*,#16019,.F.);
#22532=ORIENTED_EDGE('',*,*,#16020,.T.);
#22533=ORIENTED_EDGE('',*,*,#16016,.T.);
#22534=ORIENTED_EDGE('',*,*,#16021,.F.);
#22535=ORIENTED_EDGE('',*,*,#16022,.F.);
#22536=ORIENTED_EDGE('',*,*,#16023,.T.);
#22537=ORIENTED_EDGE('',*,*,#16019,.T.);
#22538=ORIENTED_EDGE('',*,*,#16024,.F.);
#22539=ORIENTED_EDGE('',*,*,#16025,.F.);
#22540=ORIENTED_EDGE('',*,*,#16026,.T.);
#22541=ORIENTED_EDGE('',*,*,#16022,.T.);
#22542=ORIENTED_EDGE('',*,*,#16027,.F.);
#22543=ORIENTED_EDGE('',*,*,#16028,.F.);
#22544=ORIENTED_EDGE('',*,*,#16029,.T.);
#22545=ORIENTED_EDGE('',*,*,#16025,.T.);
#22546=ORIENTED_EDGE('',*,*,#16030,.F.);
#22547=ORIENTED_EDGE('',*,*,#16031,.F.);
#22548=ORIENTED_EDGE('',*,*,#16032,.T.);
#22549=ORIENTED_EDGE('',*,*,#16028,.T.);
#22550=ORIENTED_EDGE('',*,*,#16033,.F.);
#22551=ORIENTED_EDGE('',*,*,#16034,.F.);
#22552=ORIENTED_EDGE('',*,*,#16035,.T.);
#22553=ORIENTED_EDGE('',*,*,#16031,.T.);
#22554=ORIENTED_EDGE('',*,*,#16036,.F.);
#22555=ORIENTED_EDGE('',*,*,#16037,.F.);
#22556=ORIENTED_EDGE('',*,*,#16038,.T.);
#22557=ORIENTED_EDGE('',*,*,#16034,.T.);
#22558=ORIENTED_EDGE('',*,*,#16039,.F.);
#22559=ORIENTED_EDGE('',*,*,#16040,.F.);
#22560=ORIENTED_EDGE('',*,*,#16041,.T.);
#22561=ORIENTED_EDGE('',*,*,#16037,.T.);
#22562=ORIENTED_EDGE('',*,*,#16042,.F.);
#22563=ORIENTED_EDGE('',*,*,#16043,.F.);
#22564=ORIENTED_EDGE('',*,*,#16044,.T.);
#22565=ORIENTED_EDGE('',*,*,#16040,.T.);
#22566=ORIENTED_EDGE('',*,*,#16045,.F.);
#22567=ORIENTED_EDGE('',*,*,#16046,.F.);
#22568=ORIENTED_EDGE('',*,*,#16047,.T.);
#22569=ORIENTED_EDGE('',*,*,#16043,.T.);
#22570=ORIENTED_EDGE('',*,*,#16048,.F.);
#22571=ORIENTED_EDGE('',*,*,#16049,.F.);
#22572=ORIENTED_EDGE('',*,*,#16050,.T.);
#22573=ORIENTED_EDGE('',*,*,#16046,.T.);
#22574=ORIENTED_EDGE('',*,*,#16051,.F.);
#22575=ORIENTED_EDGE('',*,*,#16052,.F.);
#22576=ORIENTED_EDGE('',*,*,#16053,.T.);
#22577=ORIENTED_EDGE('',*,*,#16049,.T.);
#22578=ORIENTED_EDGE('',*,*,#16054,.F.);
#22579=ORIENTED_EDGE('',*,*,#16055,.F.);
#22580=ORIENTED_EDGE('',*,*,#16056,.T.);
#22581=ORIENTED_EDGE('',*,*,#16052,.T.);
#22582=ORIENTED_EDGE('',*,*,#16057,.F.);
#22583=ORIENTED_EDGE('',*,*,#16058,.F.);
#22584=ORIENTED_EDGE('',*,*,#16059,.T.);
#22585=ORIENTED_EDGE('',*,*,#16055,.T.);
#22586=ORIENTED_EDGE('',*,*,#16060,.F.);
#22587=ORIENTED_EDGE('',*,*,#16061,.F.);
#22588=ORIENTED_EDGE('',*,*,#16062,.T.);
#22589=ORIENTED_EDGE('',*,*,#16058,.T.);
#22590=ORIENTED_EDGE('',*,*,#16063,.F.);
#22591=ORIENTED_EDGE('',*,*,#16064,.F.);
#22592=ORIENTED_EDGE('',*,*,#16065,.T.);
#22593=ORIENTED_EDGE('',*,*,#16061,.T.);
#22594=ORIENTED_EDGE('',*,*,#16066,.F.);
#22595=ORIENTED_EDGE('',*,*,#16067,.F.);
#22596=ORIENTED_EDGE('',*,*,#16068,.F.);
#22597=ORIENTED_EDGE('',*,*,#15999,.F.);
#22598=ORIENTED_EDGE('',*,*,#15996,.F.);
#22599=ORIENTED_EDGE('',*,*,#15993,.F.);
#22600=ORIENTED_EDGE('',*,*,#15990,.F.);
#22601=ORIENTED_EDGE('',*,*,#15987,.F.);
#22602=ORIENTED_EDGE('',*,*,#15984,.F.);
#22603=ORIENTED_EDGE('',*,*,#15981,.F.);
#22604=ORIENTED_EDGE('',*,*,#15978,.F.);
#22605=ORIENTED_EDGE('',*,*,#15975,.F.);
#22606=ORIENTED_EDGE('',*,*,#15972,.F.);
#22607=ORIENTED_EDGE('',*,*,#15969,.F.);
#22608=ORIENTED_EDGE('',*,*,#15966,.F.);
#22609=ORIENTED_EDGE('',*,*,#15963,.F.);
#22610=ORIENTED_EDGE('',*,*,#15960,.F.);
#22611=ORIENTED_EDGE('',*,*,#15957,.F.);
#22612=ORIENTED_EDGE('',*,*,#15954,.F.);
#22613=ORIENTED_EDGE('',*,*,#15951,.F.);
#22614=ORIENTED_EDGE('',*,*,#15948,.F.);
#22615=ORIENTED_EDGE('',*,*,#15945,.F.);
#22616=ORIENTED_EDGE('',*,*,#15942,.F.);
#22617=ORIENTED_EDGE('',*,*,#15939,.F.);
#22618=ORIENTED_EDGE('',*,*,#15936,.F.);
#22619=ORIENTED_EDGE('',*,*,#15933,.F.);
#22620=ORIENTED_EDGE('',*,*,#16069,.F.);
#22621=ORIENTED_EDGE('',*,*,#16070,.T.);
#22622=ORIENTED_EDGE('',*,*,#16066,.T.);
#22623=ORIENTED_EDGE('',*,*,#16063,.T.);
#22624=ORIENTED_EDGE('',*,*,#16060,.T.);
#22625=ORIENTED_EDGE('',*,*,#16057,.T.);
#22626=ORIENTED_EDGE('',*,*,#16054,.T.);
#22627=ORIENTED_EDGE('',*,*,#16051,.T.);
#22628=ORIENTED_EDGE('',*,*,#16048,.T.);
#22629=ORIENTED_EDGE('',*,*,#16045,.T.);
#22630=ORIENTED_EDGE('',*,*,#16042,.T.);
#22631=ORIENTED_EDGE('',*,*,#16039,.T.);
#22632=ORIENTED_EDGE('',*,*,#16036,.T.);
#22633=ORIENTED_EDGE('',*,*,#16033,.T.);
#22634=ORIENTED_EDGE('',*,*,#16030,.T.);
#22635=ORIENTED_EDGE('',*,*,#16027,.T.);
#22636=ORIENTED_EDGE('',*,*,#16024,.T.);
#22637=ORIENTED_EDGE('',*,*,#16021,.T.);
#22638=ORIENTED_EDGE('',*,*,#16018,.T.);
#22639=ORIENTED_EDGE('',*,*,#16015,.T.);
#22640=ORIENTED_EDGE('',*,*,#16012,.T.);
#22641=ORIENTED_EDGE('',*,*,#16009,.T.);
#22642=ORIENTED_EDGE('',*,*,#16006,.T.);
#22643=ORIENTED_EDGE('',*,*,#16003,.T.);
#22644=ORIENTED_EDGE('',*,*,#16071,.T.);
#22645=ORIENTED_EDGE('',*,*,#16072,.T.);
#22646=ORIENTED_EDGE('',*,*,#16073,.T.);
#22647=ORIENTED_EDGE('',*,*,#16074,.T.);
#22648=ORIENTED_EDGE('',*,*,#16069,.T.);
#22649=ORIENTED_EDGE('',*,*,#16064,.T.);
#22650=ORIENTED_EDGE('',*,*,#16070,.F.);
#22651=ORIENTED_EDGE('',*,*,#16074,.F.);
#22652=ORIENTED_EDGE('',*,*,#16075,.T.);
#22653=ORIENTED_EDGE('',*,*,#16076,.F.);
#22654=ORIENTED_EDGE('',*,*,#16001,.F.);
#22655=ORIENTED_EDGE('',*,*,#16005,.F.);
#22656=ORIENTED_EDGE('',*,*,#16008,.F.);
#22657=ORIENTED_EDGE('',*,*,#16011,.F.);
#22658=ORIENTED_EDGE('',*,*,#16014,.F.);
#22659=ORIENTED_EDGE('',*,*,#16017,.F.);
#22660=ORIENTED_EDGE('',*,*,#16020,.F.);
#22661=ORIENTED_EDGE('',*,*,#16023,.F.);
#22662=ORIENTED_EDGE('',*,*,#16026,.F.);
#22663=ORIENTED_EDGE('',*,*,#16029,.F.);
#22664=ORIENTED_EDGE('',*,*,#16032,.F.);
#22665=ORIENTED_EDGE('',*,*,#16035,.F.);
#22666=ORIENTED_EDGE('',*,*,#16038,.F.);
#22667=ORIENTED_EDGE('',*,*,#16041,.F.);
#22668=ORIENTED_EDGE('',*,*,#16044,.F.);
#22669=ORIENTED_EDGE('',*,*,#16047,.F.);
#22670=ORIENTED_EDGE('',*,*,#16050,.F.);
#22671=ORIENTED_EDGE('',*,*,#16053,.F.);
#22672=ORIENTED_EDGE('',*,*,#16056,.F.);
#22673=ORIENTED_EDGE('',*,*,#16059,.F.);
#22674=ORIENTED_EDGE('',*,*,#16062,.F.);
#22675=ORIENTED_EDGE('',*,*,#16065,.F.);
#22676=ORIENTED_EDGE('',*,*,#16075,.F.);
#22677=ORIENTED_EDGE('',*,*,#16073,.F.);
#22678=ORIENTED_EDGE('',*,*,#15931,.F.);
#22679=ORIENTED_EDGE('',*,*,#15935,.F.);
#22680=ORIENTED_EDGE('',*,*,#15938,.F.);
#22681=ORIENTED_EDGE('',*,*,#15941,.F.);
#22682=ORIENTED_EDGE('',*,*,#15944,.F.);
#22683=ORIENTED_EDGE('',*,*,#15947,.F.);
#22684=ORIENTED_EDGE('',*,*,#15950,.F.);
#22685=ORIENTED_EDGE('',*,*,#15953,.F.);
#22686=ORIENTED_EDGE('',*,*,#15956,.F.);
#22687=ORIENTED_EDGE('',*,*,#15959,.F.);
#22688=ORIENTED_EDGE('',*,*,#15962,.F.);
#22689=ORIENTED_EDGE('',*,*,#15965,.F.);
#22690=ORIENTED_EDGE('',*,*,#15968,.F.);
#22691=ORIENTED_EDGE('',*,*,#15971,.F.);
#22692=ORIENTED_EDGE('',*,*,#15974,.F.);
#22693=ORIENTED_EDGE('',*,*,#15977,.F.);
#22694=ORIENTED_EDGE('',*,*,#15980,.F.);
#22695=ORIENTED_EDGE('',*,*,#15983,.F.);
#22696=ORIENTED_EDGE('',*,*,#15986,.F.);
#22697=ORIENTED_EDGE('',*,*,#15989,.F.);
#22698=ORIENTED_EDGE('',*,*,#15992,.F.);
#22699=ORIENTED_EDGE('',*,*,#15995,.F.);
#22700=ORIENTED_EDGE('',*,*,#15998,.F.);
#22701=ORIENTED_EDGE('',*,*,#16077,.F.);
#22702=ORIENTED_EDGE('',*,*,#16078,.F.);
#22703=ORIENTED_EDGE('',*,*,#16079,.F.);
#22704=ORIENTED_EDGE('',*,*,#16080,.F.);
#22705=ORIENTED_EDGE('',*,*,#16081,.F.);
#22706=ORIENTED_EDGE('',*,*,#16082,.F.);
#22707=ORIENTED_EDGE('',*,*,#16083,.T.);
#22708=ORIENTED_EDGE('',*,*,#16084,.F.);
#22709=ORIENTED_EDGE('',*,*,#16083,.F.);
#22710=ORIENTED_EDGE('',*,*,#16085,.F.);
#22711=ORIENTED_EDGE('',*,*,#16086,.F.);
#22712=ORIENTED_EDGE('',*,*,#16081,.T.);
#22713=ORIENTED_EDGE('',*,*,#16087,.F.);
#22714=ORIENTED_EDGE('',*,*,#16088,.T.);
#22715=ORIENTED_EDGE('',*,*,#16089,.T.);
#22716=ORIENTED_EDGE('',*,*,#16080,.T.);
#22717=ORIENTED_EDGE('',*,*,#16090,.F.);
#22718=ORIENTED_EDGE('',*,*,#16091,.T.);
#22719=ORIENTED_EDGE('',*,*,#16087,.T.);
#22720=ORIENTED_EDGE('',*,*,#16079,.T.);
#22721=ORIENTED_EDGE('',*,*,#16092,.F.);
#22722=ORIENTED_EDGE('',*,*,#16093,.T.);
#22723=ORIENTED_EDGE('',*,*,#16090,.T.);
#22724=ORIENTED_EDGE('',*,*,#16093,.F.);
#22725=ORIENTED_EDGE('',*,*,#16094,.F.);
#22726=ORIENTED_EDGE('',*,*,#16095,.F.);
#22727=ORIENTED_EDGE('',*,*,#16096,.F.);
#22728=ORIENTED_EDGE('',*,*,#16088,.F.);
#22729=ORIENTED_EDGE('',*,*,#16091,.F.);
#22730=ORIENTED_EDGE('',*,*,#16097,.T.);
#22731=ORIENTED_EDGE('',*,*,#16078,.T.);
#22732=ORIENTED_EDGE('',*,*,#16098,.F.);
#22733=ORIENTED_EDGE('',*,*,#16094,.T.);
#22734=ORIENTED_EDGE('',*,*,#16092,.T.);
#22735=ORIENTED_EDGE('',*,*,#16086,.T.);
#22736=ORIENTED_EDGE('',*,*,#16099,.F.);
#22737=ORIENTED_EDGE('',*,*,#16095,.T.);
#22738=ORIENTED_EDGE('',*,*,#16098,.T.);
#22739=ORIENTED_EDGE('',*,*,#16085,.T.);
#22740=ORIENTED_EDGE('',*,*,#16082,.T.);
#22741=ORIENTED_EDGE('',*,*,#16089,.F.);
#22742=ORIENTED_EDGE('',*,*,#16096,.T.);
#22743=ORIENTED_EDGE('',*,*,#16099,.T.);
#22744=ORIENTED_EDGE('',*,*,#16084,.T.);
#22745=ORIENTED_EDGE('',*,*,#16100,.F.);
#22746=ORIENTED_EDGE('',*,*,#16071,.F.);
#22747=ORIENTED_EDGE('',*,*,#15932,.F.);
#22748=ORIENTED_EDGE('',*,*,#16072,.F.);
#22749=ORIENTED_EDGE('',*,*,#16101,.T.);
#22750=ORIENTED_EDGE('',*,*,#16100,.T.);
#22751=ORIENTED_EDGE('',*,*,#16101,.F.);
#22752=ORIENTED_EDGE('',*,*,#15997,.T.);
#22753=ORIENTED_EDGE('',*,*,#16068,.T.);
#22754=ORIENTED_EDGE('',*,*,#16102,.F.);
#22755=ORIENTED_EDGE('',*,*,#16077,.T.);
#22756=ORIENTED_EDGE('',*,*,#16103,.F.);
#22757=ORIENTED_EDGE('',*,*,#16102,.T.);
#22758=ORIENTED_EDGE('',*,*,#16067,.T.);
#22759=ORIENTED_EDGE('',*,*,#16002,.T.);
#22760=ORIENTED_EDGE('',*,*,#16076,.T.);
#22761=ORIENTED_EDGE('',*,*,#16097,.F.);
#22762=ORIENTED_EDGE('',*,*,#16104,.T.);
#22763=ORIENTED_EDGE('',*,*,#16103,.T.);
#22764=ORIENTED_EDGE('',*,*,#16104,.F.);
#22765=ORIENTED_EDGE('',*,*,#16105,.F.);
#22766=ORIENTED_EDGE('',*,*,#16106,.T.);
#22767=ORIENTED_EDGE('',*,*,#16107,.T.);
#22768=ORIENTED_EDGE('',*,*,#16108,.T.);
#22769=ORIENTED_EDGE('',*,*,#16109,.F.);
#22770=ORIENTED_EDGE('',*,*,#16110,.T.);
#22771=ORIENTED_EDGE('',*,*,#16105,.T.);
#22772=ORIENTED_EDGE('',*,*,#16111,.T.);
#22773=ORIENTED_EDGE('',*,*,#16112,.F.);
#22774=ORIENTED_EDGE('',*,*,#16113,.T.);
#22775=ORIENTED_EDGE('',*,*,#16109,.T.);
#22776=ORIENTED_EDGE('',*,*,#16114,.T.);
#22777=ORIENTED_EDGE('',*,*,#16115,.F.);
#22778=ORIENTED_EDGE('',*,*,#16116,.T.);
#22779=ORIENTED_EDGE('',*,*,#16112,.T.);
#22780=ORIENTED_EDGE('',*,*,#16117,.T.);
#22781=ORIENTED_EDGE('',*,*,#16118,.F.);
#22782=ORIENTED_EDGE('',*,*,#16119,.T.);
#22783=ORIENTED_EDGE('',*,*,#16115,.T.);
#22784=ORIENTED_EDGE('',*,*,#16120,.T.);
#22785=ORIENTED_EDGE('',*,*,#16121,.F.);
#22786=ORIENTED_EDGE('',*,*,#16122,.T.);
#22787=ORIENTED_EDGE('',*,*,#16118,.T.);
#22788=ORIENTED_EDGE('',*,*,#16123,.T.);
#22789=ORIENTED_EDGE('',*,*,#16124,.F.);
#22790=ORIENTED_EDGE('',*,*,#16125,.T.);
#22791=ORIENTED_EDGE('',*,*,#16121,.T.);
#22792=ORIENTED_EDGE('',*,*,#16126,.T.);
#22793=ORIENTED_EDGE('',*,*,#16127,.F.);
#22794=ORIENTED_EDGE('',*,*,#16128,.T.);
#22795=ORIENTED_EDGE('',*,*,#16124,.T.);
#22796=ORIENTED_EDGE('',*,*,#16129,.T.);
#22797=ORIENTED_EDGE('',*,*,#16130,.F.);
#22798=ORIENTED_EDGE('',*,*,#16131,.T.);
#22799=ORIENTED_EDGE('',*,*,#16127,.T.);
#22800=ORIENTED_EDGE('',*,*,#16132,.T.);
#22801=ORIENTED_EDGE('',*,*,#16133,.F.);
#22802=ORIENTED_EDGE('',*,*,#16134,.T.);
#22803=ORIENTED_EDGE('',*,*,#16130,.T.);
#22804=ORIENTED_EDGE('',*,*,#16135,.T.);
#22805=ORIENTED_EDGE('',*,*,#16136,.F.);
#22806=ORIENTED_EDGE('',*,*,#16137,.T.);
#22807=ORIENTED_EDGE('',*,*,#16133,.T.);
#22808=ORIENTED_EDGE('',*,*,#16138,.T.);
#22809=ORIENTED_EDGE('',*,*,#16139,.F.);
#22810=ORIENTED_EDGE('',*,*,#16140,.T.);
#22811=ORIENTED_EDGE('',*,*,#16136,.T.);
#22812=ORIENTED_EDGE('',*,*,#16141,.T.);
#22813=ORIENTED_EDGE('',*,*,#16142,.F.);
#22814=ORIENTED_EDGE('',*,*,#16143,.T.);
#22815=ORIENTED_EDGE('',*,*,#16139,.T.);
#22816=ORIENTED_EDGE('',*,*,#16144,.T.);
#22817=ORIENTED_EDGE('',*,*,#16145,.F.);
#22818=ORIENTED_EDGE('',*,*,#16146,.T.);
#22819=ORIENTED_EDGE('',*,*,#16142,.T.);
#22820=ORIENTED_EDGE('',*,*,#16147,.T.);
#22821=ORIENTED_EDGE('',*,*,#16148,.F.);
#22822=ORIENTED_EDGE('',*,*,#16149,.T.);
#22823=ORIENTED_EDGE('',*,*,#16145,.T.);
#22824=ORIENTED_EDGE('',*,*,#16150,.T.);
#22825=ORIENTED_EDGE('',*,*,#16151,.F.);
#22826=ORIENTED_EDGE('',*,*,#16152,.T.);
#22827=ORIENTED_EDGE('',*,*,#16148,.T.);
#22828=ORIENTED_EDGE('',*,*,#16153,.T.);
#22829=ORIENTED_EDGE('',*,*,#16154,.F.);
#22830=ORIENTED_EDGE('',*,*,#16155,.T.);
#22831=ORIENTED_EDGE('',*,*,#16151,.T.);
#22832=ORIENTED_EDGE('',*,*,#16156,.T.);
#22833=ORIENTED_EDGE('',*,*,#16157,.F.);
#22834=ORIENTED_EDGE('',*,*,#16158,.T.);
#22835=ORIENTED_EDGE('',*,*,#16154,.T.);
#22836=ORIENTED_EDGE('',*,*,#16159,.T.);
#22837=ORIENTED_EDGE('',*,*,#16160,.F.);
#22838=ORIENTED_EDGE('',*,*,#16161,.T.);
#22839=ORIENTED_EDGE('',*,*,#16157,.T.);
#22840=ORIENTED_EDGE('',*,*,#16162,.T.);
#22841=ORIENTED_EDGE('',*,*,#16163,.F.);
#22842=ORIENTED_EDGE('',*,*,#16164,.T.);
#22843=ORIENTED_EDGE('',*,*,#16160,.T.);
#22844=ORIENTED_EDGE('',*,*,#16165,.T.);
#22845=ORIENTED_EDGE('',*,*,#16166,.F.);
#22846=ORIENTED_EDGE('',*,*,#16167,.T.);
#22847=ORIENTED_EDGE('',*,*,#16163,.T.);
#22848=ORIENTED_EDGE('',*,*,#16168,.T.);
#22849=ORIENTED_EDGE('',*,*,#16169,.F.);
#22850=ORIENTED_EDGE('',*,*,#16170,.T.);
#22851=ORIENTED_EDGE('',*,*,#16166,.T.);
#22852=ORIENTED_EDGE('',*,*,#16171,.T.);
#22853=ORIENTED_EDGE('',*,*,#16172,.F.);
#22854=ORIENTED_EDGE('',*,*,#16173,.T.);
#22855=ORIENTED_EDGE('',*,*,#16169,.T.);
#22856=ORIENTED_EDGE('',*,*,#16174,.T.);
#22857=ORIENTED_EDGE('',*,*,#16175,.F.);
#22858=ORIENTED_EDGE('',*,*,#16176,.T.);
#22859=ORIENTED_EDGE('',*,*,#16177,.F.);
#22860=ORIENTED_EDGE('',*,*,#16178,.F.);
#22861=ORIENTED_EDGE('',*,*,#16179,.F.);
#22862=ORIENTED_EDGE('',*,*,#16180,.T.);
#22863=ORIENTED_EDGE('',*,*,#16175,.T.);
#22864=ORIENTED_EDGE('',*,*,#16181,.F.);
#22865=ORIENTED_EDGE('',*,*,#16182,.F.);
#22866=ORIENTED_EDGE('',*,*,#16183,.T.);
#22867=ORIENTED_EDGE('',*,*,#16179,.T.);
#22868=ORIENTED_EDGE('',*,*,#16184,.F.);
#22869=ORIENTED_EDGE('',*,*,#16185,.F.);
#22870=ORIENTED_EDGE('',*,*,#16186,.T.);
#22871=ORIENTED_EDGE('',*,*,#16182,.T.);
#22872=ORIENTED_EDGE('',*,*,#16187,.F.);
#22873=ORIENTED_EDGE('',*,*,#16188,.F.);
#22874=ORIENTED_EDGE('',*,*,#16189,.T.);
#22875=ORIENTED_EDGE('',*,*,#16185,.T.);
#22876=ORIENTED_EDGE('',*,*,#16190,.F.);
#22877=ORIENTED_EDGE('',*,*,#16191,.F.);
#22878=ORIENTED_EDGE('',*,*,#16192,.T.);
#22879=ORIENTED_EDGE('',*,*,#16188,.T.);
#22880=ORIENTED_EDGE('',*,*,#16193,.F.);
#22881=ORIENTED_EDGE('',*,*,#16194,.F.);
#22882=ORIENTED_EDGE('',*,*,#16195,.T.);
#22883=ORIENTED_EDGE('',*,*,#16191,.T.);
#22884=ORIENTED_EDGE('',*,*,#16196,.F.);
#22885=ORIENTED_EDGE('',*,*,#16197,.F.);
#22886=ORIENTED_EDGE('',*,*,#16198,.T.);
#22887=ORIENTED_EDGE('',*,*,#16194,.T.);
#22888=ORIENTED_EDGE('',*,*,#16199,.F.);
#22889=ORIENTED_EDGE('',*,*,#16200,.F.);
#22890=ORIENTED_EDGE('',*,*,#16201,.T.);
#22891=ORIENTED_EDGE('',*,*,#16197,.T.);
#22892=ORIENTED_EDGE('',*,*,#16202,.F.);
#22893=ORIENTED_EDGE('',*,*,#16203,.F.);
#22894=ORIENTED_EDGE('',*,*,#16204,.T.);
#22895=ORIENTED_EDGE('',*,*,#16200,.T.);
#22896=ORIENTED_EDGE('',*,*,#16205,.F.);
#22897=ORIENTED_EDGE('',*,*,#16206,.F.);
#22898=ORIENTED_EDGE('',*,*,#16207,.T.);
#22899=ORIENTED_EDGE('',*,*,#16203,.T.);
#22900=ORIENTED_EDGE('',*,*,#16208,.F.);
#22901=ORIENTED_EDGE('',*,*,#16209,.F.);
#22902=ORIENTED_EDGE('',*,*,#16210,.T.);
#22903=ORIENTED_EDGE('',*,*,#16206,.T.);
#22904=ORIENTED_EDGE('',*,*,#16211,.F.);
#22905=ORIENTED_EDGE('',*,*,#16212,.F.);
#22906=ORIENTED_EDGE('',*,*,#16213,.T.);
#22907=ORIENTED_EDGE('',*,*,#16209,.T.);
#22908=ORIENTED_EDGE('',*,*,#16214,.F.);
#22909=ORIENTED_EDGE('',*,*,#16215,.F.);
#22910=ORIENTED_EDGE('',*,*,#16216,.T.);
#22911=ORIENTED_EDGE('',*,*,#16212,.T.);
#22912=ORIENTED_EDGE('',*,*,#16217,.F.);
#22913=ORIENTED_EDGE('',*,*,#16218,.F.);
#22914=ORIENTED_EDGE('',*,*,#16219,.T.);
#22915=ORIENTED_EDGE('',*,*,#16215,.T.);
#22916=ORIENTED_EDGE('',*,*,#16220,.F.);
#22917=ORIENTED_EDGE('',*,*,#16221,.F.);
#22918=ORIENTED_EDGE('',*,*,#16222,.T.);
#22919=ORIENTED_EDGE('',*,*,#16218,.T.);
#22920=ORIENTED_EDGE('',*,*,#16223,.F.);
#22921=ORIENTED_EDGE('',*,*,#16224,.F.);
#22922=ORIENTED_EDGE('',*,*,#16225,.T.);
#22923=ORIENTED_EDGE('',*,*,#16221,.T.);
#22924=ORIENTED_EDGE('',*,*,#16226,.F.);
#22925=ORIENTED_EDGE('',*,*,#16227,.F.);
#22926=ORIENTED_EDGE('',*,*,#16228,.T.);
#22927=ORIENTED_EDGE('',*,*,#16224,.T.);
#22928=ORIENTED_EDGE('',*,*,#16229,.F.);
#22929=ORIENTED_EDGE('',*,*,#16230,.F.);
#22930=ORIENTED_EDGE('',*,*,#16231,.T.);
#22931=ORIENTED_EDGE('',*,*,#16227,.T.);
#22932=ORIENTED_EDGE('',*,*,#16232,.F.);
#22933=ORIENTED_EDGE('',*,*,#16233,.F.);
#22934=ORIENTED_EDGE('',*,*,#16234,.T.);
#22935=ORIENTED_EDGE('',*,*,#16230,.T.);
#22936=ORIENTED_EDGE('',*,*,#16235,.F.);
#22937=ORIENTED_EDGE('',*,*,#16236,.F.);
#22938=ORIENTED_EDGE('',*,*,#16237,.T.);
#22939=ORIENTED_EDGE('',*,*,#16233,.T.);
#22940=ORIENTED_EDGE('',*,*,#16238,.F.);
#22941=ORIENTED_EDGE('',*,*,#16239,.F.);
#22942=ORIENTED_EDGE('',*,*,#16240,.T.);
#22943=ORIENTED_EDGE('',*,*,#16236,.T.);
#22944=ORIENTED_EDGE('',*,*,#16241,.F.);
#22945=ORIENTED_EDGE('',*,*,#16242,.F.);
#22946=ORIENTED_EDGE('',*,*,#16243,.T.);
#22947=ORIENTED_EDGE('',*,*,#16239,.T.);
#22948=ORIENTED_EDGE('',*,*,#16244,.F.);
#22949=ORIENTED_EDGE('',*,*,#16177,.T.);
#22950=ORIENTED_EDGE('',*,*,#16245,.T.);
#22951=ORIENTED_EDGE('',*,*,#16246,.F.);
#22952=ORIENTED_EDGE('',*,*,#16247,.F.);
#22953=ORIENTED_EDGE('',*,*,#16248,.T.);
#22954=ORIENTED_EDGE('',*,*,#16248,.F.);
#22955=ORIENTED_EDGE('',*,*,#16249,.F.);
#22956=ORIENTED_EDGE('',*,*,#16174,.F.);
#22957=ORIENTED_EDGE('',*,*,#16171,.F.);
#22958=ORIENTED_EDGE('',*,*,#16168,.F.);
#22959=ORIENTED_EDGE('',*,*,#16165,.F.);
#22960=ORIENTED_EDGE('',*,*,#16162,.F.);
#22961=ORIENTED_EDGE('',*,*,#16159,.F.);
#22962=ORIENTED_EDGE('',*,*,#16156,.F.);
#22963=ORIENTED_EDGE('',*,*,#16153,.F.);
#22964=ORIENTED_EDGE('',*,*,#16150,.F.);
#22965=ORIENTED_EDGE('',*,*,#16147,.F.);
#22966=ORIENTED_EDGE('',*,*,#16144,.F.);
#22967=ORIENTED_EDGE('',*,*,#16141,.F.);
#22968=ORIENTED_EDGE('',*,*,#16138,.F.);
#22969=ORIENTED_EDGE('',*,*,#16135,.F.);
#22970=ORIENTED_EDGE('',*,*,#16132,.F.);
#22971=ORIENTED_EDGE('',*,*,#16129,.F.);
#22972=ORIENTED_EDGE('',*,*,#16126,.F.);
#22973=ORIENTED_EDGE('',*,*,#16123,.F.);
#22974=ORIENTED_EDGE('',*,*,#16120,.F.);
#22975=ORIENTED_EDGE('',*,*,#16117,.F.);
#22976=ORIENTED_EDGE('',*,*,#16114,.F.);
#22977=ORIENTED_EDGE('',*,*,#16111,.F.);
#22978=ORIENTED_EDGE('',*,*,#16108,.F.);
#22979=ORIENTED_EDGE('',*,*,#16250,.F.);
#22980=ORIENTED_EDGE('',*,*,#16251,.T.);
#22981=ORIENTED_EDGE('',*,*,#16244,.T.);
#22982=ORIENTED_EDGE('',*,*,#16241,.T.);
#22983=ORIENTED_EDGE('',*,*,#16238,.T.);
#22984=ORIENTED_EDGE('',*,*,#16235,.T.);
#22985=ORIENTED_EDGE('',*,*,#16232,.T.);
#22986=ORIENTED_EDGE('',*,*,#16229,.T.);
#22987=ORIENTED_EDGE('',*,*,#16226,.T.);
#22988=ORIENTED_EDGE('',*,*,#16223,.T.);
#22989=ORIENTED_EDGE('',*,*,#16220,.T.);
#22990=ORIENTED_EDGE('',*,*,#16217,.T.);
#22991=ORIENTED_EDGE('',*,*,#16214,.T.);
#22992=ORIENTED_EDGE('',*,*,#16211,.T.);
#22993=ORIENTED_EDGE('',*,*,#16208,.T.);
#22994=ORIENTED_EDGE('',*,*,#16205,.T.);
#22995=ORIENTED_EDGE('',*,*,#16202,.T.);
#22996=ORIENTED_EDGE('',*,*,#16199,.T.);
#22997=ORIENTED_EDGE('',*,*,#16196,.T.);
#22998=ORIENTED_EDGE('',*,*,#16193,.T.);
#22999=ORIENTED_EDGE('',*,*,#16190,.T.);
#23000=ORIENTED_EDGE('',*,*,#16187,.T.);
#23001=ORIENTED_EDGE('',*,*,#16184,.T.);
#23002=ORIENTED_EDGE('',*,*,#16181,.T.);
#23003=ORIENTED_EDGE('',*,*,#16178,.T.);
#23004=ORIENTED_EDGE('',*,*,#16252,.T.);
#23005=ORIENTED_EDGE('',*,*,#16253,.T.);
#23006=ORIENTED_EDGE('',*,*,#16254,.T.);
#23007=ORIENTED_EDGE('',*,*,#16255,.T.);
#23008=ORIENTED_EDGE('',*,*,#16250,.T.);
#23009=ORIENTED_EDGE('',*,*,#16242,.T.);
#23010=ORIENTED_EDGE('',*,*,#16251,.F.);
#23011=ORIENTED_EDGE('',*,*,#16255,.F.);
#23012=ORIENTED_EDGE('',*,*,#16256,.T.);
#23013=ORIENTED_EDGE('',*,*,#16245,.F.);
#23014=ORIENTED_EDGE('',*,*,#16176,.F.);
#23015=ORIENTED_EDGE('',*,*,#16180,.F.);
#23016=ORIENTED_EDGE('',*,*,#16183,.F.);
#23017=ORIENTED_EDGE('',*,*,#16186,.F.);
#23018=ORIENTED_EDGE('',*,*,#16189,.F.);
#23019=ORIENTED_EDGE('',*,*,#16192,.F.);
#23020=ORIENTED_EDGE('',*,*,#16195,.F.);
#23021=ORIENTED_EDGE('',*,*,#16198,.F.);
#23022=ORIENTED_EDGE('',*,*,#16201,.F.);
#23023=ORIENTED_EDGE('',*,*,#16204,.F.);
#23024=ORIENTED_EDGE('',*,*,#16207,.F.);
#23025=ORIENTED_EDGE('',*,*,#16210,.F.);
#23026=ORIENTED_EDGE('',*,*,#16213,.F.);
#23027=ORIENTED_EDGE('',*,*,#16216,.F.);
#23028=ORIENTED_EDGE('',*,*,#16219,.F.);
#23029=ORIENTED_EDGE('',*,*,#16222,.F.);
#23030=ORIENTED_EDGE('',*,*,#16225,.F.);
#23031=ORIENTED_EDGE('',*,*,#16228,.F.);
#23032=ORIENTED_EDGE('',*,*,#16231,.F.);
#23033=ORIENTED_EDGE('',*,*,#16234,.F.);
#23034=ORIENTED_EDGE('',*,*,#16237,.F.);
#23035=ORIENTED_EDGE('',*,*,#16240,.F.);
#23036=ORIENTED_EDGE('',*,*,#16243,.F.);
#23037=ORIENTED_EDGE('',*,*,#16256,.F.);
#23038=ORIENTED_EDGE('',*,*,#16254,.F.);
#23039=ORIENTED_EDGE('',*,*,#16106,.F.);
#23040=ORIENTED_EDGE('',*,*,#16110,.F.);
#23041=ORIENTED_EDGE('',*,*,#16113,.F.);
#23042=ORIENTED_EDGE('',*,*,#16116,.F.);
#23043=ORIENTED_EDGE('',*,*,#16119,.F.);
#23044=ORIENTED_EDGE('',*,*,#16122,.F.);
#23045=ORIENTED_EDGE('',*,*,#16125,.F.);
#23046=ORIENTED_EDGE('',*,*,#16128,.F.);
#23047=ORIENTED_EDGE('',*,*,#16131,.F.);
#23048=ORIENTED_EDGE('',*,*,#16134,.F.);
#23049=ORIENTED_EDGE('',*,*,#16137,.F.);
#23050=ORIENTED_EDGE('',*,*,#16140,.F.);
#23051=ORIENTED_EDGE('',*,*,#16143,.F.);
#23052=ORIENTED_EDGE('',*,*,#16146,.F.);
#23053=ORIENTED_EDGE('',*,*,#16149,.F.);
#23054=ORIENTED_EDGE('',*,*,#16152,.F.);
#23055=ORIENTED_EDGE('',*,*,#16155,.F.);
#23056=ORIENTED_EDGE('',*,*,#16158,.F.);
#23057=ORIENTED_EDGE('',*,*,#16161,.F.);
#23058=ORIENTED_EDGE('',*,*,#16164,.F.);
#23059=ORIENTED_EDGE('',*,*,#16167,.F.);
#23060=ORIENTED_EDGE('',*,*,#16170,.F.);
#23061=ORIENTED_EDGE('',*,*,#16173,.F.);
#23062=ORIENTED_EDGE('',*,*,#16257,.F.);
#23063=ORIENTED_EDGE('',*,*,#16247,.T.);
#23064=ORIENTED_EDGE('',*,*,#16258,.T.);
#23065=ORIENTED_EDGE('',*,*,#16259,.T.);
#23066=ORIENTED_EDGE('',*,*,#16258,.F.);
#23067=ORIENTED_EDGE('',*,*,#16246,.T.);
#23068=ORIENTED_EDGE('',*,*,#16260,.T.);
#23069=ORIENTED_EDGE('',*,*,#16172,.T.);
#23070=ORIENTED_EDGE('',*,*,#16249,.T.);
#23071=ORIENTED_EDGE('',*,*,#16260,.F.);
#23072=ORIENTED_EDGE('',*,*,#16257,.T.);
#23073=ORIENTED_EDGE('',*,*,#16261,.F.);
#23074=ORIENTED_EDGE('',*,*,#16259,.F.);
#23075=ORIENTED_EDGE('',*,*,#16262,.F.);
#23076=ORIENTED_EDGE('',*,*,#16263,.F.);
#23077=ORIENTED_EDGE('',*,*,#16264,.F.);
#23078=ORIENTED_EDGE('',*,*,#16265,.F.);
#23079=ORIENTED_EDGE('',*,*,#16266,.F.);
#23080=ORIENTED_EDGE('',*,*,#16267,.F.);
#23081=ORIENTED_EDGE('',*,*,#16268,.F.);
#23082=ORIENTED_EDGE('',*,*,#16269,.F.);
#23083=ORIENTED_EDGE('',*,*,#16270,.F.);
#23084=ORIENTED_EDGE('',*,*,#16271,.F.);
#23085=ORIENTED_EDGE('',*,*,#16272,.F.);
#23086=ORIENTED_EDGE('',*,*,#16273,.F.);
#23087=ORIENTED_EDGE('',*,*,#16274,.T.);
#23088=ORIENTED_EDGE('',*,*,#16269,.T.);
#23089=ORIENTED_EDGE('',*,*,#16267,.T.);
#23090=ORIENTED_EDGE('',*,*,#16265,.T.);
#23091=ORIENTED_EDGE('',*,*,#16263,.T.);
#23092=ORIENTED_EDGE('',*,*,#16273,.T.);
#23093=ORIENTED_EDGE('',*,*,#16271,.T.);
#23094=ORIENTED_EDGE('',*,*,#16274,.F.);
#23095=ORIENTED_EDGE('',*,*,#16275,.F.);
#23096=ORIENTED_EDGE('',*,*,#16276,.T.);
#23097=ORIENTED_EDGE('',*,*,#16262,.T.);
#23098=ORIENTED_EDGE('',*,*,#16277,.F.);
#23099=ORIENTED_EDGE('',*,*,#16278,.F.);
#23100=ORIENTED_EDGE('',*,*,#16279,.T.);
#23101=ORIENTED_EDGE('',*,*,#16272,.T.);
#23102=ORIENTED_EDGE('',*,*,#16276,.F.);
#23103=ORIENTED_EDGE('',*,*,#16280,.F.);
#23104=ORIENTED_EDGE('',*,*,#16281,.T.);
#23105=ORIENTED_EDGE('',*,*,#16270,.T.);
#23106=ORIENTED_EDGE('',*,*,#16279,.F.);
#23107=ORIENTED_EDGE('',*,*,#16282,.F.);
#23108=ORIENTED_EDGE('',*,*,#16283,.T.);
#23109=ORIENTED_EDGE('',*,*,#16268,.T.);
#23110=ORIENTED_EDGE('',*,*,#16281,.F.);
#23111=ORIENTED_EDGE('',*,*,#16284,.F.);
#23112=ORIENTED_EDGE('',*,*,#16285,.T.);
#23113=ORIENTED_EDGE('',*,*,#16266,.T.);
#23114=ORIENTED_EDGE('',*,*,#16283,.F.);
#23115=ORIENTED_EDGE('',*,*,#16286,.F.);
#23116=ORIENTED_EDGE('',*,*,#16277,.T.);
#23117=ORIENTED_EDGE('',*,*,#16264,.T.);
#23118=ORIENTED_EDGE('',*,*,#16285,.F.);
#23119=ORIENTED_EDGE('',*,*,#16287,.F.);
#23120=ORIENTED_EDGE('',*,*,#16288,.T.);
#23121=ORIENTED_EDGE('',*,*,#16289,.F.);
#23122=ORIENTED_EDGE('',*,*,#16290,.F.);
#23123=ORIENTED_EDGE('',*,*,#16291,.F.);
#23124=ORIENTED_EDGE('',*,*,#16290,.T.);
#23125=ORIENTED_EDGE('',*,*,#16292,.T.);
#23126=ORIENTED_EDGE('',*,*,#16293,.F.);
#23127=ORIENTED_EDGE('',*,*,#16292,.F.);
#23128=ORIENTED_EDGE('',*,*,#16289,.T.);
#23129=ORIENTED_EDGE('',*,*,#16294,.T.);
#23130=ORIENTED_EDGE('',*,*,#16295,.F.);
#23131=ORIENTED_EDGE('',*,*,#16294,.F.);
#23132=ORIENTED_EDGE('',*,*,#16288,.F.);
#23133=ORIENTED_EDGE('',*,*,#16296,.F.);
#23134=ORIENTED_EDGE('',*,*,#16297,.T.);
#23135=ORIENTED_EDGE('',*,*,#16298,.F.);
#23136=ORIENTED_EDGE('',*,*,#16299,.F.);
#23137=ORIENTED_EDGE('',*,*,#16300,.F.);
#23138=ORIENTED_EDGE('',*,*,#16299,.T.);
#23139=ORIENTED_EDGE('',*,*,#16301,.T.);
#23140=ORIENTED_EDGE('',*,*,#16302,.F.);
#23141=ORIENTED_EDGE('',*,*,#16301,.F.);
#23142=ORIENTED_EDGE('',*,*,#16298,.T.);
#23143=ORIENTED_EDGE('',*,*,#16303,.T.);
#23144=ORIENTED_EDGE('',*,*,#16304,.F.);
#23145=ORIENTED_EDGE('',*,*,#16303,.F.);
#23146=ORIENTED_EDGE('',*,*,#16297,.F.);
#23147=ORIENTED_EDGE('',*,*,#16305,.F.);
#23148=ORIENTED_EDGE('',*,*,#16306,.T.);
#23149=ORIENTED_EDGE('',*,*,#16307,.F.);
#23150=ORIENTED_EDGE('',*,*,#16308,.F.);
#23151=ORIENTED_EDGE('',*,*,#16309,.F.);
#23152=ORIENTED_EDGE('',*,*,#16308,.T.);
#23153=ORIENTED_EDGE('',*,*,#16310,.T.);
#23154=ORIENTED_EDGE('',*,*,#16311,.F.);
#23155=ORIENTED_EDGE('',*,*,#16310,.F.);
#23156=ORIENTED_EDGE('',*,*,#16307,.T.);
#23157=ORIENTED_EDGE('',*,*,#16312,.T.);
#23158=ORIENTED_EDGE('',*,*,#16313,.F.);
#23159=ORIENTED_EDGE('',*,*,#16312,.F.);
#23160=ORIENTED_EDGE('',*,*,#16306,.F.);
#23161=ORIENTED_EDGE('',*,*,#16314,.F.);
#23162=ORIENTED_EDGE('',*,*,#16315,.T.);
#23163=ORIENTED_EDGE('',*,*,#16316,.F.);
#23164=ORIENTED_EDGE('',*,*,#16317,.F.);
#23165=ORIENTED_EDGE('',*,*,#16318,.F.);
#23166=ORIENTED_EDGE('',*,*,#16317,.T.);
#23167=ORIENTED_EDGE('',*,*,#16319,.T.);
#23168=ORIENTED_EDGE('',*,*,#16320,.F.);
#23169=ORIENTED_EDGE('',*,*,#16319,.F.);
#23170=ORIENTED_EDGE('',*,*,#16316,.T.);
#23171=ORIENTED_EDGE('',*,*,#16321,.T.);
#23172=ORIENTED_EDGE('',*,*,#16322,.F.);
#23173=ORIENTED_EDGE('',*,*,#16321,.F.);
#23174=ORIENTED_EDGE('',*,*,#16315,.F.);
#23175=ORIENTED_EDGE('',*,*,#16323,.F.);
#23176=ORIENTED_EDGE('',*,*,#16324,.T.);
#23177=ORIENTED_EDGE('',*,*,#16325,.F.);
#23178=ORIENTED_EDGE('',*,*,#16326,.F.);
#23179=ORIENTED_EDGE('',*,*,#16327,.F.);
#23180=ORIENTED_EDGE('',*,*,#16326,.T.);
#23181=ORIENTED_EDGE('',*,*,#16328,.T.);
#23182=ORIENTED_EDGE('',*,*,#16329,.F.);
#23183=ORIENTED_EDGE('',*,*,#16328,.F.);
#23184=ORIENTED_EDGE('',*,*,#16325,.T.);
#23185=ORIENTED_EDGE('',*,*,#16330,.T.);
#23186=ORIENTED_EDGE('',*,*,#16331,.F.);
#23187=ORIENTED_EDGE('',*,*,#16330,.F.);
#23188=ORIENTED_EDGE('',*,*,#16324,.F.);
#23189=ORIENTED_EDGE('',*,*,#16332,.F.);
#23190=ORIENTED_EDGE('',*,*,#16333,.T.);
#23191=ORIENTED_EDGE('',*,*,#16334,.F.);
#23192=ORIENTED_EDGE('',*,*,#16335,.F.);
#23193=ORIENTED_EDGE('',*,*,#16336,.F.);
#23194=ORIENTED_EDGE('',*,*,#16335,.T.);
#23195=ORIENTED_EDGE('',*,*,#16337,.T.);
#23196=ORIENTED_EDGE('',*,*,#16338,.F.);
#23197=ORIENTED_EDGE('',*,*,#16337,.F.);
#23198=ORIENTED_EDGE('',*,*,#16334,.T.);
#23199=ORIENTED_EDGE('',*,*,#16339,.T.);
#23200=ORIENTED_EDGE('',*,*,#16340,.F.);
#23201=ORIENTED_EDGE('',*,*,#16339,.F.);
#23202=ORIENTED_EDGE('',*,*,#16333,.F.);
#23203=ORIENTED_EDGE('',*,*,#16341,.F.);
#23204=ORIENTED_EDGE('',*,*,#16342,.T.);
#23205=ORIENTED_EDGE('',*,*,#16343,.F.);
#23206=ORIENTED_EDGE('',*,*,#16344,.F.);
#23207=ORIENTED_EDGE('',*,*,#16345,.F.);
#23208=ORIENTED_EDGE('',*,*,#16344,.T.);
#23209=ORIENTED_EDGE('',*,*,#16346,.T.);
#23210=ORIENTED_EDGE('',*,*,#16347,.F.);
#23211=ORIENTED_EDGE('',*,*,#16346,.F.);
#23212=ORIENTED_EDGE('',*,*,#16343,.T.);
#23213=ORIENTED_EDGE('',*,*,#16348,.T.);
#23214=ORIENTED_EDGE('',*,*,#16349,.F.);
#23215=ORIENTED_EDGE('',*,*,#16348,.F.);
#23216=ORIENTED_EDGE('',*,*,#16342,.F.);
#23217=ORIENTED_EDGE('',*,*,#16350,.F.);
#23218=ORIENTED_EDGE('',*,*,#16351,.T.);
#23219=ORIENTED_EDGE('',*,*,#16352,.F.);
#23220=ORIENTED_EDGE('',*,*,#16353,.F.);
#23221=ORIENTED_EDGE('',*,*,#16354,.F.);
#23222=ORIENTED_EDGE('',*,*,#16353,.T.);
#23223=ORIENTED_EDGE('',*,*,#16355,.T.);
#23224=ORIENTED_EDGE('',*,*,#16356,.F.);
#23225=ORIENTED_EDGE('',*,*,#16355,.F.);
#23226=ORIENTED_EDGE('',*,*,#16352,.T.);
#23227=ORIENTED_EDGE('',*,*,#16357,.T.);
#23228=ORIENTED_EDGE('',*,*,#16358,.F.);
#23229=ORIENTED_EDGE('',*,*,#16357,.F.);
#23230=ORIENTED_EDGE('',*,*,#16351,.F.);
#23231=ORIENTED_EDGE('',*,*,#16359,.F.);
#23232=ORIENTED_EDGE('',*,*,#16360,.T.);
#23233=ORIENTED_EDGE('',*,*,#16361,.F.);
#23234=ORIENTED_EDGE('',*,*,#16362,.F.);
#23235=ORIENTED_EDGE('',*,*,#16363,.F.);
#23236=ORIENTED_EDGE('',*,*,#16362,.T.);
#23237=ORIENTED_EDGE('',*,*,#16364,.T.);
#23238=ORIENTED_EDGE('',*,*,#16365,.F.);
#23239=ORIENTED_EDGE('',*,*,#16366,.F.);
#23240=ORIENTED_EDGE('',*,*,#16364,.F.);
#23241=ORIENTED_EDGE('',*,*,#16361,.T.);
#23242=ORIENTED_EDGE('',*,*,#16367,.T.);
#23243=ORIENTED_EDGE('',*,*,#16368,.F.);
#23244=ORIENTED_EDGE('',*,*,#16367,.F.);
#23245=ORIENTED_EDGE('',*,*,#16360,.F.);
#23246=ORIENTED_EDGE('',*,*,#16369,.F.);
#23247=ORIENTED_EDGE('',*,*,#16370,.F.);
#23248=ORIENTED_EDGE('',*,*,#16371,.T.);
#23249=ORIENTED_EDGE('',*,*,#16372,.F.);
#23250=ORIENTED_EDGE('',*,*,#16373,.F.);
#23251=ORIENTED_EDGE('',*,*,#16374,.F.);
#23252=ORIENTED_EDGE('',*,*,#16373,.T.);
#23253=ORIENTED_EDGE('',*,*,#16375,.T.);
#23254=ORIENTED_EDGE('',*,*,#16376,.F.);
#23255=ORIENTED_EDGE('',*,*,#16375,.F.);
#23256=ORIENTED_EDGE('',*,*,#16372,.T.);
#23257=ORIENTED_EDGE('',*,*,#16377,.T.);
#23258=ORIENTED_EDGE('',*,*,#16378,.F.);
#23259=ORIENTED_EDGE('',*,*,#16377,.F.);
#23260=ORIENTED_EDGE('',*,*,#16371,.F.);
#23261=ORIENTED_EDGE('',*,*,#16379,.F.);
#23262=ORIENTED_EDGE('',*,*,#16380,.T.);
#23263=ORIENTED_EDGE('',*,*,#16381,.F.);
#23264=ORIENTED_EDGE('',*,*,#16382,.F.);
#23265=ORIENTED_EDGE('',*,*,#16383,.F.);
#23266=ORIENTED_EDGE('',*,*,#16382,.T.);
#23267=ORIENTED_EDGE('',*,*,#16384,.T.);
#23268=ORIENTED_EDGE('',*,*,#16385,.F.);
#23269=ORIENTED_EDGE('',*,*,#16384,.F.);
#23270=ORIENTED_EDGE('',*,*,#16381,.T.);
#23271=ORIENTED_EDGE('',*,*,#16386,.T.);
#23272=ORIENTED_EDGE('',*,*,#16387,.F.);
#23273=ORIENTED_EDGE('',*,*,#16386,.F.);
#23274=ORIENTED_EDGE('',*,*,#16380,.F.);
#23275=ORIENTED_EDGE('',*,*,#16388,.F.);
#23276=ORIENTED_EDGE('',*,*,#16389,.T.);
#23277=ORIENTED_EDGE('',*,*,#16390,.F.);
#23278=ORIENTED_EDGE('',*,*,#16391,.F.);
#23279=ORIENTED_EDGE('',*,*,#16392,.F.);
#23280=ORIENTED_EDGE('',*,*,#16391,.T.);
#23281=ORIENTED_EDGE('',*,*,#16393,.T.);
#23282=ORIENTED_EDGE('',*,*,#16394,.F.);
#23283=ORIENTED_EDGE('',*,*,#16393,.F.);
#23284=ORIENTED_EDGE('',*,*,#16390,.T.);
#23285=ORIENTED_EDGE('',*,*,#16395,.T.);
#23286=ORIENTED_EDGE('',*,*,#16396,.F.);
#23287=ORIENTED_EDGE('',*,*,#16395,.F.);
#23288=ORIENTED_EDGE('',*,*,#16389,.F.);
#23289=ORIENTED_EDGE('',*,*,#16397,.F.);
#23290=ORIENTED_EDGE('',*,*,#16398,.T.);
#23291=ORIENTED_EDGE('',*,*,#16399,.F.);
#23292=ORIENTED_EDGE('',*,*,#16400,.F.);
#23293=ORIENTED_EDGE('',*,*,#16401,.F.);
#23294=ORIENTED_EDGE('',*,*,#16400,.T.);
#23295=ORIENTED_EDGE('',*,*,#16402,.T.);
#23296=ORIENTED_EDGE('',*,*,#16403,.F.);
#23297=ORIENTED_EDGE('',*,*,#16402,.F.);
#23298=ORIENTED_EDGE('',*,*,#16399,.T.);
#23299=ORIENTED_EDGE('',*,*,#16404,.T.);
#23300=ORIENTED_EDGE('',*,*,#16405,.F.);
#23301=ORIENTED_EDGE('',*,*,#16404,.F.);
#23302=ORIENTED_EDGE('',*,*,#16398,.F.);
#23303=ORIENTED_EDGE('',*,*,#16406,.F.);
#23304=ORIENTED_EDGE('',*,*,#16407,.T.);
#23305=ORIENTED_EDGE('',*,*,#16408,.F.);
#23306=ORIENTED_EDGE('',*,*,#16409,.F.);
#23307=ORIENTED_EDGE('',*,*,#16410,.F.);
#23308=ORIENTED_EDGE('',*,*,#16409,.T.);
#23309=ORIENTED_EDGE('',*,*,#16411,.T.);
#23310=ORIENTED_EDGE('',*,*,#16412,.F.);
#23311=ORIENTED_EDGE('',*,*,#16411,.F.);
#23312=ORIENTED_EDGE('',*,*,#16408,.T.);
#23313=ORIENTED_EDGE('',*,*,#16413,.T.);
#23314=ORIENTED_EDGE('',*,*,#16414,.F.);
#23315=ORIENTED_EDGE('',*,*,#16413,.F.);
#23316=ORIENTED_EDGE('',*,*,#16407,.F.);
#23317=ORIENTED_EDGE('',*,*,#16415,.F.);
#23318=ORIENTED_EDGE('',*,*,#16416,.T.);
#23319=ORIENTED_EDGE('',*,*,#16417,.F.);
#23320=ORIENTED_EDGE('',*,*,#16418,.F.);
#23321=ORIENTED_EDGE('',*,*,#16419,.F.);
#23322=ORIENTED_EDGE('',*,*,#16418,.T.);
#23323=ORIENTED_EDGE('',*,*,#16420,.T.);
#23324=ORIENTED_EDGE('',*,*,#16421,.F.);
#23325=ORIENTED_EDGE('',*,*,#16420,.F.);
#23326=ORIENTED_EDGE('',*,*,#16417,.T.);
#23327=ORIENTED_EDGE('',*,*,#16422,.T.);
#23328=ORIENTED_EDGE('',*,*,#16423,.F.);
#23329=ORIENTED_EDGE('',*,*,#16422,.F.);
#23330=ORIENTED_EDGE('',*,*,#16416,.F.);
#23331=ORIENTED_EDGE('',*,*,#16424,.F.);
#23332=ORIENTED_EDGE('',*,*,#16425,.T.);
#23333=ORIENTED_EDGE('',*,*,#16426,.F.);
#23334=ORIENTED_EDGE('',*,*,#16427,.F.);
#23335=ORIENTED_EDGE('',*,*,#16428,.F.);
#23336=ORIENTED_EDGE('',*,*,#16427,.T.);
#23337=ORIENTED_EDGE('',*,*,#16429,.T.);
#23338=ORIENTED_EDGE('',*,*,#16430,.F.);
#23339=ORIENTED_EDGE('',*,*,#16429,.F.);
#23340=ORIENTED_EDGE('',*,*,#16426,.T.);
#23341=ORIENTED_EDGE('',*,*,#16431,.T.);
#23342=ORIENTED_EDGE('',*,*,#16432,.F.);
#23343=ORIENTED_EDGE('',*,*,#16431,.F.);
#23344=ORIENTED_EDGE('',*,*,#16425,.F.);
#23345=ORIENTED_EDGE('',*,*,#16433,.F.);
#23346=ORIENTED_EDGE('',*,*,#16434,.T.);
#23347=ORIENTED_EDGE('',*,*,#16435,.F.);
#23348=ORIENTED_EDGE('',*,*,#16436,.F.);
#23349=ORIENTED_EDGE('',*,*,#16437,.F.);
#23350=ORIENTED_EDGE('',*,*,#16436,.T.);
#23351=ORIENTED_EDGE('',*,*,#16438,.T.);
#23352=ORIENTED_EDGE('',*,*,#16439,.F.);
#23353=ORIENTED_EDGE('',*,*,#16438,.F.);
#23354=ORIENTED_EDGE('',*,*,#16435,.T.);
#23355=ORIENTED_EDGE('',*,*,#16440,.T.);
#23356=ORIENTED_EDGE('',*,*,#16441,.F.);
#23357=ORIENTED_EDGE('',*,*,#16440,.F.);
#23358=ORIENTED_EDGE('',*,*,#16434,.F.);
#23359=ORIENTED_EDGE('',*,*,#16442,.F.);
#23360=ORIENTED_EDGE('',*,*,#16443,.T.);
#23361=ORIENTED_EDGE('',*,*,#16444,.F.);
#23362=ORIENTED_EDGE('',*,*,#16445,.F.);
#23363=ORIENTED_EDGE('',*,*,#16446,.F.);
#23364=ORIENTED_EDGE('',*,*,#16445,.T.);
#23365=ORIENTED_EDGE('',*,*,#16447,.T.);
#23366=ORIENTED_EDGE('',*,*,#16448,.F.);
#23367=ORIENTED_EDGE('',*,*,#16447,.F.);
#23368=ORIENTED_EDGE('',*,*,#16444,.T.);
#23369=ORIENTED_EDGE('',*,*,#16449,.T.);
#23370=ORIENTED_EDGE('',*,*,#16450,.F.);
#23371=ORIENTED_EDGE('',*,*,#16449,.F.);
#23372=ORIENTED_EDGE('',*,*,#16443,.F.);
#23373=ORIENTED_EDGE('',*,*,#16451,.F.);
#23374=ORIENTED_EDGE('',*,*,#16452,.T.);
#23375=ORIENTED_EDGE('',*,*,#16453,.F.);
#23376=ORIENTED_EDGE('',*,*,#16454,.F.);
#23377=ORIENTED_EDGE('',*,*,#16455,.F.);
#23378=ORIENTED_EDGE('',*,*,#16454,.T.);
#23379=ORIENTED_EDGE('',*,*,#16456,.T.);
#23380=ORIENTED_EDGE('',*,*,#16457,.F.);
#23381=ORIENTED_EDGE('',*,*,#16456,.F.);
#23382=ORIENTED_EDGE('',*,*,#16453,.T.);
#23383=ORIENTED_EDGE('',*,*,#16458,.T.);
#23384=ORIENTED_EDGE('',*,*,#16459,.F.);
#23385=ORIENTED_EDGE('',*,*,#16458,.F.);
#23386=ORIENTED_EDGE('',*,*,#16452,.F.);
#23387=ORIENTED_EDGE('',*,*,#16460,.F.);
#23388=ORIENTED_EDGE('',*,*,#16461,.T.);
#23389=ORIENTED_EDGE('',*,*,#16462,.F.);
#23390=ORIENTED_EDGE('',*,*,#16463,.F.);
#23391=ORIENTED_EDGE('',*,*,#16464,.F.);
#23392=ORIENTED_EDGE('',*,*,#16463,.T.);
#23393=ORIENTED_EDGE('',*,*,#16465,.T.);
#23394=ORIENTED_EDGE('',*,*,#16466,.F.);
#23395=ORIENTED_EDGE('',*,*,#16465,.F.);
#23396=ORIENTED_EDGE('',*,*,#16462,.T.);
#23397=ORIENTED_EDGE('',*,*,#16467,.T.);
#23398=ORIENTED_EDGE('',*,*,#16468,.F.);
#23399=ORIENTED_EDGE('',*,*,#16467,.F.);
#23400=ORIENTED_EDGE('',*,*,#16461,.F.);
#23401=ORIENTED_EDGE('',*,*,#16469,.F.);
#23402=ORIENTED_EDGE('',*,*,#16470,.T.);
#23403=ORIENTED_EDGE('',*,*,#16471,.F.);
#23404=ORIENTED_EDGE('',*,*,#16472,.F.);
#23405=ORIENTED_EDGE('',*,*,#16473,.F.);
#23406=ORIENTED_EDGE('',*,*,#16472,.T.);
#23407=ORIENTED_EDGE('',*,*,#16474,.T.);
#23408=ORIENTED_EDGE('',*,*,#16475,.F.);
#23409=ORIENTED_EDGE('',*,*,#16474,.F.);
#23410=ORIENTED_EDGE('',*,*,#16471,.T.);
#23411=ORIENTED_EDGE('',*,*,#16476,.T.);
#23412=ORIENTED_EDGE('',*,*,#16477,.F.);
#23413=ORIENTED_EDGE('',*,*,#16476,.F.);
#23414=ORIENTED_EDGE('',*,*,#16470,.F.);
#23415=ORIENTED_EDGE('',*,*,#16478,.F.);
#23416=ORIENTED_EDGE('',*,*,#16479,.T.);
#23417=ORIENTED_EDGE('',*,*,#16480,.F.);
#23418=ORIENTED_EDGE('',*,*,#16481,.F.);
#23419=ORIENTED_EDGE('',*,*,#16482,.F.);
#23420=ORIENTED_EDGE('',*,*,#16481,.T.);
#23421=ORIENTED_EDGE('',*,*,#16483,.T.);
#23422=ORIENTED_EDGE('',*,*,#16484,.F.);
#23423=ORIENTED_EDGE('',*,*,#16483,.F.);
#23424=ORIENTED_EDGE('',*,*,#16480,.T.);
#23425=ORIENTED_EDGE('',*,*,#16485,.T.);
#23426=ORIENTED_EDGE('',*,*,#16486,.F.);
#23427=ORIENTED_EDGE('',*,*,#16485,.F.);
#23428=ORIENTED_EDGE('',*,*,#16479,.F.);
#23429=ORIENTED_EDGE('',*,*,#16487,.F.);
#23430=ORIENTED_EDGE('',*,*,#16488,.T.);
#23431=ORIENTED_EDGE('',*,*,#16489,.F.);
#23432=ORIENTED_EDGE('',*,*,#16490,.F.);
#23433=ORIENTED_EDGE('',*,*,#16491,.F.);
#23434=ORIENTED_EDGE('',*,*,#16490,.T.);
#23435=ORIENTED_EDGE('',*,*,#16492,.T.);
#23436=ORIENTED_EDGE('',*,*,#16493,.F.);
#23437=ORIENTED_EDGE('',*,*,#16492,.F.);
#23438=ORIENTED_EDGE('',*,*,#16489,.T.);
#23439=ORIENTED_EDGE('',*,*,#16494,.T.);
#23440=ORIENTED_EDGE('',*,*,#16495,.F.);
#23441=ORIENTED_EDGE('',*,*,#16494,.F.);
#23442=ORIENTED_EDGE('',*,*,#16488,.F.);
#23443=ORIENTED_EDGE('',*,*,#16496,.F.);
#23444=ORIENTED_EDGE('',*,*,#16497,.T.);
#23445=ORIENTED_EDGE('',*,*,#16498,.F.);
#23446=ORIENTED_EDGE('',*,*,#16499,.F.);
#23447=ORIENTED_EDGE('',*,*,#16500,.F.);
#23448=ORIENTED_EDGE('',*,*,#16499,.T.);
#23449=ORIENTED_EDGE('',*,*,#16501,.T.);
#23450=ORIENTED_EDGE('',*,*,#16502,.F.);
#23451=ORIENTED_EDGE('',*,*,#16501,.F.);
#23452=ORIENTED_EDGE('',*,*,#16498,.T.);
#23453=ORIENTED_EDGE('',*,*,#16503,.T.);
#23454=ORIENTED_EDGE('',*,*,#16504,.F.);
#23455=ORIENTED_EDGE('',*,*,#16503,.F.);
#23456=ORIENTED_EDGE('',*,*,#16497,.F.);
#23457=ORIENTED_EDGE('',*,*,#16505,.F.);
#23458=ORIENTED_EDGE('',*,*,#16506,.T.);
#23459=ORIENTED_EDGE('',*,*,#16507,.F.);
#23460=ORIENTED_EDGE('',*,*,#16508,.F.);
#23461=ORIENTED_EDGE('',*,*,#16509,.F.);
#23462=ORIENTED_EDGE('',*,*,#16508,.T.);
#23463=ORIENTED_EDGE('',*,*,#16510,.T.);
#23464=ORIENTED_EDGE('',*,*,#16511,.F.);
#23465=ORIENTED_EDGE('',*,*,#16510,.F.);
#23466=ORIENTED_EDGE('',*,*,#16507,.T.);
#23467=ORIENTED_EDGE('',*,*,#16512,.T.);
#23468=ORIENTED_EDGE('',*,*,#16513,.F.);
#23469=ORIENTED_EDGE('',*,*,#16512,.F.);
#23470=ORIENTED_EDGE('',*,*,#16506,.F.);
#23471=ORIENTED_EDGE('',*,*,#16514,.F.);
#23472=ORIENTED_EDGE('',*,*,#16515,.T.);
#23473=ORIENTED_EDGE('',*,*,#16516,.F.);
#23474=ORIENTED_EDGE('',*,*,#16517,.F.);
#23475=ORIENTED_EDGE('',*,*,#16518,.F.);
#23476=ORIENTED_EDGE('',*,*,#16517,.T.);
#23477=ORIENTED_EDGE('',*,*,#16519,.T.);
#23478=ORIENTED_EDGE('',*,*,#16520,.F.);
#23479=ORIENTED_EDGE('',*,*,#16519,.F.);
#23480=ORIENTED_EDGE('',*,*,#16516,.T.);
#23481=ORIENTED_EDGE('',*,*,#16521,.T.);
#23482=ORIENTED_EDGE('',*,*,#16522,.F.);
#23483=ORIENTED_EDGE('',*,*,#16521,.F.);
#23484=ORIENTED_EDGE('',*,*,#16515,.F.);
#23485=ORIENTED_EDGE('',*,*,#16523,.F.);
#23486=ORIENTED_EDGE('',*,*,#16524,.T.);
#23487=ORIENTED_EDGE('',*,*,#16525,.T.);
#23488=ORIENTED_EDGE('',*,*,#16526,.F.);
#23489=ORIENTED_EDGE('',*,*,#16527,.T.);
#23490=ORIENTED_EDGE('',*,*,#16528,.F.);
#23491=ORIENTED_EDGE('',*,*,#16524,.F.);
#23492=ORIENTED_EDGE('',*,*,#16529,.F.);
#23493=ORIENTED_EDGE('',*,*,#16525,.F.);
#23494=ORIENTED_EDGE('',*,*,#16528,.T.);
#23495=ORIENTED_EDGE('',*,*,#16530,.T.);
#23496=ORIENTED_EDGE('',*,*,#16531,.F.);
#23497=ORIENTED_EDGE('',*,*,#16530,.F.);
#23498=ORIENTED_EDGE('',*,*,#16527,.F.);
#23499=ORIENTED_EDGE('',*,*,#16532,.F.);
#23500=ORIENTED_EDGE('',*,*,#16533,.T.);
#23501=ORIENTED_EDGE('',*,*,#16534,.F.);
#23502=ORIENTED_EDGE('',*,*,#16535,.F.);
#23503=ORIENTED_EDGE('',*,*,#16536,.F.);
#23504=ORIENTED_EDGE('',*,*,#16535,.T.);
#23505=ORIENTED_EDGE('',*,*,#16537,.T.);
#23506=ORIENTED_EDGE('',*,*,#16538,.F.);
#23507=ORIENTED_EDGE('',*,*,#16537,.F.);
#23508=ORIENTED_EDGE('',*,*,#16534,.T.);
#23509=ORIENTED_EDGE('',*,*,#16539,.T.);
#23510=ORIENTED_EDGE('',*,*,#16540,.F.);
#23511=ORIENTED_EDGE('',*,*,#16539,.F.);
#23512=ORIENTED_EDGE('',*,*,#16533,.F.);
#23513=ORIENTED_EDGE('',*,*,#16541,.F.);
#23514=ORIENTED_EDGE('',*,*,#16542,.T.);
#23515=ORIENTED_EDGE('',*,*,#16543,.F.);
#23516=ORIENTED_EDGE('',*,*,#16544,.F.);
#23517=ORIENTED_EDGE('',*,*,#16545,.F.);
#23518=ORIENTED_EDGE('',*,*,#16544,.T.);
#23519=ORIENTED_EDGE('',*,*,#16546,.T.);
#23520=ORIENTED_EDGE('',*,*,#16547,.F.);
#23521=ORIENTED_EDGE('',*,*,#16546,.F.);
#23522=ORIENTED_EDGE('',*,*,#16543,.T.);
#23523=ORIENTED_EDGE('',*,*,#16548,.T.);
#23524=ORIENTED_EDGE('',*,*,#16549,.F.);
#23525=ORIENTED_EDGE('',*,*,#16548,.F.);
#23526=ORIENTED_EDGE('',*,*,#16542,.F.);
#23527=ORIENTED_EDGE('',*,*,#16550,.F.);
#23528=ORIENTED_EDGE('',*,*,#16551,.T.);
#23529=ORIENTED_EDGE('',*,*,#16552,.F.);
#23530=ORIENTED_EDGE('',*,*,#16553,.F.);
#23531=ORIENTED_EDGE('',*,*,#16554,.F.);
#23532=ORIENTED_EDGE('',*,*,#16553,.T.);
#23533=ORIENTED_EDGE('',*,*,#16555,.T.);
#23534=ORIENTED_EDGE('',*,*,#16556,.F.);
#23535=ORIENTED_EDGE('',*,*,#16555,.F.);
#23536=ORIENTED_EDGE('',*,*,#16552,.T.);
#23537=ORIENTED_EDGE('',*,*,#16557,.T.);
#23538=ORIENTED_EDGE('',*,*,#16558,.F.);
#23539=ORIENTED_EDGE('',*,*,#16557,.F.);
#23540=ORIENTED_EDGE('',*,*,#16551,.F.);
#23541=ORIENTED_EDGE('',*,*,#16559,.F.);
#23542=ORIENTED_EDGE('',*,*,#16560,.T.);
#23543=ORIENTED_EDGE('',*,*,#16561,.F.);
#23544=ORIENTED_EDGE('',*,*,#16562,.F.);
#23545=ORIENTED_EDGE('',*,*,#16563,.F.);
#23546=ORIENTED_EDGE('',*,*,#16562,.T.);
#23547=ORIENTED_EDGE('',*,*,#16564,.T.);
#23548=ORIENTED_EDGE('',*,*,#16565,.F.);
#23549=ORIENTED_EDGE('',*,*,#16564,.F.);
#23550=ORIENTED_EDGE('',*,*,#16561,.T.);
#23551=ORIENTED_EDGE('',*,*,#16566,.T.);
#23552=ORIENTED_EDGE('',*,*,#16567,.F.);
#23553=ORIENTED_EDGE('',*,*,#16566,.F.);
#23554=ORIENTED_EDGE('',*,*,#16560,.F.);
#23555=ORIENTED_EDGE('',*,*,#16568,.F.);
#23556=ORIENTED_EDGE('',*,*,#16569,.T.);
#23557=ORIENTED_EDGE('',*,*,#16570,.F.);
#23558=ORIENTED_EDGE('',*,*,#16571,.F.);
#23559=ORIENTED_EDGE('',*,*,#16572,.F.);
#23560=ORIENTED_EDGE('',*,*,#16571,.T.);
#23561=ORIENTED_EDGE('',*,*,#16573,.T.);
#23562=ORIENTED_EDGE('',*,*,#16574,.F.);
#23563=ORIENTED_EDGE('',*,*,#16573,.F.);
#23564=ORIENTED_EDGE('',*,*,#16570,.T.);
#23565=ORIENTED_EDGE('',*,*,#16575,.T.);
#23566=ORIENTED_EDGE('',*,*,#16576,.F.);
#23567=ORIENTED_EDGE('',*,*,#16575,.F.);
#23568=ORIENTED_EDGE('',*,*,#16569,.F.);
#23569=ORIENTED_EDGE('',*,*,#16577,.F.);
#23570=ORIENTED_EDGE('',*,*,#16578,.T.);
#23571=ORIENTED_EDGE('',*,*,#16579,.F.);
#23572=ORIENTED_EDGE('',*,*,#16580,.F.);
#23573=ORIENTED_EDGE('',*,*,#16581,.F.);
#23574=ORIENTED_EDGE('',*,*,#16580,.T.);
#23575=ORIENTED_EDGE('',*,*,#16582,.T.);
#23576=ORIENTED_EDGE('',*,*,#16583,.F.);
#23577=ORIENTED_EDGE('',*,*,#16582,.F.);
#23578=ORIENTED_EDGE('',*,*,#16579,.T.);
#23579=ORIENTED_EDGE('',*,*,#16584,.T.);
#23580=ORIENTED_EDGE('',*,*,#16585,.F.);
#23581=ORIENTED_EDGE('',*,*,#16584,.F.);
#23582=ORIENTED_EDGE('',*,*,#16578,.F.);
#23583=ORIENTED_EDGE('',*,*,#16586,.F.);
#23584=ORIENTED_EDGE('',*,*,#16587,.T.);
#23585=ORIENTED_EDGE('',*,*,#16588,.F.);
#23586=ORIENTED_EDGE('',*,*,#16589,.F.);
#23587=ORIENTED_EDGE('',*,*,#16590,.F.);
#23588=ORIENTED_EDGE('',*,*,#16589,.T.);
#23589=ORIENTED_EDGE('',*,*,#16591,.T.);
#23590=ORIENTED_EDGE('',*,*,#16592,.F.);
#23591=ORIENTED_EDGE('',*,*,#16591,.F.);
#23592=ORIENTED_EDGE('',*,*,#16588,.T.);
#23593=ORIENTED_EDGE('',*,*,#16593,.T.);
#23594=ORIENTED_EDGE('',*,*,#16594,.F.);
#23595=ORIENTED_EDGE('',*,*,#16593,.F.);
#23596=ORIENTED_EDGE('',*,*,#16587,.F.);
#23597=ORIENTED_EDGE('',*,*,#16595,.F.);
#23598=ORIENTED_EDGE('',*,*,#16596,.T.);
#23599=ORIENTED_EDGE('',*,*,#16597,.F.);
#23600=ORIENTED_EDGE('',*,*,#16598,.F.);
#23601=ORIENTED_EDGE('',*,*,#16599,.F.);
#23602=ORIENTED_EDGE('',*,*,#16598,.T.);
#23603=ORIENTED_EDGE('',*,*,#16600,.T.);
#23604=ORIENTED_EDGE('',*,*,#16601,.F.);
#23605=ORIENTED_EDGE('',*,*,#16600,.F.);
#23606=ORIENTED_EDGE('',*,*,#16597,.T.);
#23607=ORIENTED_EDGE('',*,*,#16602,.T.);
#23608=ORIENTED_EDGE('',*,*,#16603,.F.);
#23609=ORIENTED_EDGE('',*,*,#16602,.F.);
#23610=ORIENTED_EDGE('',*,*,#16596,.F.);
#23611=ORIENTED_EDGE('',*,*,#16604,.F.);
#23612=ORIENTED_EDGE('',*,*,#16605,.T.);
#23613=ORIENTED_EDGE('',*,*,#16606,.F.);
#23614=ORIENTED_EDGE('',*,*,#16607,.F.);
#23615=ORIENTED_EDGE('',*,*,#16608,.F.);
#23616=ORIENTED_EDGE('',*,*,#16607,.T.);
#23617=ORIENTED_EDGE('',*,*,#16609,.T.);
#23618=ORIENTED_EDGE('',*,*,#16610,.F.);
#23619=ORIENTED_EDGE('',*,*,#16609,.F.);
#23620=ORIENTED_EDGE('',*,*,#16606,.T.);
#23621=ORIENTED_EDGE('',*,*,#16611,.T.);
#23622=ORIENTED_EDGE('',*,*,#16612,.F.);
#23623=ORIENTED_EDGE('',*,*,#16611,.F.);
#23624=ORIENTED_EDGE('',*,*,#16605,.F.);
#23625=ORIENTED_EDGE('',*,*,#16613,.F.);
#23626=ORIENTED_EDGE('',*,*,#16252,.F.);
#23627=ORIENTED_EDGE('',*,*,#16107,.F.);
#23628=ORIENTED_EDGE('',*,*,#16253,.F.);
#23629=ORIENTED_EDGE('',*,*,#16614,.T.);
#23630=ORIENTED_EDGE('',*,*,#16613,.T.);
#23631=ORIENTED_EDGE('',*,*,#16614,.F.);
#23632=ORIENTED_EDGE('',*,*,#16615,.F.);
#23633=ORIENTED_EDGE('',*,*,#16616,.T.);
#23634=ORIENTED_EDGE('',*,*,#16261,.T.);
#23635=ORIENTED_EDGE('',*,*,#16616,.F.);
#23636=ORIENTED_EDGE('',*,*,#16287,.T.);
#23637=ORIENTED_EDGE('',*,*,#16617,.F.);
#23638=ORIENTED_EDGE('',*,*,#16601,.T.);
#23639=ORIENTED_EDGE('',*,*,#16603,.T.);
#23640=ORIENTED_EDGE('',*,*,#16595,.T.);
#23641=ORIENTED_EDGE('',*,*,#16618,.F.);
#23642=ORIENTED_EDGE('',*,*,#16302,.T.);
#23643=ORIENTED_EDGE('',*,*,#16304,.T.);
#23644=ORIENTED_EDGE('',*,*,#16296,.T.);
#23645=ORIENTED_EDGE('',*,*,#16619,.F.);
#23646=ORIENTED_EDGE('',*,*,#16592,.T.);
#23647=ORIENTED_EDGE('',*,*,#16594,.T.);
#23648=ORIENTED_EDGE('',*,*,#16586,.T.);
#23649=ORIENTED_EDGE('',*,*,#16620,.F.);
#23650=ORIENTED_EDGE('',*,*,#16311,.T.);
#23651=ORIENTED_EDGE('',*,*,#16313,.T.);
#23652=ORIENTED_EDGE('',*,*,#16305,.T.);
#23653=ORIENTED_EDGE('',*,*,#16621,.F.);
#23654=ORIENTED_EDGE('',*,*,#16583,.T.);
#23655=ORIENTED_EDGE('',*,*,#16585,.T.);
#23656=ORIENTED_EDGE('',*,*,#16577,.T.);
#23657=ORIENTED_EDGE('',*,*,#16622,.F.);
#23658=ORIENTED_EDGE('',*,*,#16320,.T.);
#23659=ORIENTED_EDGE('',*,*,#16322,.T.);
#23660=ORIENTED_EDGE('',*,*,#16314,.T.);
#23661=ORIENTED_EDGE('',*,*,#16623,.F.);
#23662=ORIENTED_EDGE('',*,*,#16574,.T.);
#23663=ORIENTED_EDGE('',*,*,#16576,.T.);
#23664=ORIENTED_EDGE('',*,*,#16568,.T.);
#23665=ORIENTED_EDGE('',*,*,#16624,.F.);
#23666=ORIENTED_EDGE('',*,*,#16329,.T.);
#23667=ORIENTED_EDGE('',*,*,#16331,.T.);
#23668=ORIENTED_EDGE('',*,*,#16323,.T.);
#23669=ORIENTED_EDGE('',*,*,#16625,.F.);
#23670=ORIENTED_EDGE('',*,*,#16565,.T.);
#23671=ORIENTED_EDGE('',*,*,#16567,.T.);
#23672=ORIENTED_EDGE('',*,*,#16559,.T.);
#23673=ORIENTED_EDGE('',*,*,#16626,.F.);
#23674=ORIENTED_EDGE('',*,*,#16338,.T.);
#23675=ORIENTED_EDGE('',*,*,#16340,.T.);
#23676=ORIENTED_EDGE('',*,*,#16332,.T.);
#23677=ORIENTED_EDGE('',*,*,#16627,.F.);
#23678=ORIENTED_EDGE('',*,*,#16556,.T.);
#23679=ORIENTED_EDGE('',*,*,#16558,.T.);
#23680=ORIENTED_EDGE('',*,*,#16550,.T.);
#23681=ORIENTED_EDGE('',*,*,#16628,.F.);
#23682=ORIENTED_EDGE('',*,*,#16347,.T.);
#23683=ORIENTED_EDGE('',*,*,#16349,.T.);
#23684=ORIENTED_EDGE('',*,*,#16341,.T.);
#23685=ORIENTED_EDGE('',*,*,#16629,.F.);
#23686=ORIENTED_EDGE('',*,*,#16547,.T.);
#23687=ORIENTED_EDGE('',*,*,#16549,.T.);
#23688=ORIENTED_EDGE('',*,*,#16541,.T.);
#23689=ORIENTED_EDGE('',*,*,#16630,.F.);
#23690=ORIENTED_EDGE('',*,*,#16356,.T.);
#23691=ORIENTED_EDGE('',*,*,#16358,.T.);
#23692=ORIENTED_EDGE('',*,*,#16350,.T.);
#23693=ORIENTED_EDGE('',*,*,#16631,.F.);
#23694=ORIENTED_EDGE('',*,*,#16538,.T.);
#23695=ORIENTED_EDGE('',*,*,#16540,.T.);
#23696=ORIENTED_EDGE('',*,*,#16532,.T.);
#23697=ORIENTED_EDGE('',*,*,#16632,.F.);
#23698=ORIENTED_EDGE('',*,*,#16366,.T.);
#23699=ORIENTED_EDGE('',*,*,#16368,.T.);
#23700=ORIENTED_EDGE('',*,*,#16633,.T.);
#23701=ORIENTED_EDGE('',*,*,#16615,.T.);
#23702=ORIENTED_EDGE('',*,*,#16633,.F.);
#23703=ORIENTED_EDGE('',*,*,#16369,.T.);
#23704=ORIENTED_EDGE('',*,*,#16359,.T.);
#23705=ORIENTED_EDGE('',*,*,#16634,.F.);
#23706=ORIENTED_EDGE('',*,*,#16376,.T.);
#23707=ORIENTED_EDGE('',*,*,#16378,.T.);
#23708=ORIENTED_EDGE('',*,*,#16370,.T.);
#23709=ORIENTED_EDGE('',*,*,#16635,.F.);
#23710=ORIENTED_EDGE('',*,*,#16520,.T.);
#23711=ORIENTED_EDGE('',*,*,#16522,.T.);
#23712=ORIENTED_EDGE('',*,*,#16514,.T.);
#23713=ORIENTED_EDGE('',*,*,#16636,.F.);
#23714=ORIENTED_EDGE('',*,*,#16385,.T.);
#23715=ORIENTED_EDGE('',*,*,#16387,.T.);
#23716=ORIENTED_EDGE('',*,*,#16379,.T.);
#23717=ORIENTED_EDGE('',*,*,#16637,.F.);
#23718=ORIENTED_EDGE('',*,*,#16511,.T.);
#23719=ORIENTED_EDGE('',*,*,#16513,.T.);
#23720=ORIENTED_EDGE('',*,*,#16505,.T.);
#23721=ORIENTED_EDGE('',*,*,#16638,.F.);
#23722=ORIENTED_EDGE('',*,*,#16394,.T.);
#23723=ORIENTED_EDGE('',*,*,#16396,.T.);
#23724=ORIENTED_EDGE('',*,*,#16388,.T.);
#23725=ORIENTED_EDGE('',*,*,#16639,.F.);
#23726=ORIENTED_EDGE('',*,*,#16502,.T.);
#23727=ORIENTED_EDGE('',*,*,#16504,.T.);
#23728=ORIENTED_EDGE('',*,*,#16496,.T.);
#23729=ORIENTED_EDGE('',*,*,#16640,.F.);
#23730=ORIENTED_EDGE('',*,*,#16403,.T.);
#23731=ORIENTED_EDGE('',*,*,#16405,.T.);
#23732=ORIENTED_EDGE('',*,*,#16397,.T.);
#23733=ORIENTED_EDGE('',*,*,#16641,.F.);
#23734=ORIENTED_EDGE('',*,*,#16493,.T.);
#23735=ORIENTED_EDGE('',*,*,#16495,.T.);
#23736=ORIENTED_EDGE('',*,*,#16487,.T.);
#23737=ORIENTED_EDGE('',*,*,#16642,.F.);
#23738=ORIENTED_EDGE('',*,*,#16412,.T.);
#23739=ORIENTED_EDGE('',*,*,#16414,.T.);
#23740=ORIENTED_EDGE('',*,*,#16406,.T.);
#23741=ORIENTED_EDGE('',*,*,#16643,.F.);
#23742=ORIENTED_EDGE('',*,*,#16484,.T.);
#23743=ORIENTED_EDGE('',*,*,#16486,.T.);
#23744=ORIENTED_EDGE('',*,*,#16478,.T.);
#23745=ORIENTED_EDGE('',*,*,#16644,.F.);
#23746=ORIENTED_EDGE('',*,*,#16421,.T.);
#23747=ORIENTED_EDGE('',*,*,#16423,.T.);
#23748=ORIENTED_EDGE('',*,*,#16415,.T.);
#23749=ORIENTED_EDGE('',*,*,#16645,.F.);
#23750=ORIENTED_EDGE('',*,*,#16475,.T.);
#23751=ORIENTED_EDGE('',*,*,#16477,.T.);
#23752=ORIENTED_EDGE('',*,*,#16469,.T.);
#23753=ORIENTED_EDGE('',*,*,#16646,.F.);
#23754=ORIENTED_EDGE('',*,*,#16430,.T.);
#23755=ORIENTED_EDGE('',*,*,#16432,.T.);
#23756=ORIENTED_EDGE('',*,*,#16424,.T.);
#23757=ORIENTED_EDGE('',*,*,#16647,.F.);
#23758=ORIENTED_EDGE('',*,*,#16466,.T.);
#23759=ORIENTED_EDGE('',*,*,#16468,.T.);
#23760=ORIENTED_EDGE('',*,*,#16460,.T.);
#23761=ORIENTED_EDGE('',*,*,#16648,.F.);
#23762=ORIENTED_EDGE('',*,*,#16439,.T.);
#23763=ORIENTED_EDGE('',*,*,#16441,.T.);
#23764=ORIENTED_EDGE('',*,*,#16433,.T.);
#23765=ORIENTED_EDGE('',*,*,#16649,.F.);
#23766=ORIENTED_EDGE('',*,*,#16457,.T.);
#23767=ORIENTED_EDGE('',*,*,#16459,.T.);
#23768=ORIENTED_EDGE('',*,*,#16451,.T.);
#23769=ORIENTED_EDGE('',*,*,#16650,.F.);
#23770=ORIENTED_EDGE('',*,*,#16448,.T.);
#23771=ORIENTED_EDGE('',*,*,#16450,.T.);
#23772=ORIENTED_EDGE('',*,*,#16442,.T.);
#23773=ORIENTED_EDGE('',*,*,#16651,.F.);
#23774=ORIENTED_EDGE('',*,*,#16529,.T.);
#23775=ORIENTED_EDGE('',*,*,#16531,.T.);
#23776=ORIENTED_EDGE('',*,*,#16526,.T.);
#23777=ORIENTED_EDGE('',*,*,#16652,.F.);
#23778=ORIENTED_EDGE('',*,*,#16610,.T.);
#23779=ORIENTED_EDGE('',*,*,#16612,.T.);
#23780=ORIENTED_EDGE('',*,*,#16604,.T.);
#23781=ORIENTED_EDGE('',*,*,#16653,.F.);
#23782=ORIENTED_EDGE('',*,*,#16293,.T.);
#23783=ORIENTED_EDGE('',*,*,#16295,.T.);
#23784=ORIENTED_EDGE('',*,*,#16654,.F.);
#23785=ORIENTED_EDGE('',*,*,#16655,.T.);
#23786=ORIENTED_EDGE('',*,*,#16365,.T.);
#23787=ORIENTED_EDGE('',*,*,#16632,.T.);
#23788=ORIENTED_EDGE('',*,*,#16536,.T.);
#23789=ORIENTED_EDGE('',*,*,#16631,.T.);
#23790=ORIENTED_EDGE('',*,*,#16354,.T.);
#23791=ORIENTED_EDGE('',*,*,#16630,.T.);
#23792=ORIENTED_EDGE('',*,*,#16545,.T.);
#23793=ORIENTED_EDGE('',*,*,#16629,.T.);
#23794=ORIENTED_EDGE('',*,*,#16345,.T.);
#23795=ORIENTED_EDGE('',*,*,#16628,.T.);
#23796=ORIENTED_EDGE('',*,*,#16554,.T.);
#23797=ORIENTED_EDGE('',*,*,#16627,.T.);
#23798=ORIENTED_EDGE('',*,*,#16336,.T.);
#23799=ORIENTED_EDGE('',*,*,#16626,.T.);
#23800=ORIENTED_EDGE('',*,*,#16563,.T.);
#23801=ORIENTED_EDGE('',*,*,#16625,.T.);
#23802=ORIENTED_EDGE('',*,*,#16327,.T.);
#23803=ORIENTED_EDGE('',*,*,#16624,.T.);
#23804=ORIENTED_EDGE('',*,*,#16572,.T.);
#23805=ORIENTED_EDGE('',*,*,#16623,.T.);
#23806=ORIENTED_EDGE('',*,*,#16318,.T.);
#23807=ORIENTED_EDGE('',*,*,#16622,.T.);
#23808=ORIENTED_EDGE('',*,*,#16581,.T.);
#23809=ORIENTED_EDGE('',*,*,#16621,.T.);
#23810=ORIENTED_EDGE('',*,*,#16309,.T.);
#23811=ORIENTED_EDGE('',*,*,#16620,.T.);
#23812=ORIENTED_EDGE('',*,*,#16590,.T.);
#23813=ORIENTED_EDGE('',*,*,#16619,.T.);
#23814=ORIENTED_EDGE('',*,*,#16300,.T.);
#23815=ORIENTED_EDGE('',*,*,#16618,.T.);
#23816=ORIENTED_EDGE('',*,*,#16599,.T.);
#23817=ORIENTED_EDGE('',*,*,#16617,.T.);
#23818=ORIENTED_EDGE('',*,*,#16291,.T.);
#23819=ORIENTED_EDGE('',*,*,#16653,.T.);
#23820=ORIENTED_EDGE('',*,*,#16608,.T.);
#23821=ORIENTED_EDGE('',*,*,#16652,.T.);
#23822=ORIENTED_EDGE('',*,*,#16523,.T.);
#23823=ORIENTED_EDGE('',*,*,#16651,.T.);
#23824=ORIENTED_EDGE('',*,*,#16446,.T.);
#23825=ORIENTED_EDGE('',*,*,#16650,.T.);
#23826=ORIENTED_EDGE('',*,*,#16455,.T.);
#23827=ORIENTED_EDGE('',*,*,#16649,.T.);
#23828=ORIENTED_EDGE('',*,*,#16437,.T.);
#23829=ORIENTED_EDGE('',*,*,#16648,.T.);
#23830=ORIENTED_EDGE('',*,*,#16464,.T.);
#23831=ORIENTED_EDGE('',*,*,#16647,.T.);
#23832=ORIENTED_EDGE('',*,*,#16428,.T.);
#23833=ORIENTED_EDGE('',*,*,#16646,.T.);
#23834=ORIENTED_EDGE('',*,*,#16473,.T.);
#23835=ORIENTED_EDGE('',*,*,#16645,.T.);
#23836=ORIENTED_EDGE('',*,*,#16419,.T.);
#23837=ORIENTED_EDGE('',*,*,#16644,.T.);
#23838=ORIENTED_EDGE('',*,*,#16482,.T.);
#23839=ORIENTED_EDGE('',*,*,#16643,.T.);
#23840=ORIENTED_EDGE('',*,*,#16410,.T.);
#23841=ORIENTED_EDGE('',*,*,#16642,.T.);
#23842=ORIENTED_EDGE('',*,*,#16491,.T.);
#23843=ORIENTED_EDGE('',*,*,#16641,.T.);
#23844=ORIENTED_EDGE('',*,*,#16401,.T.);
#23845=ORIENTED_EDGE('',*,*,#16640,.T.);
#23846=ORIENTED_EDGE('',*,*,#16500,.T.);
#23847=ORIENTED_EDGE('',*,*,#16639,.T.);
#23848=ORIENTED_EDGE('',*,*,#16392,.T.);
#23849=ORIENTED_EDGE('',*,*,#16638,.T.);
#23850=ORIENTED_EDGE('',*,*,#16509,.T.);
#23851=ORIENTED_EDGE('',*,*,#16637,.T.);
#23852=ORIENTED_EDGE('',*,*,#16383,.T.);
#23853=ORIENTED_EDGE('',*,*,#16636,.T.);
#23854=ORIENTED_EDGE('',*,*,#16518,.T.);
#23855=ORIENTED_EDGE('',*,*,#16635,.T.);
#23856=ORIENTED_EDGE('',*,*,#16374,.T.);
#23857=ORIENTED_EDGE('',*,*,#16634,.T.);
#23858=ORIENTED_EDGE('',*,*,#16363,.T.);
#23859=ORIENTED_EDGE('',*,*,#16655,.F.);
#23860=ORIENTED_EDGE('',*,*,#16654,.T.);
#23861=ORIENTED_EDGE('',*,*,#16275,.T.);
#23862=ORIENTED_EDGE('',*,*,#16286,.T.);
#23863=ORIENTED_EDGE('',*,*,#16284,.T.);
#23864=ORIENTED_EDGE('',*,*,#16282,.T.);
#23865=ORIENTED_EDGE('',*,*,#16280,.T.);
#23866=ORIENTED_EDGE('',*,*,#16278,.T.);
#23867=ORIENTED_EDGE('',*,*,#16656,.F.);
#23868=ORIENTED_EDGE('',*,*,#16657,.T.);
#23869=ORIENTED_EDGE('',*,*,#16658,.T.);
#23870=ORIENTED_EDGE('',*,*,#16659,.T.);
#23871=ORIENTED_EDGE('',*,*,#16660,.F.);
#23872=ORIENTED_EDGE('',*,*,#16661,.T.);
#23873=ORIENTED_EDGE('',*,*,#16656,.T.);
#23874=ORIENTED_EDGE('',*,*,#16662,.T.);
#23875=ORIENTED_EDGE('',*,*,#16663,.F.);
#23876=ORIENTED_EDGE('',*,*,#16664,.T.);
#23877=ORIENTED_EDGE('',*,*,#16660,.T.);
#23878=ORIENTED_EDGE('',*,*,#16665,.T.);
#23879=ORIENTED_EDGE('',*,*,#16666,.F.);
#23880=ORIENTED_EDGE('',*,*,#16667,.T.);
#23881=ORIENTED_EDGE('',*,*,#16663,.T.);
#23882=ORIENTED_EDGE('',*,*,#16668,.T.);
#23883=ORIENTED_EDGE('',*,*,#16669,.F.);
#23884=ORIENTED_EDGE('',*,*,#16670,.T.);
#23885=ORIENTED_EDGE('',*,*,#16666,.T.);
#23886=ORIENTED_EDGE('',*,*,#16671,.T.);
#23887=ORIENTED_EDGE('',*,*,#16672,.F.);
#23888=ORIENTED_EDGE('',*,*,#16673,.T.);
#23889=ORIENTED_EDGE('',*,*,#16669,.T.);
#23890=ORIENTED_EDGE('',*,*,#16674,.T.);
#23891=ORIENTED_EDGE('',*,*,#16675,.F.);
#23892=ORIENTED_EDGE('',*,*,#16676,.T.);
#23893=ORIENTED_EDGE('',*,*,#16672,.T.);
#23894=ORIENTED_EDGE('',*,*,#16677,.T.);
#23895=ORIENTED_EDGE('',*,*,#16678,.F.);
#23896=ORIENTED_EDGE('',*,*,#16679,.T.);
#23897=ORIENTED_EDGE('',*,*,#16675,.T.);
#23898=ORIENTED_EDGE('',*,*,#16680,.T.);
#23899=ORIENTED_EDGE('',*,*,#16681,.F.);
#23900=ORIENTED_EDGE('',*,*,#16682,.T.);
#23901=ORIENTED_EDGE('',*,*,#16678,.T.);
#23902=ORIENTED_EDGE('',*,*,#16683,.T.);
#23903=ORIENTED_EDGE('',*,*,#16684,.F.);
#23904=ORIENTED_EDGE('',*,*,#16685,.T.);
#23905=ORIENTED_EDGE('',*,*,#16681,.T.);
#23906=ORIENTED_EDGE('',*,*,#16686,.T.);
#23907=ORIENTED_EDGE('',*,*,#16687,.F.);
#23908=ORIENTED_EDGE('',*,*,#16688,.T.);
#23909=ORIENTED_EDGE('',*,*,#16684,.T.);
#23910=ORIENTED_EDGE('',*,*,#16689,.T.);
#23911=ORIENTED_EDGE('',*,*,#16690,.F.);
#23912=ORIENTED_EDGE('',*,*,#16691,.T.);
#23913=ORIENTED_EDGE('',*,*,#16687,.T.);
#23914=ORIENTED_EDGE('',*,*,#16692,.T.);
#23915=ORIENTED_EDGE('',*,*,#16693,.F.);
#23916=ORIENTED_EDGE('',*,*,#16694,.T.);
#23917=ORIENTED_EDGE('',*,*,#16690,.T.);
#23918=ORIENTED_EDGE('',*,*,#16695,.T.);
#23919=ORIENTED_EDGE('',*,*,#16696,.F.);
#23920=ORIENTED_EDGE('',*,*,#16697,.T.);
#23921=ORIENTED_EDGE('',*,*,#16693,.T.);
#23922=ORIENTED_EDGE('',*,*,#16698,.T.);
#23923=ORIENTED_EDGE('',*,*,#16699,.F.);
#23924=ORIENTED_EDGE('',*,*,#16700,.T.);
#23925=ORIENTED_EDGE('',*,*,#16696,.T.);
#23926=ORIENTED_EDGE('',*,*,#16701,.T.);
#23927=ORIENTED_EDGE('',*,*,#16702,.F.);
#23928=ORIENTED_EDGE('',*,*,#16703,.T.);
#23929=ORIENTED_EDGE('',*,*,#16699,.T.);
#23930=ORIENTED_EDGE('',*,*,#16704,.T.);
#23931=ORIENTED_EDGE('',*,*,#16705,.F.);
#23932=ORIENTED_EDGE('',*,*,#16706,.T.);
#23933=ORIENTED_EDGE('',*,*,#16702,.T.);
#23934=ORIENTED_EDGE('',*,*,#16707,.T.);
#23935=ORIENTED_EDGE('',*,*,#16708,.F.);
#23936=ORIENTED_EDGE('',*,*,#16709,.T.);
#23937=ORIENTED_EDGE('',*,*,#16705,.T.);
#23938=ORIENTED_EDGE('',*,*,#16710,.T.);
#23939=ORIENTED_EDGE('',*,*,#16711,.F.);
#23940=ORIENTED_EDGE('',*,*,#16712,.T.);
#23941=ORIENTED_EDGE('',*,*,#16708,.T.);
#23942=ORIENTED_EDGE('',*,*,#16713,.T.);
#23943=ORIENTED_EDGE('',*,*,#16714,.F.);
#23944=ORIENTED_EDGE('',*,*,#16715,.F.);
#23945=ORIENTED_EDGE('',*,*,#16716,.T.);
#23946=ORIENTED_EDGE('',*,*,#16711,.T.);
#23947=ORIENTED_EDGE('',*,*,#16717,.T.);
#23948=ORIENTED_EDGE('',*,*,#16718,.F.);
#23949=ORIENTED_EDGE('',*,*,#16719,.T.);
#23950=ORIENTED_EDGE('',*,*,#16720,.F.);
#23951=ORIENTED_EDGE('',*,*,#16721,.F.);
#23952=ORIENTED_EDGE('',*,*,#16722,.F.);
#23953=ORIENTED_EDGE('',*,*,#16723,.T.);
#23954=ORIENTED_EDGE('',*,*,#16718,.T.);
#23955=ORIENTED_EDGE('',*,*,#16724,.F.);
#23956=ORIENTED_EDGE('',*,*,#16725,.F.);
#23957=ORIENTED_EDGE('',*,*,#16726,.T.);
#23958=ORIENTED_EDGE('',*,*,#16722,.T.);
#23959=ORIENTED_EDGE('',*,*,#16727,.F.);
#23960=ORIENTED_EDGE('',*,*,#16728,.F.);
#23961=ORIENTED_EDGE('',*,*,#16729,.T.);
#23962=ORIENTED_EDGE('',*,*,#16725,.T.);
#23963=ORIENTED_EDGE('',*,*,#16730,.F.);
#23964=ORIENTED_EDGE('',*,*,#16731,.F.);
#23965=ORIENTED_EDGE('',*,*,#16732,.T.);
#23966=ORIENTED_EDGE('',*,*,#16728,.T.);
#23967=ORIENTED_EDGE('',*,*,#16733,.F.);
#23968=ORIENTED_EDGE('',*,*,#16734,.F.);
#23969=ORIENTED_EDGE('',*,*,#16735,.T.);
#23970=ORIENTED_EDGE('',*,*,#16731,.T.);
#23971=ORIENTED_EDGE('',*,*,#16736,.F.);
#23972=ORIENTED_EDGE('',*,*,#16737,.F.);
#23973=ORIENTED_EDGE('',*,*,#16738,.T.);
#23974=ORIENTED_EDGE('',*,*,#16734,.T.);
#23975=ORIENTED_EDGE('',*,*,#16739,.F.);
#23976=ORIENTED_EDGE('',*,*,#16740,.F.);
#23977=ORIENTED_EDGE('',*,*,#16741,.T.);
#23978=ORIENTED_EDGE('',*,*,#16737,.T.);
#23979=ORIENTED_EDGE('',*,*,#16742,.F.);
#23980=ORIENTED_EDGE('',*,*,#16743,.F.);
#23981=ORIENTED_EDGE('',*,*,#16744,.T.);
#23982=ORIENTED_EDGE('',*,*,#16740,.T.);
#23983=ORIENTED_EDGE('',*,*,#16745,.F.);
#23984=ORIENTED_EDGE('',*,*,#16746,.F.);
#23985=ORIENTED_EDGE('',*,*,#16747,.T.);
#23986=ORIENTED_EDGE('',*,*,#16743,.T.);
#23987=ORIENTED_EDGE('',*,*,#16748,.F.);
#23988=ORIENTED_EDGE('',*,*,#16749,.F.);
#23989=ORIENTED_EDGE('',*,*,#16750,.T.);
#23990=ORIENTED_EDGE('',*,*,#16746,.T.);
#23991=ORIENTED_EDGE('',*,*,#16751,.F.);
#23992=ORIENTED_EDGE('',*,*,#16752,.F.);
#23993=ORIENTED_EDGE('',*,*,#16753,.T.);
#23994=ORIENTED_EDGE('',*,*,#16749,.T.);
#23995=ORIENTED_EDGE('',*,*,#16754,.F.);
#23996=ORIENTED_EDGE('',*,*,#16755,.F.);
#23997=ORIENTED_EDGE('',*,*,#16756,.T.);
#23998=ORIENTED_EDGE('',*,*,#16752,.T.);
#23999=ORIENTED_EDGE('',*,*,#16757,.F.);
#24000=ORIENTED_EDGE('',*,*,#16758,.F.);
#24001=ORIENTED_EDGE('',*,*,#16759,.T.);
#24002=ORIENTED_EDGE('',*,*,#16755,.T.);
#24003=ORIENTED_EDGE('',*,*,#16760,.F.);
#24004=ORIENTED_EDGE('',*,*,#16761,.F.);
#24005=ORIENTED_EDGE('',*,*,#16762,.T.);
#24006=ORIENTED_EDGE('',*,*,#16758,.T.);
#24007=ORIENTED_EDGE('',*,*,#16763,.F.);
#24008=ORIENTED_EDGE('',*,*,#16764,.F.);
#24009=ORIENTED_EDGE('',*,*,#16765,.T.);
#24010=ORIENTED_EDGE('',*,*,#16761,.T.);
#24011=ORIENTED_EDGE('',*,*,#16766,.F.);
#24012=ORIENTED_EDGE('',*,*,#16767,.F.);
#24013=ORIENTED_EDGE('',*,*,#16768,.T.);
#24014=ORIENTED_EDGE('',*,*,#16764,.T.);
#24015=ORIENTED_EDGE('',*,*,#16769,.F.);
#24016=ORIENTED_EDGE('',*,*,#16770,.F.);
#24017=ORIENTED_EDGE('',*,*,#16771,.T.);
#24018=ORIENTED_EDGE('',*,*,#16767,.T.);
#24019=ORIENTED_EDGE('',*,*,#16772,.F.);
#24020=ORIENTED_EDGE('',*,*,#16773,.F.);
#24021=ORIENTED_EDGE('',*,*,#16774,.T.);
#24022=ORIENTED_EDGE('',*,*,#16770,.T.);
#24023=ORIENTED_EDGE('',*,*,#16775,.F.);
#24024=ORIENTED_EDGE('',*,*,#16720,.T.);
#24025=ORIENTED_EDGE('',*,*,#16776,.T.);
#24026=ORIENTED_EDGE('',*,*,#16777,.F.);
#24027=ORIENTED_EDGE('',*,*,#16778,.T.);
#24028=ORIENTED_EDGE('',*,*,#16778,.F.);
#24029=ORIENTED_EDGE('',*,*,#16779,.F.);
#24030=ORIENTED_EDGE('',*,*,#16717,.F.);
#24031=ORIENTED_EDGE('',*,*,#16713,.F.);
#24032=ORIENTED_EDGE('',*,*,#16710,.F.);
#24033=ORIENTED_EDGE('',*,*,#16707,.F.);
#24034=ORIENTED_EDGE('',*,*,#16704,.F.);
#24035=ORIENTED_EDGE('',*,*,#16701,.F.);
#24036=ORIENTED_EDGE('',*,*,#16698,.F.);
#24037=ORIENTED_EDGE('',*,*,#16695,.F.);
#24038=ORIENTED_EDGE('',*,*,#16692,.F.);
#24039=ORIENTED_EDGE('',*,*,#16689,.F.);
#24040=ORIENTED_EDGE('',*,*,#16686,.F.);
#24041=ORIENTED_EDGE('',*,*,#16683,.F.);
#24042=ORIENTED_EDGE('',*,*,#16680,.F.);
#24043=ORIENTED_EDGE('',*,*,#16677,.F.);
#24044=ORIENTED_EDGE('',*,*,#16674,.F.);
#24045=ORIENTED_EDGE('',*,*,#16671,.F.);
#24046=ORIENTED_EDGE('',*,*,#16668,.F.);
#24047=ORIENTED_EDGE('',*,*,#16665,.F.);
#24048=ORIENTED_EDGE('',*,*,#16662,.F.);
#24049=ORIENTED_EDGE('',*,*,#16659,.F.);
#24050=ORIENTED_EDGE('',*,*,#16780,.F.);
#24051=ORIENTED_EDGE('',*,*,#16781,.T.);
#24052=ORIENTED_EDGE('',*,*,#16775,.T.);
#24053=ORIENTED_EDGE('',*,*,#16772,.T.);
#24054=ORIENTED_EDGE('',*,*,#16769,.T.);
#24055=ORIENTED_EDGE('',*,*,#16766,.T.);
#24056=ORIENTED_EDGE('',*,*,#16763,.T.);
#24057=ORIENTED_EDGE('',*,*,#16760,.T.);
#24058=ORIENTED_EDGE('',*,*,#16757,.T.);
#24059=ORIENTED_EDGE('',*,*,#16754,.T.);
#24060=ORIENTED_EDGE('',*,*,#16751,.T.);
#24061=ORIENTED_EDGE('',*,*,#16748,.T.);
#24062=ORIENTED_EDGE('',*,*,#16745,.T.);
#24063=ORIENTED_EDGE('',*,*,#16742,.T.);
#24064=ORIENTED_EDGE('',*,*,#16739,.T.);
#24065=ORIENTED_EDGE('',*,*,#16736,.T.);
#24066=ORIENTED_EDGE('',*,*,#16733,.T.);
#24067=ORIENTED_EDGE('',*,*,#16730,.T.);
#24068=ORIENTED_EDGE('',*,*,#16727,.T.);
#24069=ORIENTED_EDGE('',*,*,#16724,.T.);
#24070=ORIENTED_EDGE('',*,*,#16721,.T.);
#24071=ORIENTED_EDGE('',*,*,#16782,.T.);
#24072=ORIENTED_EDGE('',*,*,#16783,.T.);
#24073=ORIENTED_EDGE('',*,*,#16784,.T.);
#24074=ORIENTED_EDGE('',*,*,#16785,.T.);
#24075=ORIENTED_EDGE('',*,*,#16780,.T.);
#24076=ORIENTED_EDGE('',*,*,#16773,.T.);
#24077=ORIENTED_EDGE('',*,*,#16781,.F.);
#24078=ORIENTED_EDGE('',*,*,#16785,.F.);
#24079=ORIENTED_EDGE('',*,*,#16786,.T.);
#24080=ORIENTED_EDGE('',*,*,#16776,.F.);
#24081=ORIENTED_EDGE('',*,*,#16719,.F.);
#24082=ORIENTED_EDGE('',*,*,#16723,.F.);
#24083=ORIENTED_EDGE('',*,*,#16726,.F.);
#24084=ORIENTED_EDGE('',*,*,#16729,.F.);
#24085=ORIENTED_EDGE('',*,*,#16732,.F.);
#24086=ORIENTED_EDGE('',*,*,#16735,.F.);
#24087=ORIENTED_EDGE('',*,*,#16738,.F.);
#24088=ORIENTED_EDGE('',*,*,#16741,.F.);
#24089=ORIENTED_EDGE('',*,*,#16744,.F.);
#24090=ORIENTED_EDGE('',*,*,#16747,.F.);
#24091=ORIENTED_EDGE('',*,*,#16750,.F.);
#24092=ORIENTED_EDGE('',*,*,#16753,.F.);
#24093=ORIENTED_EDGE('',*,*,#16756,.F.);
#24094=ORIENTED_EDGE('',*,*,#16759,.F.);
#24095=ORIENTED_EDGE('',*,*,#16762,.F.);
#24096=ORIENTED_EDGE('',*,*,#16765,.F.);
#24097=ORIENTED_EDGE('',*,*,#16768,.F.);
#24098=ORIENTED_EDGE('',*,*,#16771,.F.);
#24099=ORIENTED_EDGE('',*,*,#16774,.F.);
#24100=ORIENTED_EDGE('',*,*,#16786,.F.);
#24101=ORIENTED_EDGE('',*,*,#16784,.F.);
#24102=ORIENTED_EDGE('',*,*,#16657,.F.);
#24103=ORIENTED_EDGE('',*,*,#16661,.F.);
#24104=ORIENTED_EDGE('',*,*,#16664,.F.);
#24105=ORIENTED_EDGE('',*,*,#16667,.F.);
#24106=ORIENTED_EDGE('',*,*,#16670,.F.);
#24107=ORIENTED_EDGE('',*,*,#16673,.F.);
#24108=ORIENTED_EDGE('',*,*,#16676,.F.);
#24109=ORIENTED_EDGE('',*,*,#16679,.F.);
#24110=ORIENTED_EDGE('',*,*,#16682,.F.);
#24111=ORIENTED_EDGE('',*,*,#16685,.F.);
#24112=ORIENTED_EDGE('',*,*,#16688,.F.);
#24113=ORIENTED_EDGE('',*,*,#16691,.F.);
#24114=ORIENTED_EDGE('',*,*,#16694,.F.);
#24115=ORIENTED_EDGE('',*,*,#16697,.F.);
#24116=ORIENTED_EDGE('',*,*,#16700,.F.);
#24117=ORIENTED_EDGE('',*,*,#16703,.F.);
#24118=ORIENTED_EDGE('',*,*,#16706,.F.);
#24119=ORIENTED_EDGE('',*,*,#16709,.F.);
#24120=ORIENTED_EDGE('',*,*,#16712,.F.);
#24121=ORIENTED_EDGE('',*,*,#16716,.F.);
#24122=ORIENTED_EDGE('',*,*,#16715,.T.);
#24123=ORIENTED_EDGE('',*,*,#16787,.T.);
#24124=ORIENTED_EDGE('',*,*,#16788,.T.);
#24125=ORIENTED_EDGE('',*,*,#16787,.F.);
#24126=ORIENTED_EDGE('',*,*,#16789,.T.);
#24127=ORIENTED_EDGE('',*,*,#16777,.T.);
#24128=ORIENTED_EDGE('',*,*,#16714,.T.);
#24129=ORIENTED_EDGE('',*,*,#16779,.T.);
#24130=ORIENTED_EDGE('',*,*,#16789,.F.);
#24131=ORIENTED_EDGE('',*,*,#16790,.F.);
#24132=ORIENTED_EDGE('',*,*,#16788,.F.);
#24133=ORIENTED_EDGE('',*,*,#16791,.F.);
#24134=ORIENTED_EDGE('',*,*,#16792,.F.);
#24135=ORIENTED_EDGE('',*,*,#16793,.F.);
#24136=ORIENTED_EDGE('',*,*,#16794,.F.);
#24137=ORIENTED_EDGE('',*,*,#16795,.F.);
#24138=ORIENTED_EDGE('',*,*,#16796,.F.);
#24139=ORIENTED_EDGE('',*,*,#16797,.F.);
#24140=ORIENTED_EDGE('',*,*,#16798,.F.);
#24141=ORIENTED_EDGE('',*,*,#16799,.F.);
#24142=ORIENTED_EDGE('',*,*,#16800,.F.);
#24143=ORIENTED_EDGE('',*,*,#16801,.F.);
#24144=ORIENTED_EDGE('',*,*,#16802,.F.);
#24145=ORIENTED_EDGE('',*,*,#16803,.T.);
#24146=ORIENTED_EDGE('',*,*,#16798,.T.);
#24147=ORIENTED_EDGE('',*,*,#16796,.T.);
#24148=ORIENTED_EDGE('',*,*,#16794,.T.);
#24149=ORIENTED_EDGE('',*,*,#16792,.T.);
#24150=ORIENTED_EDGE('',*,*,#16802,.T.);
#24151=ORIENTED_EDGE('',*,*,#16800,.T.);
#24152=ORIENTED_EDGE('',*,*,#16803,.F.);
#24153=ORIENTED_EDGE('',*,*,#16804,.F.);
#24154=ORIENTED_EDGE('',*,*,#16805,.T.);
#24155=ORIENTED_EDGE('',*,*,#16791,.T.);
#24156=ORIENTED_EDGE('',*,*,#16806,.F.);
#24157=ORIENTED_EDGE('',*,*,#16807,.F.);
#24158=ORIENTED_EDGE('',*,*,#16808,.T.);
#24159=ORIENTED_EDGE('',*,*,#16801,.T.);
#24160=ORIENTED_EDGE('',*,*,#16805,.F.);
#24161=ORIENTED_EDGE('',*,*,#16809,.F.);
#24162=ORIENTED_EDGE('',*,*,#16810,.T.);
#24163=ORIENTED_EDGE('',*,*,#16799,.T.);
#24164=ORIENTED_EDGE('',*,*,#16808,.F.);
#24165=ORIENTED_EDGE('',*,*,#16811,.F.);
#24166=ORIENTED_EDGE('',*,*,#16812,.T.);
#24167=ORIENTED_EDGE('',*,*,#16797,.T.);
#24168=ORIENTED_EDGE('',*,*,#16810,.F.);
#24169=ORIENTED_EDGE('',*,*,#16813,.F.);
#24170=ORIENTED_EDGE('',*,*,#16814,.T.);
#24171=ORIENTED_EDGE('',*,*,#16795,.T.);
#24172=ORIENTED_EDGE('',*,*,#16812,.F.);
#24173=ORIENTED_EDGE('',*,*,#16815,.F.);
#24174=ORIENTED_EDGE('',*,*,#16806,.T.);
#24175=ORIENTED_EDGE('',*,*,#16793,.T.);
#24176=ORIENTED_EDGE('',*,*,#16814,.F.);
#24177=ORIENTED_EDGE('',*,*,#16816,.F.);
#24178=ORIENTED_EDGE('',*,*,#16817,.T.);
#24179=ORIENTED_EDGE('',*,*,#16818,.F.);
#24180=ORIENTED_EDGE('',*,*,#16819,.F.);
#24181=ORIENTED_EDGE('',*,*,#16820,.F.);
#24182=ORIENTED_EDGE('',*,*,#16819,.T.);
#24183=ORIENTED_EDGE('',*,*,#16821,.T.);
#24184=ORIENTED_EDGE('',*,*,#16822,.F.);
#24185=ORIENTED_EDGE('',*,*,#16821,.F.);
#24186=ORIENTED_EDGE('',*,*,#16818,.T.);
#24187=ORIENTED_EDGE('',*,*,#16823,.T.);
#24188=ORIENTED_EDGE('',*,*,#16824,.F.);
#24189=ORIENTED_EDGE('',*,*,#16823,.F.);
#24190=ORIENTED_EDGE('',*,*,#16817,.F.);
#24191=ORIENTED_EDGE('',*,*,#16825,.F.);
#24192=ORIENTED_EDGE('',*,*,#16826,.T.);
#24193=ORIENTED_EDGE('',*,*,#16827,.F.);
#24194=ORIENTED_EDGE('',*,*,#16828,.F.);
#24195=ORIENTED_EDGE('',*,*,#16829,.F.);
#24196=ORIENTED_EDGE('',*,*,#16828,.T.);
#24197=ORIENTED_EDGE('',*,*,#16830,.T.);
#24198=ORIENTED_EDGE('',*,*,#16831,.F.);
#24199=ORIENTED_EDGE('',*,*,#16830,.F.);
#24200=ORIENTED_EDGE('',*,*,#16827,.T.);
#24201=ORIENTED_EDGE('',*,*,#16832,.T.);
#24202=ORIENTED_EDGE('',*,*,#16833,.F.);
#24203=ORIENTED_EDGE('',*,*,#16832,.F.);
#24204=ORIENTED_EDGE('',*,*,#16826,.F.);
#24205=ORIENTED_EDGE('',*,*,#16834,.F.);
#24206=ORIENTED_EDGE('',*,*,#16835,.T.);
#24207=ORIENTED_EDGE('',*,*,#16836,.F.);
#24208=ORIENTED_EDGE('',*,*,#16837,.F.);
#24209=ORIENTED_EDGE('',*,*,#16838,.F.);
#24210=ORIENTED_EDGE('',*,*,#16837,.T.);
#24211=ORIENTED_EDGE('',*,*,#16839,.T.);
#24212=ORIENTED_EDGE('',*,*,#16840,.F.);
#24213=ORIENTED_EDGE('',*,*,#16839,.F.);
#24214=ORIENTED_EDGE('',*,*,#16836,.T.);
#24215=ORIENTED_EDGE('',*,*,#16841,.T.);
#24216=ORIENTED_EDGE('',*,*,#16842,.F.);
#24217=ORIENTED_EDGE('',*,*,#16841,.F.);
#24218=ORIENTED_EDGE('',*,*,#16835,.F.);
#24219=ORIENTED_EDGE('',*,*,#16843,.F.);
#24220=ORIENTED_EDGE('',*,*,#16844,.T.);
#24221=ORIENTED_EDGE('',*,*,#16845,.F.);
#24222=ORIENTED_EDGE('',*,*,#16846,.F.);
#24223=ORIENTED_EDGE('',*,*,#16847,.F.);
#24224=ORIENTED_EDGE('',*,*,#16846,.T.);
#24225=ORIENTED_EDGE('',*,*,#16848,.T.);
#24226=ORIENTED_EDGE('',*,*,#16849,.F.);
#24227=ORIENTED_EDGE('',*,*,#16848,.F.);
#24228=ORIENTED_EDGE('',*,*,#16845,.T.);
#24229=ORIENTED_EDGE('',*,*,#16850,.T.);
#24230=ORIENTED_EDGE('',*,*,#16851,.F.);
#24231=ORIENTED_EDGE('',*,*,#16850,.F.);
#24232=ORIENTED_EDGE('',*,*,#16844,.F.);
#24233=ORIENTED_EDGE('',*,*,#16852,.F.);
#24234=ORIENTED_EDGE('',*,*,#16853,.T.);
#24235=ORIENTED_EDGE('',*,*,#16854,.F.);
#24236=ORIENTED_EDGE('',*,*,#16855,.F.);
#24237=ORIENTED_EDGE('',*,*,#16856,.F.);
#24238=ORIENTED_EDGE('',*,*,#16855,.T.);
#24239=ORIENTED_EDGE('',*,*,#16857,.T.);
#24240=ORIENTED_EDGE('',*,*,#16858,.F.);
#24241=ORIENTED_EDGE('',*,*,#16857,.F.);
#24242=ORIENTED_EDGE('',*,*,#16854,.T.);
#24243=ORIENTED_EDGE('',*,*,#16859,.T.);
#24244=ORIENTED_EDGE('',*,*,#16860,.F.);
#24245=ORIENTED_EDGE('',*,*,#16859,.F.);
#24246=ORIENTED_EDGE('',*,*,#16853,.F.);
#24247=ORIENTED_EDGE('',*,*,#16861,.F.);
#24248=ORIENTED_EDGE('',*,*,#16862,.T.);
#24249=ORIENTED_EDGE('',*,*,#16863,.F.);
#24250=ORIENTED_EDGE('',*,*,#16864,.F.);
#24251=ORIENTED_EDGE('',*,*,#16865,.F.);
#24252=ORIENTED_EDGE('',*,*,#16864,.T.);
#24253=ORIENTED_EDGE('',*,*,#16866,.T.);
#24254=ORIENTED_EDGE('',*,*,#16867,.F.);
#24255=ORIENTED_EDGE('',*,*,#16866,.F.);
#24256=ORIENTED_EDGE('',*,*,#16863,.T.);
#24257=ORIENTED_EDGE('',*,*,#16868,.T.);
#24258=ORIENTED_EDGE('',*,*,#16869,.F.);
#24259=ORIENTED_EDGE('',*,*,#16868,.F.);
#24260=ORIENTED_EDGE('',*,*,#16862,.F.);
#24261=ORIENTED_EDGE('',*,*,#16870,.F.);
#24262=ORIENTED_EDGE('',*,*,#16871,.T.);
#24263=ORIENTED_EDGE('',*,*,#16872,.F.);
#24264=ORIENTED_EDGE('',*,*,#16873,.F.);
#24265=ORIENTED_EDGE('',*,*,#16874,.F.);
#24266=ORIENTED_EDGE('',*,*,#16873,.T.);
#24267=ORIENTED_EDGE('',*,*,#16875,.T.);
#24268=ORIENTED_EDGE('',*,*,#16876,.F.);
#24269=ORIENTED_EDGE('',*,*,#16875,.F.);
#24270=ORIENTED_EDGE('',*,*,#16872,.T.);
#24271=ORIENTED_EDGE('',*,*,#16877,.T.);
#24272=ORIENTED_EDGE('',*,*,#16878,.F.);
#24273=ORIENTED_EDGE('',*,*,#16877,.F.);
#24274=ORIENTED_EDGE('',*,*,#16871,.F.);
#24275=ORIENTED_EDGE('',*,*,#16879,.F.);
#24276=ORIENTED_EDGE('',*,*,#16880,.T.);
#24277=ORIENTED_EDGE('',*,*,#16881,.F.);
#24278=ORIENTED_EDGE('',*,*,#16882,.F.);
#24279=ORIENTED_EDGE('',*,*,#16883,.F.);
#24280=ORIENTED_EDGE('',*,*,#16882,.T.);
#24281=ORIENTED_EDGE('',*,*,#16884,.T.);
#24282=ORIENTED_EDGE('',*,*,#16885,.F.);
#24283=ORIENTED_EDGE('',*,*,#16884,.F.);
#24284=ORIENTED_EDGE('',*,*,#16881,.T.);
#24285=ORIENTED_EDGE('',*,*,#16886,.T.);
#24286=ORIENTED_EDGE('',*,*,#16887,.F.);
#24287=ORIENTED_EDGE('',*,*,#16886,.F.);
#24288=ORIENTED_EDGE('',*,*,#16880,.F.);
#24289=ORIENTED_EDGE('',*,*,#16888,.F.);
#24290=ORIENTED_EDGE('',*,*,#16889,.T.);
#24291=ORIENTED_EDGE('',*,*,#16890,.F.);
#24292=ORIENTED_EDGE('',*,*,#16891,.F.);
#24293=ORIENTED_EDGE('',*,*,#16892,.F.);
#24294=ORIENTED_EDGE('',*,*,#16891,.T.);
#24295=ORIENTED_EDGE('',*,*,#16893,.T.);
#24296=ORIENTED_EDGE('',*,*,#16894,.F.);
#24297=ORIENTED_EDGE('',*,*,#16895,.F.);
#24298=ORIENTED_EDGE('',*,*,#16893,.F.);
#24299=ORIENTED_EDGE('',*,*,#16890,.T.);
#24300=ORIENTED_EDGE('',*,*,#16896,.T.);
#24301=ORIENTED_EDGE('',*,*,#16897,.F.);
#24302=ORIENTED_EDGE('',*,*,#16896,.F.);
#24303=ORIENTED_EDGE('',*,*,#16889,.F.);
#24304=ORIENTED_EDGE('',*,*,#16898,.F.);
#24305=ORIENTED_EDGE('',*,*,#16899,.F.);
#24306=ORIENTED_EDGE('',*,*,#16900,.T.);
#24307=ORIENTED_EDGE('',*,*,#16901,.F.);
#24308=ORIENTED_EDGE('',*,*,#16902,.F.);
#24309=ORIENTED_EDGE('',*,*,#16903,.F.);
#24310=ORIENTED_EDGE('',*,*,#16902,.T.);
#24311=ORIENTED_EDGE('',*,*,#16904,.T.);
#24312=ORIENTED_EDGE('',*,*,#16905,.F.);
#24313=ORIENTED_EDGE('',*,*,#16904,.F.);
#24314=ORIENTED_EDGE('',*,*,#16901,.T.);
#24315=ORIENTED_EDGE('',*,*,#16906,.T.);
#24316=ORIENTED_EDGE('',*,*,#16907,.F.);
#24317=ORIENTED_EDGE('',*,*,#16906,.F.);
#24318=ORIENTED_EDGE('',*,*,#16900,.F.);
#24319=ORIENTED_EDGE('',*,*,#16908,.F.);
#24320=ORIENTED_EDGE('',*,*,#16909,.T.);
#24321=ORIENTED_EDGE('',*,*,#16910,.F.);
#24322=ORIENTED_EDGE('',*,*,#16911,.F.);
#24323=ORIENTED_EDGE('',*,*,#16912,.F.);
#24324=ORIENTED_EDGE('',*,*,#16911,.T.);
#24325=ORIENTED_EDGE('',*,*,#16913,.T.);
#24326=ORIENTED_EDGE('',*,*,#16914,.F.);
#24327=ORIENTED_EDGE('',*,*,#16913,.F.);
#24328=ORIENTED_EDGE('',*,*,#16910,.T.);
#24329=ORIENTED_EDGE('',*,*,#16915,.T.);
#24330=ORIENTED_EDGE('',*,*,#16916,.F.);
#24331=ORIENTED_EDGE('',*,*,#16915,.F.);
#24332=ORIENTED_EDGE('',*,*,#16909,.F.);
#24333=ORIENTED_EDGE('',*,*,#16917,.F.);
#24334=ORIENTED_EDGE('',*,*,#16918,.T.);
#24335=ORIENTED_EDGE('',*,*,#16919,.F.);
#24336=ORIENTED_EDGE('',*,*,#16920,.F.);
#24337=ORIENTED_EDGE('',*,*,#16921,.F.);
#24338=ORIENTED_EDGE('',*,*,#16920,.T.);
#24339=ORIENTED_EDGE('',*,*,#16922,.T.);
#24340=ORIENTED_EDGE('',*,*,#16923,.F.);
#24341=ORIENTED_EDGE('',*,*,#16922,.F.);
#24342=ORIENTED_EDGE('',*,*,#16919,.T.);
#24343=ORIENTED_EDGE('',*,*,#16924,.T.);
#24344=ORIENTED_EDGE('',*,*,#16925,.F.);
#24345=ORIENTED_EDGE('',*,*,#16924,.F.);
#24346=ORIENTED_EDGE('',*,*,#16918,.F.);
#24347=ORIENTED_EDGE('',*,*,#16926,.F.);
#24348=ORIENTED_EDGE('',*,*,#16927,.T.);
#24349=ORIENTED_EDGE('',*,*,#16928,.F.);
#24350=ORIENTED_EDGE('',*,*,#16929,.F.);
#24351=ORIENTED_EDGE('',*,*,#16930,.F.);
#24352=ORIENTED_EDGE('',*,*,#16929,.T.);
#24353=ORIENTED_EDGE('',*,*,#16931,.T.);
#24354=ORIENTED_EDGE('',*,*,#16932,.F.);
#24355=ORIENTED_EDGE('',*,*,#16931,.F.);
#24356=ORIENTED_EDGE('',*,*,#16928,.T.);
#24357=ORIENTED_EDGE('',*,*,#16933,.T.);
#24358=ORIENTED_EDGE('',*,*,#16934,.F.);
#24359=ORIENTED_EDGE('',*,*,#16933,.F.);
#24360=ORIENTED_EDGE('',*,*,#16927,.F.);
#24361=ORIENTED_EDGE('',*,*,#16935,.F.);
#24362=ORIENTED_EDGE('',*,*,#16936,.T.);
#24363=ORIENTED_EDGE('',*,*,#16937,.F.);
#24364=ORIENTED_EDGE('',*,*,#16938,.F.);
#24365=ORIENTED_EDGE('',*,*,#16939,.F.);
#24366=ORIENTED_EDGE('',*,*,#16938,.T.);
#24367=ORIENTED_EDGE('',*,*,#16940,.T.);
#24368=ORIENTED_EDGE('',*,*,#16941,.F.);
#24369=ORIENTED_EDGE('',*,*,#16940,.F.);
#24370=ORIENTED_EDGE('',*,*,#16937,.T.);
#24371=ORIENTED_EDGE('',*,*,#16942,.T.);
#24372=ORIENTED_EDGE('',*,*,#16943,.F.);
#24373=ORIENTED_EDGE('',*,*,#16942,.F.);
#24374=ORIENTED_EDGE('',*,*,#16936,.F.);
#24375=ORIENTED_EDGE('',*,*,#16944,.F.);
#24376=ORIENTED_EDGE('',*,*,#16945,.T.);
#24377=ORIENTED_EDGE('',*,*,#16946,.F.);
#24378=ORIENTED_EDGE('',*,*,#16947,.F.);
#24379=ORIENTED_EDGE('',*,*,#16948,.F.);
#24380=ORIENTED_EDGE('',*,*,#16947,.T.);
#24381=ORIENTED_EDGE('',*,*,#16949,.T.);
#24382=ORIENTED_EDGE('',*,*,#16950,.F.);
#24383=ORIENTED_EDGE('',*,*,#16949,.F.);
#24384=ORIENTED_EDGE('',*,*,#16946,.T.);
#24385=ORIENTED_EDGE('',*,*,#16951,.T.);
#24386=ORIENTED_EDGE('',*,*,#16952,.F.);
#24387=ORIENTED_EDGE('',*,*,#16951,.F.);
#24388=ORIENTED_EDGE('',*,*,#16945,.F.);
#24389=ORIENTED_EDGE('',*,*,#16953,.F.);
#24390=ORIENTED_EDGE('',*,*,#16954,.T.);
#24391=ORIENTED_EDGE('',*,*,#16955,.F.);
#24392=ORIENTED_EDGE('',*,*,#16956,.F.);
#24393=ORIENTED_EDGE('',*,*,#16957,.F.);
#24394=ORIENTED_EDGE('',*,*,#16956,.T.);
#24395=ORIENTED_EDGE('',*,*,#16958,.T.);
#24396=ORIENTED_EDGE('',*,*,#16959,.F.);
#24397=ORIENTED_EDGE('',*,*,#16958,.F.);
#24398=ORIENTED_EDGE('',*,*,#16955,.T.);
#24399=ORIENTED_EDGE('',*,*,#16960,.T.);
#24400=ORIENTED_EDGE('',*,*,#16961,.F.);
#24401=ORIENTED_EDGE('',*,*,#16960,.F.);
#24402=ORIENTED_EDGE('',*,*,#16954,.F.);
#24403=ORIENTED_EDGE('',*,*,#16962,.F.);
#24404=ORIENTED_EDGE('',*,*,#16963,.T.);
#24405=ORIENTED_EDGE('',*,*,#16964,.F.);
#24406=ORIENTED_EDGE('',*,*,#16965,.F.);
#24407=ORIENTED_EDGE('',*,*,#16966,.F.);
#24408=ORIENTED_EDGE('',*,*,#16965,.T.);
#24409=ORIENTED_EDGE('',*,*,#16967,.T.);
#24410=ORIENTED_EDGE('',*,*,#16968,.F.);
#24411=ORIENTED_EDGE('',*,*,#16967,.F.);
#24412=ORIENTED_EDGE('',*,*,#16964,.T.);
#24413=ORIENTED_EDGE('',*,*,#16969,.T.);
#24414=ORIENTED_EDGE('',*,*,#16970,.F.);
#24415=ORIENTED_EDGE('',*,*,#16969,.F.);
#24416=ORIENTED_EDGE('',*,*,#16963,.F.);
#24417=ORIENTED_EDGE('',*,*,#16971,.F.);
#24418=ORIENTED_EDGE('',*,*,#16972,.T.);
#24419=ORIENTED_EDGE('',*,*,#16973,.F.);
#24420=ORIENTED_EDGE('',*,*,#16974,.F.);
#24421=ORIENTED_EDGE('',*,*,#16975,.F.);
#24422=ORIENTED_EDGE('',*,*,#16974,.T.);
#24423=ORIENTED_EDGE('',*,*,#16976,.T.);
#24424=ORIENTED_EDGE('',*,*,#16977,.F.);
#24425=ORIENTED_EDGE('',*,*,#16976,.F.);
#24426=ORIENTED_EDGE('',*,*,#16973,.T.);
#24427=ORIENTED_EDGE('',*,*,#16978,.T.);
#24428=ORIENTED_EDGE('',*,*,#16979,.F.);
#24429=ORIENTED_EDGE('',*,*,#16978,.F.);
#24430=ORIENTED_EDGE('',*,*,#16972,.F.);
#24431=ORIENTED_EDGE('',*,*,#16980,.F.);
#24432=ORIENTED_EDGE('',*,*,#16981,.T.);
#24433=ORIENTED_EDGE('',*,*,#16982,.F.);
#24434=ORIENTED_EDGE('',*,*,#16983,.F.);
#24435=ORIENTED_EDGE('',*,*,#16984,.F.);
#24436=ORIENTED_EDGE('',*,*,#16983,.T.);
#24437=ORIENTED_EDGE('',*,*,#16985,.T.);
#24438=ORIENTED_EDGE('',*,*,#16986,.F.);
#24439=ORIENTED_EDGE('',*,*,#16985,.F.);
#24440=ORIENTED_EDGE('',*,*,#16982,.T.);
#24441=ORIENTED_EDGE('',*,*,#16987,.T.);
#24442=ORIENTED_EDGE('',*,*,#16988,.F.);
#24443=ORIENTED_EDGE('',*,*,#16987,.F.);
#24444=ORIENTED_EDGE('',*,*,#16981,.F.);
#24445=ORIENTED_EDGE('',*,*,#16989,.F.);
#24446=ORIENTED_EDGE('',*,*,#16990,.T.);
#24447=ORIENTED_EDGE('',*,*,#16991,.F.);
#24448=ORIENTED_EDGE('',*,*,#16992,.F.);
#24449=ORIENTED_EDGE('',*,*,#16993,.F.);
#24450=ORIENTED_EDGE('',*,*,#16992,.T.);
#24451=ORIENTED_EDGE('',*,*,#16994,.T.);
#24452=ORIENTED_EDGE('',*,*,#16995,.F.);
#24453=ORIENTED_EDGE('',*,*,#16994,.F.);
#24454=ORIENTED_EDGE('',*,*,#16991,.T.);
#24455=ORIENTED_EDGE('',*,*,#16996,.T.);
#24456=ORIENTED_EDGE('',*,*,#16997,.F.);
#24457=ORIENTED_EDGE('',*,*,#16996,.F.);
#24458=ORIENTED_EDGE('',*,*,#16990,.F.);
#24459=ORIENTED_EDGE('',*,*,#16998,.F.);
#24460=ORIENTED_EDGE('',*,*,#16999,.T.);
#24461=ORIENTED_EDGE('',*,*,#17000,.F.);
#24462=ORIENTED_EDGE('',*,*,#17001,.F.);
#24463=ORIENTED_EDGE('',*,*,#17002,.F.);
#24464=ORIENTED_EDGE('',*,*,#17001,.T.);
#24465=ORIENTED_EDGE('',*,*,#17003,.T.);
#24466=ORIENTED_EDGE('',*,*,#17004,.F.);
#24467=ORIENTED_EDGE('',*,*,#17003,.F.);
#24468=ORIENTED_EDGE('',*,*,#17000,.T.);
#24469=ORIENTED_EDGE('',*,*,#17005,.T.);
#24470=ORIENTED_EDGE('',*,*,#17006,.F.);
#24471=ORIENTED_EDGE('',*,*,#17005,.F.);
#24472=ORIENTED_EDGE('',*,*,#16999,.F.);
#24473=ORIENTED_EDGE('',*,*,#17007,.F.);
#24474=ORIENTED_EDGE('',*,*,#17008,.T.);
#24475=ORIENTED_EDGE('',*,*,#17009,.F.);
#24476=ORIENTED_EDGE('',*,*,#17010,.F.);
#24477=ORIENTED_EDGE('',*,*,#17011,.F.);
#24478=ORIENTED_EDGE('',*,*,#17010,.T.);
#24479=ORIENTED_EDGE('',*,*,#17012,.T.);
#24480=ORIENTED_EDGE('',*,*,#17013,.F.);
#24481=ORIENTED_EDGE('',*,*,#17012,.F.);
#24482=ORIENTED_EDGE('',*,*,#17009,.T.);
#24483=ORIENTED_EDGE('',*,*,#17014,.T.);
#24484=ORIENTED_EDGE('',*,*,#17015,.F.);
#24485=ORIENTED_EDGE('',*,*,#17014,.F.);
#24486=ORIENTED_EDGE('',*,*,#17008,.F.);
#24487=ORIENTED_EDGE('',*,*,#17016,.F.);
#24488=ORIENTED_EDGE('',*,*,#17017,.T.);
#24489=ORIENTED_EDGE('',*,*,#17018,.F.);
#24490=ORIENTED_EDGE('',*,*,#17019,.F.);
#24491=ORIENTED_EDGE('',*,*,#17020,.F.);
#24492=ORIENTED_EDGE('',*,*,#17019,.T.);
#24493=ORIENTED_EDGE('',*,*,#17021,.T.);
#24494=ORIENTED_EDGE('',*,*,#17022,.F.);
#24495=ORIENTED_EDGE('',*,*,#17021,.F.);
#24496=ORIENTED_EDGE('',*,*,#17018,.T.);
#24497=ORIENTED_EDGE('',*,*,#17023,.T.);
#24498=ORIENTED_EDGE('',*,*,#17024,.F.);
#24499=ORIENTED_EDGE('',*,*,#17023,.F.);
#24500=ORIENTED_EDGE('',*,*,#17017,.F.);
#24501=ORIENTED_EDGE('',*,*,#17025,.F.);
#24502=ORIENTED_EDGE('',*,*,#17026,.T.);
#24503=ORIENTED_EDGE('',*,*,#17027,.F.);
#24504=ORIENTED_EDGE('',*,*,#17028,.F.);
#24505=ORIENTED_EDGE('',*,*,#17029,.F.);
#24506=ORIENTED_EDGE('',*,*,#17028,.T.);
#24507=ORIENTED_EDGE('',*,*,#17030,.T.);
#24508=ORIENTED_EDGE('',*,*,#17031,.F.);
#24509=ORIENTED_EDGE('',*,*,#17030,.F.);
#24510=ORIENTED_EDGE('',*,*,#17027,.T.);
#24511=ORIENTED_EDGE('',*,*,#17032,.T.);
#24512=ORIENTED_EDGE('',*,*,#17033,.F.);
#24513=ORIENTED_EDGE('',*,*,#17032,.F.);
#24514=ORIENTED_EDGE('',*,*,#17026,.F.);
#24515=ORIENTED_EDGE('',*,*,#17034,.F.);
#24516=ORIENTED_EDGE('',*,*,#17035,.T.);
#24517=ORIENTED_EDGE('',*,*,#17036,.F.);
#24518=ORIENTED_EDGE('',*,*,#17037,.F.);
#24519=ORIENTED_EDGE('',*,*,#17038,.F.);
#24520=ORIENTED_EDGE('',*,*,#17037,.T.);
#24521=ORIENTED_EDGE('',*,*,#17039,.T.);
#24522=ORIENTED_EDGE('',*,*,#17040,.F.);
#24523=ORIENTED_EDGE('',*,*,#17039,.F.);
#24524=ORIENTED_EDGE('',*,*,#17036,.T.);
#24525=ORIENTED_EDGE('',*,*,#17041,.T.);
#24526=ORIENTED_EDGE('',*,*,#17042,.F.);
#24527=ORIENTED_EDGE('',*,*,#17041,.F.);
#24528=ORIENTED_EDGE('',*,*,#17035,.F.);
#24529=ORIENTED_EDGE('',*,*,#17043,.F.);
#24530=ORIENTED_EDGE('',*,*,#17044,.T.);
#24531=ORIENTED_EDGE('',*,*,#17045,.F.);
#24532=ORIENTED_EDGE('',*,*,#17046,.F.);
#24533=ORIENTED_EDGE('',*,*,#17047,.F.);
#24534=ORIENTED_EDGE('',*,*,#17046,.T.);
#24535=ORIENTED_EDGE('',*,*,#17048,.T.);
#24536=ORIENTED_EDGE('',*,*,#17049,.F.);
#24537=ORIENTED_EDGE('',*,*,#17048,.F.);
#24538=ORIENTED_EDGE('',*,*,#17045,.T.);
#24539=ORIENTED_EDGE('',*,*,#17050,.T.);
#24540=ORIENTED_EDGE('',*,*,#17051,.F.);
#24541=ORIENTED_EDGE('',*,*,#17050,.F.);
#24542=ORIENTED_EDGE('',*,*,#17044,.F.);
#24543=ORIENTED_EDGE('',*,*,#17052,.F.);
#24544=ORIENTED_EDGE('',*,*,#17053,.T.);
#24545=ORIENTED_EDGE('',*,*,#17054,.T.);
#24546=ORIENTED_EDGE('',*,*,#17055,.F.);
#24547=ORIENTED_EDGE('',*,*,#17056,.T.);
#24548=ORIENTED_EDGE('',*,*,#17057,.F.);
#24549=ORIENTED_EDGE('',*,*,#17053,.F.);
#24550=ORIENTED_EDGE('',*,*,#17058,.F.);
#24551=ORIENTED_EDGE('',*,*,#17054,.F.);
#24552=ORIENTED_EDGE('',*,*,#17057,.T.);
#24553=ORIENTED_EDGE('',*,*,#17059,.T.);
#24554=ORIENTED_EDGE('',*,*,#17060,.F.);
#24555=ORIENTED_EDGE('',*,*,#17059,.F.);
#24556=ORIENTED_EDGE('',*,*,#17056,.F.);
#24557=ORIENTED_EDGE('',*,*,#17061,.F.);
#24558=ORIENTED_EDGE('',*,*,#17062,.T.);
#24559=ORIENTED_EDGE('',*,*,#17063,.F.);
#24560=ORIENTED_EDGE('',*,*,#17064,.F.);
#24561=ORIENTED_EDGE('',*,*,#17065,.F.);
#24562=ORIENTED_EDGE('',*,*,#17064,.T.);
#24563=ORIENTED_EDGE('',*,*,#17066,.T.);
#24564=ORIENTED_EDGE('',*,*,#17067,.F.);
#24565=ORIENTED_EDGE('',*,*,#17066,.F.);
#24566=ORIENTED_EDGE('',*,*,#17063,.T.);
#24567=ORIENTED_EDGE('',*,*,#17068,.T.);
#24568=ORIENTED_EDGE('',*,*,#17069,.F.);
#24569=ORIENTED_EDGE('',*,*,#17068,.F.);
#24570=ORIENTED_EDGE('',*,*,#17062,.F.);
#24571=ORIENTED_EDGE('',*,*,#17070,.F.);
#24572=ORIENTED_EDGE('',*,*,#17071,.T.);
#24573=ORIENTED_EDGE('',*,*,#17072,.F.);
#24574=ORIENTED_EDGE('',*,*,#17073,.F.);
#24575=ORIENTED_EDGE('',*,*,#17074,.F.);
#24576=ORIENTED_EDGE('',*,*,#17073,.T.);
#24577=ORIENTED_EDGE('',*,*,#17075,.T.);
#24578=ORIENTED_EDGE('',*,*,#17076,.F.);
#24579=ORIENTED_EDGE('',*,*,#17075,.F.);
#24580=ORIENTED_EDGE('',*,*,#17072,.T.);
#24581=ORIENTED_EDGE('',*,*,#17077,.T.);
#24582=ORIENTED_EDGE('',*,*,#17078,.F.);
#24583=ORIENTED_EDGE('',*,*,#17077,.F.);
#24584=ORIENTED_EDGE('',*,*,#17071,.F.);
#24585=ORIENTED_EDGE('',*,*,#17079,.F.);
#24586=ORIENTED_EDGE('',*,*,#17080,.T.);
#24587=ORIENTED_EDGE('',*,*,#17081,.F.);
#24588=ORIENTED_EDGE('',*,*,#17082,.F.);
#24589=ORIENTED_EDGE('',*,*,#17083,.F.);
#24590=ORIENTED_EDGE('',*,*,#17082,.T.);
#24591=ORIENTED_EDGE('',*,*,#17084,.T.);
#24592=ORIENTED_EDGE('',*,*,#17085,.F.);
#24593=ORIENTED_EDGE('',*,*,#17084,.F.);
#24594=ORIENTED_EDGE('',*,*,#17081,.T.);
#24595=ORIENTED_EDGE('',*,*,#17086,.T.);
#24596=ORIENTED_EDGE('',*,*,#17087,.F.);
#24597=ORIENTED_EDGE('',*,*,#17086,.F.);
#24598=ORIENTED_EDGE('',*,*,#17080,.F.);
#24599=ORIENTED_EDGE('',*,*,#17088,.F.);
#24600=ORIENTED_EDGE('',*,*,#17089,.T.);
#24601=ORIENTED_EDGE('',*,*,#17090,.F.);
#24602=ORIENTED_EDGE('',*,*,#17091,.F.);
#24603=ORIENTED_EDGE('',*,*,#17092,.F.);
#24604=ORIENTED_EDGE('',*,*,#17091,.T.);
#24605=ORIENTED_EDGE('',*,*,#17093,.T.);
#24606=ORIENTED_EDGE('',*,*,#17094,.F.);
#24607=ORIENTED_EDGE('',*,*,#17093,.F.);
#24608=ORIENTED_EDGE('',*,*,#17090,.T.);
#24609=ORIENTED_EDGE('',*,*,#17095,.T.);
#24610=ORIENTED_EDGE('',*,*,#17096,.F.);
#24611=ORIENTED_EDGE('',*,*,#17095,.F.);
#24612=ORIENTED_EDGE('',*,*,#17089,.F.);
#24613=ORIENTED_EDGE('',*,*,#17097,.F.);
#24614=ORIENTED_EDGE('',*,*,#17098,.T.);
#24615=ORIENTED_EDGE('',*,*,#17099,.F.);
#24616=ORIENTED_EDGE('',*,*,#17100,.F.);
#24617=ORIENTED_EDGE('',*,*,#17101,.F.);
#24618=ORIENTED_EDGE('',*,*,#17100,.T.);
#24619=ORIENTED_EDGE('',*,*,#17102,.T.);
#24620=ORIENTED_EDGE('',*,*,#17103,.F.);
#24621=ORIENTED_EDGE('',*,*,#17102,.F.);
#24622=ORIENTED_EDGE('',*,*,#17099,.T.);
#24623=ORIENTED_EDGE('',*,*,#17104,.T.);
#24624=ORIENTED_EDGE('',*,*,#17105,.F.);
#24625=ORIENTED_EDGE('',*,*,#17104,.F.);
#24626=ORIENTED_EDGE('',*,*,#17098,.F.);
#24627=ORIENTED_EDGE('',*,*,#17106,.F.);
#24628=ORIENTED_EDGE('',*,*,#17107,.T.);
#24629=ORIENTED_EDGE('',*,*,#17108,.F.);
#24630=ORIENTED_EDGE('',*,*,#17109,.F.);
#24631=ORIENTED_EDGE('',*,*,#17110,.F.);
#24632=ORIENTED_EDGE('',*,*,#17109,.T.);
#24633=ORIENTED_EDGE('',*,*,#17111,.T.);
#24634=ORIENTED_EDGE('',*,*,#17112,.F.);
#24635=ORIENTED_EDGE('',*,*,#17111,.F.);
#24636=ORIENTED_EDGE('',*,*,#17108,.T.);
#24637=ORIENTED_EDGE('',*,*,#17113,.T.);
#24638=ORIENTED_EDGE('',*,*,#17114,.F.);
#24639=ORIENTED_EDGE('',*,*,#17113,.F.);
#24640=ORIENTED_EDGE('',*,*,#17107,.F.);
#24641=ORIENTED_EDGE('',*,*,#17115,.F.);
#24642=ORIENTED_EDGE('',*,*,#17116,.T.);
#24643=ORIENTED_EDGE('',*,*,#17117,.F.);
#24644=ORIENTED_EDGE('',*,*,#17118,.F.);
#24645=ORIENTED_EDGE('',*,*,#17119,.F.);
#24646=ORIENTED_EDGE('',*,*,#17118,.T.);
#24647=ORIENTED_EDGE('',*,*,#17120,.T.);
#24648=ORIENTED_EDGE('',*,*,#17121,.F.);
#24649=ORIENTED_EDGE('',*,*,#17120,.F.);
#24650=ORIENTED_EDGE('',*,*,#17117,.T.);
#24651=ORIENTED_EDGE('',*,*,#17122,.T.);
#24652=ORIENTED_EDGE('',*,*,#17123,.F.);
#24653=ORIENTED_EDGE('',*,*,#17122,.F.);
#24654=ORIENTED_EDGE('',*,*,#17116,.F.);
#24655=ORIENTED_EDGE('',*,*,#17124,.F.);
#24656=ORIENTED_EDGE('',*,*,#17125,.T.);
#24657=ORIENTED_EDGE('',*,*,#17126,.F.);
#24658=ORIENTED_EDGE('',*,*,#17127,.F.);
#24659=ORIENTED_EDGE('',*,*,#17128,.F.);
#24660=ORIENTED_EDGE('',*,*,#17127,.T.);
#24661=ORIENTED_EDGE('',*,*,#17129,.T.);
#24662=ORIENTED_EDGE('',*,*,#17130,.F.);
#24663=ORIENTED_EDGE('',*,*,#17129,.F.);
#24664=ORIENTED_EDGE('',*,*,#17126,.T.);
#24665=ORIENTED_EDGE('',*,*,#17131,.T.);
#24666=ORIENTED_EDGE('',*,*,#17132,.F.);
#24667=ORIENTED_EDGE('',*,*,#17131,.F.);
#24668=ORIENTED_EDGE('',*,*,#17125,.F.);
#24669=ORIENTED_EDGE('',*,*,#17133,.F.);
#24670=ORIENTED_EDGE('',*,*,#17134,.T.);
#24671=ORIENTED_EDGE('',*,*,#17135,.F.);
#24672=ORIENTED_EDGE('',*,*,#17136,.F.);
#24673=ORIENTED_EDGE('',*,*,#17137,.F.);
#24674=ORIENTED_EDGE('',*,*,#17136,.T.);
#24675=ORIENTED_EDGE('',*,*,#17138,.T.);
#24676=ORIENTED_EDGE('',*,*,#17139,.F.);
#24677=ORIENTED_EDGE('',*,*,#17138,.F.);
#24678=ORIENTED_EDGE('',*,*,#17135,.T.);
#24679=ORIENTED_EDGE('',*,*,#17140,.T.);
#24680=ORIENTED_EDGE('',*,*,#17141,.F.);
#24681=ORIENTED_EDGE('',*,*,#17140,.F.);
#24682=ORIENTED_EDGE('',*,*,#17134,.F.);
#24683=ORIENTED_EDGE('',*,*,#17142,.F.);
#24684=ORIENTED_EDGE('',*,*,#16782,.F.);
#24685=ORIENTED_EDGE('',*,*,#16658,.F.);
#24686=ORIENTED_EDGE('',*,*,#16783,.F.);
#24687=ORIENTED_EDGE('',*,*,#17143,.T.);
#24688=ORIENTED_EDGE('',*,*,#17142,.T.);
#24689=ORIENTED_EDGE('',*,*,#17143,.F.);
#24690=ORIENTED_EDGE('',*,*,#17144,.F.);
#24691=ORIENTED_EDGE('',*,*,#17145,.T.);
#24692=ORIENTED_EDGE('',*,*,#16790,.T.);
#24693=ORIENTED_EDGE('',*,*,#17145,.F.);
#24694=ORIENTED_EDGE('',*,*,#16816,.T.);
#24695=ORIENTED_EDGE('',*,*,#17146,.F.);
#24696=ORIENTED_EDGE('',*,*,#17130,.T.);
#24697=ORIENTED_EDGE('',*,*,#17132,.T.);
#24698=ORIENTED_EDGE('',*,*,#17124,.T.);
#24699=ORIENTED_EDGE('',*,*,#17147,.F.);
#24700=ORIENTED_EDGE('',*,*,#16831,.T.);
#24701=ORIENTED_EDGE('',*,*,#16833,.T.);
#24702=ORIENTED_EDGE('',*,*,#16825,.T.);
#24703=ORIENTED_EDGE('',*,*,#17148,.F.);
#24704=ORIENTED_EDGE('',*,*,#17121,.T.);
#24705=ORIENTED_EDGE('',*,*,#17123,.T.);
#24706=ORIENTED_EDGE('',*,*,#17115,.T.);
#24707=ORIENTED_EDGE('',*,*,#17149,.F.);
#24708=ORIENTED_EDGE('',*,*,#16840,.T.);
#24709=ORIENTED_EDGE('',*,*,#16842,.T.);
#24710=ORIENTED_EDGE('',*,*,#16834,.T.);
#24711=ORIENTED_EDGE('',*,*,#17150,.F.);
#24712=ORIENTED_EDGE('',*,*,#17112,.T.);
#24713=ORIENTED_EDGE('',*,*,#17114,.T.);
#24714=ORIENTED_EDGE('',*,*,#17106,.T.);
#24715=ORIENTED_EDGE('',*,*,#17151,.F.);
#24716=ORIENTED_EDGE('',*,*,#16849,.T.);
#24717=ORIENTED_EDGE('',*,*,#16851,.T.);
#24718=ORIENTED_EDGE('',*,*,#16843,.T.);
#24719=ORIENTED_EDGE('',*,*,#17152,.F.);
#24720=ORIENTED_EDGE('',*,*,#17103,.T.);
#24721=ORIENTED_EDGE('',*,*,#17105,.T.);
#24722=ORIENTED_EDGE('',*,*,#17097,.T.);
#24723=ORIENTED_EDGE('',*,*,#17153,.F.);
#24724=ORIENTED_EDGE('',*,*,#16858,.T.);
#24725=ORIENTED_EDGE('',*,*,#16860,.T.);
#24726=ORIENTED_EDGE('',*,*,#16852,.T.);
#24727=ORIENTED_EDGE('',*,*,#17154,.F.);
#24728=ORIENTED_EDGE('',*,*,#17094,.T.);
#24729=ORIENTED_EDGE('',*,*,#17096,.T.);
#24730=ORIENTED_EDGE('',*,*,#17088,.T.);
#24731=ORIENTED_EDGE('',*,*,#17155,.F.);
#24732=ORIENTED_EDGE('',*,*,#16867,.T.);
#24733=ORIENTED_EDGE('',*,*,#16869,.T.);
#24734=ORIENTED_EDGE('',*,*,#16861,.T.);
#24735=ORIENTED_EDGE('',*,*,#17156,.F.);
#24736=ORIENTED_EDGE('',*,*,#17085,.T.);
#24737=ORIENTED_EDGE('',*,*,#17087,.T.);
#24738=ORIENTED_EDGE('',*,*,#17079,.T.);
#24739=ORIENTED_EDGE('',*,*,#17157,.F.);
#24740=ORIENTED_EDGE('',*,*,#16876,.T.);
#24741=ORIENTED_EDGE('',*,*,#16878,.T.);
#24742=ORIENTED_EDGE('',*,*,#16870,.T.);
#24743=ORIENTED_EDGE('',*,*,#17158,.F.);
#24744=ORIENTED_EDGE('',*,*,#17076,.T.);
#24745=ORIENTED_EDGE('',*,*,#17078,.T.);
#24746=ORIENTED_EDGE('',*,*,#17070,.T.);
#24747=ORIENTED_EDGE('',*,*,#17159,.F.);
#24748=ORIENTED_EDGE('',*,*,#16885,.T.);
#24749=ORIENTED_EDGE('',*,*,#16887,.T.);
#24750=ORIENTED_EDGE('',*,*,#16879,.T.);
#24751=ORIENTED_EDGE('',*,*,#17160,.F.);
#24752=ORIENTED_EDGE('',*,*,#17067,.T.);
#24753=ORIENTED_EDGE('',*,*,#17069,.T.);
#24754=ORIENTED_EDGE('',*,*,#17061,.T.);
#24755=ORIENTED_EDGE('',*,*,#17161,.F.);
#24756=ORIENTED_EDGE('',*,*,#16895,.T.);
#24757=ORIENTED_EDGE('',*,*,#16897,.T.);
#24758=ORIENTED_EDGE('',*,*,#17162,.T.);
#24759=ORIENTED_EDGE('',*,*,#17144,.T.);
#24760=ORIENTED_EDGE('',*,*,#17162,.F.);
#24761=ORIENTED_EDGE('',*,*,#16898,.T.);
#24762=ORIENTED_EDGE('',*,*,#16888,.T.);
#24763=ORIENTED_EDGE('',*,*,#17163,.F.);
#24764=ORIENTED_EDGE('',*,*,#16905,.T.);
#24765=ORIENTED_EDGE('',*,*,#16907,.T.);
#24766=ORIENTED_EDGE('',*,*,#16899,.T.);
#24767=ORIENTED_EDGE('',*,*,#17164,.F.);
#24768=ORIENTED_EDGE('',*,*,#17049,.T.);
#24769=ORIENTED_EDGE('',*,*,#17051,.T.);
#24770=ORIENTED_EDGE('',*,*,#17043,.T.);
#24771=ORIENTED_EDGE('',*,*,#17165,.F.);
#24772=ORIENTED_EDGE('',*,*,#16914,.T.);
#24773=ORIENTED_EDGE('',*,*,#16916,.T.);
#24774=ORIENTED_EDGE('',*,*,#16908,.T.);
#24775=ORIENTED_EDGE('',*,*,#17166,.F.);
#24776=ORIENTED_EDGE('',*,*,#17040,.T.);
#24777=ORIENTED_EDGE('',*,*,#17042,.T.);
#24778=ORIENTED_EDGE('',*,*,#17034,.T.);
#24779=ORIENTED_EDGE('',*,*,#17167,.F.);
#24780=ORIENTED_EDGE('',*,*,#16923,.T.);
#24781=ORIENTED_EDGE('',*,*,#16925,.T.);
#24782=ORIENTED_EDGE('',*,*,#16917,.T.);
#24783=ORIENTED_EDGE('',*,*,#17168,.F.);
#24784=ORIENTED_EDGE('',*,*,#17031,.T.);
#24785=ORIENTED_EDGE('',*,*,#17033,.T.);
#24786=ORIENTED_EDGE('',*,*,#17025,.T.);
#24787=ORIENTED_EDGE('',*,*,#17169,.F.);
#24788=ORIENTED_EDGE('',*,*,#16932,.T.);
#24789=ORIENTED_EDGE('',*,*,#16934,.T.);
#24790=ORIENTED_EDGE('',*,*,#16926,.T.);
#24791=ORIENTED_EDGE('',*,*,#17170,.F.);
#24792=ORIENTED_EDGE('',*,*,#17022,.T.);
#24793=ORIENTED_EDGE('',*,*,#17024,.T.);
#24794=ORIENTED_EDGE('',*,*,#17016,.T.);
#24795=ORIENTED_EDGE('',*,*,#17171,.F.);
#24796=ORIENTED_EDGE('',*,*,#16941,.T.);
#24797=ORIENTED_EDGE('',*,*,#16943,.T.);
#24798=ORIENTED_EDGE('',*,*,#16935,.T.);
#24799=ORIENTED_EDGE('',*,*,#17172,.F.);
#24800=ORIENTED_EDGE('',*,*,#17013,.T.);
#24801=ORIENTED_EDGE('',*,*,#17015,.T.);
#24802=ORIENTED_EDGE('',*,*,#17007,.T.);
#24803=ORIENTED_EDGE('',*,*,#17173,.F.);
#24804=ORIENTED_EDGE('',*,*,#16950,.T.);
#24805=ORIENTED_EDGE('',*,*,#16952,.T.);
#24806=ORIENTED_EDGE('',*,*,#16944,.T.);
#24807=ORIENTED_EDGE('',*,*,#17174,.F.);
#24808=ORIENTED_EDGE('',*,*,#17004,.T.);
#24809=ORIENTED_EDGE('',*,*,#17006,.T.);
#24810=ORIENTED_EDGE('',*,*,#16998,.T.);
#24811=ORIENTED_EDGE('',*,*,#17175,.F.);
#24812=ORIENTED_EDGE('',*,*,#16959,.T.);
#24813=ORIENTED_EDGE('',*,*,#16961,.T.);
#24814=ORIENTED_EDGE('',*,*,#16953,.T.);
#24815=ORIENTED_EDGE('',*,*,#17176,.F.);
#24816=ORIENTED_EDGE('',*,*,#16995,.T.);
#24817=ORIENTED_EDGE('',*,*,#16997,.T.);
#24818=ORIENTED_EDGE('',*,*,#16989,.T.);
#24819=ORIENTED_EDGE('',*,*,#17177,.F.);
#24820=ORIENTED_EDGE('',*,*,#16968,.T.);
#24821=ORIENTED_EDGE('',*,*,#16970,.T.);
#24822=ORIENTED_EDGE('',*,*,#16962,.T.);
#24823=ORIENTED_EDGE('',*,*,#17178,.F.);
#24824=ORIENTED_EDGE('',*,*,#16986,.T.);
#24825=ORIENTED_EDGE('',*,*,#16988,.T.);
#24826=ORIENTED_EDGE('',*,*,#16980,.T.);
#24827=ORIENTED_EDGE('',*,*,#17179,.F.);
#24828=ORIENTED_EDGE('',*,*,#16977,.T.);
#24829=ORIENTED_EDGE('',*,*,#16979,.T.);
#24830=ORIENTED_EDGE('',*,*,#16971,.T.);
#24831=ORIENTED_EDGE('',*,*,#17180,.F.);
#24832=ORIENTED_EDGE('',*,*,#17058,.T.);
#24833=ORIENTED_EDGE('',*,*,#17060,.T.);
#24834=ORIENTED_EDGE('',*,*,#17055,.T.);
#24835=ORIENTED_EDGE('',*,*,#17181,.F.);
#24836=ORIENTED_EDGE('',*,*,#17139,.T.);
#24837=ORIENTED_EDGE('',*,*,#17141,.T.);
#24838=ORIENTED_EDGE('',*,*,#17133,.T.);
#24839=ORIENTED_EDGE('',*,*,#17182,.F.);
#24840=ORIENTED_EDGE('',*,*,#16822,.T.);
#24841=ORIENTED_EDGE('',*,*,#16824,.T.);
#24842=ORIENTED_EDGE('',*,*,#17183,.F.);
#24843=ORIENTED_EDGE('',*,*,#17184,.T.);
#24844=ORIENTED_EDGE('',*,*,#16894,.T.);
#24845=ORIENTED_EDGE('',*,*,#17161,.T.);
#24846=ORIENTED_EDGE('',*,*,#17065,.T.);
#24847=ORIENTED_EDGE('',*,*,#17160,.T.);
#24848=ORIENTED_EDGE('',*,*,#16883,.T.);
#24849=ORIENTED_EDGE('',*,*,#17159,.T.);
#24850=ORIENTED_EDGE('',*,*,#17074,.T.);
#24851=ORIENTED_EDGE('',*,*,#17158,.T.);
#24852=ORIENTED_EDGE('',*,*,#16874,.T.);
#24853=ORIENTED_EDGE('',*,*,#17157,.T.);
#24854=ORIENTED_EDGE('',*,*,#17083,.T.);
#24855=ORIENTED_EDGE('',*,*,#17156,.T.);
#24856=ORIENTED_EDGE('',*,*,#16865,.T.);
#24857=ORIENTED_EDGE('',*,*,#17155,.T.);
#24858=ORIENTED_EDGE('',*,*,#17092,.T.);
#24859=ORIENTED_EDGE('',*,*,#17154,.T.);
#24860=ORIENTED_EDGE('',*,*,#16856,.T.);
#24861=ORIENTED_EDGE('',*,*,#17153,.T.);
#24862=ORIENTED_EDGE('',*,*,#17101,.T.);
#24863=ORIENTED_EDGE('',*,*,#17152,.T.);
#24864=ORIENTED_EDGE('',*,*,#16847,.T.);
#24865=ORIENTED_EDGE('',*,*,#17151,.T.);
#24866=ORIENTED_EDGE('',*,*,#17110,.T.);
#24867=ORIENTED_EDGE('',*,*,#17150,.T.);
#24868=ORIENTED_EDGE('',*,*,#16838,.T.);
#24869=ORIENTED_EDGE('',*,*,#17149,.T.);
#24870=ORIENTED_EDGE('',*,*,#17119,.T.);
#24871=ORIENTED_EDGE('',*,*,#17148,.T.);
#24872=ORIENTED_EDGE('',*,*,#16829,.T.);
#24873=ORIENTED_EDGE('',*,*,#17147,.T.);
#24874=ORIENTED_EDGE('',*,*,#17128,.T.);
#24875=ORIENTED_EDGE('',*,*,#17146,.T.);
#24876=ORIENTED_EDGE('',*,*,#16820,.T.);
#24877=ORIENTED_EDGE('',*,*,#17182,.T.);
#24878=ORIENTED_EDGE('',*,*,#17137,.T.);
#24879=ORIENTED_EDGE('',*,*,#17181,.T.);
#24880=ORIENTED_EDGE('',*,*,#17052,.T.);
#24881=ORIENTED_EDGE('',*,*,#17180,.T.);
#24882=ORIENTED_EDGE('',*,*,#16975,.T.);
#24883=ORIENTED_EDGE('',*,*,#17179,.T.);
#24884=ORIENTED_EDGE('',*,*,#16984,.T.);
#24885=ORIENTED_EDGE('',*,*,#17178,.T.);
#24886=ORIENTED_EDGE('',*,*,#16966,.T.);
#24887=ORIENTED_EDGE('',*,*,#17177,.T.);
#24888=ORIENTED_EDGE('',*,*,#16993,.T.);
#24889=ORIENTED_EDGE('',*,*,#17176,.T.);
#24890=ORIENTED_EDGE('',*,*,#16957,.T.);
#24891=ORIENTED_EDGE('',*,*,#17175,.T.);
#24892=ORIENTED_EDGE('',*,*,#17002,.T.);
#24893=ORIENTED_EDGE('',*,*,#17174,.T.);
#24894=ORIENTED_EDGE('',*,*,#16948,.T.);
#24895=ORIENTED_EDGE('',*,*,#17173,.T.);
#24896=ORIENTED_EDGE('',*,*,#17011,.T.);
#24897=ORIENTED_EDGE('',*,*,#17172,.T.);
#24898=ORIENTED_EDGE('',*,*,#16939,.T.);
#24899=ORIENTED_EDGE('',*,*,#17171,.T.);
#24900=ORIENTED_EDGE('',*,*,#17020,.T.);
#24901=ORIENTED_EDGE('',*,*,#17170,.T.);
#24902=ORIENTED_EDGE('',*,*,#16930,.T.);
#24903=ORIENTED_EDGE('',*,*,#17169,.T.);
#24904=ORIENTED_EDGE('',*,*,#17029,.T.);
#24905=ORIENTED_EDGE('',*,*,#17168,.T.);
#24906=ORIENTED_EDGE('',*,*,#16921,.T.);
#24907=ORIENTED_EDGE('',*,*,#17167,.T.);
#24908=ORIENTED_EDGE('',*,*,#17038,.T.);
#24909=ORIENTED_EDGE('',*,*,#17166,.T.);
#24910=ORIENTED_EDGE('',*,*,#16912,.T.);
#24911=ORIENTED_EDGE('',*,*,#17165,.T.);
#24912=ORIENTED_EDGE('',*,*,#17047,.T.);
#24913=ORIENTED_EDGE('',*,*,#17164,.T.);
#24914=ORIENTED_EDGE('',*,*,#16903,.T.);
#24915=ORIENTED_EDGE('',*,*,#17163,.T.);
#24916=ORIENTED_EDGE('',*,*,#16892,.T.);
#24917=ORIENTED_EDGE('',*,*,#17184,.F.);
#24918=ORIENTED_EDGE('',*,*,#17183,.T.);
#24919=ORIENTED_EDGE('',*,*,#16804,.T.);
#24920=ORIENTED_EDGE('',*,*,#16815,.T.);
#24921=ORIENTED_EDGE('',*,*,#16813,.T.);
#24922=ORIENTED_EDGE('',*,*,#16811,.T.);
#24923=ORIENTED_EDGE('',*,*,#16809,.T.);
#24924=ORIENTED_EDGE('',*,*,#16807,.T.);
#24925=CONICAL_SURFACE('',#26907,1.15732233047034,1.17809724509618);
#24926=CONICAL_SURFACE('',#26911,1.15732233047033,1.17809724509616);
#24927=CONICAL_SURFACE('',#26915,1.15732233047033,1.17809724509616);
#24928=CONICAL_SURFACE('',#26919,1.15732233047034,1.17809724509617);
#24929=CONICAL_SURFACE('',#26924,1.075,0.785398163397438);
#24930=CONICAL_SURFACE('',#26927,1.07500000000001,0.785398163397438);
#24931=CONICAL_SURFACE('',#26934,0.530000000000003,0.785398163397457);
#24932=CONICAL_SURFACE('',#26948,0.530000000000003,0.785398163397457);
#24933=CONICAL_SURFACE('',#26952,0.529999999999999,0.785398163397457);
#24934=CONICAL_SURFACE('',#26956,0.529999999999999,0.785398163397457);
#24935=CONICAL_SURFACE('',#26968,1.01767766952966,0.392699081698724);
#24936=CONICAL_SURFACE('',#26972,1.01767766952966,0.392699081698724);
#24937=CONICAL_SURFACE('',#26977,1.01767766952967,0.392699081698667);
#24938=CONICAL_SURFACE('',#26980,1.01767766952966,0.392699081698703);
#24939=CONICAL_SURFACE('',#27007,1.84267766952967,1.17809724509616);
#24940=CONICAL_SURFACE('',#27010,1.84267766952967,1.17809724509616);
#24941=CONICAL_SURFACE('',#27013,1.84267766952966,1.17809724509616);
#24942=CONICAL_SURFACE('',#27016,1.84267766952966,1.17809724509618);
#24943=CONICAL_SURFACE('',#27020,1.925,0.785398163397446);
#24944=CONICAL_SURFACE('',#27023,1.925,0.785398163397438);
#24945=CONICAL_SURFACE('',#27026,1.98232233047034,0.392699081698708);
#24946=CONICAL_SURFACE('',#27031,1.98232233047034,0.392699081698714);
#24947=CONICAL_SURFACE('',#27035,1.98232233047034,0.392699081698739);
#24948=CONICAL_SURFACE('',#27038,1.98232233047034,0.392699081698699);
#24949=CONICAL_SURFACE('',#27049,1.98232233047034,0.392699081698715);
#24950=CONICAL_SURFACE('',#27053,1.98232233047033,0.392699081698728);
#24951=CONICAL_SURFACE('',#27056,1.95,0.78539816339746);
#24952=CONICAL_SURFACE('',#27059,1.95,0.785398163397448);
#24953=CONICAL_SURFACE('',#27064,1.89267766952966,1.17809724509616);
#24954=CONICAL_SURFACE('',#27068,1.89267766952966,1.17809724509617);
#24955=CONICAL_SURFACE('',#27078,1.98232233047033,0.392699081698725);
#24956=CONICAL_SURFACE('',#27081,1.98232233047034,0.392699081698759);
#24957=CONICAL_SURFACE('',#27089,1.95,0.78539816339746);
#24958=CONICAL_SURFACE('',#27092,1.95,0.785398163397448);
#24959=CONICAL_SURFACE('',#27122,1.075,0.785398163397446);
#24960=CONICAL_SURFACE('',#27124,1.075,0.785398163397446);
#24961=CONICAL_SURFACE('',#27126,1.925,0.785398163397446);
#24962=CONICAL_SURFACE('',#27128,1.925,0.785398163397438);
#24963=CONICAL_SURFACE('',#27133,0.252500000000001,1.02974425867666);
#24964=CONICAL_SURFACE('',#27134,0.252500000000001,1.02974425867666);
#24965=CONICAL_SURFACE('',#27135,0.2525,1.02974425867665);
#24966=CONICAL_SURFACE('',#27136,0.2525,1.02974425867665);
#24967=CONICAL_SURFACE('',#27142,1.69267766952967,1.17809724509617);
#24968=CONICAL_SURFACE('',#27146,1.75,0.785398163397413);
#24969=CONICAL_SURFACE('',#27151,1.78232233047033,0.39269908169871);
#24970=CONICAL_SURFACE('',#27155,0.330000000000001,0.785398163397462);
#24971=CONICAL_SURFACE('',#27160,5.4,0.785398163397451);
#24972=CONICAL_SURFACE('',#27170,0.329999999999999,0.785398163397428);
#24973=CONICAL_SURFACE('',#27186,5.29267766952966,1.17809724509617);
#24974=CONICAL_SURFACE('',#27189,5.4,0.785398163397442);
#24975=CONICAL_SURFACE('',#27199,5.48232233047034,0.392699081698728);
#24976=CONICAL_SURFACE('',#27202,19.3603883884215,0.785398163397445);
#24977=CONICAL_SURFACE('',#27211,0.975,0.785398163397449);
#24978=CONICAL_SURFACE('',#27215,0.975,0.785398163397449);
#24979=CONICAL_SURFACE('',#27223,0.975,0.785398163397454);
#24980=CONICAL_SURFACE('',#27225,0.975000000000002,0.785398163397454);
#24981=CONICAL_SURFACE('',#27243,0.575000000000001,0.785398163397457);
#24982=CONICAL_SURFACE('',#27246,0.575000000000001,0.785398163397457);
#24983=CONICAL_SURFACE('',#27252,0.575000000000001,0.785398163397457);
#24984=CONICAL_SURFACE('',#27255,0.575000000000001,0.785398163397457);
#24985=CONICAL_SURFACE('',#27261,0.575000000000001,0.785398163397457);
#24986=CONICAL_SURFACE('',#27264,0.575000000000001,0.785398163397457);
#24987=CONICAL_SURFACE('',#27270,0.575000000000001,0.785398163397457);
#24988=CONICAL_SURFACE('',#27273,0.575000000000001,0.785398163397457);
#24989=CONICAL_SURFACE('',#27278,0.330000000000001,0.785398163397462);
#24990=CONICAL_SURFACE('',#27285,0.33,0.785398163397456);
#24991=CONICAL_SURFACE('',#27292,0.575000000000001,0.785398163397457);
#24992=CONICAL_SURFACE('',#27296,0.575000000000001,0.785398163397457);
#24993=CONICAL_SURFACE('',#27311,0.575000000000001,0.785398163397457);
#24994=CONICAL_SURFACE('',#27314,0.575000000000001,0.785398163397457);
#24995=CONICAL_SURFACE('',#27317,0.575000000000001,0.785398163397457);
#24996=CONICAL_SURFACE('',#27320,0.575000000000001,0.785398163397457);
#24997=CONICAL_SURFACE('',#27323,0.575000000000001,0.785398163397457);
#24998=CONICAL_SURFACE('',#27326,0.575000000000001,0.785398163397457);
#24999=CONICAL_SURFACE('',#27328,0.975,0.785398163397454);
#25000=CONICAL_SURFACE('',#27331,0.975,0.785398163397449);
#25001=CONICAL_SURFACE('',#27334,0.975,0.785398163397449);
#25002=CONICAL_SURFACE('',#27337,0.975000000000002,0.785398163397454);
#25003=CONICAL_SURFACE('',#27345,19.3603883884215,0.785398163397445);
#25004=CONICAL_SURFACE('',#27380,0.1525,1.02974425867665);
#25005=CONICAL_SURFACE('',#27381,0.1525,1.02974425867665);
#25006=CONICAL_SURFACE('',#27382,0.1525,1.02974425867665);
#25007=CONICAL_SURFACE('',#27383,0.1525,1.02974425867665);
#25008=CONICAL_SURFACE('',#27396,3.08422464300993,0.974356912318788);
#25009=CONICAL_SURFACE('',#27400,3.2985,0.377917497842688);
#25010=CONICAL_SURFACE('',#27563,3.447,0.785398163397451);
#25011=CONICAL_SURFACE('',#27566,1.6023112,0.798216012485968);
#25012=CONICAL_SURFACE('',#27568,1.4090882,0.0259641639514023);
#25013=CONICAL_SURFACE('',#27576,1.63201114386566,0.248658708390703);
#25014=CONICAL_SURFACE('',#27581,1.60375905110103,0.0262813588168537);
#25015=CONICAL_SURFACE('',#27583,1.64516810220205,0.523598775598299);
#25016=CONICAL_SURFACE('',#27586,1.2192801,0.785398163397437);
#25017=CONICAL_SURFACE('',#27588,1.41081505,0.0259641639514023);
#25018=CONICAL_SURFACE('',#27676,0.892677669529664,1.17809724509616);
#25019=CONICAL_SURFACE('',#27680,0.95,0.785398163397441);
#25020=CONICAL_SURFACE('',#27685,0.430000000000001,0.785398163397455);
#25021=CONICAL_SURFACE('',#27692,0.974822330470337,0.392699081698707);
#25022=CONICAL_SURFACE('',#27694,0.949822330470333,0.392699081698761);
#25023=CONICAL_SURFACE('',#27700,0.202500000000001,1.02974425867666);
#25024=CONICAL_SURFACE('',#27708,0.975,0.785398163397451);
#25025=CONICAL_SURFACE('',#27714,1.575,0.785398163397459);
#25026=CONICAL_SURFACE('',#27718,1.575,0.785398163397459);
#25027=CONICAL_SURFACE('',#27722,1.11232233047034,1.17809724509617);
#25028=CONICAL_SURFACE('',#27726,1.055,0.78539816339745);
#25029=CONICAL_SURFACE('',#27731,1.02267766952966,0.39269908169873);
#25030=CONICAL_SURFACE('',#27745,1.975,0.785398163397442);
#25031=CONICAL_SURFACE('',#27748,1.975,0.785398163397442);
#25032=CONICAL_SURFACE('',#27752,1.055,0.78539816339745);
#25033=CONICAL_SURFACE('',#27754,1.825,0.785398163397442);
#25034=CONICAL_SURFACE('',#27762,6.14267766952966,1.17809724509617);
#25035=CONICAL_SURFACE('',#27766,6.2,0.785398163397448);
#25036=CONICAL_SURFACE('',#27775,6.23232233047034,0.392699081698724);
#25037=CONICAL_SURFACE('',#27781,6.23232233047034,0.392699081698724);
#25038=CONICAL_SURFACE('',#27784,6.2,0.785398163397444);
#25039=CONICAL_SURFACE('',#27787,6.14267766952966,1.17809724509617);
#25040=CONICAL_SURFACE('',#27795,2.78232233047034,0.39269908169872);
#25041=CONICAL_SURFACE('',#27800,2.75,0.785398163397444);
#25042=CONICAL_SURFACE('',#27804,2.69267766952966,1.17809724509617);
#25043=CONICAL_SURFACE('',#27808,1.825,0.785398163397451);
#25044=CONICAL_SURFACE('',#27819,3.47,0.785398163397439);
#25045=CONICAL_SURFACE('',#27826,2.48232233047034,0.392699081698724);
#25046=CONICAL_SURFACE('',#27834,2.45,0.785398163397451);
#25047=CONICAL_SURFACE('',#27837,2.48232233047034,0.392699081698723);
#25048=CONICAL_SURFACE('',#27840,2.45,0.785398163397449);
#25049=CONICAL_SURFACE('',#27843,2.39267766952966,1.17809724509617);
#25050=CONICAL_SURFACE('',#27847,2.39267766952966,1.17809724509617);
#25051=CONICAL_SURFACE('',#27861,0.775,0.0320403135474668);
#25052=CONICAL_SURFACE('',#27862,0.775,0.0320403135474668);
#25053=CONICAL_SURFACE('',#27863,0.775000000000002,0.0320403135474665);
#25054=CONICAL_SURFACE('',#27864,0.774999999999997,0.032040313547468);
#25055=CONICAL_SURFACE('',#27936,0.173205080756888,1.03037682652431);
#25056=CONICAL_SURFACE('',#28163,0.375,0.785398163397448);
#25057=CONICAL_SURFACE('',#28164,0.635,0.785398163397449);
#25058=CONICAL_SURFACE('',#28203,0.625,0.785398163397448);
#25059=CONICAL_SURFACE('',#28208,0.24,0.785398163397459);
#25060=CONICAL_SURFACE('',#28212,0.24,0.785398163397459);
#25061=CONICAL_SURFACE('',#28220,0.2375,0.785398163397475);
#25062=CONICAL_SURFACE('',#28224,0.2375,0.785398163397475);
#25063=CONICAL_SURFACE('',#28251,1.34,1.10714871779407);
#25064=CONICAL_SURFACE('',#28254,1.425,0.643501108793273);
#25065=CONICAL_SURFACE('',#28262,0.699999999999993,0.0225236710696234);
#25066=CONICAL_SURFACE('',#28276,0.575000000000003,0.785398163397484);
#25067=CONICAL_SURFACE('',#28286,0.975000000000001,0.785398163397413);
#25068=CONICAL_SURFACE('',#28337,0.37,0.785398163397449);
#25069=CONICAL_SURFACE('',#28341,0.26,0.785398163397448);
#25070=CONICAL_SURFACE('',#28412,1.28782032302755,1.0471975511966);
#25071=CONICAL_SURFACE('',#28425,0.77,0.785398163397448);
#25072=CONICAL_SURFACE('',#28432,0.912322330470337,1.1780972450962);
#25073=CONICAL_SURFACE('',#28435,0.855,0.785398163397455);
#25074=CONICAL_SURFACE('',#28442,0.822677669529664,0.392699081698729);
#25075=CONICAL_SURFACE('',#28446,0.822677669529664,0.392699081698729);
#25076=CONICAL_SURFACE('',#28448,0.855,0.785398163397456);
#25077=CONICAL_SURFACE('',#28450,0.912322330470337,1.1780972450962);
#25078=CONICAL_SURFACE('',#28457,0.782322330470333,0.392699081698756);
#25079=CONICAL_SURFACE('',#28461,0.782322330470341,0.392699081698706);
#25080=CONICAL_SURFACE('',#28465,0.782322330470341,0.392699081698703);
#25081=CONICAL_SURFACE('',#28469,0.782322330470335,0.39269908169872);
#25082=CONICAL_SURFACE('',#28480,0.749999999999996,0.785398163397465);
#25083=CONICAL_SURFACE('',#28482,0.749999999999995,0.785398163397465);
#25084=CONICAL_SURFACE('',#28484,0.692677669529668,1.17809724509619);
#25085=CONICAL_SURFACE('',#28487,0.692677669529657,1.1780972450962);
#25086=CONICAL_SURFACE('',#28490,0.692677669529655,1.17809724509618);
#25087=CONICAL_SURFACE('',#28493,0.692677669529664,1.1780972450962);
#25088=CONICAL_SURFACE('',#28495,0.749999999999995,0.785398163397466);
#25089=CONICAL_SURFACE('',#28498,0.750000000000004,0.785398163397447);
#25090=CONICAL_SURFACE('',#28502,0.782322330470341,0.392699081698714);
#25091=CONICAL_SURFACE('',#28504,0.782322330470333,0.392699081698756);
#25092=CONICAL_SURFACE('',#28506,0.782322330470335,0.39269908169872);
#25093=CONICAL_SURFACE('',#28510,0.782322330470341,0.392699081698703);
#25094=CONICAL_SURFACE('',#28513,0.749999999999996,0.785398163397466);
#25095=CONICAL_SURFACE('',#28515,0.750000000000004,0.785398163397447);
#25096=CONICAL_SURFACE('',#28518,0.750000000000004,0.785398163397447);
#25097=CONICAL_SURFACE('',#28520,0.750000000000004,0.785398163397447);
#25098=CONICAL_SURFACE('',#28526,1.53,0.785398163397458);
#25099=CONICAL_SURFACE('',#28529,1.53,0.785398163397447);
#25100=CONICAL_SURFACE('',#28538,1.725,0.785398163397451);
#25101=CONICAL_SURFACE('',#28549,1.695,0.785398163397442);
#25102=CONICAL_SURFACE('',#28613,0.972115242270663,1.0471975511966);
#25103=CONICAL_SURFACE('',#28626,0.57,0.785398163397447);
#25104=CONICAL_SURFACE('',#28708,0.23094010767585,1.03037682652431);
#25105=CONICAL_SURFACE('',#28935,0.475,0.78539816339745);
#25106=CONICAL_SURFACE('',#28936,0.785,0.785398163397449);
#25107=CONICAL_SURFACE('',#28975,0.775,0.785398163397448);
#25108=CONICAL_SURFACE('',#29047,0.144337567297406,1.03037682652431);
#25109=CONICAL_SURFACE('',#29274,0.275,0.785398163397448);
#25110=CONICAL_SURFACE('',#29275,0.485,0.785398163397448);
#25111=CONICAL_SURFACE('',#29314,0.475,0.785398163397449);
#25112=ADVANCED_FACE('',(#2524),#24925,.F.);
#25113=ADVANCED_FACE('',(#2525),#1656,.T.);
#25114=ADVANCED_FACE('',(#2526),#24926,.F.);
#25115=ADVANCED_FACE('',(#2527),#1657,.T.);
#25116=ADVANCED_FACE('',(#2528),#24927,.F.);
#25117=ADVANCED_FACE('',(#2529),#1658,.T.);
#25118=ADVANCED_FACE('',(#2530),#24928,.F.);
#25119=ADVANCED_FACE('',(#2531),#1659,.T.);
#25120=ADVANCED_FACE('',(#2532),#1660,.T.);
#25121=ADVANCED_FACE('',(#2533),#24929,.F.);
#25122=ADVANCED_FACE('',(#2534),#1661,.T.);
#25123=ADVANCED_FACE('',(#2535),#24930,.F.);
#25124=ADVANCED_FACE('',(#2536,#1553),#1662,.T.);
#25125=ADVANCED_FACE('',(#2537),#24931,.F.);
#25126=ADVANCED_FACE('',(#2538,#1554,#1555,#1556,#1557,#1558,#1559),#1663,
 .T.);
#25127=ADVANCED_FACE('',(#2539),#1103,.F.);
#25128=ADVANCED_FACE('',(#2540),#24932,.F.);
#25129=ADVANCED_FACE('',(#2541),#1104,.F.);
#25130=ADVANCED_FACE('',(#2542),#24933,.F.);
#25131=ADVANCED_FACE('',(#2543),#1105,.F.);
#25132=ADVANCED_FACE('',(#2544),#24934,.F.);
#25133=ADVANCED_FACE('',(#2545),#1106,.F.);
#25134=ADVANCED_FACE('',(#2546),#1664,.T.);
#25135=ADVANCED_FACE('',(#2547),#1665,.T.);
#25136=ADVANCED_FACE('',(#2548),#1666,.T.);
#25137=ADVANCED_FACE('',(#2549),#1667,.T.);
#25138=ADVANCED_FACE('',(#2550),#1668,.F.);
#25139=ADVANCED_FACE('',(#2551),#1669,.F.);
#25140=ADVANCED_FACE('',(#2552),#1670,.T.);
#25141=ADVANCED_FACE('',(#2553),#24935,.F.);
#25142=ADVANCED_FACE('',(#2554),#1671,.T.);
#25143=ADVANCED_FACE('',(#2555),#24936,.F.);
#25144=ADVANCED_FACE('',(#2556),#1672,.T.);
#25145=ADVANCED_FACE('',(#2557),#24937,.F.);
#25146=ADVANCED_FACE('',(#2558),#1673,.T.);
#25147=ADVANCED_FACE('',(#2559),#24938,.F.);
#25148=ADVANCED_FACE('',(#2560),#1674,.F.);
#25149=ADVANCED_FACE('',(#2561),#1107,.F.);
#25150=ADVANCED_FACE('',(#2562),#1675,.F.);
#25151=ADVANCED_FACE('',(#2563),#1108,.F.);
#25152=ADVANCED_FACE('',(#2564),#1676,.F.);
#25153=ADVANCED_FACE('',(#2565),#1109,.F.);
#25154=ADVANCED_FACE('',(#2566),#1677,.T.);
#25155=ADVANCED_FACE('',(#2567),#1678,.T.);
#25156=ADVANCED_FACE('',(#2568),#1679,.T.);
#25157=ADVANCED_FACE('',(#2569),#1680,.T.);
#25158=ADVANCED_FACE('',(#2570),#1681,.T.);
#25159=ADVANCED_FACE('',(#2571),#1682,.T.);
#25160=ADVANCED_FACE('',(#2572),#1683,.T.);
#25161=ADVANCED_FACE('',(#2573),#1684,.T.);
#25162=ADVANCED_FACE('',(#2574),#1685,.T.);
#25163=ADVANCED_FACE('',(#2575),#1686,.T.);
#25164=ADVANCED_FACE('',(#2576),#24939,.T.);
#25165=ADVANCED_FACE('',(#2577),#1687,.T.);
#25166=ADVANCED_FACE('',(#2578),#24940,.T.);
#25167=ADVANCED_FACE('',(#2579),#1688,.T.);
#25168=ADVANCED_FACE('',(#2580),#24941,.T.);
#25169=ADVANCED_FACE('',(#2581),#1689,.T.);
#25170=ADVANCED_FACE('',(#2582),#24942,.T.);
#25171=ADVANCED_FACE('',(#2583),#1690,.T.);
#25172=ADVANCED_FACE('',(#2584),#1691,.T.);
#25173=ADVANCED_FACE('',(#2585),#24943,.T.);
#25174=ADVANCED_FACE('',(#2586),#1692,.T.);
#25175=ADVANCED_FACE('',(#2587),#24944,.T.);
#25176=ADVANCED_FACE('',(#2588),#1693,.T.);
#25177=ADVANCED_FACE('',(#2589),#24945,.T.);
#25178=ADVANCED_FACE('',(#2590),#1694,.T.);
#25179=ADVANCED_FACE('',(#2591),#24946,.T.);
#25180=ADVANCED_FACE('',(#2592),#1695,.T.);
#25181=ADVANCED_FACE('',(#2593),#24947,.T.);
#25182=ADVANCED_FACE('',(#2594),#1696,.T.);
#25183=ADVANCED_FACE('',(#2595),#24948,.T.);
#25184=ADVANCED_FACE('',(#2596),#1697,.T.);
#25185=ADVANCED_FACE('',(#2597),#1110,.T.);
#25186=ADVANCED_FACE('',(#2598),#1698,.T.);
#25187=ADVANCED_FACE('',(#2599),#1111,.T.);
#25188=ADVANCED_FACE('',(#2600),#1699,.T.);
#25189=ADVANCED_FACE('',(#2601),#24949,.T.);
#25190=ADVANCED_FACE('',(#2602),#1700,.T.);
#25191=ADVANCED_FACE('',(#2603),#24950,.T.);
#25192=ADVANCED_FACE('',(#2604),#1701,.T.);
#25193=ADVANCED_FACE('',(#2605),#24951,.T.);
#25194=ADVANCED_FACE('',(#2606),#1702,.T.);
#25195=ADVANCED_FACE('',(#2607),#24952,.T.);
#25196=ADVANCED_FACE('',(#2608),#1703,.T.);
#25197=ADVANCED_FACE('',(#2609),#1704,.T.);
#25198=ADVANCED_FACE('',(#2610),#1705,.T.);
#25199=ADVANCED_FACE('',(#2611),#24953,.T.);
#25200=ADVANCED_FACE('',(#2612),#1706,.T.);
#25201=ADVANCED_FACE('',(#2613),#24954,.T.);
#25202=ADVANCED_FACE('',(#2614),#1707,.T.);
#25203=ADVANCED_FACE('',(#2615),#1708,.T.);
#25204=ADVANCED_FACE('',(#2616),#1709,.T.);
#25205=ADVANCED_FACE('',(#2617),#1710,.T.);
#25206=ADVANCED_FACE('',(#2618),#1711,.T.);
#25207=ADVANCED_FACE('',(#2619),#1712,.T.);
#25208=ADVANCED_FACE('',(#2620),#1713,.T.);
#25209=ADVANCED_FACE('',(#2621),#24955,.T.);
#25210=ADVANCED_FACE('',(#2622),#1714,.T.);
#25211=ADVANCED_FACE('',(#2623),#24956,.T.);
#25212=ADVANCED_FACE('',(#2624),#1715,.T.);
#25213=ADVANCED_FACE('',(#2625),#1716,.T.);
#25214=ADVANCED_FACE('',(#2626),#1717,.T.);
#25215=ADVANCED_FACE('',(#2627),#1718,.T.);
#25216=ADVANCED_FACE('',(#2628),#1719,.T.);
#25217=ADVANCED_FACE('',(#2629),#24957,.T.);
#25218=ADVANCED_FACE('',(#2630),#1720,.T.);
#25219=ADVANCED_FACE('',(#2631),#1721,.T.);
#25220=ADVANCED_FACE('',(#2632),#24958,.T.);
#25221=ADVANCED_FACE('',(#2633),#1722,.F.);
#25222=ADVANCED_FACE('',(#2634,#1560),#1723,.F.);
#25223=ADVANCED_FACE('',(#2635),#1724,.F.);
#25224=ADVANCED_FACE('',(#2636),#1725,.F.);
#25225=ADVANCED_FACE('',(#2637),#1726,.T.);
#25226=ADVANCED_FACE('',(#2638),#1727,.T.);
#25227=ADVANCED_FACE('',(#2639),#1728,.F.);
#25228=ADVANCED_FACE('',(#2640),#1079,.F.);
#25229=ADVANCED_FACE('',(#2641),#1112,.F.);
#25230=ADVANCED_FACE('',(#2642),#1080,.F.);
#25231=ADVANCED_FACE('',(#2643),#1113,.F.);
#25232=ADVANCED_FACE('',(#2644),#1081,.F.);
#25233=ADVANCED_FACE('',(#2645),#1114,.F.);
#25234=ADVANCED_FACE('',(#2646),#1082,.F.);
#25235=ADVANCED_FACE('',(#2647),#1115,.F.);
#25236=ADVANCED_FACE('',(#2648),#1116,.F.);
#25237=ADVANCED_FACE('',(#2649),#1729,.F.);
#25238=ADVANCED_FACE('',(#2650),#1117,.F.);
#25239=ADVANCED_FACE('',(#2651),#24959,.F.);
#25240=ADVANCED_FACE('',(#2652),#1730,.T.);
#25241=ADVANCED_FACE('',(#2653),#24960,.F.);
#25242=ADVANCED_FACE('',(#2654),#1731,.T.);
#25243=ADVANCED_FACE('',(#2655),#24961,.T.);
#25244=ADVANCED_FACE('',(#2656),#1732,.T.);
#25245=ADVANCED_FACE('',(#2657),#24962,.T.);
#25246=ADVANCED_FACE('',(#2658),#1733,.T.);
#25247=ADVANCED_FACE('',(#2659),#1118,.T.);
#25248=ADVANCED_FACE('',(#2660),#1119,.F.);
#25249=ADVANCED_FACE('',(#2661),#1120,.F.);
#25250=ADVANCED_FACE('',(#2662),#24963,.F.);
#25251=ADVANCED_FACE('',(#2663),#24964,.F.);
#25252=ADVANCED_FACE('',(#2664),#24965,.F.);
#25253=ADVANCED_FACE('',(#2665),#24966,.F.);
#25254=ADVANCED_FACE('',(#2666),#1734,.F.);
#25255=ADVANCED_FACE('',(#2667),#1735,.F.);
#25256=ADVANCED_FACE('',(#2668),#1736,.F.);
#25257=ADVANCED_FACE('',(#2669),#1121,.T.);
#25258=ADVANCED_FACE('',(#2670),#24967,.T.);
#25259=ADVANCED_FACE('',(#2671),#24968,.T.);
#25260=ADVANCED_FACE('',(#2672,#1561),#1737,.T.);
#25261=ADVANCED_FACE('',(#2673),#24969,.T.);
#25262=ADVANCED_FACE('',(#2674),#1122,.T.);
#25263=ADVANCED_FACE('',(#2675),#24970,.F.);
#25264=ADVANCED_FACE('',(#2676),#24971,.T.);
#25265=ADVANCED_FACE('',(#2677),#1123,.F.);
#25266=ADVANCED_FACE('',(#2678),#24972,.F.);
#25267=ADVANCED_FACE('',(#2679),#1124,.F.);
#25268=ADVANCED_FACE('',(#2680),#1738,.T.);
#25269=ADVANCED_FACE('',(#2681,#1562,#1563),#1739,.F.);
#25270=ADVANCED_FACE('',(#2682),#1740,.T.);
#25271=ADVANCED_FACE('',(#2683),#1741,.T.);
#25272=ADVANCED_FACE('',(#2684),#24973,.T.);
#25273=ADVANCED_FACE('',(#2685),#24974,.T.);
#25274=ADVANCED_FACE('',(#2686,#1564),#1742,.T.);
#25275=ADVANCED_FACE('',(#2687),#138,.T.);
#25276=ADVANCED_FACE('',(#2688,#1565,#1566,#1567),#1125,.T.);
#25277=ADVANCED_FACE('',(#2689),#1126,.F.);
#25278=ADVANCED_FACE('',(#2690),#24975,.T.);
#25279=ADVANCED_FACE('',(#2691),#1743,.T.);
#25280=ADVANCED_FACE('',(#2692),#1744,.F.);
#25281=ADVANCED_FACE('',(#2693),#24976,.T.);
#25282=ADVANCED_FACE('',(#2694),#139,.T.);
#25283=ADVANCED_FACE('',(#2695),#140,.T.);
#25284=ADVANCED_FACE('',(#2696),#141,.T.);
#25285=ADVANCED_FACE('',(#2697),#1745,.T.);
#25286=ADVANCED_FACE('',(#2698),#1746,.T.);
#25287=ADVANCED_FACE('',(#2699),#1747,.T.);
#25288=ADVANCED_FACE('',(#2700),#1748,.T.);
#25289=ADVANCED_FACE('',(#2701),#1749,.T.);
#25290=ADVANCED_FACE('',(#2702),#1750,.T.);
#25291=ADVANCED_FACE('',(#2703),#24977,.T.);
#25292=ADVANCED_FACE('',(#2704),#1751,.T.);
#25293=ADVANCED_FACE('',(#2705),#24978,.T.);
#25294=ADVANCED_FACE('',(#2706),#1752,.T.);
#25295=ADVANCED_FACE('',(#2707),#1753,.T.);
#25296=ADVANCED_FACE('',(#2708),#1754,.T.);
#25297=ADVANCED_FACE('',(#2709),#1755,.T.);
#25298=ADVANCED_FACE('',(#2710),#1756,.T.);
#25299=ADVANCED_FACE('',(#2711),#24979,.T.);
#25300=ADVANCED_FACE('',(#2712),#24980,.T.);
#25301=ADVANCED_FACE('',(#2713),#142,.T.);
#25302=ADVANCED_FACE('',(#2714),#143,.T.);
#25303=ADVANCED_FACE('',(#2715),#144,.T.);
#25304=ADVANCED_FACE('',(#2716),#1757,.T.);
#25305=ADVANCED_FACE('',(#2717),#1127,.T.);
#25306=ADVANCED_FACE('',(#2718,#1568),#1758,.T.);
#25307=ADVANCED_FACE('',(#2719),#1128,.T.);
#25308=ADVANCED_FACE('',(#2720),#1759,.F.);
#25309=ADVANCED_FACE('',(#2721),#1760,.F.);
#25310=ADVANCED_FACE('',(#2722),#1761,.F.);
#25311=ADVANCED_FACE('',(#2723,#1569,#1570),#1762,.F.);
#25312=ADVANCED_FACE('',(#2724),#1763,.T.);
#25313=ADVANCED_FACE('',(#2725),#24981,.F.);
#25314=ADVANCED_FACE('',(#2726),#1764,.T.);
#25315=ADVANCED_FACE('',(#2727),#24982,.F.);
#25316=ADVANCED_FACE('',(#2728),#1129,.F.);
#25317=ADVANCED_FACE('',(#2729),#1765,.F.);
#25318=ADVANCED_FACE('',(#2730),#1766,.T.);
#25319=ADVANCED_FACE('',(#2731),#24983,.F.);
#25320=ADVANCED_FACE('',(#2732),#1767,.T.);
#25321=ADVANCED_FACE('',(#2733),#24984,.F.);
#25322=ADVANCED_FACE('',(#2734),#1130,.F.);
#25323=ADVANCED_FACE('',(#2735),#1768,.F.);
#25324=ADVANCED_FACE('',(#2736),#1769,.T.);
#25325=ADVANCED_FACE('',(#2737),#24985,.F.);
#25326=ADVANCED_FACE('',(#2738),#1770,.T.);
#25327=ADVANCED_FACE('',(#2739),#24986,.F.);
#25328=ADVANCED_FACE('',(#2740),#1131,.F.);
#25329=ADVANCED_FACE('',(#2741),#1771,.F.);
#25330=ADVANCED_FACE('',(#2742),#1772,.T.);
#25331=ADVANCED_FACE('',(#2743),#24987,.F.);
#25332=ADVANCED_FACE('',(#2744),#1773,.T.);
#25333=ADVANCED_FACE('',(#2745),#24988,.F.);
#25334=ADVANCED_FACE('',(#2746),#1132,.F.);
#25335=ADVANCED_FACE('',(#2747),#1774,.F.);
#25336=ADVANCED_FACE('',(#2748),#24989,.F.);
#25337=ADVANCED_FACE('',(#2749),#1133,.F.);
#25338=ADVANCED_FACE('',(#2750),#24990,.F.);
#25339=ADVANCED_FACE('',(#2751),#1134,.F.);
#25340=ADVANCED_FACE('',(#2752),#1775,.T.);
#25341=ADVANCED_FACE('',(#2753),#24991,.F.);
#25342=ADVANCED_FACE('',(#2754),#1776,.T.);
#25343=ADVANCED_FACE('',(#2755),#24992,.F.);
#25344=ADVANCED_FACE('',(#2756),#1135,.F.);
#25345=ADVANCED_FACE('',(#2757,#1571,#1572,#1573,#1574),#1777,.T.);
#25346=ADVANCED_FACE('',(#2758),#1778,.T.);
#25347=ADVANCED_FACE('',(#2759),#24993,.F.);
#25348=ADVANCED_FACE('',(#2760),#1779,.T.);
#25349=ADVANCED_FACE('',(#2761),#24994,.F.);
#25350=ADVANCED_FACE('',(#2762),#1136,.F.);
#25351=ADVANCED_FACE('',(#2763),#1780,.T.);
#25352=ADVANCED_FACE('',(#2764),#24995,.F.);
#25353=ADVANCED_FACE('',(#2765),#1781,.T.);
#25354=ADVANCED_FACE('',(#2766),#24996,.F.);
#25355=ADVANCED_FACE('',(#2767),#1137,.F.);
#25356=ADVANCED_FACE('',(#2768),#1782,.T.);
#25357=ADVANCED_FACE('',(#2769),#24997,.F.);
#25358=ADVANCED_FACE('',(#2770),#1783,.T.);
#25359=ADVANCED_FACE('',(#2771),#24998,.F.);
#25360=ADVANCED_FACE('',(#2772),#1138,.F.);
#25361=ADVANCED_FACE('',(#2773),#145,.T.);
#25362=ADVANCED_FACE('',(#2774),#146,.T.);
#25363=ADVANCED_FACE('',(#2775),#147,.T.);
#25364=ADVANCED_FACE('',(#2776),#24999,.T.);
#25365=ADVANCED_FACE('',(#2777),#1784,.T.);
#25366=ADVANCED_FACE('',(#2778),#25000,.T.);
#25367=ADVANCED_FACE('',(#2779),#1785,.T.);
#25368=ADVANCED_FACE('',(#2780),#25001,.T.);
#25369=ADVANCED_FACE('',(#2781),#1786,.T.);
#25370=ADVANCED_FACE('',(#2782),#25002,.T.);
#25371=ADVANCED_FACE('',(#2783),#148,.T.);
#25372=ADVANCED_FACE('',(#2784),#149,.T.);
#25373=ADVANCED_FACE('',(#2785),#150,.T.);
#25374=ADVANCED_FACE('',(#2786),#1139,.T.);
#25375=ADVANCED_FACE('',(#2787),#1140,.T.);
#25376=ADVANCED_FACE('',(#2788),#1787,.T.);
#25377=ADVANCED_FACE('',(#2789),#1141,.T.);
#25378=ADVANCED_FACE('',(#2790),#1788,.T.);
#25379=ADVANCED_FACE('',(#2791),#1789,.T.);
#25380=ADVANCED_FACE('',(#2792),#25003,.T.);
#25381=ADVANCED_FACE('',(#2793),#151,.T.);
#25382=ADVANCED_FACE('',(#2794),#152,.T.);
#25383=ADVANCED_FACE('',(#2795),#153,.T.);
#25384=ADVANCED_FACE('',(#2796),#1790,.T.);
#25385=ADVANCED_FACE('',(#2797),#1142,.F.);
#25386=ADVANCED_FACE('',(#2798),#1791,.T.);
#25387=ADVANCED_FACE('',(#2799),#1792,.T.);
#25388=ADVANCED_FACE('',(#2800),#154,.T.);
#25389=ADVANCED_FACE('',(#2801),#1793,.F.);
#25390=ADVANCED_FACE('',(#2802),#1143,.T.);
#25391=ADVANCED_FACE('',(#2803),#1794,.T.);
#25392=ADVANCED_FACE('',(#2804),#155,.T.);
#25393=ADVANCED_FACE('',(#2805),#1795,.T.);
#25394=ADVANCED_FACE('',(#2806),#1144,.T.);
#25395=ADVANCED_FACE('',(#2807),#156,.F.);
#25396=ADVANCED_FACE('',(#2808),#157,.F.);
#25397=ADVANCED_FACE('',(#2809),#1145,.T.);
#25398=ADVANCED_FACE('',(#2810),#1796,.T.);
#25399=ADVANCED_FACE('',(#2811),#1146,.T.);
#25400=ADVANCED_FACE('',(#2812),#1147,.T.);
#25401=ADVANCED_FACE('',(#2813),#1083,.T.);
#25402=ADVANCED_FACE('',(#2814),#1148,.T.);
#25403=ADVANCED_FACE('',(#2815),#1149,.T.);
#25404=ADVANCED_FACE('',(#2816),#1150,.T.);
#25405=ADVANCED_FACE('',(#2817),#1084,.F.);
#25406=ADVANCED_FACE('',(#2818),#1797,.F.);
#25407=ADVANCED_FACE('',(#2819),#1798,.F.);
#25408=ADVANCED_FACE('',(#2820),#1799,.F.);
#25409=ADVANCED_FACE('',(#2821),#1800,.F.);
#25410=ADVANCED_FACE('',(#2822),#25004,.F.);
#25411=ADVANCED_FACE('',(#2823),#25005,.F.);
#25412=ADVANCED_FACE('',(#2824),#25006,.F.);
#25413=ADVANCED_FACE('',(#2825),#25007,.F.);
#25414=ADVANCED_FACE('',(#2826,#1575),#1801,.F.);
#25415=ADVANCED_FACE('',(#2827),#1151,.F.);
#25416=ADVANCED_FACE('',(#2828),#1152,.F.);
#25417=ADVANCED_FACE('',(#2829,#1576),#1802,.F.);
#25418=ADVANCED_FACE('',(#2830),#1153,.F.);
#25419=ADVANCED_FACE('',(#2831,#1577,#1578),#1154,.F.);
#25420=ADVANCED_FACE('',(#2832,#1579),#1803,.T.);
#25421=ADVANCED_FACE('',(#2833),#25008,.T.);
#25422=ADVANCED_FACE('',(#2834),#25009,.T.);
#25423=ADVANCED_FACE('',(#2835,#1580),#1804,.T.);
#25424=ADVANCED_FACE('',(#2836),#1805,.F.);
#25425=ADVANCED_FACE('',(#2837),#1806,.F.);
#25426=ADVANCED_FACE('',(#2838),#1807,.F.);
#25427=ADVANCED_FACE('',(#2839),#1808,.F.);
#25428=ADVANCED_FACE('',(#2840),#1809,.F.);
#25429=ADVANCED_FACE('',(#2841),#1810,.F.);
#25430=ADVANCED_FACE('',(#2842),#1811,.F.);
#25431=ADVANCED_FACE('',(#2843),#1812,.F.);
#25432=ADVANCED_FACE('',(#2844),#1813,.F.);
#25433=ADVANCED_FACE('',(#2845),#1814,.F.);
#25434=ADVANCED_FACE('',(#2846),#1815,.F.);
#25435=ADVANCED_FACE('',(#2847),#1816,.F.);
#25436=ADVANCED_FACE('',(#2848),#1817,.F.);
#25437=ADVANCED_FACE('',(#2849),#1818,.F.);
#25438=ADVANCED_FACE('',(#2850),#1819,.F.);
#25439=ADVANCED_FACE('',(#2851),#1820,.F.);
#25440=ADVANCED_FACE('',(#2852),#1821,.F.);
#25441=ADVANCED_FACE('',(#2853),#1822,.F.);
#25442=ADVANCED_FACE('',(#2854),#1823,.F.);
#25443=ADVANCED_FACE('',(#2855),#1824,.F.);
#25444=ADVANCED_FACE('',(#2856),#1825,.F.);
#25445=ADVANCED_FACE('',(#2857),#1826,.F.);
#25446=ADVANCED_FACE('',(#2858),#1827,.F.);
#25447=ADVANCED_FACE('',(#2859),#1828,.F.);
#25448=ADVANCED_FACE('',(#2860),#1829,.F.);
#25449=ADVANCED_FACE('',(#2861),#1830,.F.);
#25450=ADVANCED_FACE('',(#2862),#1831,.F.);
#25451=ADVANCED_FACE('',(#2863),#1832,.F.);
#25452=ADVANCED_FACE('',(#2864),#1833,.F.);
#25453=ADVANCED_FACE('',(#2865),#1834,.F.);
#25454=ADVANCED_FACE('',(#2866),#1835,.F.);
#25455=ADVANCED_FACE('',(#2867),#1836,.F.);
#25456=ADVANCED_FACE('',(#2868),#1837,.F.);
#25457=ADVANCED_FACE('',(#2869),#1838,.F.);
#25458=ADVANCED_FACE('',(#2870),#1839,.F.);
#25459=ADVANCED_FACE('',(#2871),#1840,.F.);
#25460=ADVANCED_FACE('',(#2872),#1841,.F.);
#25461=ADVANCED_FACE('',(#2873),#1842,.F.);
#25462=ADVANCED_FACE('',(#2874),#1843,.F.);
#25463=ADVANCED_FACE('',(#2875),#1844,.F.);
#25464=ADVANCED_FACE('',(#2876),#1845,.F.);
#25465=ADVANCED_FACE('',(#2877),#1846,.F.);
#25466=ADVANCED_FACE('',(#2878),#1847,.F.);
#25467=ADVANCED_FACE('',(#2879),#1848,.F.);
#25468=ADVANCED_FACE('',(#2880),#1849,.F.);
#25469=ADVANCED_FACE('',(#2881),#1850,.F.);
#25470=ADVANCED_FACE('',(#2882),#1851,.F.);
#25471=ADVANCED_FACE('',(#2883),#1852,.F.);
#25472=ADVANCED_FACE('',(#2884),#1853,.F.);
#25473=ADVANCED_FACE('',(#2885),#1854,.F.);
#25474=ADVANCED_FACE('',(#2886),#1855,.F.);
#25475=ADVANCED_FACE('',(#2887),#1856,.F.);
#25476=ADVANCED_FACE('',(#2888),#1857,.F.);
#25477=ADVANCED_FACE('',(#2889),#1858,.F.);
#25478=ADVANCED_FACE('',(#2890),#1859,.F.);
#25479=ADVANCED_FACE('',(#2891),#1860,.F.);
#25480=ADVANCED_FACE('',(#2892),#1861,.F.);
#25481=ADVANCED_FACE('',(#2893),#1862,.F.);
#25482=ADVANCED_FACE('',(#2894),#1863,.F.);
#25483=ADVANCED_FACE('',(#2895),#1864,.F.);
#25484=ADVANCED_FACE('',(#2896),#1865,.F.);
#25485=ADVANCED_FACE('',(#2897),#1866,.F.);
#25486=ADVANCED_FACE('',(#2898),#1867,.F.);
#25487=ADVANCED_FACE('',(#2899),#1868,.F.);
#25488=ADVANCED_FACE('',(#2900),#1869,.F.);
#25489=ADVANCED_FACE('',(#2901),#1870,.F.);
#25490=ADVANCED_FACE('',(#2902),#1871,.F.);
#25491=ADVANCED_FACE('',(#2903),#1872,.F.);
#25492=ADVANCED_FACE('',(#2904),#1873,.F.);
#25493=ADVANCED_FACE('',(#2905),#1874,.F.);
#25494=ADVANCED_FACE('',(#2906),#1875,.F.);
#25495=ADVANCED_FACE('',(#2907),#1876,.F.);
#25496=ADVANCED_FACE('',(#2908),#1877,.F.);
#25497=ADVANCED_FACE('',(#2909),#1878,.F.);
#25498=ADVANCED_FACE('',(#2910),#1879,.F.);
#25499=ADVANCED_FACE('',(#2911),#1880,.F.);
#25500=ADVANCED_FACE('',(#2912),#1881,.F.);
#25501=ADVANCED_FACE('',(#2913),#1882,.F.);
#25502=ADVANCED_FACE('',(#2914),#1883,.F.);
#25503=ADVANCED_FACE('',(#2915),#1884,.F.);
#25504=ADVANCED_FACE('',(#2916),#1885,.F.);
#25505=ADVANCED_FACE('',(#2917),#1886,.F.);
#25506=ADVANCED_FACE('',(#2918),#1887,.F.);
#25507=ADVANCED_FACE('',(#2919),#1888,.F.);
#25508=ADVANCED_FACE('',(#2920),#1889,.F.);
#25509=ADVANCED_FACE('',(#2921),#1890,.F.);
#25510=ADVANCED_FACE('',(#2922),#1891,.F.);
#25511=ADVANCED_FACE('',(#2923),#1892,.F.);
#25512=ADVANCED_FACE('',(#2924),#1893,.F.);
#25513=ADVANCED_FACE('',(#2925),#1894,.F.);
#25514=ADVANCED_FACE('',(#2926),#1895,.F.);
#25515=ADVANCED_FACE('',(#2927),#1896,.F.);
#25516=ADVANCED_FACE('',(#2928),#1897,.F.);
#25517=ADVANCED_FACE('',(#2929),#1898,.F.);
#25518=ADVANCED_FACE('',(#2930),#1899,.F.);
#25519=ADVANCED_FACE('',(#2931),#1900,.F.);
#25520=ADVANCED_FACE('',(#2932),#1901,.F.);
#25521=ADVANCED_FACE('',(#2933),#1902,.F.);
#25522=ADVANCED_FACE('',(#2934),#1903,.F.);
#25523=ADVANCED_FACE('',(#2935),#1904,.F.);
#25524=ADVANCED_FACE('',(#2936),#1905,.F.);
#25525=ADVANCED_FACE('',(#2937),#1906,.F.);
#25526=ADVANCED_FACE('',(#2938),#1907,.F.);
#25527=ADVANCED_FACE('',(#2939),#1908,.F.);
#25528=ADVANCED_FACE('',(#2940),#1909,.F.);
#25529=ADVANCED_FACE('',(#2941),#1910,.F.);
#25530=ADVANCED_FACE('',(#2942),#1155,.F.);
#25531=ADVANCED_FACE('',(#2943),#1911,.F.);
#25532=ADVANCED_FACE('',(#2944),#1156,.F.);
#25533=ADVANCED_FACE('',(#2945),#1912,.F.);
#25534=ADVANCED_FACE('',(#2946),#1157,.F.);
#25535=ADVANCED_FACE('',(#2947,#1581),#1913,.T.);
#25536=ADVANCED_FACE('',(#2948),#25010,.T.);
#25537=ADVANCED_FACE('',(#2949,#1582,#1583,#1584,#1585,#1586,#1587,#1588,
#1589,#1590,#1591,#1592,#1593,#1594,#1595,#1596,#1597,#1598,#1599,#1600,
#1601,#1602,#1603),#1158,.T.);
#25538=ADVANCED_FACE('',(#2950),#25011,.F.);
#25539=ADVANCED_FACE('',(#2951),#25012,.F.);
#25540=ADVANCED_FACE('',(#2952,#1604),#1914,.T.);
#25541=ADVANCED_FACE('',(#2953),#1159,.F.);
#25542=ADVANCED_FACE('',(#2954,#1605),#1915,.T.);
#25543=ADVANCED_FACE('',(#2955),#25013,.T.);
#25544=ADVANCED_FACE('',(#2956),#25014,.T.);
#25545=ADVANCED_FACE('',(#2957),#25015,.T.);
#25546=ADVANCED_FACE('',(#2958),#1916,.T.);
#25547=ADVANCED_FACE('',(#2959),#25016,.T.);
#25548=ADVANCED_FACE('',(#2960),#25017,.T.);
#25549=ADVANCED_FACE('',(#2961),#1160,.T.);
#25550=ADVANCED_FACE('',(#2962),#1161,.T.);
#25551=ADVANCED_FACE('',(#2963),#1162,.T.);
#25552=ADVANCED_FACE('',(#2964),#1163,.T.);
#25553=ADVANCED_FACE('',(#2965),#1164,.T.);
#25554=ADVANCED_FACE('',(#2966),#1165,.T.);
#25555=ADVANCED_FACE('',(#2967),#1166,.T.);
#25556=ADVANCED_FACE('',(#2968),#1167,.T.);
#25557=ADVANCED_FACE('',(#2969),#1168,.T.);
#25558=ADVANCED_FACE('',(#2970),#1169,.T.);
#25559=ADVANCED_FACE('',(#2971),#1170,.T.);
#25560=ADVANCED_FACE('',(#2972),#1171,.T.);
#25561=ADVANCED_FACE('',(#2973),#1172,.T.);
#25562=ADVANCED_FACE('',(#2974),#1173,.T.);
#25563=ADVANCED_FACE('',(#2975),#1174,.T.);
#25564=ADVANCED_FACE('',(#2976),#1175,.T.);
#25565=ADVANCED_FACE('',(#2977),#1176,.T.);
#25566=ADVANCED_FACE('',(#2978),#1177,.T.);
#25567=ADVANCED_FACE('',(#2979),#1178,.T.);
#25568=ADVANCED_FACE('',(#2980),#1179,.T.);
#25569=ADVANCED_FACE('',(#2981),#1180,.T.);
#25570=ADVANCED_FACE('',(#2982),#1181,.T.);
#25571=ADVANCED_FACE('',(#2983),#1182,.T.);
#25572=ADVANCED_FACE('',(#2984),#1183,.T.);
#25573=ADVANCED_FACE('',(#2985),#1184,.T.);
#25574=ADVANCED_FACE('',(#2986),#1185,.T.);
#25575=ADVANCED_FACE('',(#2987),#1186,.T.);
#25576=ADVANCED_FACE('',(#2988),#1187,.T.);
#25577=ADVANCED_FACE('',(#2989),#1188,.T.);
#25578=ADVANCED_FACE('',(#2990),#1189,.T.);
#25579=ADVANCED_FACE('',(#2991),#1190,.T.);
#25580=ADVANCED_FACE('',(#2992),#1191,.T.);
#25581=ADVANCED_FACE('',(#2993),#1192,.T.);
#25582=ADVANCED_FACE('',(#2994),#1193,.T.);
#25583=ADVANCED_FACE('',(#2995),#1194,.T.);
#25584=ADVANCED_FACE('',(#2996),#1195,.T.);
#25585=ADVANCED_FACE('',(#2997),#1196,.T.);
#25586=ADVANCED_FACE('',(#2998),#1197,.T.);
#25587=ADVANCED_FACE('',(#2999),#1198,.T.);
#25588=ADVANCED_FACE('',(#3000),#1199,.T.);
#25589=ADVANCED_FACE('',(#3001),#1200,.T.);
#25590=ADVANCED_FACE('',(#3002),#1201,.T.);
#25591=ADVANCED_FACE('',(#3003),#1202,.T.);
#25592=ADVANCED_FACE('',(#3004),#1203,.T.);
#25593=ADVANCED_FACE('',(#3005),#1204,.T.);
#25594=ADVANCED_FACE('',(#3006),#1205,.T.);
#25595=ADVANCED_FACE('',(#3007),#1206,.T.);
#25596=ADVANCED_FACE('',(#3008),#1207,.T.);
#25597=ADVANCED_FACE('',(#3009),#1208,.T.);
#25598=ADVANCED_FACE('',(#3010),#1209,.T.);
#25599=ADVANCED_FACE('',(#3011),#1210,.T.);
#25600=ADVANCED_FACE('',(#3012),#1211,.T.);
#25601=ADVANCED_FACE('',(#3013),#1212,.T.);
#25602=ADVANCED_FACE('',(#3014),#1213,.T.);
#25603=ADVANCED_FACE('',(#3015),#1214,.T.);
#25604=ADVANCED_FACE('',(#3016),#1215,.T.);
#25605=ADVANCED_FACE('',(#3017),#1216,.T.);
#25606=ADVANCED_FACE('',(#3018),#1217,.T.);
#25607=ADVANCED_FACE('',(#3019),#1218,.T.);
#25608=ADVANCED_FACE('',(#3020),#1219,.T.);
#25609=ADVANCED_FACE('',(#3021),#1220,.T.);
#25610=ADVANCED_FACE('',(#3022),#1221,.T.);
#25611=ADVANCED_FACE('',(#3023),#1222,.T.);
#25612=ADVANCED_FACE('',(#3024),#1223,.T.);
#25613=ADVANCED_FACE('',(#3025),#1224,.T.);
#25614=ADVANCED_FACE('',(#3026),#1225,.T.);
#25615=ADVANCED_FACE('',(#3027),#1226,.T.);
#25616=ADVANCED_FACE('',(#3028),#1227,.T.);
#25617=ADVANCED_FACE('',(#3029),#1228,.T.);
#25618=ADVANCED_FACE('',(#3030),#1229,.T.);
#25619=ADVANCED_FACE('',(#3031),#1230,.T.);
#25620=ADVANCED_FACE('',(#3032),#1231,.T.);
#25621=ADVANCED_FACE('',(#3033),#1232,.T.);
#25622=ADVANCED_FACE('',(#3034),#1233,.T.);
#25623=ADVANCED_FACE('',(#3035),#1234,.T.);
#25624=ADVANCED_FACE('',(#3036),#1235,.T.);
#25625=ADVANCED_FACE('',(#3037),#1236,.T.);
#25626=ADVANCED_FACE('',(#3038),#1237,.T.);
#25627=ADVANCED_FACE('',(#3039),#1238,.T.);
#25628=ADVANCED_FACE('',(#3040),#1239,.T.);
#25629=ADVANCED_FACE('',(#3041),#1240,.T.);
#25630=ADVANCED_FACE('',(#3042),#1241,.T.);
#25631=ADVANCED_FACE('',(#3043),#1242,.T.);
#25632=ADVANCED_FACE('',(#3044),#1243,.T.);
#25633=ADVANCED_FACE('',(#3045),#25018,.T.);
#25634=ADVANCED_FACE('',(#3046),#25019,.T.);
#25635=ADVANCED_FACE('',(#3047),#1917,.T.);
#25636=ADVANCED_FACE('',(#3048),#25020,.F.);
#25637=ADVANCED_FACE('',(#3049),#1244,.F.);
#25638=ADVANCED_FACE('',(#3050,#1606),#1918,.T.);
#25639=ADVANCED_FACE('',(#3051),#25021,.T.);
#25640=ADVANCED_FACE('',(#3052),#158,.F.);
#25641=ADVANCED_FACE('',(#3053),#25022,.T.);
#25642=ADVANCED_FACE('',(#3054),#1919,.F.);
#25643=ADVANCED_FACE('',(#3055),#159,.F.);
#25644=ADVANCED_FACE('',(#3056),#1245,.T.);
#25645=ADVANCED_FACE('',(#3057),#1246,.T.);
#25646=ADVANCED_FACE('',(#3058),#25023,.F.);
#25647=ADVANCED_FACE('',(#3059),#1920,.F.);
#25648=ADVANCED_FACE('',(#3060),#1247,.F.);
#25649=ADVANCED_FACE('',(#3061),#1921,.F.);
#25650=ADVANCED_FACE('',(#3062),#1248,.F.);
#25651=ADVANCED_FACE('',(#3063),#1922,.T.);
#25652=ADVANCED_FACE('',(#3064),#25024,.T.);
#25653=ADVANCED_FACE('',(#3065,#1607),#1249,.T.);
#25654=ADVANCED_FACE('',(#3066,#1608),#1923,.T.);
#25655=ADVANCED_FACE('',(#3067),#25025,.T.);
#25656=ADVANCED_FACE('',(#3068),#1250,.T.);
#25657=ADVANCED_FACE('',(#3069),#25026,.T.);
#25658=ADVANCED_FACE('',(#3070,#1609),#1924,.T.);
#25659=ADVANCED_FACE('',(#3071),#25027,.F.);
#25660=ADVANCED_FACE('',(#3072),#25028,.F.);
#25661=ADVANCED_FACE('',(#3073,#1610),#1925,.T.);
#25662=ADVANCED_FACE('',(#3074),#25029,.F.);
#25663=ADVANCED_FACE('',(#3075),#1251,.F.);
#25664=ADVANCED_FACE('',(#3076,#1611),#1926,.F.);
#25665=ADVANCED_FACE('',(#3077),#1252,.T.);
#25666=ADVANCED_FACE('',(#3078,#1612),#1927,.F.);
#25667=ADVANCED_FACE('',(#3079),#1253,.T.);
#25668=ADVANCED_FACE('',(#3080),#25030,.T.);
#25669=ADVANCED_FACE('',(#3081),#1254,.T.);
#25670=ADVANCED_FACE('',(#3082),#25031,.T.);
#25671=ADVANCED_FACE('',(#3083,#1613),#1928,.T.);
#25672=ADVANCED_FACE('',(#3084),#25032,.F.);
#25673=ADVANCED_FACE('',(#3085),#25033,.F.);
#25674=ADVANCED_FACE('',(#3086,#1614),#1929,.T.);
#25675=ADVANCED_FACE('',(#3087),#1255,.F.);
#25676=ADVANCED_FACE('',(#3088),#25034,.T.);
#25677=ADVANCED_FACE('',(#3089),#25035,.T.);
#25678=ADVANCED_FACE('',(#3090,#1615,#1616,#1617,#1618,#1619),#1930,.T.);
#25679=ADVANCED_FACE('',(#3091),#25036,.T.);
#25680=ADVANCED_FACE('',(#3092),#1256,.T.);
#25681=ADVANCED_FACE('',(#3093),#25037,.T.);
#25682=ADVANCED_FACE('',(#3094),#25038,.T.);
#25683=ADVANCED_FACE('',(#3095),#25039,.T.);
#25684=ADVANCED_FACE('',(#3096,#1620,#1621,#1622,#1623,#1624),#1931,.T.);
#25685=ADVANCED_FACE('',(#3097),#25040,.T.);
#25686=ADVANCED_FACE('',(#3098),#25041,.T.);
#25687=ADVANCED_FACE('',(#3099),#1257,.T.);
#25688=ADVANCED_FACE('',(#3100),#25042,.T.);
#25689=ADVANCED_FACE('',(#3101,#1625),#1932,.T.);
#25690=ADVANCED_FACE('',(#3102),#25043,.F.);
#25691=ADVANCED_FACE('',(#3103),#1258,.F.);
#25692=ADVANCED_FACE('',(#3104),#1259,.F.);
#25693=ADVANCED_FACE('',(#3105),#1260,.F.);
#25694=ADVANCED_FACE('',(#3106),#1261,.F.);
#25695=ADVANCED_FACE('',(#3107),#1262,.F.);
#25696=ADVANCED_FACE('',(#3108),#1263,.T.);
#25697=ADVANCED_FACE('',(#3109),#25044,.T.);
#25698=ADVANCED_FACE('',(#3110,#1626),#1933,.T.);
#25699=ADVANCED_FACE('',(#3111),#1264,.F.);
#25700=ADVANCED_FACE('',(#3112,#1627),#1934,.T.);
#25701=ADVANCED_FACE('',(#3113),#25045,.T.);
#25702=ADVANCED_FACE('',(#3114,#1628,#1629,#1630,#1631),#1265,.T.);
#25703=ADVANCED_FACE('',(#3115),#25046,.T.);
#25704=ADVANCED_FACE('',(#3116),#25047,.T.);
#25705=ADVANCED_FACE('',(#3117),#25048,.T.);
#25706=ADVANCED_FACE('',(#3118),#25049,.T.);
#25707=ADVANCED_FACE('',(#3119,#1632),#1935,.T.);
#25708=ADVANCED_FACE('',(#3120),#25050,.T.);
#25709=ADVANCED_FACE('',(#3121,#1633),#1936,.T.);
#25710=ADVANCED_FACE('',(#3122),#1937,.T.);
#25711=ADVANCED_FACE('',(#3123),#1938,.T.);
#25712=ADVANCED_FACE('',(#3124),#1939,.T.);
#25713=ADVANCED_FACE('',(#3125),#1940,.F.);
#25714=ADVANCED_FACE('',(#3126),#1941,.F.);
#25715=ADVANCED_FACE('',(#3127),#1942,.F.);
#25716=ADVANCED_FACE('',(#3128),#1266,.F.);
#25717=ADVANCED_FACE('',(#3129),#25051,.T.);
#25718=ADVANCED_FACE('',(#3130),#25052,.T.);
#25719=ADVANCED_FACE('',(#3131),#25053,.T.);
#25720=ADVANCED_FACE('',(#3132),#25054,.T.);
#25721=ADVANCED_FACE('',(#3133),#1085,.T.);
#25722=ADVANCED_FACE('',(#3134),#1267,.F.);
#25723=ADVANCED_FACE('',(#3135,#1634),#1943,.T.);
#25724=ADVANCED_FACE('',(#3136),#1268,.T.);
#25725=ADVANCED_FACE('',(#3137),#1269,.T.);
#25726=ADVANCED_FACE('',(#3138),#1270,.T.);
#25727=ADVANCED_FACE('',(#3139),#1271,.T.);
#25728=ADVANCED_FACE('',(#3140),#1272,.T.);
#25729=ADVANCED_FACE('',(#3141),#1273,.T.);
#25730=ADVANCED_FACE('',(#3142),#1274,.T.);
#25731=ADVANCED_FACE('',(#3143),#1275,.T.);
#25732=ADVANCED_FACE('',(#3144),#1276,.T.);
#25733=ADVANCED_FACE('',(#3145),#1277,.T.);
#25734=ADVANCED_FACE('',(#3146),#1278,.T.);
#25735=ADVANCED_FACE('',(#3147),#1279,.T.);
#25736=ADVANCED_FACE('',(#3148),#1280,.T.);
#25737=ADVANCED_FACE('',(#3149),#1281,.T.);
#25738=ADVANCED_FACE('',(#3150),#1282,.T.);
#25739=ADVANCED_FACE('',(#3151),#1283,.T.);
#25740=ADVANCED_FACE('',(#3152),#1284,.T.);
#25741=ADVANCED_FACE('',(#3153),#1285,.T.);
#25742=ADVANCED_FACE('',(#3154),#1286,.T.);
#25743=ADVANCED_FACE('',(#3155),#1287,.T.);
#25744=ADVANCED_FACE('',(#3156),#1288,.T.);
#25745=ADVANCED_FACE('',(#3157),#1289,.T.);
#25746=ADVANCED_FACE('',(#3158),#1290,.T.);
#25747=ADVANCED_FACE('',(#3159),#1291,.T.);
#25748=ADVANCED_FACE('',(#3160),#1292,.T.);
#25749=ADVANCED_FACE('',(#3161),#1293,.T.);
#25750=ADVANCED_FACE('',(#3162),#1294,.T.);
#25751=ADVANCED_FACE('',(#3163),#1295,.T.);
#25752=ADVANCED_FACE('',(#3164),#1296,.T.);
#25753=ADVANCED_FACE('',(#3165),#1297,.T.);
#25754=ADVANCED_FACE('',(#3166),#1298,.T.);
#25755=ADVANCED_FACE('',(#3167),#1944,.F.);
#25756=ADVANCED_FACE('',(#3168),#160,.F.);
#25757=ADVANCED_FACE('',(#3169),#1945,.T.);
#25758=ADVANCED_FACE('',(#3170),#1299,.T.);
#25759=ADVANCED_FACE('',(#3171),#161,.F.);
#25760=ADVANCED_FACE('',(#3172),#1086,.F.);
#25761=ADVANCED_FACE('',(#3173),#1300,.T.);
#25762=ADVANCED_FACE('',(#3174,#1635),#1946,.T.);
#25763=ADVANCED_FACE('',(#3175),#1947,.F.);
#25764=ADVANCED_FACE('',(#3176),#1948,.F.);
#25765=ADVANCED_FACE('',(#3177),#1949,.F.);
#25766=ADVANCED_FACE('',(#3178),#1950,.F.);
#25767=ADVANCED_FACE('',(#3179),#1951,.F.);
#25768=ADVANCED_FACE('',(#3180),#1952,.F.);
#25769=ADVANCED_FACE('',(#3181),#25055,.F.);
#25770=ADVANCED_FACE('',(#3182),#1953,.F.);
#25771=ADVANCED_FACE('',(#3183),#1954,.F.);
#25772=ADVANCED_FACE('',(#3184),#1955,.F.);
#25773=ADVANCED_FACE('',(#3185),#1956,.F.);
#25774=ADVANCED_FACE('',(#3186),#1957,.F.);
#25775=ADVANCED_FACE('',(#3187),#1958,.F.);
#25776=ADVANCED_FACE('',(#3188),#1959,.F.);
#25777=ADVANCED_FACE('',(#3189),#1960,.F.);
#25778=ADVANCED_FACE('',(#3190),#1961,.F.);
#25779=ADVANCED_FACE('',(#3191),#1962,.F.);
#25780=ADVANCED_FACE('',(#3192),#1963,.F.);
#25781=ADVANCED_FACE('',(#3193),#1964,.F.);
#25782=ADVANCED_FACE('',(#3194),#1965,.F.);
#25783=ADVANCED_FACE('',(#3195),#1966,.F.);
#25784=ADVANCED_FACE('',(#3196),#1967,.F.);
#25785=ADVANCED_FACE('',(#3197),#1968,.F.);
#25786=ADVANCED_FACE('',(#3198),#1969,.F.);
#25787=ADVANCED_FACE('',(#3199),#1970,.F.);
#25788=ADVANCED_FACE('',(#3200),#1971,.F.);
#25789=ADVANCED_FACE('',(#3201),#1972,.F.);
#25790=ADVANCED_FACE('',(#3202),#1973,.F.);
#25791=ADVANCED_FACE('',(#3203),#1974,.F.);
#25792=ADVANCED_FACE('',(#3204),#1975,.F.);
#25793=ADVANCED_FACE('',(#3205),#1976,.F.);
#25794=ADVANCED_FACE('',(#3206),#1977,.F.);
#25795=ADVANCED_FACE('',(#3207),#1978,.F.);
#25796=ADVANCED_FACE('',(#3208),#1979,.F.);
#25797=ADVANCED_FACE('',(#3209),#1980,.F.);
#25798=ADVANCED_FACE('',(#3210),#1981,.F.);
#25799=ADVANCED_FACE('',(#3211),#1982,.F.);
#25800=ADVANCED_FACE('',(#3212),#1983,.F.);
#25801=ADVANCED_FACE('',(#3213),#1984,.F.);
#25802=ADVANCED_FACE('',(#3214),#1985,.F.);
#25803=ADVANCED_FACE('',(#3215),#1986,.F.);
#25804=ADVANCED_FACE('',(#3216),#1987,.F.);
#25805=ADVANCED_FACE('',(#3217),#1988,.F.);
#25806=ADVANCED_FACE('',(#3218),#1989,.F.);
#25807=ADVANCED_FACE('',(#3219),#1990,.F.);
#25808=ADVANCED_FACE('',(#3220),#1991,.F.);
#25809=ADVANCED_FACE('',(#3221),#1992,.F.);
#25810=ADVANCED_FACE('',(#3222),#1993,.F.);
#25811=ADVANCED_FACE('',(#3223),#1994,.F.);
#25812=ADVANCED_FACE('',(#3224),#1995,.F.);
#25813=ADVANCED_FACE('',(#3225),#1996,.F.);
#25814=ADVANCED_FACE('',(#3226),#1997,.F.);
#25815=ADVANCED_FACE('',(#3227),#1998,.F.);
#25816=ADVANCED_FACE('',(#3228),#1999,.F.);
#25817=ADVANCED_FACE('',(#3229),#2000,.F.);
#25818=ADVANCED_FACE('',(#3230),#2001,.F.);
#25819=ADVANCED_FACE('',(#3231),#2002,.F.);
#25820=ADVANCED_FACE('',(#3232),#2003,.F.);
#25821=ADVANCED_FACE('',(#3233),#2004,.F.);
#25822=ADVANCED_FACE('',(#3234),#2005,.F.);
#25823=ADVANCED_FACE('',(#3235),#2006,.F.);
#25824=ADVANCED_FACE('',(#3236),#2007,.F.);
#25825=ADVANCED_FACE('',(#3237),#2008,.F.);
#25826=ADVANCED_FACE('',(#3238),#2009,.F.);
#25827=ADVANCED_FACE('',(#3239),#2010,.F.);
#25828=ADVANCED_FACE('',(#3240),#2011,.F.);
#25829=ADVANCED_FACE('',(#3241),#2012,.F.);
#25830=ADVANCED_FACE('',(#3242),#2013,.F.);
#25831=ADVANCED_FACE('',(#3243),#2014,.F.);
#25832=ADVANCED_FACE('',(#3244),#2015,.F.);
#25833=ADVANCED_FACE('',(#3245),#2016,.F.);
#25834=ADVANCED_FACE('',(#3246),#2017,.F.);
#25835=ADVANCED_FACE('',(#3247),#2018,.F.);
#25836=ADVANCED_FACE('',(#3248),#2019,.F.);
#25837=ADVANCED_FACE('',(#3249),#2020,.F.);
#25838=ADVANCED_FACE('',(#3250),#2021,.F.);
#25839=ADVANCED_FACE('',(#3251),#2022,.F.);
#25840=ADVANCED_FACE('',(#3252),#2023,.F.);
#25841=ADVANCED_FACE('',(#3253),#2024,.F.);
#25842=ADVANCED_FACE('',(#3254),#2025,.F.);
#25843=ADVANCED_FACE('',(#3255),#2026,.F.);
#25844=ADVANCED_FACE('',(#3256),#2027,.F.);
#25845=ADVANCED_FACE('',(#3257),#2028,.F.);
#25846=ADVANCED_FACE('',(#3258),#2029,.F.);
#25847=ADVANCED_FACE('',(#3259),#2030,.F.);
#25848=ADVANCED_FACE('',(#3260),#2031,.F.);
#25849=ADVANCED_FACE('',(#3261),#2032,.F.);
#25850=ADVANCED_FACE('',(#3262),#2033,.F.);
#25851=ADVANCED_FACE('',(#3263),#2034,.F.);
#25852=ADVANCED_FACE('',(#3264),#2035,.F.);
#25853=ADVANCED_FACE('',(#3265),#2036,.F.);
#25854=ADVANCED_FACE('',(#3266),#2037,.F.);
#25855=ADVANCED_FACE('',(#3267),#2038,.F.);
#25856=ADVANCED_FACE('',(#3268),#2039,.F.);
#25857=ADVANCED_FACE('',(#3269),#2040,.F.);
#25858=ADVANCED_FACE('',(#3270),#2041,.F.);
#25859=ADVANCED_FACE('',(#3271),#2042,.F.);
#25860=ADVANCED_FACE('',(#3272),#2043,.F.);
#25861=ADVANCED_FACE('',(#3273),#2044,.F.);
#25862=ADVANCED_FACE('',(#3274),#2045,.F.);
#25863=ADVANCED_FACE('',(#3275),#2046,.F.);
#25864=ADVANCED_FACE('',(#3276),#2047,.F.);
#25865=ADVANCED_FACE('',(#3277),#2048,.F.);
#25866=ADVANCED_FACE('',(#3278),#2049,.F.);
#25867=ADVANCED_FACE('',(#3279),#2050,.F.);
#25868=ADVANCED_FACE('',(#3280),#2051,.F.);
#25869=ADVANCED_FACE('',(#3281),#2052,.F.);
#25870=ADVANCED_FACE('',(#3282),#2053,.F.);
#25871=ADVANCED_FACE('',(#3283),#2054,.F.);
#25872=ADVANCED_FACE('',(#3284),#2055,.F.);
#25873=ADVANCED_FACE('',(#3285),#2056,.F.);
#25874=ADVANCED_FACE('',(#3286),#2057,.F.);
#25875=ADVANCED_FACE('',(#3287),#2058,.F.);
#25876=ADVANCED_FACE('',(#3288),#2059,.F.);
#25877=ADVANCED_FACE('',(#3289),#2060,.F.);
#25878=ADVANCED_FACE('',(#3290),#2061,.F.);
#25879=ADVANCED_FACE('',(#3291),#2062,.F.);
#25880=ADVANCED_FACE('',(#3292),#2063,.F.);
#25881=ADVANCED_FACE('',(#3293),#2064,.F.);
#25882=ADVANCED_FACE('',(#3294),#2065,.F.);
#25883=ADVANCED_FACE('',(#3295),#2066,.F.);
#25884=ADVANCED_FACE('',(#3296),#2067,.F.);
#25885=ADVANCED_FACE('',(#3297),#2068,.F.);
#25886=ADVANCED_FACE('',(#3298),#2069,.F.);
#25887=ADVANCED_FACE('',(#3299),#2070,.F.);
#25888=ADVANCED_FACE('',(#3300),#2071,.F.);
#25889=ADVANCED_FACE('',(#3301),#2072,.F.);
#25890=ADVANCED_FACE('',(#3302),#2073,.F.);
#25891=ADVANCED_FACE('',(#3303),#2074,.F.);
#25892=ADVANCED_FACE('',(#3304),#2075,.F.);
#25893=ADVANCED_FACE('',(#3305),#2076,.F.);
#25894=ADVANCED_FACE('',(#3306),#2077,.F.);
#25895=ADVANCED_FACE('',(#3307),#2078,.F.);
#25896=ADVANCED_FACE('',(#3308),#2079,.F.);
#25897=ADVANCED_FACE('',(#3309),#2080,.F.);
#25898=ADVANCED_FACE('',(#3310),#2081,.F.);
#25899=ADVANCED_FACE('',(#3311),#2082,.F.);
#25900=ADVANCED_FACE('',(#3312),#2083,.F.);
#25901=ADVANCED_FACE('',(#3313),#2084,.F.);
#25902=ADVANCED_FACE('',(#3314),#2085,.F.);
#25903=ADVANCED_FACE('',(#3315),#2086,.F.);
#25904=ADVANCED_FACE('',(#3316),#2087,.F.);
#25905=ADVANCED_FACE('',(#3317),#2088,.F.);
#25906=ADVANCED_FACE('',(#3318),#2089,.F.);
#25907=ADVANCED_FACE('',(#3319),#2090,.F.);
#25908=ADVANCED_FACE('',(#3320),#2091,.F.);
#25909=ADVANCED_FACE('',(#3321),#2092,.F.);
#25910=ADVANCED_FACE('',(#3322),#2093,.F.);
#25911=ADVANCED_FACE('',(#3323),#2094,.F.);
#25912=ADVANCED_FACE('',(#3324),#2095,.F.);
#25913=ADVANCED_FACE('',(#3325),#2096,.F.);
#25914=ADVANCED_FACE('',(#3326),#2097,.F.);
#25915=ADVANCED_FACE('',(#3327),#2098,.F.);
#25916=ADVANCED_FACE('',(#3328),#2099,.F.);
#25917=ADVANCED_FACE('',(#3329),#2100,.F.);
#25918=ADVANCED_FACE('',(#3330),#2101,.F.);
#25919=ADVANCED_FACE('',(#3331),#2102,.F.);
#25920=ADVANCED_FACE('',(#3332),#2103,.T.);
#25921=ADVANCED_FACE('',(#3333),#25056,.T.);
#25922=ADVANCED_FACE('',(#3334),#25057,.T.);
#25923=ADVANCED_FACE('',(#3335),#1301,.T.);
#25924=ADVANCED_FACE('',(#3336),#25058,.T.);
#25925=ADVANCED_FACE('',(#3337,#1636),#2104,.T.);
#25926=ADVANCED_FACE('',(#3338),#2105,.T.);
#25927=ADVANCED_FACE('',(#3339),#25059,.T.);
#25928=ADVANCED_FACE('',(#3340),#2106,.T.);
#25929=ADVANCED_FACE('',(#3341),#25060,.T.);
#25930=ADVANCED_FACE('',(#3342),#1302,.T.);
#25931=ADVANCED_FACE('',(#3343),#2107,.T.);
#25932=ADVANCED_FACE('',(#3344),#2108,.F.);
#25933=ADVANCED_FACE('',(#3345),#2109,.T.);
#25934=ADVANCED_FACE('',(#3346),#25061,.T.);
#25935=ADVANCED_FACE('',(#3347),#2110,.T.);
#25936=ADVANCED_FACE('',(#3348),#25062,.T.);
#25937=ADVANCED_FACE('',(#3349),#1303,.T.);
#25938=ADVANCED_FACE('',(#3350),#2111,.T.);
#25939=ADVANCED_FACE('',(#3351),#2112,.T.);
#25940=ADVANCED_FACE('',(#3352),#1304,.T.);
#25941=ADVANCED_FACE('',(#3353),#1305,.T.);
#25942=ADVANCED_FACE('',(#3354),#1306,.T.);
#25943=ADVANCED_FACE('',(#3355),#1307,.T.);
#25944=ADVANCED_FACE('',(#3356),#1308,.T.);
#25945=ADVANCED_FACE('',(#3357),#1309,.T.);
#25946=ADVANCED_FACE('',(#3358),#1310,.T.);
#25947=ADVANCED_FACE('',(#3359),#1311,.T.);
#25948=ADVANCED_FACE('',(#3360),#1312,.T.);
#25949=ADVANCED_FACE('',(#3361),#1313,.T.);
#25950=ADVANCED_FACE('',(#3362),#1314,.T.);
#25951=ADVANCED_FACE('',(#3363),#1315,.T.);
#25952=ADVANCED_FACE('',(#3364),#1316,.T.);
#25953=ADVANCED_FACE('',(#3365),#1317,.T.);
#25954=ADVANCED_FACE('',(#3366),#1318,.T.);
#25955=ADVANCED_FACE('',(#3367),#1319,.T.);
#25956=ADVANCED_FACE('',(#3368),#1320,.T.);
#25957=ADVANCED_FACE('',(#3369),#1321,.T.);
#25958=ADVANCED_FACE('',(#3370),#1322,.T.);
#25959=ADVANCED_FACE('',(#3371),#25063,.T.);
#25960=ADVANCED_FACE('',(#3372),#25064,.T.);
#25961=ADVANCED_FACE('',(#3373),#162,.F.);
#25962=ADVANCED_FACE('',(#3374),#2113,.T.);
#25963=ADVANCED_FACE('',(#3375),#1323,.T.);
#25964=ADVANCED_FACE('',(#3376),#163,.F.);
#25965=ADVANCED_FACE('',(#3377),#25065,.T.);
#25966=ADVANCED_FACE('',(#3378),#137,.T.);
#25967=ADVANCED_FACE('',(#3379),#2114,.T.);
#25968=ADVANCED_FACE('',(#3380),#2115,.T.);
#25969=ADVANCED_FACE('',(#3381),#2116,.T.);
#25970=ADVANCED_FACE('',(#3382),#25066,.T.);
#25971=ADVANCED_FACE('',(#3383),#1324,.T.);
#25972=ADVANCED_FACE('',(#3384,#1637),#2117,.T.);
#25973=ADVANCED_FACE('',(#3385),#1325,.T.);
#25974=ADVANCED_FACE('',(#3386),#1326,.F.);
#25975=ADVANCED_FACE('',(#3387),#1327,.T.);
#25976=ADVANCED_FACE('',(#3388),#25067,.T.);
#25977=ADVANCED_FACE('',(#3389),#2118,.T.);
#25978=ADVANCED_FACE('',(#3390),#1328,.T.);
#25979=ADVANCED_FACE('',(#3391),#1329,.T.);
#25980=ADVANCED_FACE('',(#3392),#1330,.T.);
#25981=ADVANCED_FACE('',(#3393),#1331,.T.);
#25982=ADVANCED_FACE('',(#3394),#1332,.T.);
#25983=ADVANCED_FACE('',(#3395),#1333,.T.);
#25984=ADVANCED_FACE('',(#3396),#1334,.T.);
#25985=ADVANCED_FACE('',(#3397),#1335,.T.);
#25986=ADVANCED_FACE('',(#3398),#1336,.T.);
#25987=ADVANCED_FACE('',(#3399),#1337,.T.);
#25988=ADVANCED_FACE('',(#3400),#1338,.T.);
#25989=ADVANCED_FACE('',(#3401),#1339,.T.);
#25990=ADVANCED_FACE('',(#3402),#1340,.T.);
#25991=ADVANCED_FACE('',(#3403),#1341,.T.);
#25992=ADVANCED_FACE('',(#3404),#1342,.T.);
#25993=ADVANCED_FACE('',(#3405),#1343,.T.);
#25994=ADVANCED_FACE('',(#3406),#1344,.T.);
#25995=ADVANCED_FACE('',(#3407),#1345,.T.);
#25996=ADVANCED_FACE('',(#3408),#1346,.T.);
#25997=ADVANCED_FACE('',(#3409),#1347,.T.);
#25998=ADVANCED_FACE('',(#3410),#1348,.T.);
#25999=ADVANCED_FACE('',(#3411),#1349,.T.);
#26000=ADVANCED_FACE('',(#3412),#1350,.T.);
#26001=ADVANCED_FACE('',(#3413),#1351,.T.);
#26002=ADVANCED_FACE('',(#3414),#1352,.T.);
#26003=ADVANCED_FACE('',(#3415),#1353,.T.);
#26004=ADVANCED_FACE('',(#3416),#1354,.T.);
#26005=ADVANCED_FACE('',(#3417),#1355,.T.);
#26006=ADVANCED_FACE('',(#3418),#164,.F.);
#26007=ADVANCED_FACE('',(#3419),#2119,.T.);
#26008=ADVANCED_FACE('',(#3420),#1356,.T.);
#26009=ADVANCED_FACE('',(#3421),#165,.F.);
#26010=ADVANCED_FACE('',(#3422,#1638),#2120,.T.);
#26011=ADVANCED_FACE('',(#3423),#2121,.F.);
#26012=ADVANCED_FACE('',(#3424),#2122,.F.);
#26013=ADVANCED_FACE('',(#3425),#2123,.F.);
#26014=ADVANCED_FACE('',(#3426),#2124,.F.);
#26015=ADVANCED_FACE('',(#3427),#2125,.F.);
#26016=ADVANCED_FACE('',(#3428),#2126,.F.);
#26017=ADVANCED_FACE('',(#3429),#2127,.F.);
#26018=ADVANCED_FACE('',(#3430,#1639),#2128,.T.);
#26019=ADVANCED_FACE('',(#3431),#25068,.T.);
#26020=ADVANCED_FACE('',(#3432),#1357,.T.);
#26021=ADVANCED_FACE('',(#3433),#1358,.T.);
#26022=ADVANCED_FACE('',(#3434),#25069,.T.);
#26023=ADVANCED_FACE('',(#3435),#2129,.T.);
#26024=ADVANCED_FACE('',(#3436),#2130,.T.);
#26025=ADVANCED_FACE('',(#3437),#2131,.T.);
#26026=ADVANCED_FACE('',(#3438),#2132,.T.);
#26027=ADVANCED_FACE('',(#3439),#2133,.T.);
#26028=ADVANCED_FACE('',(#3440),#2134,.T.);
#26029=ADVANCED_FACE('',(#3441),#2135,.T.);
#26030=ADVANCED_FACE('',(#3442),#2136,.T.);
#26031=ADVANCED_FACE('',(#3443),#2137,.T.);
#26032=ADVANCED_FACE('',(#3444),#2138,.T.);
#26033=ADVANCED_FACE('',(#3445),#2139,.T.);
#26034=ADVANCED_FACE('',(#3446),#2140,.T.);
#26035=ADVANCED_FACE('',(#3447),#2141,.T.);
#26036=ADVANCED_FACE('',(#3448),#2142,.T.);
#26037=ADVANCED_FACE('',(#3449),#2143,.T.);
#26038=ADVANCED_FACE('',(#3450),#2144,.F.);
#26039=ADVANCED_FACE('',(#3451),#2145,.T.);
#26040=ADVANCED_FACE('',(#3452),#2146,.T.);
#26041=ADVANCED_FACE('',(#3453),#2147,.T.);
#26042=ADVANCED_FACE('',(#3454),#1359,.T.);
#26043=ADVANCED_FACE('',(#3455),#1360,.T.);
#26044=ADVANCED_FACE('',(#3456),#1361,.T.);
#26045=ADVANCED_FACE('',(#3457),#1362,.T.);
#26046=ADVANCED_FACE('',(#3458),#1363,.T.);
#26047=ADVANCED_FACE('',(#3459),#1364,.T.);
#26048=ADVANCED_FACE('',(#3460),#1365,.T.);
#26049=ADVANCED_FACE('',(#3461),#1366,.T.);
#26050=ADVANCED_FACE('',(#3462),#1367,.T.);
#26051=ADVANCED_FACE('',(#3463),#1368,.T.);
#26052=ADVANCED_FACE('',(#3464),#1369,.T.);
#26053=ADVANCED_FACE('',(#3465),#1370,.T.);
#26054=ADVANCED_FACE('',(#3466),#1371,.T.);
#26055=ADVANCED_FACE('',(#3467),#1372,.T.);
#26056=ADVANCED_FACE('',(#3468),#1373,.T.);
#26057=ADVANCED_FACE('',(#3469),#1374,.T.);
#26058=ADVANCED_FACE('',(#3470),#1375,.T.);
#26059=ADVANCED_FACE('',(#3471),#1376,.T.);
#26060=ADVANCED_FACE('',(#3472),#1377,.T.);
#26061=ADVANCED_FACE('',(#3473),#1378,.T.);
#26062=ADVANCED_FACE('',(#3474),#1379,.T.);
#26063=ADVANCED_FACE('',(#3475),#1380,.T.);
#26064=ADVANCED_FACE('',(#3476),#1381,.T.);
#26065=ADVANCED_FACE('',(#3477),#1382,.T.);
#26066=ADVANCED_FACE('',(#3478),#1383,.T.);
#26067=ADVANCED_FACE('',(#3479),#1384,.T.);
#26068=ADVANCED_FACE('',(#3480),#1385,.T.);
#26069=ADVANCED_FACE('',(#3481),#1386,.T.);
#26070=ADVANCED_FACE('',(#3482),#1387,.T.);
#26071=ADVANCED_FACE('',(#3483),#1388,.T.);
#26072=ADVANCED_FACE('',(#3484),#1389,.T.);
#26073=ADVANCED_FACE('',(#3485),#1390,.T.);
#26074=ADVANCED_FACE('',(#3486),#1391,.T.);
#26075=ADVANCED_FACE('',(#3487),#1392,.T.);
#26076=ADVANCED_FACE('',(#3488),#1393,.T.);
#26077=ADVANCED_FACE('',(#3489),#1394,.T.);
#26078=ADVANCED_FACE('',(#3490),#1395,.T.);
#26079=ADVANCED_FACE('',(#3491),#1396,.T.);
#26080=ADVANCED_FACE('',(#3492),#1397,.T.);
#26081=ADVANCED_FACE('',(#3493),#1398,.T.);
#26082=ADVANCED_FACE('',(#3494),#166,.F.);
#26083=ADVANCED_FACE('',(#3495),#2148,.T.);
#26084=ADVANCED_FACE('',(#3496),#1399,.T.);
#26085=ADVANCED_FACE('',(#3497),#167,.F.);
#26086=ADVANCED_FACE('',(#3498),#25070,.T.);
#26087=ADVANCED_FACE('',(#3499),#2149,.T.);
#26088=ADVANCED_FACE('',(#3500),#2150,.T.);
#26089=ADVANCED_FACE('',(#3501),#2151,.T.);
#26090=ADVANCED_FACE('',(#3502,#1640),#2152,.F.);
#26091=ADVANCED_FACE('',(#3503),#2153,.T.);
#26092=ADVANCED_FACE('',(#3504),#2154,.T.);
#26093=ADVANCED_FACE('',(#3505),#2155,.T.);
#26094=ADVANCED_FACE('',(#3506),#2156,.T.);
#26095=ADVANCED_FACE('',(#3507),#2157,.T.);
#26096=ADVANCED_FACE('',(#3508),#25071,.T.);
#26097=ADVANCED_FACE('',(#3509),#1400,.T.);
#26098=ADVANCED_FACE('',(#3510,#1641),#2158,.T.);
#26099=ADVANCED_FACE('',(#3511),#1401,.T.);
#26100=ADVANCED_FACE('',(#3512),#25072,.F.);
#26101=ADVANCED_FACE('',(#3513),#25073,.F.);
#26102=ADVANCED_FACE('',(#3514,#1642),#2159,.T.);
#26103=ADVANCED_FACE('',(#3515),#25074,.F.);
#26104=ADVANCED_FACE('',(#3516),#1402,.F.);
#26105=ADVANCED_FACE('',(#3517),#25075,.F.);
#26106=ADVANCED_FACE('',(#3518),#25076,.F.);
#26107=ADVANCED_FACE('',(#3519),#25077,.F.);
#26108=ADVANCED_FACE('',(#3520,#1643),#2160,.F.);
#26109=ADVANCED_FACE('',(#3521),#25078,.T.);
#26110=ADVANCED_FACE('',(#3522),#2161,.T.);
#26111=ADVANCED_FACE('',(#3523),#25079,.T.);
#26112=ADVANCED_FACE('',(#3524),#2162,.T.);
#26113=ADVANCED_FACE('',(#3525),#25080,.T.);
#26114=ADVANCED_FACE('',(#3526),#2163,.T.);
#26115=ADVANCED_FACE('',(#3527),#25081,.T.);
#26116=ADVANCED_FACE('',(#3528),#2164,.T.);
#26117=ADVANCED_FACE('',(#3529),#2165,.T.);
#26118=ADVANCED_FACE('',(#3530),#1403,.T.);
#26119=ADVANCED_FACE('',(#3531),#2166,.T.);
#26120=ADVANCED_FACE('',(#3532),#1404,.T.);
#26121=ADVANCED_FACE('',(#3533),#2167,.T.);
#26122=ADVANCED_FACE('',(#3534),#25082,.T.);
#26123=ADVANCED_FACE('',(#3535),#2168,.T.);
#26124=ADVANCED_FACE('',(#3536),#25083,.T.);
#26125=ADVANCED_FACE('',(#3537),#2169,.T.);
#26126=ADVANCED_FACE('',(#3538),#25084,.T.);
#26127=ADVANCED_FACE('',(#3539),#2170,.T.);
#26128=ADVANCED_FACE('',(#3540),#25085,.T.);
#26129=ADVANCED_FACE('',(#3541),#2171,.T.);
#26130=ADVANCED_FACE('',(#3542),#25086,.T.);
#26131=ADVANCED_FACE('',(#3543),#2172,.T.);
#26132=ADVANCED_FACE('',(#3544),#25087,.T.);
#26133=ADVANCED_FACE('',(#3545),#25088,.T.);
#26134=ADVANCED_FACE('',(#3546),#2173,.T.);
#26135=ADVANCED_FACE('',(#3547),#25089,.T.);
#26136=ADVANCED_FACE('',(#3548),#2174,.T.);
#26137=ADVANCED_FACE('',(#3549),#2175,.T.);
#26138=ADVANCED_FACE('',(#3550),#25090,.T.);
#26139=ADVANCED_FACE('',(#3551),#2176,.T.);
#26140=ADVANCED_FACE('',(#3552),#25091,.T.);
#26141=ADVANCED_FACE('',(#3553),#2177,.T.);
#26142=ADVANCED_FACE('',(#3554),#25092,.T.);
#26143=ADVANCED_FACE('',(#3555),#2178,.T.);
#26144=ADVANCED_FACE('',(#3556),#25093,.T.);
#26145=ADVANCED_FACE('',(#3557),#25094,.T.);
#26146=ADVANCED_FACE('',(#3558),#2179,.T.);
#26147=ADVANCED_FACE('',(#3559),#25095,.T.);
#26148=ADVANCED_FACE('',(#3560),#2180,.T.);
#26149=ADVANCED_FACE('',(#3561),#2181,.T.);
#26150=ADVANCED_FACE('',(#3562),#25096,.T.);
#26151=ADVANCED_FACE('',(#3563),#2182,.T.);
#26152=ADVANCED_FACE('',(#3564),#25097,.T.);
#26153=ADVANCED_FACE('',(#3565),#1405,.T.);
#26154=ADVANCED_FACE('',(#3566),#2183,.T.);
#26155=ADVANCED_FACE('',(#3567),#1406,.T.);
#26156=ADVANCED_FACE('',(#3568),#2184,.T.);
#26157=ADVANCED_FACE('',(#3569),#25098,.T.);
#26158=ADVANCED_FACE('',(#3570),#25099,.T.);
#26159=ADVANCED_FACE('',(#3571),#1407,.T.);
#26160=ADVANCED_FACE('',(#3572),#1408,.F.);
#26161=ADVANCED_FACE('',(#3573,#1644),#2185,.T.);
#26162=ADVANCED_FACE('',(#3574),#25100,.T.);
#26163=ADVANCED_FACE('',(#3575),#1409,.T.);
#26164=ADVANCED_FACE('',(#3576,#1645),#2186,.T.);
#26165=ADVANCED_FACE('',(#3577),#1410,.T.);
#26166=ADVANCED_FACE('',(#3578,#1646),#2187,.T.);
#26167=ADVANCED_FACE('',(#3579),#1411,.T.);
#26168=ADVANCED_FACE('',(#3580),#25101,.T.);
#26169=ADVANCED_FACE('',(#3581,#1647),#2188,.T.);
#26170=ADVANCED_FACE('',(#3582),#1412,.F.);
#26171=ADVANCED_FACE('',(#3583,#1648),#2189,.T.);
#26172=ADVANCED_FACE('',(#3584),#1413,.F.);
#26173=ADVANCED_FACE('',(#3585,#1649),#2190,.T.);
#26174=ADVANCED_FACE('',(#3586),#1414,.T.);
#26175=ADVANCED_FACE('',(#3587),#1415,.T.);
#26176=ADVANCED_FACE('',(#3588),#1416,.T.);
#26177=ADVANCED_FACE('',(#3589),#1417,.T.);
#26178=ADVANCED_FACE('',(#3590),#1418,.T.);
#26179=ADVANCED_FACE('',(#3591),#1419,.T.);
#26180=ADVANCED_FACE('',(#3592),#1420,.T.);
#26181=ADVANCED_FACE('',(#3593),#1421,.T.);
#26182=ADVANCED_FACE('',(#3594),#1422,.T.);
#26183=ADVANCED_FACE('',(#3595),#1423,.T.);
#26184=ADVANCED_FACE('',(#3596),#1424,.T.);
#26185=ADVANCED_FACE('',(#3597),#1425,.T.);
#26186=ADVANCED_FACE('',(#3598),#1426,.T.);
#26187=ADVANCED_FACE('',(#3599),#1427,.T.);
#26188=ADVANCED_FACE('',(#3600),#1428,.T.);
#26189=ADVANCED_FACE('',(#3601),#1429,.T.);
#26190=ADVANCED_FACE('',(#3602),#1430,.T.);
#26191=ADVANCED_FACE('',(#3603),#1431,.T.);
#26192=ADVANCED_FACE('',(#3604),#1432,.T.);
#26193=ADVANCED_FACE('',(#3605),#1433,.T.);
#26194=ADVANCED_FACE('',(#3606),#1434,.T.);
#26195=ADVANCED_FACE('',(#3607),#1435,.T.);
#26196=ADVANCED_FACE('',(#3608),#1436,.T.);
#26197=ADVANCED_FACE('',(#3609),#1437,.T.);
#26198=ADVANCED_FACE('',(#3610),#1438,.T.);
#26199=ADVANCED_FACE('',(#3611),#1439,.T.);
#26200=ADVANCED_FACE('',(#3612),#1440,.T.);
#26201=ADVANCED_FACE('',(#3613),#1441,.T.);
#26202=ADVANCED_FACE('',(#3614),#1442,.T.);
#26203=ADVANCED_FACE('',(#3615),#1443,.T.);
#26204=ADVANCED_FACE('',(#3616),#1444,.T.);
#26205=ADVANCED_FACE('',(#3617),#1445,.T.);
#26206=ADVANCED_FACE('',(#3618),#1446,.T.);
#26207=ADVANCED_FACE('',(#3619),#1447,.T.);
#26208=ADVANCED_FACE('',(#3620),#1448,.T.);
#26209=ADVANCED_FACE('',(#3621),#1449,.T.);
#26210=ADVANCED_FACE('',(#3622),#1450,.T.);
#26211=ADVANCED_FACE('',(#3623),#1451,.T.);
#26212=ADVANCED_FACE('',(#3624),#1452,.T.);
#26213=ADVANCED_FACE('',(#3625),#1453,.T.);
#26214=ADVANCED_FACE('',(#3626),#1454,.T.);
#26215=ADVANCED_FACE('',(#3627),#1455,.T.);
#26216=ADVANCED_FACE('',(#3628),#1456,.T.);
#26217=ADVANCED_FACE('',(#3629),#1457,.T.);
#26218=ADVANCED_FACE('',(#3630),#1458,.T.);
#26219=ADVANCED_FACE('',(#3631),#168,.F.);
#26220=ADVANCED_FACE('',(#3632),#2191,.T.);
#26221=ADVANCED_FACE('',(#3633),#1459,.T.);
#26222=ADVANCED_FACE('',(#3634),#169,.F.);
#26223=ADVANCED_FACE('',(#3635),#25102,.T.);
#26224=ADVANCED_FACE('',(#3636),#2192,.T.);
#26225=ADVANCED_FACE('',(#3637),#2193,.T.);
#26226=ADVANCED_FACE('',(#3638),#2194,.T.);
#26227=ADVANCED_FACE('',(#3639,#1650),#2195,.F.);
#26228=ADVANCED_FACE('',(#3640),#2196,.T.);
#26229=ADVANCED_FACE('',(#3641),#2197,.T.);
#26230=ADVANCED_FACE('',(#3642),#2198,.T.);
#26231=ADVANCED_FACE('',(#3643),#2199,.T.);
#26232=ADVANCED_FACE('',(#3644),#2200,.T.);
#26233=ADVANCED_FACE('',(#3645),#25103,.T.);
#26234=ADVANCED_FACE('',(#3646),#1460,.T.);
#26235=ADVANCED_FACE('',(#3647,#1651),#2201,.T.);
#26236=ADVANCED_FACE('',(#3648),#1461,.T.);
#26237=ADVANCED_FACE('',(#3649),#1462,.T.);
#26238=ADVANCED_FACE('',(#3650),#1463,.T.);
#26239=ADVANCED_FACE('',(#3651),#1464,.T.);
#26240=ADVANCED_FACE('',(#3652),#1465,.T.);
#26241=ADVANCED_FACE('',(#3653),#1466,.T.);
#26242=ADVANCED_FACE('',(#3654),#1467,.T.);
#26243=ADVANCED_FACE('',(#3655),#1468,.T.);
#26244=ADVANCED_FACE('',(#3656),#1469,.T.);
#26245=ADVANCED_FACE('',(#3657),#1470,.T.);
#26246=ADVANCED_FACE('',(#3658),#1471,.T.);
#26247=ADVANCED_FACE('',(#3659),#1472,.T.);
#26248=ADVANCED_FACE('',(#3660),#1473,.T.);
#26249=ADVANCED_FACE('',(#3661),#1474,.T.);
#26250=ADVANCED_FACE('',(#3662),#1475,.T.);
#26251=ADVANCED_FACE('',(#3663),#1476,.T.);
#26252=ADVANCED_FACE('',(#3664),#1477,.T.);
#26253=ADVANCED_FACE('',(#3665),#1478,.T.);
#26254=ADVANCED_FACE('',(#3666),#1479,.T.);
#26255=ADVANCED_FACE('',(#3667),#1480,.T.);
#26256=ADVANCED_FACE('',(#3668),#1481,.T.);
#26257=ADVANCED_FACE('',(#3669),#1482,.T.);
#26258=ADVANCED_FACE('',(#3670),#1483,.T.);
#26259=ADVANCED_FACE('',(#3671),#1484,.T.);
#26260=ADVANCED_FACE('',(#3672),#1485,.T.);
#26261=ADVANCED_FACE('',(#3673),#1486,.T.);
#26262=ADVANCED_FACE('',(#3674),#1487,.T.);
#26263=ADVANCED_FACE('',(#3675),#1488,.T.);
#26264=ADVANCED_FACE('',(#3676),#1489,.T.);
#26265=ADVANCED_FACE('',(#3677),#1490,.T.);
#26266=ADVANCED_FACE('',(#3678),#1491,.T.);
#26267=ADVANCED_FACE('',(#3679),#1492,.T.);
#26268=ADVANCED_FACE('',(#3680),#1493,.T.);
#26269=ADVANCED_FACE('',(#3681),#1494,.T.);
#26270=ADVANCED_FACE('',(#3682),#1495,.T.);
#26271=ADVANCED_FACE('',(#3683),#1496,.T.);
#26272=ADVANCED_FACE('',(#3684),#1497,.T.);
#26273=ADVANCED_FACE('',(#3685),#1498,.T.);
#26274=ADVANCED_FACE('',(#3686),#1499,.T.);
#26275=ADVANCED_FACE('',(#3687),#1500,.T.);
#26276=ADVANCED_FACE('',(#3688),#1501,.T.);
#26277=ADVANCED_FACE('',(#3689),#1502,.T.);
#26278=ADVANCED_FACE('',(#3690),#1503,.T.);
#26279=ADVANCED_FACE('',(#3691),#1504,.T.);
#26280=ADVANCED_FACE('',(#3692),#1505,.T.);
#26281=ADVANCED_FACE('',(#3693),#1506,.T.);
#26282=ADVANCED_FACE('',(#3694),#1507,.T.);
#26283=ADVANCED_FACE('',(#3695),#2202,.F.);
#26284=ADVANCED_FACE('',(#3696),#170,.F.);
#26285=ADVANCED_FACE('',(#3697),#2203,.T.);
#26286=ADVANCED_FACE('',(#3698),#1508,.T.);
#26287=ADVANCED_FACE('',(#3699),#171,.F.);
#26288=ADVANCED_FACE('',(#3700),#1087,.F.);
#26289=ADVANCED_FACE('',(#3701),#1509,.T.);
#26290=ADVANCED_FACE('',(#3702,#1652),#2204,.T.);
#26291=ADVANCED_FACE('',(#3703),#2205,.F.);
#26292=ADVANCED_FACE('',(#3704),#2206,.F.);
#26293=ADVANCED_FACE('',(#3705),#2207,.F.);
#26294=ADVANCED_FACE('',(#3706),#2208,.F.);
#26295=ADVANCED_FACE('',(#3707),#2209,.F.);
#26296=ADVANCED_FACE('',(#3708),#2210,.F.);
#26297=ADVANCED_FACE('',(#3709),#25104,.F.);
#26298=ADVANCED_FACE('',(#3710),#2211,.F.);
#26299=ADVANCED_FACE('',(#3711),#2212,.F.);
#26300=ADVANCED_FACE('',(#3712),#2213,.F.);
#26301=ADVANCED_FACE('',(#3713),#2214,.F.);
#26302=ADVANCED_FACE('',(#3714),#2215,.F.);
#26303=ADVANCED_FACE('',(#3715),#2216,.F.);
#26304=ADVANCED_FACE('',(#3716),#2217,.F.);
#26305=ADVANCED_FACE('',(#3717),#2218,.F.);
#26306=ADVANCED_FACE('',(#3718),#2219,.F.);
#26307=ADVANCED_FACE('',(#3719),#2220,.F.);
#26308=ADVANCED_FACE('',(#3720),#2221,.F.);
#26309=ADVANCED_FACE('',(#3721),#2222,.F.);
#26310=ADVANCED_FACE('',(#3722),#2223,.F.);
#26311=ADVANCED_FACE('',(#3723),#2224,.F.);
#26312=ADVANCED_FACE('',(#3724),#2225,.F.);
#26313=ADVANCED_FACE('',(#3725),#2226,.F.);
#26314=ADVANCED_FACE('',(#3726),#2227,.F.);
#26315=ADVANCED_FACE('',(#3727),#2228,.F.);
#26316=ADVANCED_FACE('',(#3728),#2229,.F.);
#26317=ADVANCED_FACE('',(#3729),#2230,.F.);
#26318=ADVANCED_FACE('',(#3730),#2231,.F.);
#26319=ADVANCED_FACE('',(#3731),#2232,.F.);
#26320=ADVANCED_FACE('',(#3732),#2233,.F.);
#26321=ADVANCED_FACE('',(#3733),#2234,.F.);
#26322=ADVANCED_FACE('',(#3734),#2235,.F.);
#26323=ADVANCED_FACE('',(#3735),#2236,.F.);
#26324=ADVANCED_FACE('',(#3736),#2237,.F.);
#26325=ADVANCED_FACE('',(#3737),#2238,.F.);
#26326=ADVANCED_FACE('',(#3738),#2239,.F.);
#26327=ADVANCED_FACE('',(#3739),#2240,.F.);
#26328=ADVANCED_FACE('',(#3740),#2241,.F.);
#26329=ADVANCED_FACE('',(#3741),#2242,.F.);
#26330=ADVANCED_FACE('',(#3742),#2243,.F.);
#26331=ADVANCED_FACE('',(#3743),#2244,.F.);
#26332=ADVANCED_FACE('',(#3744),#2245,.F.);
#26333=ADVANCED_FACE('',(#3745),#2246,.F.);
#26334=ADVANCED_FACE('',(#3746),#2247,.F.);
#26335=ADVANCED_FACE('',(#3747),#2248,.F.);
#26336=ADVANCED_FACE('',(#3748),#2249,.F.);
#26337=ADVANCED_FACE('',(#3749),#2250,.F.);
#26338=ADVANCED_FACE('',(#3750),#2251,.F.);
#26339=ADVANCED_FACE('',(#3751),#2252,.F.);
#26340=ADVANCED_FACE('',(#3752),#2253,.F.);
#26341=ADVANCED_FACE('',(#3753),#2254,.F.);
#26342=ADVANCED_FACE('',(#3754),#2255,.F.);
#26343=ADVANCED_FACE('',(#3755),#2256,.F.);
#26344=ADVANCED_FACE('',(#3756),#2257,.F.);
#26345=ADVANCED_FACE('',(#3757),#2258,.F.);
#26346=ADVANCED_FACE('',(#3758),#2259,.F.);
#26347=ADVANCED_FACE('',(#3759),#2260,.F.);
#26348=ADVANCED_FACE('',(#3760),#2261,.F.);
#26349=ADVANCED_FACE('',(#3761),#2262,.F.);
#26350=ADVANCED_FACE('',(#3762),#2263,.F.);
#26351=ADVANCED_FACE('',(#3763),#2264,.F.);
#26352=ADVANCED_FACE('',(#3764),#2265,.F.);
#26353=ADVANCED_FACE('',(#3765),#2266,.F.);
#26354=ADVANCED_FACE('',(#3766),#2267,.F.);
#26355=ADVANCED_FACE('',(#3767),#2268,.F.);
#26356=ADVANCED_FACE('',(#3768),#2269,.F.);
#26357=ADVANCED_FACE('',(#3769),#2270,.F.);
#26358=ADVANCED_FACE('',(#3770),#2271,.F.);
#26359=ADVANCED_FACE('',(#3771),#2272,.F.);
#26360=ADVANCED_FACE('',(#3772),#2273,.F.);
#26361=ADVANCED_FACE('',(#3773),#2274,.F.);
#26362=ADVANCED_FACE('',(#3774),#2275,.F.);
#26363=ADVANCED_FACE('',(#3775),#2276,.F.);
#26364=ADVANCED_FACE('',(#3776),#2277,.F.);
#26365=ADVANCED_FACE('',(#3777),#2278,.F.);
#26366=ADVANCED_FACE('',(#3778),#2279,.F.);
#26367=ADVANCED_FACE('',(#3779),#2280,.F.);
#26368=ADVANCED_FACE('',(#3780),#2281,.F.);
#26369=ADVANCED_FACE('',(#3781),#2282,.F.);
#26370=ADVANCED_FACE('',(#3782),#2283,.F.);
#26371=ADVANCED_FACE('',(#3783),#2284,.F.);
#26372=ADVANCED_FACE('',(#3784),#2285,.F.);
#26373=ADVANCED_FACE('',(#3785),#2286,.F.);
#26374=ADVANCED_FACE('',(#3786),#2287,.F.);
#26375=ADVANCED_FACE('',(#3787),#2288,.F.);
#26376=ADVANCED_FACE('',(#3788),#2289,.F.);
#26377=ADVANCED_FACE('',(#3789),#2290,.F.);
#26378=ADVANCED_FACE('',(#3790),#2291,.F.);
#26379=ADVANCED_FACE('',(#3791),#2292,.F.);
#26380=ADVANCED_FACE('',(#3792),#2293,.F.);
#26381=ADVANCED_FACE('',(#3793),#2294,.F.);
#26382=ADVANCED_FACE('',(#3794),#2295,.F.);
#26383=ADVANCED_FACE('',(#3795),#2296,.F.);
#26384=ADVANCED_FACE('',(#3796),#2297,.F.);
#26385=ADVANCED_FACE('',(#3797),#2298,.F.);
#26386=ADVANCED_FACE('',(#3798),#2299,.F.);
#26387=ADVANCED_FACE('',(#3799),#2300,.F.);
#26388=ADVANCED_FACE('',(#3800),#2301,.F.);
#26389=ADVANCED_FACE('',(#3801),#2302,.F.);
#26390=ADVANCED_FACE('',(#3802),#2303,.F.);
#26391=ADVANCED_FACE('',(#3803),#2304,.F.);
#26392=ADVANCED_FACE('',(#3804),#2305,.F.);
#26393=ADVANCED_FACE('',(#3805),#2306,.F.);
#26394=ADVANCED_FACE('',(#3806),#2307,.F.);
#26395=ADVANCED_FACE('',(#3807),#2308,.F.);
#26396=ADVANCED_FACE('',(#3808),#2309,.F.);
#26397=ADVANCED_FACE('',(#3809),#2310,.F.);
#26398=ADVANCED_FACE('',(#3810),#2311,.F.);
#26399=ADVANCED_FACE('',(#3811),#2312,.F.);
#26400=ADVANCED_FACE('',(#3812),#2313,.F.);
#26401=ADVANCED_FACE('',(#3813),#2314,.F.);
#26402=ADVANCED_FACE('',(#3814),#2315,.F.);
#26403=ADVANCED_FACE('',(#3815),#2316,.F.);
#26404=ADVANCED_FACE('',(#3816),#2317,.F.);
#26405=ADVANCED_FACE('',(#3817),#2318,.F.);
#26406=ADVANCED_FACE('',(#3818),#2319,.F.);
#26407=ADVANCED_FACE('',(#3819),#2320,.F.);
#26408=ADVANCED_FACE('',(#3820),#2321,.F.);
#26409=ADVANCED_FACE('',(#3821),#2322,.F.);
#26410=ADVANCED_FACE('',(#3822),#2323,.F.);
#26411=ADVANCED_FACE('',(#3823),#2324,.F.);
#26412=ADVANCED_FACE('',(#3824),#2325,.F.);
#26413=ADVANCED_FACE('',(#3825),#2326,.F.);
#26414=ADVANCED_FACE('',(#3826),#2327,.F.);
#26415=ADVANCED_FACE('',(#3827),#2328,.F.);
#26416=ADVANCED_FACE('',(#3828),#2329,.F.);
#26417=ADVANCED_FACE('',(#3829),#2330,.F.);
#26418=ADVANCED_FACE('',(#3830),#2331,.F.);
#26419=ADVANCED_FACE('',(#3831),#2332,.F.);
#26420=ADVANCED_FACE('',(#3832),#2333,.F.);
#26421=ADVANCED_FACE('',(#3833),#2334,.F.);
#26422=ADVANCED_FACE('',(#3834),#2335,.F.);
#26423=ADVANCED_FACE('',(#3835),#2336,.F.);
#26424=ADVANCED_FACE('',(#3836),#2337,.F.);
#26425=ADVANCED_FACE('',(#3837),#2338,.F.);
#26426=ADVANCED_FACE('',(#3838),#2339,.F.);
#26427=ADVANCED_FACE('',(#3839),#2340,.F.);
#26428=ADVANCED_FACE('',(#3840),#2341,.F.);
#26429=ADVANCED_FACE('',(#3841),#2342,.F.);
#26430=ADVANCED_FACE('',(#3842),#2343,.F.);
#26431=ADVANCED_FACE('',(#3843),#2344,.F.);
#26432=ADVANCED_FACE('',(#3844),#2345,.F.);
#26433=ADVANCED_FACE('',(#3845),#2346,.F.);
#26434=ADVANCED_FACE('',(#3846),#2347,.F.);
#26435=ADVANCED_FACE('',(#3847),#2348,.F.);
#26436=ADVANCED_FACE('',(#3848),#2349,.F.);
#26437=ADVANCED_FACE('',(#3849),#2350,.F.);
#26438=ADVANCED_FACE('',(#3850),#2351,.F.);
#26439=ADVANCED_FACE('',(#3851),#2352,.F.);
#26440=ADVANCED_FACE('',(#3852),#2353,.F.);
#26441=ADVANCED_FACE('',(#3853),#2354,.F.);
#26442=ADVANCED_FACE('',(#3854),#2355,.F.);
#26443=ADVANCED_FACE('',(#3855),#2356,.F.);
#26444=ADVANCED_FACE('',(#3856),#2357,.F.);
#26445=ADVANCED_FACE('',(#3857),#2358,.F.);
#26446=ADVANCED_FACE('',(#3858),#2359,.F.);
#26447=ADVANCED_FACE('',(#3859),#2360,.F.);
#26448=ADVANCED_FACE('',(#3860),#2361,.T.);
#26449=ADVANCED_FACE('',(#3861),#25105,.T.);
#26450=ADVANCED_FACE('',(#3862),#25106,.T.);
#26451=ADVANCED_FACE('',(#3863),#1510,.T.);
#26452=ADVANCED_FACE('',(#3864),#25107,.T.);
#26453=ADVANCED_FACE('',(#3865,#1653),#2362,.T.);
#26454=ADVANCED_FACE('',(#3866),#1511,.T.);
#26455=ADVANCED_FACE('',(#3867),#1512,.T.);
#26456=ADVANCED_FACE('',(#3868),#1513,.T.);
#26457=ADVANCED_FACE('',(#3869),#1514,.T.);
#26458=ADVANCED_FACE('',(#3870),#1515,.T.);
#26459=ADVANCED_FACE('',(#3871),#1516,.T.);
#26460=ADVANCED_FACE('',(#3872),#1517,.T.);
#26461=ADVANCED_FACE('',(#3873),#1518,.T.);
#26462=ADVANCED_FACE('',(#3874),#1519,.T.);
#26463=ADVANCED_FACE('',(#3875),#1520,.T.);
#26464=ADVANCED_FACE('',(#3876),#1521,.T.);
#26465=ADVANCED_FACE('',(#3877),#1522,.T.);
#26466=ADVANCED_FACE('',(#3878),#1523,.T.);
#26467=ADVANCED_FACE('',(#3879),#1524,.T.);
#26468=ADVANCED_FACE('',(#3880),#1525,.T.);
#26469=ADVANCED_FACE('',(#3881),#1526,.T.);
#26470=ADVANCED_FACE('',(#3882),#1527,.T.);
#26471=ADVANCED_FACE('',(#3883),#1528,.T.);
#26472=ADVANCED_FACE('',(#3884),#1529,.T.);
#26473=ADVANCED_FACE('',(#3885),#1530,.T.);
#26474=ADVANCED_FACE('',(#3886),#1531,.T.);
#26475=ADVANCED_FACE('',(#3887),#1532,.T.);
#26476=ADVANCED_FACE('',(#3888),#1533,.T.);
#26477=ADVANCED_FACE('',(#3889),#1534,.T.);
#26478=ADVANCED_FACE('',(#3890),#1535,.T.);
#26479=ADVANCED_FACE('',(#3891),#1536,.T.);
#26480=ADVANCED_FACE('',(#3892),#1537,.T.);
#26481=ADVANCED_FACE('',(#3893),#1538,.T.);
#26482=ADVANCED_FACE('',(#3894),#1539,.T.);
#26483=ADVANCED_FACE('',(#3895),#1540,.T.);
#26484=ADVANCED_FACE('',(#3896),#1541,.T.);
#26485=ADVANCED_FACE('',(#3897),#1542,.T.);
#26486=ADVANCED_FACE('',(#3898),#1543,.T.);
#26487=ADVANCED_FACE('',(#3899),#1544,.T.);
#26488=ADVANCED_FACE('',(#3900),#1545,.T.);
#26489=ADVANCED_FACE('',(#3901),#1546,.T.);
#26490=ADVANCED_FACE('',(#3902),#1547,.T.);
#26491=ADVANCED_FACE('',(#3903),#1548,.T.);
#26492=ADVANCED_FACE('',(#3904),#1549,.T.);
#26493=ADVANCED_FACE('',(#3905),#2363,.F.);
#26494=ADVANCED_FACE('',(#3906),#172,.F.);
#26495=ADVANCED_FACE('',(#3907),#2364,.T.);
#26496=ADVANCED_FACE('',(#3908),#1550,.T.);
#26497=ADVANCED_FACE('',(#3909),#173,.F.);
#26498=ADVANCED_FACE('',(#3910),#1088,.F.);
#26499=ADVANCED_FACE('',(#3911),#1551,.T.);
#26500=ADVANCED_FACE('',(#3912,#1654),#2365,.T.);
#26501=ADVANCED_FACE('',(#3913),#2366,.F.);
#26502=ADVANCED_FACE('',(#3914),#2367,.F.);
#26503=ADVANCED_FACE('',(#3915),#2368,.F.);
#26504=ADVANCED_FACE('',(#3916),#2369,.F.);
#26505=ADVANCED_FACE('',(#3917),#2370,.F.);
#26506=ADVANCED_FACE('',(#3918),#2371,.F.);
#26507=ADVANCED_FACE('',(#3919),#25108,.F.);
#26508=ADVANCED_FACE('',(#3920),#2372,.F.);
#26509=ADVANCED_FACE('',(#3921),#2373,.F.);
#26510=ADVANCED_FACE('',(#3922),#2374,.F.);
#26511=ADVANCED_FACE('',(#3923),#2375,.F.);
#26512=ADVANCED_FACE('',(#3924),#2376,.F.);
#26513=ADVANCED_FACE('',(#3925),#2377,.F.);
#26514=ADVANCED_FACE('',(#3926),#2378,.F.);
#26515=ADVANCED_FACE('',(#3927),#2379,.F.);
#26516=ADVANCED_FACE('',(#3928),#2380,.F.);
#26517=ADVANCED_FACE('',(#3929),#2381,.F.);
#26518=ADVANCED_FACE('',(#3930),#2382,.F.);
#26519=ADVANCED_FACE('',(#3931),#2383,.F.);
#26520=ADVANCED_FACE('',(#3932),#2384,.F.);
#26521=ADVANCED_FACE('',(#3933),#2385,.F.);
#26522=ADVANCED_FACE('',(#3934),#2386,.F.);
#26523=ADVANCED_FACE('',(#3935),#2387,.F.);
#26524=ADVANCED_FACE('',(#3936),#2388,.F.);
#26525=ADVANCED_FACE('',(#3937),#2389,.F.);
#26526=ADVANCED_FACE('',(#3938),#2390,.F.);
#26527=ADVANCED_FACE('',(#3939),#2391,.F.);
#26528=ADVANCED_FACE('',(#3940),#2392,.F.);
#26529=ADVANCED_FACE('',(#3941),#2393,.F.);
#26530=ADVANCED_FACE('',(#3942),#2394,.F.);
#26531=ADVANCED_FACE('',(#3943),#2395,.F.);
#26532=ADVANCED_FACE('',(#3944),#2396,.F.);
#26533=ADVANCED_FACE('',(#3945),#2397,.F.);
#26534=ADVANCED_FACE('',(#3946),#2398,.F.);
#26535=ADVANCED_FACE('',(#3947),#2399,.F.);
#26536=ADVANCED_FACE('',(#3948),#2400,.F.);
#26537=ADVANCED_FACE('',(#3949),#2401,.F.);
#26538=ADVANCED_FACE('',(#3950),#2402,.F.);
#26539=ADVANCED_FACE('',(#3951),#2403,.F.);
#26540=ADVANCED_FACE('',(#3952),#2404,.F.);
#26541=ADVANCED_FACE('',(#3953),#2405,.F.);
#26542=ADVANCED_FACE('',(#3954),#2406,.F.);
#26543=ADVANCED_FACE('',(#3955),#2407,.F.);
#26544=ADVANCED_FACE('',(#3956),#2408,.F.);
#26545=ADVANCED_FACE('',(#3957),#2409,.F.);
#26546=ADVANCED_FACE('',(#3958),#2410,.F.);
#26547=ADVANCED_FACE('',(#3959),#2411,.F.);
#26548=ADVANCED_FACE('',(#3960),#2412,.F.);
#26549=ADVANCED_FACE('',(#3961),#2413,.F.);
#26550=ADVANCED_FACE('',(#3962),#2414,.F.);
#26551=ADVANCED_FACE('',(#3963),#2415,.F.);
#26552=ADVANCED_FACE('',(#3964),#2416,.F.);
#26553=ADVANCED_FACE('',(#3965),#2417,.F.);
#26554=ADVANCED_FACE('',(#3966),#2418,.F.);
#26555=ADVANCED_FACE('',(#3967),#2419,.F.);
#26556=ADVANCED_FACE('',(#3968),#2420,.F.);
#26557=ADVANCED_FACE('',(#3969),#2421,.F.);
#26558=ADVANCED_FACE('',(#3970),#2422,.F.);
#26559=ADVANCED_FACE('',(#3971),#2423,.F.);
#26560=ADVANCED_FACE('',(#3972),#2424,.F.);
#26561=ADVANCED_FACE('',(#3973),#2425,.F.);
#26562=ADVANCED_FACE('',(#3974),#2426,.F.);
#26563=ADVANCED_FACE('',(#3975),#2427,.F.);
#26564=ADVANCED_FACE('',(#3976),#2428,.F.);
#26565=ADVANCED_FACE('',(#3977),#2429,.F.);
#26566=ADVANCED_FACE('',(#3978),#2430,.F.);
#26567=ADVANCED_FACE('',(#3979),#2431,.F.);
#26568=ADVANCED_FACE('',(#3980),#2432,.F.);
#26569=ADVANCED_FACE('',(#3981),#2433,.F.);
#26570=ADVANCED_FACE('',(#3982),#2434,.F.);
#26571=ADVANCED_FACE('',(#3983),#2435,.F.);
#26572=ADVANCED_FACE('',(#3984),#2436,.F.);
#26573=ADVANCED_FACE('',(#3985),#2437,.F.);
#26574=ADVANCED_FACE('',(#3986),#2438,.F.);
#26575=ADVANCED_FACE('',(#3987),#2439,.F.);
#26576=ADVANCED_FACE('',(#3988),#2440,.F.);
#26577=ADVANCED_FACE('',(#3989),#2441,.F.);
#26578=ADVANCED_FACE('',(#3990),#2442,.F.);
#26579=ADVANCED_FACE('',(#3991),#2443,.F.);
#26580=ADVANCED_FACE('',(#3992),#2444,.F.);
#26581=ADVANCED_FACE('',(#3993),#2445,.F.);
#26582=ADVANCED_FACE('',(#3994),#2446,.F.);
#26583=ADVANCED_FACE('',(#3995),#2447,.F.);
#26584=ADVANCED_FACE('',(#3996),#2448,.F.);
#26585=ADVANCED_FACE('',(#3997),#2449,.F.);
#26586=ADVANCED_FACE('',(#3998),#2450,.F.);
#26587=ADVANCED_FACE('',(#3999),#2451,.F.);
#26588=ADVANCED_FACE('',(#4000),#2452,.F.);
#26589=ADVANCED_FACE('',(#4001),#2453,.F.);
#26590=ADVANCED_FACE('',(#4002),#2454,.F.);
#26591=ADVANCED_FACE('',(#4003),#2455,.F.);
#26592=ADVANCED_FACE('',(#4004),#2456,.F.);
#26593=ADVANCED_FACE('',(#4005),#2457,.F.);
#26594=ADVANCED_FACE('',(#4006),#2458,.F.);
#26595=ADVANCED_FACE('',(#4007),#2459,.F.);
#26596=ADVANCED_FACE('',(#4008),#2460,.F.);
#26597=ADVANCED_FACE('',(#4009),#2461,.F.);
#26598=ADVANCED_FACE('',(#4010),#2462,.F.);
#26599=ADVANCED_FACE('',(#4011),#2463,.F.);
#26600=ADVANCED_FACE('',(#4012),#2464,.F.);
#26601=ADVANCED_FACE('',(#4013),#2465,.F.);
#26602=ADVANCED_FACE('',(#4014),#2466,.F.);
#26603=ADVANCED_FACE('',(#4015),#2467,.F.);
#26604=ADVANCED_FACE('',(#4016),#2468,.F.);
#26605=ADVANCED_FACE('',(#4017),#2469,.F.);
#26606=ADVANCED_FACE('',(#4018),#2470,.F.);
#26607=ADVANCED_FACE('',(#4019),#2471,.F.);
#26608=ADVANCED_FACE('',(#4020),#2472,.F.);
#26609=ADVANCED_FACE('',(#4021),#2473,.F.);
#26610=ADVANCED_FACE('',(#4022),#2474,.F.);
#26611=ADVANCED_FACE('',(#4023),#2475,.F.);
#26612=ADVANCED_FACE('',(#4024),#2476,.F.);
#26613=ADVANCED_FACE('',(#4025),#2477,.F.);
#26614=ADVANCED_FACE('',(#4026),#2478,.F.);
#26615=ADVANCED_FACE('',(#4027),#2479,.F.);
#26616=ADVANCED_FACE('',(#4028),#2480,.F.);
#26617=ADVANCED_FACE('',(#4029),#2481,.F.);
#26618=ADVANCED_FACE('',(#4030),#2482,.F.);
#26619=ADVANCED_FACE('',(#4031),#2483,.F.);
#26620=ADVANCED_FACE('',(#4032),#2484,.F.);
#26621=ADVANCED_FACE('',(#4033),#2485,.F.);
#26622=ADVANCED_FACE('',(#4034),#2486,.F.);
#26623=ADVANCED_FACE('',(#4035),#2487,.F.);
#26624=ADVANCED_FACE('',(#4036),#2488,.F.);
#26625=ADVANCED_FACE('',(#4037),#2489,.F.);
#26626=ADVANCED_FACE('',(#4038),#2490,.F.);
#26627=ADVANCED_FACE('',(#4039),#2491,.F.);
#26628=ADVANCED_FACE('',(#4040),#2492,.F.);
#26629=ADVANCED_FACE('',(#4041),#2493,.F.);
#26630=ADVANCED_FACE('',(#4042),#2494,.F.);
#26631=ADVANCED_FACE('',(#4043),#2495,.F.);
#26632=ADVANCED_FACE('',(#4044),#2496,.F.);
#26633=ADVANCED_FACE('',(#4045),#2497,.F.);
#26634=ADVANCED_FACE('',(#4046),#2498,.F.);
#26635=ADVANCED_FACE('',(#4047),#2499,.F.);
#26636=ADVANCED_FACE('',(#4048),#2500,.F.);
#26637=ADVANCED_FACE('',(#4049),#2501,.F.);
#26638=ADVANCED_FACE('',(#4050),#2502,.F.);
#26639=ADVANCED_FACE('',(#4051),#2503,.F.);
#26640=ADVANCED_FACE('',(#4052),#2504,.F.);
#26641=ADVANCED_FACE('',(#4053),#2505,.F.);
#26642=ADVANCED_FACE('',(#4054),#2506,.F.);
#26643=ADVANCED_FACE('',(#4055),#2507,.F.);
#26644=ADVANCED_FACE('',(#4056),#2508,.F.);
#26645=ADVANCED_FACE('',(#4057),#2509,.F.);
#26646=ADVANCED_FACE('',(#4058),#2510,.F.);
#26647=ADVANCED_FACE('',(#4059),#2511,.F.);
#26648=ADVANCED_FACE('',(#4060),#2512,.F.);
#26649=ADVANCED_FACE('',(#4061),#2513,.F.);
#26650=ADVANCED_FACE('',(#4062),#2514,.F.);
#26651=ADVANCED_FACE('',(#4063),#2515,.F.);
#26652=ADVANCED_FACE('',(#4064),#2516,.F.);
#26653=ADVANCED_FACE('',(#4065),#2517,.F.);
#26654=ADVANCED_FACE('',(#4066),#2518,.F.);
#26655=ADVANCED_FACE('',(#4067),#2519,.F.);
#26656=ADVANCED_FACE('',(#4068),#2520,.F.);
#26657=ADVANCED_FACE('',(#4069),#2521,.F.);
#26658=ADVANCED_FACE('',(#4070),#2522,.T.);
#26659=ADVANCED_FACE('',(#4071),#25109,.T.);
#26660=ADVANCED_FACE('',(#4072),#25110,.T.);
#26661=ADVANCED_FACE('',(#4073),#1552,.T.);
#26662=ADVANCED_FACE('',(#4074),#25111,.T.);
#26663=ADVANCED_FACE('',(#4075,#1655),#2523,.T.);
#26664=CLOSED_SHELL('',(#25112,#25113,#25114,#25115,#25116,#25117,#25118,
#25119,#25120,#25121,#25122,#25123,#25124,#25125,#25126,#25127,#25128,#25129,
#25130,#25131,#25132,#25133,#25134,#25135,#25136,#25137,#25138,#25139,#25140,
#25141,#25142,#25143,#25144,#25145,#25146,#25147,#25148,#25149,#25150,#25151,
#25152,#25153,#25154,#25155,#25156,#25157,#25158,#25159,#25160,#25161,#25162,
#25163,#25164,#25165,#25166,#25167,#25168,#25169,#25170,#25171,#25172,#25173,
#25174,#25175,#25176,#25177,#25178,#25179,#25180,#25181,#25182,#25183,#25184,
#25185,#25186,#25187,#25188,#25189,#25190,#25191,#25192,#25193,#25194,#25195,
#25196,#25197,#25198,#25199,#25200,#25201,#25202,#25203,#25204,#25205,#25206,
#25207,#25208,#25209,#25210,#25211,#25212,#25213,#25214,#25215,#25216,#25217,
#25218,#25219,#25220,#25221,#25222,#25223,#25224,#25225,#25226,#25227,#25228,
#25229,#25230,#25231,#25232,#25233,#25234,#25235,#25236,#25237,#25238,#25239,
#25240,#25241,#25242,#25243,#25244,#25245,#25246,#25247,#25248,#25249,#25250,
#25251,#25252,#25253,#25254,#25255,#25256,#25257));
#26665=CLOSED_SHELL('',(#25258,#25259,#25260,#25261,#25262,#25263,#25264,
#25265,#25266,#25267,#25268,#25269,#25270,#25271,#25272,#25273,#25274,#25275,
#25276,#25277,#25278,#25279,#25280,#25281,#25282,#25283,#25284,#25285,#25286,
#25287,#25288,#25289,#25290,#25291,#25292,#25293,#25294,#25295,#25296,#25297,
#25298,#25299,#25300,#25301,#25302,#25303,#25304,#25305,#25306,#25307,#25308,
#25309,#25310,#25311,#25312,#25313,#25314,#25315,#25316,#25317,#25318,#25319,
#25320,#25321,#25322,#25323,#25324,#25325,#25326,#25327,#25328,#25329,#25330,
#25331,#25332,#25333,#25334,#25335,#25336,#25337,#25338,#25339,#25340,#25341,
#25342,#25343,#25344,#25345,#25346,#25347,#25348,#25349,#25350,#25351,#25352,
#25353,#25354,#25355,#25356,#25357,#25358,#25359,#25360,#25361,#25362,#25363,
#25364,#25365,#25366,#25367,#25368,#25369,#25370,#25371,#25372,#25373,#25374,
#25375,#25376,#25377,#25378,#25379,#25380,#25381,#25382,#25383,#25384,#25385,
#25386,#25387,#25388,#25389,#25390,#25391,#25392,#25393,#25394,#25395,#25396,
#25397,#25398,#25399,#25400,#25401,#25402,#25403,#25404,#25405,#25406,#25407,
#25408,#25409,#25410,#25411,#25412,#25413,#25414,#25415,#25416,#25417,#25418,
#25419,#25420));
#26666=CLOSED_SHELL('',(#25421,#25422,#25423,#25424,#25425,#25426,#25427,
#25428,#25429,#25430,#25431,#25432,#25433,#25434,#25435,#25436,#25437,#25438,
#25439,#25440,#25441,#25442,#25443,#25444,#25445,#25446,#25447,#25448,#25449,
#25450,#25451,#25452,#25453,#25454,#25455,#25456,#25457,#25458,#25459,#25460,
#25461,#25462,#25463,#25464,#25465,#25466,#25467,#25468,#25469,#25470,#25471,
#25472,#25473,#25474,#25475,#25476,#25477,#25478,#25479,#25480,#25481,#25482,
#25483,#25484,#25485,#25486,#25487,#25488,#25489,#25490,#25491,#25492,#25493,
#25494,#25495,#25496,#25497,#25498,#25499,#25500,#25501,#25502,#25503,#25504,
#25505,#25506,#25507,#25508,#25509,#25510,#25511,#25512,#25513,#25514,#25515,
#25516,#25517,#25518,#25519,#25520,#25521,#25522,#25523,#25524,#25525,#25526,
#25527,#25528,#25529,#25530,#25531,#25532,#25533,#25534,#25535,#25536,#25537,
#25538,#25539,#25540,#25541,#25542));
#26667=CLOSED_SHELL('',(#25543,#25544,#25545,#25546,#25547,#25548));
#26668=CLOSED_SHELL('',(#25549,#25550,#25551,#25552,#25553,#25554,#25555,
#25556,#25557,#25558,#25559,#25560,#25561,#25562,#25563,#25564,#25565,#25566,
#25567,#25568,#25569,#25570,#25571,#25572,#25573,#25574,#25575,#25576,#25577,
#25578,#25579,#25580,#25581,#25582,#25583,#25584,#25585,#25586,#25587,#25588,
#25589,#25590,#25591,#25592,#25593,#25594,#25595,#25596,#25597,#25598,#25599,
#25600,#25601,#25602,#25603,#25604,#25605,#25606,#25607,#25608,#25609,#25610,
#25611,#25612,#25613,#25614,#25615,#25616,#25617,#25618,#25619,#25620,#25621,
#25622,#25623,#25624,#25625,#25626,#25627,#25628,#25629,#25630,#25631,#25632,
#25633,#25634,#25635,#25636,#25637,#25638,#25639,#25640,#25641,#25642,#25643,
#25644,#25645,#25646,#25647,#25648,#25649,#25650,#25651,#25652,#25653,#25654,
#25655,#25656,#25657,#25658));
#26669=CLOSED_SHELL('',(#25659,#25660,#25661,#25662,#25663,#25664,#25665,
#25666,#25667,#25668,#25669,#25670,#25671,#25672));
#26670=CLOSED_SHELL('',(#25673,#25674,#25675,#25676,#25677,#25678,#25679,
#25680,#25681,#25682,#25683,#25684,#25685,#25686,#25687,#25688,#25689,#25690,
#25691,#25692,#25693,#25694,#25695,#25696,#25697,#25698,#25699,#25700));
#26671=CLOSED_SHELL('',(#25701,#25702,#25703,#25704,#25705,#25706,#25707,
#25708,#25709,#25710,#25711,#25712,#25713,#25714,#25715,#25716,#25717,#25718,
#25719,#25720,#25721,#25722,#25723));
#26672=CLOSED_SHELL('',(#25724,#25725,#25726,#25727,#25728,#25729,#25730,
#25731,#25732,#25733,#25734,#25735,#25736,#25737,#25738,#25739,#25740,#25741,
#25742,#25743,#25744,#25745,#25746,#25747,#25748,#25749,#25750,#25751,#25752,
#25753,#25754,#25755,#25756,#25757,#25758,#25759,#25760,#25761,#25762,#25763,
#25764,#25765,#25766,#25767,#25768,#25769,#25770,#25771,#25772,#25773,#25774,
#25775,#25776,#25777,#25778,#25779,#25780,#25781,#25782,#25783,#25784,#25785,
#25786,#25787,#25788,#25789,#25790,#25791,#25792,#25793,#25794,#25795,#25796,
#25797,#25798,#25799,#25800,#25801,#25802,#25803,#25804,#25805,#25806,#25807,
#25808,#25809,#25810,#25811,#25812,#25813,#25814,#25815,#25816,#25817,#25818,
#25819,#25820,#25821,#25822,#25823,#25824,#25825,#25826,#25827,#25828,#25829,
#25830,#25831,#25832,#25833,#25834,#25835,#25836,#25837,#25838,#25839,#25840,
#25841,#25842,#25843,#25844,#25845,#25846,#25847,#25848,#25849,#25850,#25851,
#25852,#25853,#25854,#25855,#25856,#25857,#25858,#25859,#25860,#25861,#25862,
#25863,#25864,#25865,#25866,#25867,#25868,#25869,#25870,#25871,#25872,#25873,
#25874,#25875,#25876,#25877,#25878,#25879,#25880,#25881,#25882,#25883,#25884,
#25885,#25886,#25887,#25888,#25889,#25890,#25891,#25892,#25893,#25894,#25895,
#25896,#25897,#25898,#25899,#25900,#25901,#25902,#25903,#25904,#25905,#25906,
#25907,#25908,#25909,#25910,#25911,#25912,#25913,#25914,#25915,#25916,#25917,
#25918,#25919,#25920,#25921,#25922,#25923,#25924,#25925));
#26673=CLOSED_SHELL('',(#25926,#25927,#25928,#25929,#25930,#25931,#25932,
#25933,#25934,#25935,#25936,#25937,#25938,#25939));
#26674=CLOSED_SHELL('',(#25940,#25941,#25942,#25943,#25944,#25945,#25946,
#25947,#25948,#25949,#25950,#25951,#25952,#25953,#25954,#25955,#25956,#25957,
#25958,#25959,#25960,#25961,#25962,#25963,#25964,#25965,#25966,#25967,#25968,
#25969,#25970,#25971,#25972,#25973));
#26675=CLOSED_SHELL('',(#25974,#25975,#25976,#25977));
#26676=CLOSED_SHELL('',(#25978,#25979,#25980,#25981,#25982,#25983,#25984,
#25985,#25986,#25987,#25988,#25989,#25990,#25991,#25992,#25993,#25994,#25995,
#25996,#25997,#25998,#25999,#26000,#26001,#26002,#26003,#26004,#26005,#26006,
#26007,#26008,#26009,#26010,#26011,#26012,#26013,#26014,#26015,#26016,#26017,
#26018,#26019,#26020,#26021,#26022,#26023));
#26677=CLOSED_SHELL('',(#26024,#26025,#26026,#26027,#26028,#26029,#26030,
#26031,#26032,#26033,#26034,#26035,#26036,#26037,#26038,#26039,#26040,#26041));
#26678=CLOSED_SHELL('',(#26042,#26043,#26044,#26045,#26046,#26047,#26048,
#26049,#26050,#26051,#26052,#26053,#26054,#26055,#26056,#26057,#26058,#26059,
#26060,#26061,#26062,#26063,#26064,#26065,#26066,#26067,#26068,#26069,#26070,
#26071,#26072,#26073,#26074,#26075,#26076,#26077,#26078,#26079,#26080,#26081,
#26082,#26083,#26084,#26085,#26086,#26087,#26088,#26089,#26090,#26091,#26092,
#26093,#26094,#26095,#26096,#26097,#26098,#26099));
#26679=CLOSED_SHELL('',(#26100,#26101,#26102,#26103,#26104,#26105,#26106,
#26107,#26108,#26109,#26110,#26111,#26112,#26113,#26114,#26115,#26116,#26117,
#26118,#26119,#26120,#26121,#26122,#26123,#26124,#26125,#26126,#26127,#26128,
#26129,#26130,#26131,#26132,#26133,#26134,#26135,#26136,#26137,#26138,#26139,
#26140,#26141,#26142,#26143,#26144,#26145,#26146,#26147,#26148,#26149,#26150,
#26151,#26152,#26153,#26154,#26155,#26156));
#26680=CLOSED_SHELL('',(#26157,#26158,#26159,#26160,#26161,#26162,#26163,
#26164,#26165,#26166,#26167,#26168,#26169,#26170,#26171,#26172,#26173));
#26681=CLOSED_SHELL('',(#26174,#26175,#26176,#26177,#26178,#26179,#26180,
#26181,#26182,#26183,#26184,#26185,#26186,#26187,#26188,#26189,#26190,#26191,
#26192,#26193,#26194,#26195,#26196,#26197,#26198,#26199,#26200,#26201,#26202,
#26203,#26204,#26205,#26206,#26207,#26208,#26209,#26210,#26211,#26212,#26213,
#26214,#26215,#26216,#26217,#26218,#26219,#26220,#26221,#26222,#26223,#26224,
#26225,#26226,#26227,#26228,#26229,#26230,#26231,#26232,#26233,#26234,#26235,
#26236));
#26682=CLOSED_SHELL('',(#26237,#26238,#26239,#26240,#26241,#26242,#26243,
#26244,#26245,#26246,#26247,#26248,#26249,#26250,#26251,#26252,#26253,#26254,
#26255,#26256,#26257,#26258,#26259,#26260,#26261,#26262,#26263,#26264,#26265,
#26266,#26267,#26268,#26269,#26270,#26271,#26272,#26273,#26274,#26275,#26276,
#26277,#26278,#26279,#26280,#26281,#26282,#26283,#26284,#26285,#26286,#26287,
#26288,#26289,#26290,#26291,#26292,#26293,#26294,#26295,#26296,#26297,#26298,
#26299,#26300,#26301,#26302,#26303,#26304,#26305,#26306,#26307,#26308,#26309,
#26310,#26311,#26312,#26313,#26314,#26315,#26316,#26317,#26318,#26319,#26320,
#26321,#26322,#26323,#26324,#26325,#26326,#26327,#26328,#26329,#26330,#26331,
#26332,#26333,#26334,#26335,#26336,#26337,#26338,#26339,#26340,#26341,#26342,
#26343,#26344,#26345,#26346,#26347,#26348,#26349,#26350,#26351,#26352,#26353,
#26354,#26355,#26356,#26357,#26358,#26359,#26360,#26361,#26362,#26363,#26364,
#26365,#26366,#26367,#26368,#26369,#26370,#26371,#26372,#26373,#26374,#26375,
#26376,#26377,#26378,#26379,#26380,#26381,#26382,#26383,#26384,#26385,#26386,
#26387,#26388,#26389,#26390,#26391,#26392,#26393,#26394,#26395,#26396,#26397,
#26398,#26399,#26400,#26401,#26402,#26403,#26404,#26405,#26406,#26407,#26408,
#26409,#26410,#26411,#26412,#26413,#26414,#26415,#26416,#26417,#26418,#26419,
#26420,#26421,#26422,#26423,#26424,#26425,#26426,#26427,#26428,#26429,#26430,
#26431,#26432,#26433,#26434,#26435,#26436,#26437,#26438,#26439,#26440,#26441,
#26442,#26443,#26444,#26445,#26446,#26447,#26448,#26449,#26450,#26451,#26452,
#26453));
#26683=CLOSED_SHELL('',(#26454,#26455,#26456,#26457,#26458,#26459,#26460,
#26461,#26462,#26463,#26464,#26465,#26466,#26467,#26468,#26469,#26470,#26471,
#26472,#26473,#26474,#26475,#26476,#26477,#26478,#26479,#26480,#26481,#26482,
#26483,#26484,#26485,#26486,#26487,#26488,#26489,#26490,#26491,#26492,#26493,
#26494,#26495,#26496,#26497,#26498,#26499,#26500,#26501,#26502,#26503,#26504,
#26505,#26506,#26507,#26508,#26509,#26510,#26511,#26512,#26513,#26514,#26515,
#26516,#26517,#26518,#26519,#26520,#26521,#26522,#26523,#26524,#26525,#26526,
#26527,#26528,#26529,#26530,#26531,#26532,#26533,#26534,#26535,#26536,#26537,
#26538,#26539,#26540,#26541,#26542,#26543,#26544,#26545,#26546,#26547,#26548,
#26549,#26550,#26551,#26552,#26553,#26554,#26555,#26556,#26557,#26558,#26559,
#26560,#26561,#26562,#26563,#26564,#26565,#26566,#26567,#26568,#26569,#26570,
#26571,#26572,#26573,#26574,#26575,#26576,#26577,#26578,#26579,#26580,#26581,
#26582,#26583,#26584,#26585,#26586,#26587,#26588,#26589,#26590,#26591,#26592,
#26593,#26594,#26595,#26596,#26597,#26598,#26599,#26600,#26601,#26602,#26603,
#26604,#26605,#26606,#26607,#26608,#26609,#26610,#26611,#26612,#26613,#26614,
#26615,#26616,#26617,#26618,#26619,#26620,#26621,#26622,#26623,#26624,#26625,
#26626,#26627,#26628,#26629,#26630,#26631,#26632,#26633,#26634,#26635,#26636,
#26637,#26638,#26639,#26640,#26641,#26642,#26643,#26644,#26645,#26646,#26647,
#26648,#26649,#26650,#26651,#26652,#26653,#26654,#26655,#26656,#26657,#26658,
#26659,#26660,#26661,#26662,#26663));
#26684=DERIVED_UNIT_ELEMENT(#26724,1.);
#26685=DERIVED_UNIT_ELEMENT(#76662,-3.);
#26686=DERIVED_UNIT_ELEMENT(#26724,1.);
#26687=DERIVED_UNIT_ELEMENT(#76662,-3.);
#26688=DERIVED_UNIT_ELEMENT(#26724,1.);
#26689=DERIVED_UNIT_ELEMENT(#76662,-3.);
#26690=DERIVED_UNIT_ELEMENT(#26724,1.);
#26691=DERIVED_UNIT_ELEMENT(#76662,-3.);
#26692=DERIVED_UNIT_ELEMENT(#26724,1.);
#26693=DERIVED_UNIT_ELEMENT(#76662,-3.);
#26694=DERIVED_UNIT_ELEMENT(#26724,1.);
#26695=DERIVED_UNIT_ELEMENT(#76662,-3.);
#26696=DERIVED_UNIT_ELEMENT(#26724,1.);
#26697=DERIVED_UNIT_ELEMENT(#76662,-3.);
#26698=DERIVED_UNIT_ELEMENT(#26724,1.);
#26699=DERIVED_UNIT_ELEMENT(#76662,-3.);
#26700=DERIVED_UNIT_ELEMENT(#26724,1.);
#26701=DERIVED_UNIT_ELEMENT(#76662,-3.);
#26702=DERIVED_UNIT_ELEMENT(#26724,1.);
#26703=DERIVED_UNIT_ELEMENT(#76662,-3.);
#26704=DERIVED_UNIT_ELEMENT(#26724,1.);
#26705=DERIVED_UNIT_ELEMENT(#76662,-3.);
#26706=DERIVED_UNIT_ELEMENT(#26724,1.);
#26707=DERIVED_UNIT_ELEMENT(#76662,-3.);
#26708=DERIVED_UNIT_ELEMENT(#26724,1.);
#26709=DERIVED_UNIT_ELEMENT(#76662,-3.);
#26710=DERIVED_UNIT_ELEMENT(#26724,1.);
#26711=DERIVED_UNIT_ELEMENT(#76662,-3.);
#26712=DERIVED_UNIT_ELEMENT(#26724,1.);
#26713=DERIVED_UNIT_ELEMENT(#76662,-3.);
#26714=DERIVED_UNIT_ELEMENT(#26724,1.);
#26715=DERIVED_UNIT_ELEMENT(#76662,-3.);
#26716=DERIVED_UNIT_ELEMENT(#26724,1.);
#26717=DERIVED_UNIT_ELEMENT(#76662,-3.);
#26718=DERIVED_UNIT_ELEMENT(#26724,1.);
#26719=DERIVED_UNIT_ELEMENT(#76662,-3.);
#26720=DERIVED_UNIT_ELEMENT(#26724,1.);
#26721=DERIVED_UNIT_ELEMENT(#76662,-3.);
#26722=DERIVED_UNIT_ELEMENT(#26724,1.);
#26723=DERIVED_UNIT_ELEMENT(#76662,-3.);
#26724=(
MASS_UNIT()
NAMED_UNIT(*)
SI_UNIT(.KILO.,.GRAM.)
);
#26725=DERIVED_UNIT((#26684,#26685));
#26726=DERIVED_UNIT((#26686,#26687));
#26727=DERIVED_UNIT((#26688,#26689));
#26728=DERIVED_UNIT((#26690,#26691));
#26729=DERIVED_UNIT((#26692,#26693));
#26730=DERIVED_UNIT((#26694,#26695));
#26731=DERIVED_UNIT((#26696,#26697));
#26732=DERIVED_UNIT((#26698,#26699));
#26733=DERIVED_UNIT((#26700,#26701));
#26734=DERIVED_UNIT((#26702,#26703));
#26735=DERIVED_UNIT((#26704,#26705));
#26736=DERIVED_UNIT((#26706,#26707));
#26737=DERIVED_UNIT((#26708,#26709));
#26738=DERIVED_UNIT((#26710,#26711));
#26739=DERIVED_UNIT((#26712,#26713));
#26740=DERIVED_UNIT((#26714,#26715));
#26741=DERIVED_UNIT((#26716,#26717));
#26742=DERIVED_UNIT((#26718,#26719));
#26743=DERIVED_UNIT((#26720,#26721));
#26744=DERIVED_UNIT((#26722,#26723));
#26745=MEASURE_REPRESENTATION_ITEM('density measure',
POSITIVE_RATIO_MEASURE(7150.),#26725);
#26746=MEASURE_REPRESENTATION_ITEM('density measure',
POSITIVE_RATIO_MEASURE(7150.),#26726);
#26747=MEASURE_REPRESENTATION_ITEM('density measure',
POSITIVE_RATIO_MEASURE(7730.),#26727);
#26748=MEASURE_REPRESENTATION_ITEM('density measure',
POSITIVE_RATIO_MEASURE(7730.),#26728);
#26749=MEASURE_REPRESENTATION_ITEM('density measure',
POSITIVE_RATIO_MEASURE(7850.),#26729);
#26750=MEASURE_REPRESENTATION_ITEM('density measure',
POSITIVE_RATIO_MEASURE(8470.),#26730);
#26751=MEASURE_REPRESENTATION_ITEM('density measure',
POSITIVE_RATIO_MEASURE(7150.),#26731);
#26752=MEASURE_REPRESENTATION_ITEM('density measure',
POSITIVE_RATIO_MEASURE(7150.),#26732);
#26753=MEASURE_REPRESENTATION_ITEM('density measure',
POSITIVE_RATIO_MEASURE(7730.),#26733);
#26754=MEASURE_REPRESENTATION_ITEM('density measure',
POSITIVE_RATIO_MEASURE(7850.),#26734);
#26755=MEASURE_REPRESENTATION_ITEM('density measure',
POSITIVE_RATIO_MEASURE(7850.),#26735);
#26756=MEASURE_REPRESENTATION_ITEM('density measure',
POSITIVE_RATIO_MEASURE(8470.),#26736);
#26757=MEASURE_REPRESENTATION_ITEM('density measure',
POSITIVE_RATIO_MEASURE(7730.),#26737);
#26758=MEASURE_REPRESENTATION_ITEM('density measure',
POSITIVE_RATIO_MEASURE(7850.),#26738);
#26759=MEASURE_REPRESENTATION_ITEM('density measure',
POSITIVE_RATIO_MEASURE(7850.),#26739);
#26760=MEASURE_REPRESENTATION_ITEM('density measure',
POSITIVE_RATIO_MEASURE(7850.),#26740);
#26761=MEASURE_REPRESENTATION_ITEM('density measure',
POSITIVE_RATIO_MEASURE(7730.),#26741);
#26762=MEASURE_REPRESENTATION_ITEM('density measure',
POSITIVE_RATIO_MEASURE(7850.),#26742);
#26763=MEASURE_REPRESENTATION_ITEM('density measure',
POSITIVE_RATIO_MEASURE(7730.),#26743);
#26764=MEASURE_REPRESENTATION_ITEM('density measure',
POSITIVE_RATIO_MEASURE(7730.),#26744);
#26765=PROPERTY_DEFINITION_REPRESENTATION(#26865,#26805);
#26766=PROPERTY_DEFINITION_REPRESENTATION(#26866,#26806);
#26767=PROPERTY_DEFINITION_REPRESENTATION(#26867,#26807);
#26768=PROPERTY_DEFINITION_REPRESENTATION(#26868,#26808);
#26769=PROPERTY_DEFINITION_REPRESENTATION(#26869,#26809);
#26770=PROPERTY_DEFINITION_REPRESENTATION(#26870,#26810);
#26771=PROPERTY_DEFINITION_REPRESENTATION(#26871,#26811);
#26772=PROPERTY_DEFINITION_REPRESENTATION(#26872,#26812);
#26773=PROPERTY_DEFINITION_REPRESENTATION(#26873,#26813);
#26774=PROPERTY_DEFINITION_REPRESENTATION(#26874,#26814);
#26775=PROPERTY_DEFINITION_REPRESENTATION(#26875,#26815);
#26776=PROPERTY_DEFINITION_REPRESENTATION(#26876,#26816);
#26777=PROPERTY_DEFINITION_REPRESENTATION(#26877,#26817);
#26778=PROPERTY_DEFINITION_REPRESENTATION(#26878,#26818);
#26779=PROPERTY_DEFINITION_REPRESENTATION(#26879,#26819);
#26780=PROPERTY_DEFINITION_REPRESENTATION(#26880,#26820);
#26781=PROPERTY_DEFINITION_REPRESENTATION(#26881,#26821);
#26782=PROPERTY_DEFINITION_REPRESENTATION(#26882,#26822);
#26783=PROPERTY_DEFINITION_REPRESENTATION(#26883,#26823);
#26784=PROPERTY_DEFINITION_REPRESENTATION(#26884,#26824);
#26785=PROPERTY_DEFINITION_REPRESENTATION(#26885,#26825);
#26786=PROPERTY_DEFINITION_REPRESENTATION(#26886,#26826);
#26787=PROPERTY_DEFINITION_REPRESENTATION(#26887,#26827);
#26788=PROPERTY_DEFINITION_REPRESENTATION(#26888,#26828);
#26789=PROPERTY_DEFINITION_REPRESENTATION(#26889,#26829);
#26790=PROPERTY_DEFINITION_REPRESENTATION(#26890,#26830);
#26791=PROPERTY_DEFINITION_REPRESENTATION(#26891,#26831);
#26792=PROPERTY_DEFINITION_REPRESENTATION(#26892,#26832);
#26793=PROPERTY_DEFINITION_REPRESENTATION(#26893,#26833);
#26794=PROPERTY_DEFINITION_REPRESENTATION(#26894,#26834);
#26795=PROPERTY_DEFINITION_REPRESENTATION(#26895,#26835);
#26796=PROPERTY_DEFINITION_REPRESENTATION(#26896,#26836);
#26797=PROPERTY_DEFINITION_REPRESENTATION(#26897,#26837);
#26798=PROPERTY_DEFINITION_REPRESENTATION(#26898,#26838);
#26799=PROPERTY_DEFINITION_REPRESENTATION(#26899,#26839);
#26800=PROPERTY_DEFINITION_REPRESENTATION(#26900,#26840);
#26801=PROPERTY_DEFINITION_REPRESENTATION(#26901,#26841);
#26802=PROPERTY_DEFINITION_REPRESENTATION(#26902,#26842);
#26803=PROPERTY_DEFINITION_REPRESENTATION(#26903,#26843);
#26804=PROPERTY_DEFINITION_REPRESENTATION(#26904,#26844);
#26805=REPRESENTATION('material name',(#26845),#76640);
#26806=REPRESENTATION('density',(#26745),#76640);
#26807=REPRESENTATION('material name',(#26846),#76641);
#26808=REPRESENTATION('density',(#26746),#76641);
#26809=REPRESENTATION('material name',(#26847),#76642);
#26810=REPRESENTATION('density',(#26747),#76642);
#26811=REPRESENTATION('material name',(#26848),#76643);
#26812=REPRESENTATION('density',(#26748),#76643);
#26813=REPRESENTATION('material name',(#26849),#76644);
#26814=REPRESENTATION('density',(#26749),#76644);
#26815=REPRESENTATION('material name',(#26850),#76645);
#26816=REPRESENTATION('density',(#26750),#76645);
#26817=REPRESENTATION('material name',(#26851),#76646);
#26818=REPRESENTATION('density',(#26751),#76646);
#26819=REPRESENTATION('material name',(#26852),#76647);
#26820=REPRESENTATION('density',(#26752),#76647);
#26821=REPRESENTATION('material name',(#26853),#76648);
#26822=REPRESENTATION('density',(#26753),#76648);
#26823=REPRESENTATION('material name',(#26854),#76649);
#26824=REPRESENTATION('density',(#26754),#76649);
#26825=REPRESENTATION('material name',(#26855),#76650);
#26826=REPRESENTATION('density',(#26755),#76650);
#26827=REPRESENTATION('material name',(#26856),#76651);
#26828=REPRESENTATION('density',(#26756),#76651);
#26829=REPRESENTATION('material name',(#26857),#76652);
#26830=REPRESENTATION('density',(#26757),#76652);
#26831=REPRESENTATION('material name',(#26858),#76653);
#26832=REPRESENTATION('density',(#26758),#76653);
#26833=REPRESENTATION('material name',(#26859),#76654);
#26834=REPRESENTATION('density',(#26759),#76654);
#26835=REPRESENTATION('material name',(#26860),#76655);
#26836=REPRESENTATION('density',(#26760),#76655);
#26837=REPRESENTATION('material name',(#26861),#76656);
#26838=REPRESENTATION('density',(#26761),#76656);
#26839=REPRESENTATION('material name',(#26862),#76657);
#26840=REPRESENTATION('density',(#26762),#76657);
#26841=REPRESENTATION('material name',(#26863),#76658);
#26842=REPRESENTATION('density',(#26763),#76658);
#26843=REPRESENTATION('material name',(#26864),#76659);
#26844=REPRESENTATION('density',(#26764),#76659);
#26845=DESCRIPTIVE_REPRESENTATION_ITEM('Iron, Cast','Iron, Cast');
#26846=DESCRIPTIVE_REPRESENTATION_ITEM('Iron, Cast','Iron, Cast');
#26847=DESCRIPTIVE_REPRESENTATION_ITEM('Steel, Alloy','Steel, Alloy');
#26848=DESCRIPTIVE_REPRESENTATION_ITEM('Steel, Alloy','Steel, Alloy');
#26849=DESCRIPTIVE_REPRESENTATION_ITEM('Steel','Steel');
#26850=DESCRIPTIVE_REPRESENTATION_ITEM('Bronze','Bronze');
#26851=DESCRIPTIVE_REPRESENTATION_ITEM('Iron, Cast','Iron, Cast');
#26852=DESCRIPTIVE_REPRESENTATION_ITEM('Iron, Cast','Iron, Cast');
#26853=DESCRIPTIVE_REPRESENTATION_ITEM('Steel, Alloy','Steel, Alloy');
#26854=DESCRIPTIVE_REPRESENTATION_ITEM('Steel','Steel');
#26855=DESCRIPTIVE_REPRESENTATION_ITEM('Steel','Steel');
#26856=DESCRIPTIVE_REPRESENTATION_ITEM('Bronze','Bronze');
#26857=DESCRIPTIVE_REPRESENTATION_ITEM('Steel, Alloy','Steel, Alloy');
#26858=DESCRIPTIVE_REPRESENTATION_ITEM('Steel','Steel');
#26859=DESCRIPTIVE_REPRESENTATION_ITEM('Steel','Steel');
#26860=DESCRIPTIVE_REPRESENTATION_ITEM('Steel','Steel');
#26861=DESCRIPTIVE_REPRESENTATION_ITEM('Steel, Alloy','Steel, Alloy');
#26862=DESCRIPTIVE_REPRESENTATION_ITEM('Steel','Steel');
#26863=DESCRIPTIVE_REPRESENTATION_ITEM('Steel, Alloy','Steel, Alloy');
#26864=DESCRIPTIVE_REPRESENTATION_ITEM('Steel, Alloy','Steel, Alloy');
#26865=PROPERTY_DEFINITION('material property','material name',#76758);
#26866=PROPERTY_DEFINITION('material property','density of part',#76758);
#26867=PROPERTY_DEFINITION('material property','material name',#76759);
#26868=PROPERTY_DEFINITION('material property','density of part',#76759);
#26869=PROPERTY_DEFINITION('material property','material name',#76760);
#26870=PROPERTY_DEFINITION('material property','density of part',#76760);
#26871=PROPERTY_DEFINITION('material property','material name',#76761);
#26872=PROPERTY_DEFINITION('material property','density of part',#76761);
#26873=PROPERTY_DEFINITION('material property','material name',#76762);
#26874=PROPERTY_DEFINITION('material property','density of part',#76762);
#26875=PROPERTY_DEFINITION('material property','material name',#76763);
#26876=PROPERTY_DEFINITION('material property','density of part',#76763);
#26877=PROPERTY_DEFINITION('material property','material name',#76764);
#26878=PROPERTY_DEFINITION('material property','density of part',#76764);
#26879=PROPERTY_DEFINITION('material property','material name',#76765);
#26880=PROPERTY_DEFINITION('material property','density of part',#76765);
#26881=PROPERTY_DEFINITION('material property','material name',#76766);
#26882=PROPERTY_DEFINITION('material property','density of part',#76766);
#26883=PROPERTY_DEFINITION('material property','material name',#76767);
#26884=PROPERTY_DEFINITION('material property','density of part',#76767);
#26885=PROPERTY_DEFINITION('material property','material name',#76768);
#26886=PROPERTY_DEFINITION('material property','density of part',#76768);
#26887=PROPERTY_DEFINITION('material property','material name',#76769);
#26888=PROPERTY_DEFINITION('material property','density of part',#76769);
#26889=PROPERTY_DEFINITION('material property','material name',#76770);
#26890=PROPERTY_DEFINITION('material property','density of part',#76770);
#26891=PROPERTY_DEFINITION('material property','material name',#76771);
#26892=PROPERTY_DEFINITION('material property','density of part',#76771);
#26893=PROPERTY_DEFINITION('material property','material name',#76772);
#26894=PROPERTY_DEFINITION('material property','density of part',#76772);
#26895=PROPERTY_DEFINITION('material property','material name',#76773);
#26896=PROPERTY_DEFINITION('material property','density of part',#76773);
#26897=PROPERTY_DEFINITION('material property','material name',#76774);
#26898=PROPERTY_DEFINITION('material property','density of part',#76774);
#26899=PROPERTY_DEFINITION('material property','material name',#76775);
#26900=PROPERTY_DEFINITION('material property','density of part',#76775);
#26901=PROPERTY_DEFINITION('material property','material name',#76776);
#26902=PROPERTY_DEFINITION('material property','density of part',#76776);
#26903=PROPERTY_DEFINITION('material property','material name',#76777);
#26904=PROPERTY_DEFINITION('material property','density of part',#76777);
#26905=AXIS2_PLACEMENT_3D('',#36381,#29345,#29346);
#26906=AXIS2_PLACEMENT_3D('',#36382,#29347,#29348);
#26907=AXIS2_PLACEMENT_3D('',#36383,#29349,#29350);
#26908=AXIS2_PLACEMENT_3D('',#36388,#29352,#29353);
#26909=AXIS2_PLACEMENT_3D('',#36391,#29355,#29356);
#26910=AXIS2_PLACEMENT_3D('',#36392,#29357,#29358);
#26911=AXIS2_PLACEMENT_3D('',#36398,#29362,#29363);
#26912=AXIS2_PLACEMENT_3D('',#36402,#29365,#29366);
#26913=AXIS2_PLACEMENT_3D('',#36403,#29367,#29368);
#26914=AXIS2_PLACEMENT_3D('',#36404,#29369,#29370);
#26915=AXIS2_PLACEMENT_3D('',#36410,#29374,#29375);
#26916=AXIS2_PLACEMENT_3D('',#36414,#29377,#29378);
#26917=AXIS2_PLACEMENT_3D('',#36415,#29379,#29380);
#26918=AXIS2_PLACEMENT_3D('',#36416,#29381,#29382);
#26919=AXIS2_PLACEMENT_3D('',#36422,#29386,#29387);
#26920=AXIS2_PLACEMENT_3D('',#36426,#29389,#29390);
#26921=AXIS2_PLACEMENT_3D('',#36427,#29391,#29392);
#26922=AXIS2_PLACEMENT_3D('',#36428,#29393,#29394);
#26923=AXIS2_PLACEMENT_3D('',#36431,#29397,#29398);
#26924=AXIS2_PLACEMENT_3D('',#36437,#29402,#29403);
#26925=AXIS2_PLACEMENT_3D('',#36440,#29405,#29406);
#26926=AXIS2_PLACEMENT_3D('',#36441,#29407,#29408);
#26927=AXIS2_PLACEMENT_3D('',#36445,#29411,#29412);
#26928=AXIS2_PLACEMENT_3D('',#36448,#29414,#29415);
#26929=AXIS2_PLACEMENT_3D('',#36449,#29416,#29417);
#26930=AXIS2_PLACEMENT_3D('',#36452,#29418,#29419);
#26931=AXIS2_PLACEMENT_3D('',#36456,#29421,#29422);
#26932=AXIS2_PLACEMENT_3D('',#36460,#29424,#29425);
#26933=AXIS2_PLACEMENT_3D('',#36464,#29427,#29428);
#26934=AXIS2_PLACEMENT_3D('',#36466,#29430,#29431);
#26935=AXIS2_PLACEMENT_3D('',#36468,#29432,#29433);
#26936=AXIS2_PLACEMENT_3D('',#36471,#29435,#29436);
#26937=AXIS2_PLACEMENT_3D('',#36472,#29437,#29438);
#26938=AXIS2_PLACEMENT_3D('',#36475,#29439,#29440);
#26939=AXIS2_PLACEMENT_3D('',#36479,#29442,#29443);
#26940=AXIS2_PLACEMENT_3D('',#36483,#29445,#29446);
#26941=AXIS2_PLACEMENT_3D('',#36487,#29448,#29449);
#26942=AXIS2_PLACEMENT_3D('',#36490,#29451,#29452);
#26943=AXIS2_PLACEMENT_3D('',#36492,#29453,#29454);
#26944=AXIS2_PLACEMENT_3D('',#36494,#29455,#29456);
#26945=AXIS2_PLACEMENT_3D('',#36504,#29461,#29462);
#26946=AXIS2_PLACEMENT_3D('',#36505,#29463,#29464);
#26947=AXIS2_PLACEMENT_3D('',#36507,#29465,#29466);
#26948=AXIS2_PLACEMENT_3D('',#36509,#29468,#29469);
#26949=AXIS2_PLACEMENT_3D('',#36512,#29471,#29472);
#26950=AXIS2_PLACEMENT_3D('',#36513,#29473,#29474);
#26951=AXIS2_PLACEMENT_3D('',#36515,#29475,#29476);
#26952=AXIS2_PLACEMENT_3D('',#36517,#29478,#29479);
#26953=AXIS2_PLACEMENT_3D('',#36520,#29481,#29482);
#26954=AXIS2_PLACEMENT_3D('',#36521,#29483,#29484);
#26955=AXIS2_PLACEMENT_3D('',#36523,#29485,#29486);
#26956=AXIS2_PLACEMENT_3D('',#36525,#29488,#29489);
#26957=AXIS2_PLACEMENT_3D('',#36528,#29491,#29492);
#26958=AXIS2_PLACEMENT_3D('',#36529,#29493,#29494);
#26959=AXIS2_PLACEMENT_3D('',#36531,#29495,#29496);
#26960=AXIS2_PLACEMENT_3D('',#36533,#29498,#29499);
#26961=AXIS2_PLACEMENT_3D('',#36539,#29503,#29504);
#26962=AXIS2_PLACEMENT_3D('',#36545,#29508,#29509);
#26963=AXIS2_PLACEMENT_3D('',#36547,#29511,#29512);
#26964=AXIS2_PLACEMENT_3D('',#36549,#29514,#29515);
#26965=AXIS2_PLACEMENT_3D('',#36555,#29519,#29520);
#26966=AXIS2_PLACEMENT_3D('',#36559,#29523,#29524);
#26967=AXIS2_PLACEMENT_3D('',#36562,#29525,#29526);
#26968=AXIS2_PLACEMENT_3D('',#36569,#29531,#29532);
#26969=AXIS2_PLACEMENT_3D('',#36573,#29534,#29535);
#26970=AXIS2_PLACEMENT_3D('',#36574,#29536,#29537);
#26971=AXIS2_PLACEMENT_3D('',#36575,#29538,#29539);
#26972=AXIS2_PLACEMENT_3D('',#36581,#29543,#29544);
#26973=AXIS2_PLACEMENT_3D('',#36585,#29546,#29547);
#26974=AXIS2_PLACEMENT_3D('',#36586,#29548,#29549);
#26975=AXIS2_PLACEMENT_3D('',#36587,#29550,#29551);
#26976=AXIS2_PLACEMENT_3D('',#36590,#29552,#29553);
#26977=AXIS2_PLACEMENT_3D('',#36596,#29558,#29559);
#26978=AXIS2_PLACEMENT_3D('',#36599,#29561,#29562);
#26979=AXIS2_PLACEMENT_3D('',#36600,#29563,#29564);
#26980=AXIS2_PLACEMENT_3D('',#36604,#29567,#29568);
#26981=AXIS2_PLACEMENT_3D('',#36605,#29569,#29570);
#26982=AXIS2_PLACEMENT_3D('',#36606,#29571,#29572);
#26983=AXIS2_PLACEMENT_3D('',#36613,#29576,#29577);
#26984=AXIS2_PLACEMENT_3D('',#36614,#29578,#29579);
#26985=AXIS2_PLACEMENT_3D('',#36615,#29580,#29581);
#26986=AXIS2_PLACEMENT_3D('',#36618,#29583,#29584);
#26987=AXIS2_PLACEMENT_3D('',#36619,#29585,#29586);
#26988=AXIS2_PLACEMENT_3D('',#36623,#29589,#29590);
#26989=AXIS2_PLACEMENT_3D('',#36626,#29592,#29593);
#26990=AXIS2_PLACEMENT_3D('',#36627,#29594,#29595);
#26991=AXIS2_PLACEMENT_3D('',#36629,#29596,#29597);
#26992=AXIS2_PLACEMENT_3D('',#36630,#29598,#29599);
#26993=AXIS2_PLACEMENT_3D('',#36634,#29602,#29603);
#26994=AXIS2_PLACEMENT_3D('',#36638,#29605,#29606);
#26995=AXIS2_PLACEMENT_3D('',#36640,#29607,#29608);
#26996=AXIS2_PLACEMENT_3D('',#36641,#29609,#29610);
#26997=AXIS2_PLACEMENT_3D('',#36642,#29611,#29612);
#26998=AXIS2_PLACEMENT_3D('',#36653,#29618,#29619);
#26999=AXIS2_PLACEMENT_3D('',#36659,#29623,#29624);
#27000=AXIS2_PLACEMENT_3D('',#36667,#29629,#29630);
#27001=AXIS2_PLACEMENT_3D('',#36677,#29636,#29637);
#27002=AXIS2_PLACEMENT_3D('',#36685,#29642,#29643);
#27003=AXIS2_PLACEMENT_3D('',#36693,#29648,#29649);
#27004=AXIS2_PLACEMENT_3D('',#36699,#29653,#29654);
#27005=AXIS2_PLACEMENT_3D('',#36705,#29658,#29659);
#27006=AXIS2_PLACEMENT_3D('',#36711,#29663,#29664);
#27007=AXIS2_PLACEMENT_3D('',#36715,#29667,#29668);
#27008=AXIS2_PLACEMENT_3D('',#36719,#29670,#29671);
#27009=AXIS2_PLACEMENT_3D('',#36721,#29673,#29674);
#27010=AXIS2_PLACEMENT_3D('',#36725,#29677,#29678);
#27011=AXIS2_PLACEMENT_3D('',#36728,#29680,#29681);
#27012=AXIS2_PLACEMENT_3D('',#36729,#29682,#29683);
#27013=AXIS2_PLACEMENT_3D('',#36733,#29686,#29687);
#27014=AXIS2_PLACEMENT_3D('',#36736,#29689,#29690);
#27015=AXIS2_PLACEMENT_3D('',#36737,#29691,#29692);
#27016=AXIS2_PLACEMENT_3D('',#36741,#29695,#29696);
#27017=AXIS2_PLACEMENT_3D('',#36744,#29698,#29699);
#27018=AXIS2_PLACEMENT_3D('',#36745,#29700,#29701);
#27019=AXIS2_PLACEMENT_3D('',#36747,#29703,#29704);
#27020=AXIS2_PLACEMENT_3D('',#36753,#29708,#29709);
#27021=AXIS2_PLACEMENT_3D('',#36756,#29711,#29712);
#27022=AXIS2_PLACEMENT_3D('',#36757,#29713,#29714);
#27023=AXIS2_PLACEMENT_3D('',#36761,#29717,#29718);
#27024=AXIS2_PLACEMENT_3D('',#36764,#29720,#29721);
#27025=AXIS2_PLACEMENT_3D('',#36765,#29722,#29723);
#27026=AXIS2_PLACEMENT_3D('',#36771,#29727,#29728);
#27027=AXIS2_PLACEMENT_3D('',#36775,#29730,#29731);
#27028=AXIS2_PLACEMENT_3D('',#36776,#29732,#29733);
#27029=AXIS2_PLACEMENT_3D('',#36777,#29734,#29735);
#27030=AXIS2_PLACEMENT_3D('',#36780,#29736,#29737);
#27031=AXIS2_PLACEMENT_3D('',#36787,#29742,#29743);
#27032=AXIS2_PLACEMENT_3D('',#36790,#29745,#29746);
#27033=AXIS2_PLACEMENT_3D('',#36791,#29747,#29748);
#27034=AXIS2_PLACEMENT_3D('',#36792,#29749,#29750);
#27035=AXIS2_PLACEMENT_3D('',#36795,#29753,#29754);
#27036=AXIS2_PLACEMENT_3D('',#36798,#29756,#29757);
#27037=AXIS2_PLACEMENT_3D('',#36799,#29758,#29759);
#27038=AXIS2_PLACEMENT_3D('',#36804,#29763,#29764);
#27039=AXIS2_PLACEMENT_3D('',#36805,#29765,#29766);
#27040=AXIS2_PLACEMENT_3D('',#36806,#29767,#29768);
#27041=AXIS2_PLACEMENT_3D('',#36813,#29772,#29773);
#27042=AXIS2_PLACEMENT_3D('',#36814,#29774,#29775);
#27043=AXIS2_PLACEMENT_3D('',#36815,#29776,#29777);
#27044=AXIS2_PLACEMENT_3D('',#36817,#29779,#29780);
#27045=AXIS2_PLACEMENT_3D('',#36818,#29781,#29782);
#27046=AXIS2_PLACEMENT_3D('',#36826,#29787,#29788);
#27047=AXIS2_PLACEMENT_3D('',#36829,#29790,#29791);
#27048=AXIS2_PLACEMENT_3D('',#36830,#29792,#29793);
#27049=AXIS2_PLACEMENT_3D('',#36834,#29796,#29797);
#27050=AXIS2_PLACEMENT_3D('',#36837,#29799,#29800);
#27051=AXIS2_PLACEMENT_3D('',#36838,#29801,#29802);
#27052=AXIS2_PLACEMENT_3D('',#36839,#29803,#29804);
#27053=AXIS2_PLACEMENT_3D('',#36843,#29807,#29808);
#27054=AXIS2_PLACEMENT_3D('',#36844,#29809,#29810);
#27055=AXIS2_PLACEMENT_3D('',#36845,#29811,#29812);
#27056=AXIS2_PLACEMENT_3D('',#36849,#29815,#29816);
#27057=AXIS2_PLACEMENT_3D('',#36852,#29818,#29819);
#27058=AXIS2_PLACEMENT_3D('',#36853,#29820,#29821);
#27059=AXIS2_PLACEMENT_3D('',#36857,#29824,#29825);
#27060=AXIS2_PLACEMENT_3D('',#36858,#29826,#29827);
#27061=AXIS2_PLACEMENT_3D('',#36859,#29828,#29829);
#27062=AXIS2_PLACEMENT_3D('',#36866,#29833,#29834);
#27063=AXIS2_PLACEMENT_3D('',#36873,#29838,#29839);
#27064=AXIS2_PLACEMENT_3D('',#36879,#29843,#29844);
#27065=AXIS2_PLACEMENT_3D('',#36883,#29846,#29847);
#27066=AXIS2_PLACEMENT_3D('',#36884,#29848,#29849);
#27067=AXIS2_PLACEMENT_3D('',#36885,#29850,#29851);
#27068=AXIS2_PLACEMENT_3D('',#36891,#29855,#29856);
#27069=AXIS2_PLACEMENT_3D('',#36895,#29858,#29859);
#27070=AXIS2_PLACEMENT_3D('',#36896,#29860,#29861);
#27071=AXIS2_PLACEMENT_3D('',#36897,#29862,#29863);
#27072=AXIS2_PLACEMENT_3D('',#36900,#29866,#29867);
#27073=AXIS2_PLACEMENT_3D('',#36903,#29870,#29871);
#27074=AXIS2_PLACEMENT_3D('',#36911,#29876,#29877);
#27075=AXIS2_PLACEMENT_3D('',#36919,#29882,#29883);
#27076=AXIS2_PLACEMENT_3D('',#36923,#29886,#29887);
#27077=AXIS2_PLACEMENT_3D('',#36925,#29889,#29890);
#27078=AXIS2_PLACEMENT_3D('',#36929,#29893,#29894);
#27079=AXIS2_PLACEMENT_3D('',#36932,#29896,#29897);
#27080=AXIS2_PLACEMENT_3D('',#36933,#29898,#29899);
#27081=AXIS2_PLACEMENT_3D('',#36937,#29902,#29903);
#27082=AXIS2_PLACEMENT_3D('',#36940,#29905,#29906);
#27083=AXIS2_PLACEMENT_3D('',#36941,#29907,#29908);
#27084=AXIS2_PLACEMENT_3D('',#36942,#29909,#29910);
#27085=AXIS2_PLACEMENT_3D('',#36944,#29912,#29913);
#27086=AXIS2_PLACEMENT_3D('',#36947,#29916,#29917);
#27087=AXIS2_PLACEMENT_3D('',#36950,#29920,#29921);
#27088=AXIS2_PLACEMENT_3D('',#36952,#29923,#29924);
#27089=AXIS2_PLACEMENT_3D('',#36955,#29927,#29928);
#27090=AXIS2_PLACEMENT_3D('',#36958,#29931,#29932);
#27091=AXIS2_PLACEMENT_3D('',#36960,#29934,#29935);
#27092=AXIS2_PLACEMENT_3D('',#36962,#29937,#29938);
#27093=AXIS2_PLACEMENT_3D('',#36963,#29939,#29940);
#27094=AXIS2_PLACEMENT_3D('',#36965,#29942,#29943);
#27095=AXIS2_PLACEMENT_3D('',#36968,#29945,#29946);
#27096=AXIS2_PLACEMENT_3D('',#36969,#29947,#29948);
#27097=AXIS2_PLACEMENT_3D('',#36970,#29949,#29950);
#27098=AXIS2_PLACEMENT_3D('',#36971,#29951,#29952);
#27099=AXIS2_PLACEMENT_3D('',#36972,#29953,#29954);
#27100=AXIS2_PLACEMENT_3D('',#36973,#29955,#29956);
#27101=AXIS2_PLACEMENT_3D('',#36974,#29957,#29958);
#27102=AXIS2_PLACEMENT_3D('',#36976,#29959,#29960);
#27103=AXIS2_PLACEMENT_3D('',#36977,#29961,#29962);
#27104=AXIS2_PLACEMENT_3D('',#36978,#29963,#29964);
#27105=AXIS2_PLACEMENT_3D('',#36979,#29965,#29966);
#27106=AXIS2_PLACEMENT_3D('',#36980,#29967,#29968);
#27107=AXIS2_PLACEMENT_3D('',#36981,#29969,#29970);
#27108=AXIS2_PLACEMENT_3D('',#36982,#29971,#29972);
#27109=AXIS2_PLACEMENT_3D('',#36983,#29973,#29974);
#27110=AXIS2_PLACEMENT_3D('',#36984,#29975,#29976);
#27111=AXIS2_PLACEMENT_3D('',#36985,#29977,#29978);
#27112=AXIS2_PLACEMENT_3D('',#36986,#29979,#29980);
#27113=AXIS2_PLACEMENT_3D('',#36987,#29981,#29982);
#27114=AXIS2_PLACEMENT_3D('',#36988,#29983,#29984);
#27115=AXIS2_PLACEMENT_3D('',#36989,#29985,#29986);
#27116=AXIS2_PLACEMENT_3D('',#36991,#29987,#29988);
#27117=AXIS2_PLACEMENT_3D('',#36992,#29989,#29990);
#27118=AXIS2_PLACEMENT_3D('',#36993,#29991,#29992);
#27119=AXIS2_PLACEMENT_3D('',#36995,#29994,#29995);
#27120=AXIS2_PLACEMENT_3D('',#36997,#29997,#29998);
#27121=AXIS2_PLACEMENT_3D('',#36999,#30000,#30001);
#27122=AXIS2_PLACEMENT_3D('',#37000,#30002,#30003);
#27123=AXIS2_PLACEMENT_3D('',#37002,#30005,#30006);
#27124=AXIS2_PLACEMENT_3D('',#37004,#30008,#30009);
#27125=AXIS2_PLACEMENT_3D('',#37006,#30011,#30012);
#27126=AXIS2_PLACEMENT_3D('',#37007,#30013,#30014);
#27127=AXIS2_PLACEMENT_3D('',#37009,#30016,#30017);
#27128=AXIS2_PLACEMENT_3D('',#37011,#30019,#30020);
#27129=AXIS2_PLACEMENT_3D('',#37013,#30022,#30023);
#27130=AXIS2_PLACEMENT_3D('',#37014,#30024,#30025);
#27131=AXIS2_PLACEMENT_3D('',#37015,#30026,#30027);
#27132=AXIS2_PLACEMENT_3D('',#37017,#30029,#30030);
#27133=AXIS2_PLACEMENT_3D('',#37019,#30032,#30033);
#27134=AXIS2_PLACEMENT_3D('',#37022,#30035,#30036);
#27135=AXIS2_PLACEMENT_3D('',#37025,#30038,#30039);
#27136=AXIS2_PLACEMENT_3D('',#37028,#30041,#30042);
#27137=AXIS2_PLACEMENT_3D('',#37031,#30044,#30045);
#27138=AXIS2_PLACEMENT_3D('',#37035,#30048,#30049);
#27139=AXIS2_PLACEMENT_3D('',#37037,#30051,#30052);
#27140=AXIS2_PLACEMENT_3D('',#37038,#30053,#30054);
#27141=AXIS2_PLACEMENT_3D('',#37039,#30055,#30056);
#27142=AXIS2_PLACEMENT_3D('',#37040,#30057,#30058);
#27143=AXIS2_PLACEMENT_3D('',#37042,#30059,#30060);
#27144=AXIS2_PLACEMENT_3D('',#37046,#30062,#30063);
#27145=AXIS2_PLACEMENT_3D('',#37047,#30064,#30065);
#27146=AXIS2_PLACEMENT_3D('',#37048,#30066,#30067);
#27147=AXIS2_PLACEMENT_3D('',#37052,#30069,#30070);
#27148=AXIS2_PLACEMENT_3D('',#37053,#30071,#30072);
#27149=AXIS2_PLACEMENT_3D('',#37054,#30073,#30074);
#27150=AXIS2_PLACEMENT_3D('',#37056,#30075,#30076);
#27151=AXIS2_PLACEMENT_3D('',#37057,#30077,#30078);
#27152=AXIS2_PLACEMENT_3D('',#37061,#30080,#30081);
#27153=AXIS2_PLACEMENT_3D('',#37062,#30082,#30083);
#27154=AXIS2_PLACEMENT_3D('',#37063,#30084,#30085);
#27155=AXIS2_PLACEMENT_3D('',#37135,#30087,#30088);
#27156=AXIS2_PLACEMENT_3D('',#37145,#30089,#30090);
#27157=AXIS2_PLACEMENT_3D('',#37149,#30092,#30093);
#27158=AXIS2_PLACEMENT_3D('',#37150,#30094,#30095);
#27159=AXIS2_PLACEMENT_3D('',#37151,#30096,#30097);
#27160=AXIS2_PLACEMENT_3D('',#37152,#30098,#30099);
#27161=AXIS2_PLACEMENT_3D('',#37155,#30100,#30101);
#27162=AXIS2_PLACEMENT_3D('',#37156,#30102,#30103);
#27163=AXIS2_PLACEMENT_3D('',#37159,#30105,#30106);
#27164=AXIS2_PLACEMENT_3D('',#37161,#30107,#30108);
#27165=AXIS2_PLACEMENT_3D('',#37170,#30109,#30110);
#27166=AXIS2_PLACEMENT_3D('',#37179,#30111,#30112);
#27167=AXIS2_PLACEMENT_3D('',#37187,#30113,#30114);
#27168=AXIS2_PLACEMENT_3D('',#37188,#30115,#30116);
#27169=AXIS2_PLACEMENT_3D('',#37190,#30117,#30118);
#27170=AXIS2_PLACEMENT_3D('',#37192,#30120,#30121);
#27171=AXIS2_PLACEMENT_3D('',#37194,#30122,#30123);
#27172=AXIS2_PLACEMENT_3D('',#37197,#30125,#30126);
#27173=AXIS2_PLACEMENT_3D('',#37198,#30127,#30128);
#27174=AXIS2_PLACEMENT_3D('',#37199,#30129,#30130);
#27175=AXIS2_PLACEMENT_3D('',#37201,#30131,#30132);
#27176=AXIS2_PLACEMENT_3D('',#37203,#30134,#30135);
#27177=AXIS2_PLACEMENT_3D('',#37216,#30142,#30143);
#27178=AXIS2_PLACEMENT_3D('',#37220,#30145,#30146);
#27179=AXIS2_PLACEMENT_3D('',#37234,#30148,#30149);
#27180=AXIS2_PLACEMENT_3D('',#37240,#30152,#30153);
#27181=AXIS2_PLACEMENT_3D('',#37243,#30155,#30156);
#27182=AXIS2_PLACEMENT_3D('',#37248,#30158,#30159);
#27183=AXIS2_PLACEMENT_3D('',#37251,#30161,#30162);
#27184=AXIS2_PLACEMENT_3D('',#37252,#30163,#30164);
#27185=AXIS2_PLACEMENT_3D('',#37258,#30168,#30169);
#27186=AXIS2_PLACEMENT_3D('',#37264,#30173,#30174);
#27187=AXIS2_PLACEMENT_3D('',#37266,#30175,#30176);
#27188=AXIS2_PLACEMENT_3D('',#37269,#30178,#30179);
#27189=AXIS2_PLACEMENT_3D('',#37270,#30180,#30181);
#27190=AXIS2_PLACEMENT_3D('',#37273,#30183,#30184);
#27191=AXIS2_PLACEMENT_3D('',#37274,#30185,#30186);
#27192=AXIS2_PLACEMENT_3D('',#37276,#30187,#30188);
#27193=AXIS2_PLACEMENT_3D('',#37573,#30190,#30191);
#27194=AXIS2_PLACEMENT_3D('',#37576,#30192,#30193);
#27195=AXIS2_PLACEMENT_3D('',#37577,#30194,#30195);
#27196=AXIS2_PLACEMENT_3D('',#37640,#30199,#30200);
#27197=AXIS2_PLACEMENT_3D('',#37651,#30201,#30202);
#27198=AXIS2_PLACEMENT_3D('',#37654,#30204,#30205);
#27199=AXIS2_PLACEMENT_3D('',#37655,#30206,#30207);
#27200=AXIS2_PLACEMENT_3D('',#37657,#30209,#30210);
#27201=AXIS2_PLACEMENT_3D('',#37666,#30215,#30216);
#27202=AXIS2_PLACEMENT_3D('',#37672,#30220,#30221);
#27203=AXIS2_PLACEMENT_3D('',#37674,#30222,#30223);
#27204=AXIS2_PLACEMENT_3D('',#37677,#30225,#30226);
#27205=AXIS2_PLACEMENT_3D('',#37976,#30230,#30231);
#27206=AXIS2_PLACEMENT_3D('',#37982,#30235,#30236);
#27207=AXIS2_PLACEMENT_3D('',#37988,#30240,#30241);
#27208=AXIS2_PLACEMENT_3D('',#37995,#30245,#30246);
#27209=AXIS2_PLACEMENT_3D('',#38001,#30250,#30251);
#27210=AXIS2_PLACEMENT_3D('',#38008,#30255,#30256);
#27211=AXIS2_PLACEMENT_3D('',#38014,#30260,#30261);
#27212=AXIS2_PLACEMENT_3D('',#38018,#30263,#30264);
#27213=AXIS2_PLACEMENT_3D('',#38019,#30265,#30266);
#27214=AXIS2_PLACEMENT_3D('',#38020,#30267,#30268);
#27215=AXIS2_PLACEMENT_3D('',#38026,#30272,#30273);
#27216=AXIS2_PLACEMENT_3D('',#38030,#30275,#30276);
#27217=AXIS2_PLACEMENT_3D('',#38031,#30277,#30278);
#27218=AXIS2_PLACEMENT_3D('',#38032,#30279,#30280);
#27219=AXIS2_PLACEMENT_3D('',#38035,#30283,#30284);
#27220=AXIS2_PLACEMENT_3D('',#38041,#30288,#30289);
#27221=AXIS2_PLACEMENT_3D('',#38044,#30292,#30293);
#27222=AXIS2_PLACEMENT_3D('',#38047,#30296,#30297);
#27223=AXIS2_PLACEMENT_3D('',#38050,#30300,#30301);
#27224=AXIS2_PLACEMENT_3D('',#38052,#30302,#30303);
#27225=AXIS2_PLACEMENT_3D('',#38054,#30305,#30306);
#27226=AXIS2_PLACEMENT_3D('',#38057,#30308,#30309);
#27227=AXIS2_PLACEMENT_3D('',#38130,#30311,#30312);
#27228=AXIS2_PLACEMENT_3D('',#38136,#30316,#30317);
#27229=AXIS2_PLACEMENT_3D('',#38196,#30319,#30320);
#27230=AXIS2_PLACEMENT_3D('',#38197,#30321,#30322);
#27231=AXIS2_PLACEMENT_3D('',#38208,#30328,#30329);
#27232=AXIS2_PLACEMENT_3D('',#38218,#30334,#30335);
#27233=AXIS2_PLACEMENT_3D('',#38222,#30338,#30339);
#27234=AXIS2_PLACEMENT_3D('',#38223,#30340,#30341);
#27235=AXIS2_PLACEMENT_3D('',#38225,#30343,#30344);
#27236=AXIS2_PLACEMENT_3D('',#38227,#30346,#30347);
#27237=AXIS2_PLACEMENT_3D('',#38228,#30348,#30349);
#27238=AXIS2_PLACEMENT_3D('',#38233,#30351,#30352);
#27239=AXIS2_PLACEMENT_3D('',#38236,#30354,#30355);
#27240=AXIS2_PLACEMENT_3D('',#38241,#30357,#30358);
#27241=AXIS2_PLACEMENT_3D('',#38244,#30360,#30361);
#27242=AXIS2_PLACEMENT_3D('',#38245,#30362,#30363);
#27243=AXIS2_PLACEMENT_3D('',#38251,#30367,#30368);
#27244=AXIS2_PLACEMENT_3D('',#38254,#30370,#30371);
#27245=AXIS2_PLACEMENT_3D('',#38255,#30372,#30373);
#27246=AXIS2_PLACEMENT_3D('',#38259,#30376,#30377);
#27247=AXIS2_PLACEMENT_3D('',#38260,#30378,#30379);
#27248=AXIS2_PLACEMENT_3D('',#38261,#30380,#30381);
#27249=AXIS2_PLACEMENT_3D('',#38265,#30383,#30384);
#27250=AXIS2_PLACEMENT_3D('',#38267,#30386,#30387);
#27251=AXIS2_PLACEMENT_3D('',#38271,#30390,#30391);
#27252=AXIS2_PLACEMENT_3D('',#38277,#30395,#30396);
#27253=AXIS2_PLACEMENT_3D('',#38280,#30398,#30399);
#27254=AXIS2_PLACEMENT_3D('',#38281,#30400,#30401);
#27255=AXIS2_PLACEMENT_3D('',#38285,#30404,#30405);
#27256=AXIS2_PLACEMENT_3D('',#38286,#30406,#30407);
#27257=AXIS2_PLACEMENT_3D('',#38287,#30408,#30409);
#27258=AXIS2_PLACEMENT_3D('',#38291,#30411,#30412);
#27259=AXIS2_PLACEMENT_3D('',#38293,#30414,#30415);
#27260=AXIS2_PLACEMENT_3D('',#38297,#30418,#30419);
#27261=AXIS2_PLACEMENT_3D('',#38303,#30423,#30424);
#27262=AXIS2_PLACEMENT_3D('',#38306,#30426,#30427);
#27263=AXIS2_PLACEMENT_3D('',#38307,#30428,#30429);
#27264=AXIS2_PLACEMENT_3D('',#38311,#30432,#30433);
#27265=AXIS2_PLACEMENT_3D('',#38312,#30434,#30435);
#27266=AXIS2_PLACEMENT_3D('',#38313,#30436,#30437);
#27267=AXIS2_PLACEMENT_3D('',#38317,#30439,#30440);
#27268=AXIS2_PLACEMENT_3D('',#38319,#30442,#30443);
#27269=AXIS2_PLACEMENT_3D('',#38323,#30446,#30447);
#27270=AXIS2_PLACEMENT_3D('',#38329,#30451,#30452);
#27271=AXIS2_PLACEMENT_3D('',#38332,#30454,#30455);
#27272=AXIS2_PLACEMENT_3D('',#38333,#30456,#30457);
#27273=AXIS2_PLACEMENT_3D('',#38337,#30460,#30461);
#27274=AXIS2_PLACEMENT_3D('',#38338,#30462,#30463);
#27275=AXIS2_PLACEMENT_3D('',#38339,#30464,#30465);
#27276=AXIS2_PLACEMENT_3D('',#38343,#30467,#30468);
#27277=AXIS2_PLACEMENT_3D('',#38345,#30470,#30471);
#27278=AXIS2_PLACEMENT_3D('',#38349,#30474,#30475);
#27279=AXIS2_PLACEMENT_3D('',#38351,#30476,#30477);
#27280=AXIS2_PLACEMENT_3D('',#38355,#30479,#30480);
#27281=AXIS2_PLACEMENT_3D('',#38356,#30481,#30482);
#27282=AXIS2_PLACEMENT_3D('',#38357,#30483,#30484);
#27283=AXIS2_PLACEMENT_3D('',#38358,#30485,#30486);
#27284=AXIS2_PLACEMENT_3D('',#38360,#30487,#30488);
#27285=AXIS2_PLACEMENT_3D('',#38362,#30490,#30491);
#27286=AXIS2_PLACEMENT_3D('',#38364,#30492,#30493);
#27287=AXIS2_PLACEMENT_3D('',#38367,#30495,#30496);
#27288=AXIS2_PLACEMENT_3D('',#38368,#30497,#30498);
#27289=AXIS2_PLACEMENT_3D('',#38369,#30499,#30500);
#27290=AXIS2_PLACEMENT_3D('',#38371,#30501,#30502);
#27291=AXIS2_PLACEMENT_3D('',#38373,#30504,#30505);
#27292=AXIS2_PLACEMENT_3D('',#38379,#30509,#30510);
#27293=AXIS2_PLACEMENT_3D('',#38383,#30512,#30513);
#27294=AXIS2_PLACEMENT_3D('',#38384,#30514,#30515);
#27295=AXIS2_PLACEMENT_3D('',#38385,#30516,#30517);
#27296=AXIS2_PLACEMENT_3D('',#38390,#30521,#30522);
#27297=AXIS2_PLACEMENT_3D('',#38391,#30523,#30524);
#27298=AXIS2_PLACEMENT_3D('',#38392,#30525,#30526);
#27299=AXIS2_PLACEMENT_3D('',#38394,#30528,#30529);
#27300=AXIS2_PLACEMENT_3D('',#38428,#30541,#30542);
#27301=AXIS2_PLACEMENT_3D('',#38432,#30544,#30545);
#27302=AXIS2_PLACEMENT_3D('',#38436,#30547,#30548);
#27303=AXIS2_PLACEMENT_3D('',#38439,#30550,#30551);
#27304=AXIS2_PLACEMENT_3D('',#38444,#30553,#30554);
#27305=AXIS2_PLACEMENT_3D('',#38447,#30556,#30557);
#27306=AXIS2_PLACEMENT_3D('',#38452,#30559,#30560);
#27307=AXIS2_PLACEMENT_3D('',#38455,#30562,#30563);
#27308=AXIS2_PLACEMENT_3D('',#38460,#30565,#30566);
#27309=AXIS2_PLACEMENT_3D('',#38463,#30568,#30569);
#27310=AXIS2_PLACEMENT_3D('',#38464,#30570,#30571);
#27311=AXIS2_PLACEMENT_3D('',#38467,#30574,#30575);
#27312=AXIS2_PLACEMENT_3D('',#38470,#30577,#30578);
#27313=AXIS2_PLACEMENT_3D('',#38471,#30579,#30580);
#27314=AXIS2_PLACEMENT_3D('',#38474,#30583,#30584);
#27315=AXIS2_PLACEMENT_3D('',#38475,#30585,#30586);
#27316=AXIS2_PLACEMENT_3D('',#38477,#30588,#30589);
#27317=AXIS2_PLACEMENT_3D('',#38480,#30592,#30593);
#27318=AXIS2_PLACEMENT_3D('',#38483,#30595,#30596);
#27319=AXIS2_PLACEMENT_3D('',#38484,#30597,#30598);
#27320=AXIS2_PLACEMENT_3D('',#38487,#30601,#30602);
#27321=AXIS2_PLACEMENT_3D('',#38488,#30603,#30604);
#27322=AXIS2_PLACEMENT_3D('',#38490,#30606,#30607);
#27323=AXIS2_PLACEMENT_3D('',#38493,#30610,#30611);
#27324=AXIS2_PLACEMENT_3D('',#38496,#30613,#30614);
#27325=AXIS2_PLACEMENT_3D('',#38497,#30615,#30616);
#27326=AXIS2_PLACEMENT_3D('',#38500,#30619,#30620);
#27327=AXIS2_PLACEMENT_3D('',#38501,#30621,#30622);
#27328=AXIS2_PLACEMENT_3D('',#38766,#30625,#30626);
#27329=AXIS2_PLACEMENT_3D('',#38771,#30629,#30630);
#27330=AXIS2_PLACEMENT_3D('',#38772,#30631,#30632);
#27331=AXIS2_PLACEMENT_3D('',#38776,#30635,#30636);
#27332=AXIS2_PLACEMENT_3D('',#38779,#30638,#30639);
#27333=AXIS2_PLACEMENT_3D('',#38780,#30640,#30641);
#27334=AXIS2_PLACEMENT_3D('',#38784,#30644,#30645);
#27335=AXIS2_PLACEMENT_3D('',#38786,#30647,#30648);
#27336=AXIS2_PLACEMENT_3D('',#38787,#30649,#30650);
#27337=AXIS2_PLACEMENT_3D('',#38789,#30652,#30653);
#27338=AXIS2_PLACEMENT_3D('',#38878,#30656,#30657);
#27339=AXIS2_PLACEMENT_3D('',#38879,#30658,#30659);
#27340=AXIS2_PLACEMENT_3D('',#38880,#30660,#30661);
#27341=AXIS2_PLACEMENT_3D('',#38882,#30663,#30664);
#27342=AXIS2_PLACEMENT_3D('',#38884,#30666,#30667);
#27343=AXIS2_PLACEMENT_3D('',#38886,#30669,#30670);
#27344=AXIS2_PLACEMENT_3D('',#38888,#30672,#30673);
#27345=AXIS2_PLACEMENT_3D('',#38897,#30676,#30677);
#27346=AXIS2_PLACEMENT_3D('',#38899,#30678,#30679);
#27347=AXIS2_PLACEMENT_3D('',#38902,#30681,#30682);
#27348=AXIS2_PLACEMENT_3D('',#39077,#30685,#30686);
#27349=AXIS2_PLACEMENT_3D('',#39081,#30689,#30690);
#27350=AXIS2_PLACEMENT_3D('',#39084,#30692,#30693);
#27351=AXIS2_PLACEMENT_3D('',#39085,#30694,#30695);
#27352=AXIS2_PLACEMENT_3D('',#39087,#30697,#30698);
#27353=AXIS2_PLACEMENT_3D('',#39100,#30701,#30702);
#27354=AXIS2_PLACEMENT_3D('',#39143,#30703,#30704);
#27355=AXIS2_PLACEMENT_3D('',#39145,#30706,#30707);
#27356=AXIS2_PLACEMENT_3D('',#39154,#30708,#30709);
#27357=AXIS2_PLACEMENT_3D('',#39155,#30710,#30711);
#27358=AXIS2_PLACEMENT_3D('',#39200,#30713,#30714);
#27359=AXIS2_PLACEMENT_3D('',#39208,#30716,#30717);
#27360=AXIS2_PLACEMENT_3D('',#39209,#30718,#30719);
#27361=AXIS2_PLACEMENT_3D('',#39210,#30720,#30721);
#27362=AXIS2_PLACEMENT_3D('',#39300,#30722,#30723);
#27363=AXIS2_PLACEMENT_3D('',#39311,#30724,#30725);
#27364=AXIS2_PLACEMENT_3D('',#39313,#30727,#30728);
#27365=AXIS2_PLACEMENT_3D('',#39314,#30729,#30730);
#27366=AXIS2_PLACEMENT_3D('',#39315,#30731,#30732);
#27367=AXIS2_PLACEMENT_3D('',#39316,#30733,#30734);
#27368=AXIS2_PLACEMENT_3D('',#39317,#30735,#30736);
#27369=AXIS2_PLACEMENT_3D('',#39318,#30737,#30738);
#27370=AXIS2_PLACEMENT_3D('',#39319,#30739,#30740);
#27371=AXIS2_PLACEMENT_3D('',#39320,#30741,#30742);
#27372=AXIS2_PLACEMENT_3D('',#39321,#30743,#30744);
#27373=AXIS2_PLACEMENT_3D('',#39322,#30745,#30746);
#27374=AXIS2_PLACEMENT_3D('',#39323,#30747,#30748);
#27375=AXIS2_PLACEMENT_3D('',#39324,#30749,#30750);
#27376=AXIS2_PLACEMENT_3D('',#39325,#30751,#30752);
#27377=AXIS2_PLACEMENT_3D('',#39326,#30753,#30754);
#27378=AXIS2_PLACEMENT_3D('',#39327,#30755,#30756);
#27379=AXIS2_PLACEMENT_3D('',#39328,#30757,#30758);
#27380=AXIS2_PLACEMENT_3D('',#39329,#30759,#30760);
#27381=AXIS2_PLACEMENT_3D('',#39332,#30762,#30763);
#27382=AXIS2_PLACEMENT_3D('',#39335,#30765,#30766);
#27383=AXIS2_PLACEMENT_3D('',#39338,#30768,#30769);
#27384=AXIS2_PLACEMENT_3D('',#39341,#30771,#30772);
#27385=AXIS2_PLACEMENT_3D('',#39343,#30773,#30774);
#27386=AXIS2_PLACEMENT_3D('',#39344,#30775,#30776);
#27387=AXIS2_PLACEMENT_3D('',#39384,#30778,#30779);
#27388=AXIS2_PLACEMENT_3D('',#39425,#30781,#30782);
#27389=AXIS2_PLACEMENT_3D('',#39426,#30783,#30784);
#27390=AXIS2_PLACEMENT_3D('',#39428,#30785,#30786);
#27391=AXIS2_PLACEMENT_3D('',#39429,#30787,#30788);
#27392=AXIS2_PLACEMENT_3D('',#39431,#30790,#30791);
#27393=AXIS2_PLACEMENT_3D('',#39433,#30792,#30793);
#27394=AXIS2_PLACEMENT_3D('',#39435,#30795,#30796);
#27395=AXIS2_PLACEMENT_3D('',#39436,#30797,#30798);
#27396=AXIS2_PLACEMENT_3D('',#39437,#30799,#30800);
#27397=AXIS2_PLACEMENT_3D('',#39439,#30801,#30802);
#27398=AXIS2_PLACEMENT_3D('',#39443,#30804,#30805);
#27399=AXIS2_PLACEMENT_3D('',#39444,#30806,#30807);
#27400=AXIS2_PLACEMENT_3D('',#39445,#30808,#30809);
#27401=AXIS2_PLACEMENT_3D('',#39448,#30811,#30812);
#27402=AXIS2_PLACEMENT_3D('',#39449,#30813,#30814);
#27403=AXIS2_PLACEMENT_3D('',#39451,#30815,#30816);
#27404=AXIS2_PLACEMENT_3D('',#39452,#30817,#30818);
#27405=AXIS2_PLACEMENT_3D('',#39461,#30823,#30824);
#27406=AXIS2_PLACEMENT_3D('',#39463,#30825,#30826);
#27407=AXIS2_PLACEMENT_3D('',#39467,#30829,#30830);
#27408=AXIS2_PLACEMENT_3D('',#39473,#30834,#30835);
#27409=AXIS2_PLACEMENT_3D('',#39474,#30836,#30837);
#27410=AXIS2_PLACEMENT_3D('',#39476,#30839,#30840);
#27411=AXIS2_PLACEMENT_3D('',#39477,#30841,#30842);
#27412=AXIS2_PLACEMENT_3D('',#39486,#30847,#30848);
#27413=AXIS2_PLACEMENT_3D('',#39488,#30849,#30850);
#27414=AXIS2_PLACEMENT_3D('',#39492,#30853,#30854);
#27415=AXIS2_PLACEMENT_3D('',#39498,#30858,#30859);
#27416=AXIS2_PLACEMENT_3D('',#39499,#30860,#30861);
#27417=AXIS2_PLACEMENT_3D('',#39501,#30863,#30864);
#27418=AXIS2_PLACEMENT_3D('',#39502,#30865,#30866);
#27419=AXIS2_PLACEMENT_3D('',#39511,#30871,#30872);
#27420=AXIS2_PLACEMENT_3D('',#39513,#30873,#30874);
#27421=AXIS2_PLACEMENT_3D('',#39517,#30877,#30878);
#27422=AXIS2_PLACEMENT_3D('',#39523,#30882,#30883);
#27423=AXIS2_PLACEMENT_3D('',#39524,#30884,#30885);
#27424=AXIS2_PLACEMENT_3D('',#39526,#30887,#30888);
#27425=AXIS2_PLACEMENT_3D('',#39527,#30889,#30890);
#27426=AXIS2_PLACEMENT_3D('',#39536,#30895,#30896);
#27427=AXIS2_PLACEMENT_3D('',#39538,#30897,#30898);
#27428=AXIS2_PLACEMENT_3D('',#39542,#30901,#30902);
#27429=AXIS2_PLACEMENT_3D('',#39548,#30906,#30907);
#27430=AXIS2_PLACEMENT_3D('',#39549,#30908,#30909);
#27431=AXIS2_PLACEMENT_3D('',#39551,#30911,#30912);
#27432=AXIS2_PLACEMENT_3D('',#39552,#30913,#30914);
#27433=AXIS2_PLACEMENT_3D('',#39561,#30919,#30920);
#27434=AXIS2_PLACEMENT_3D('',#39563,#30921,#30922);
#27435=AXIS2_PLACEMENT_3D('',#39567,#30925,#30926);
#27436=AXIS2_PLACEMENT_3D('',#39573,#30930,#30931);
#27437=AXIS2_PLACEMENT_3D('',#39574,#30932,#30933);
#27438=AXIS2_PLACEMENT_3D('',#39576,#30935,#30936);
#27439=AXIS2_PLACEMENT_3D('',#39577,#30937,#30938);
#27440=AXIS2_PLACEMENT_3D('',#39586,#30943,#30944);
#27441=AXIS2_PLACEMENT_3D('',#39588,#30945,#30946);
#27442=AXIS2_PLACEMENT_3D('',#39592,#30949,#30950);
#27443=AXIS2_PLACEMENT_3D('',#39598,#30954,#30955);
#27444=AXIS2_PLACEMENT_3D('',#39599,#30956,#30957);
#27445=AXIS2_PLACEMENT_3D('',#39601,#30959,#30960);
#27446=AXIS2_PLACEMENT_3D('',#39602,#30961,#30962);
#27447=AXIS2_PLACEMENT_3D('',#39611,#30967,#30968);
#27448=AXIS2_PLACEMENT_3D('',#39613,#30969,#30970);
#27449=AXIS2_PLACEMENT_3D('',#39617,#30973,#30974);
#27450=AXIS2_PLACEMENT_3D('',#39623,#30978,#30979);
#27451=AXIS2_PLACEMENT_3D('',#39624,#30980,#30981);
#27452=AXIS2_PLACEMENT_3D('',#39626,#30983,#30984);
#27453=AXIS2_PLACEMENT_3D('',#39627,#30985,#30986);
#27454=AXIS2_PLACEMENT_3D('',#39636,#30991,#30992);
#27455=AXIS2_PLACEMENT_3D('',#39638,#30993,#30994);
#27456=AXIS2_PLACEMENT_3D('',#39642,#30997,#30998);
#27457=AXIS2_PLACEMENT_3D('',#39648,#31002,#31003);
#27458=AXIS2_PLACEMENT_3D('',#39649,#31004,#31005);
#27459=AXIS2_PLACEMENT_3D('',#39651,#31007,#31008);
#27460=AXIS2_PLACEMENT_3D('',#39652,#31009,#31010);
#27461=AXIS2_PLACEMENT_3D('',#39661,#31015,#31016);
#27462=AXIS2_PLACEMENT_3D('',#39663,#31017,#31018);
#27463=AXIS2_PLACEMENT_3D('',#39667,#31021,#31022);
#27464=AXIS2_PLACEMENT_3D('',#39673,#31026,#31027);
#27465=AXIS2_PLACEMENT_3D('',#39674,#31028,#31029);
#27466=AXIS2_PLACEMENT_3D('',#39676,#31031,#31032);
#27467=AXIS2_PLACEMENT_3D('',#39677,#31033,#31034);
#27468=AXIS2_PLACEMENT_3D('',#39686,#31039,#31040);
#27469=AXIS2_PLACEMENT_3D('',#39688,#31041,#31042);
#27470=AXIS2_PLACEMENT_3D('',#39692,#31045,#31046);
#27471=AXIS2_PLACEMENT_3D('',#39698,#31050,#31051);
#27472=AXIS2_PLACEMENT_3D('',#39699,#31052,#31053);
#27473=AXIS2_PLACEMENT_3D('',#39701,#31055,#31056);
#27474=AXIS2_PLACEMENT_3D('',#39702,#31057,#31058);
#27475=AXIS2_PLACEMENT_3D('',#39711,#31063,#31064);
#27476=AXIS2_PLACEMENT_3D('',#39713,#31065,#31066);
#27477=AXIS2_PLACEMENT_3D('',#39717,#31069,#31070);
#27478=AXIS2_PLACEMENT_3D('',#39723,#31074,#31075);
#27479=AXIS2_PLACEMENT_3D('',#39724,#31076,#31077);
#27480=AXIS2_PLACEMENT_3D('',#39726,#31079,#31080);
#27481=AXIS2_PLACEMENT_3D('',#39727,#31081,#31082);
#27482=AXIS2_PLACEMENT_3D('',#39736,#31087,#31088);
#27483=AXIS2_PLACEMENT_3D('',#39738,#31089,#31090);
#27484=AXIS2_PLACEMENT_3D('',#39742,#31093,#31094);
#27485=AXIS2_PLACEMENT_3D('',#39748,#31098,#31099);
#27486=AXIS2_PLACEMENT_3D('',#39749,#31100,#31101);
#27487=AXIS2_PLACEMENT_3D('',#39751,#31103,#31104);
#27488=AXIS2_PLACEMENT_3D('',#39752,#31105,#31106);
#27489=AXIS2_PLACEMENT_3D('',#39761,#31111,#31112);
#27490=AXIS2_PLACEMENT_3D('',#39763,#31113,#31114);
#27491=AXIS2_PLACEMENT_3D('',#39767,#31117,#31118);
#27492=AXIS2_PLACEMENT_3D('',#39773,#31122,#31123);
#27493=AXIS2_PLACEMENT_3D('',#39774,#31124,#31125);
#27494=AXIS2_PLACEMENT_3D('',#39776,#31127,#31128);
#27495=AXIS2_PLACEMENT_3D('',#39777,#31129,#31130);
#27496=AXIS2_PLACEMENT_3D('',#39786,#31135,#31136);
#27497=AXIS2_PLACEMENT_3D('',#39788,#31137,#31138);
#27498=AXIS2_PLACEMENT_3D('',#39792,#31141,#31142);
#27499=AXIS2_PLACEMENT_3D('',#39798,#31146,#31147);
#27500=AXIS2_PLACEMENT_3D('',#39799,#31148,#31149);
#27501=AXIS2_PLACEMENT_3D('',#39801,#31151,#31152);
#27502=AXIS2_PLACEMENT_3D('',#39802,#31153,#31154);
#27503=AXIS2_PLACEMENT_3D('',#39811,#31159,#31160);
#27504=AXIS2_PLACEMENT_3D('',#39813,#31161,#31162);
#27505=AXIS2_PLACEMENT_3D('',#39817,#31165,#31166);
#27506=AXIS2_PLACEMENT_3D('',#39823,#31170,#31171);
#27507=AXIS2_PLACEMENT_3D('',#39824,#31172,#31173);
#27508=AXIS2_PLACEMENT_3D('',#39826,#31175,#31176);
#27509=AXIS2_PLACEMENT_3D('',#39827,#31177,#31178);
#27510=AXIS2_PLACEMENT_3D('',#39836,#31183,#31184);
#27511=AXIS2_PLACEMENT_3D('',#39838,#31185,#31186);
#27512=AXIS2_PLACEMENT_3D('',#39842,#31189,#31190);
#27513=AXIS2_PLACEMENT_3D('',#39848,#31194,#31195);
#27514=AXIS2_PLACEMENT_3D('',#39849,#31196,#31197);
#27515=AXIS2_PLACEMENT_3D('',#39851,#31199,#31200);
#27516=AXIS2_PLACEMENT_3D('',#39852,#31201,#31202);
#27517=AXIS2_PLACEMENT_3D('',#39861,#31207,#31208);
#27518=AXIS2_PLACEMENT_3D('',#39863,#31209,#31210);
#27519=AXIS2_PLACEMENT_3D('',#39867,#31213,#31214);
#27520=AXIS2_PLACEMENT_3D('',#39873,#31218,#31219);
#27521=AXIS2_PLACEMENT_3D('',#39874,#31220,#31221);
#27522=AXIS2_PLACEMENT_3D('',#39876,#31223,#31224);
#27523=AXIS2_PLACEMENT_3D('',#39877,#31225,#31226);
#27524=AXIS2_PLACEMENT_3D('',#39886,#31231,#31232);
#27525=AXIS2_PLACEMENT_3D('',#39888,#31233,#31234);
#27526=AXIS2_PLACEMENT_3D('',#39892,#31237,#31238);
#27527=AXIS2_PLACEMENT_3D('',#39898,#31242,#31243);
#27528=AXIS2_PLACEMENT_3D('',#39899,#31244,#31245);
#27529=AXIS2_PLACEMENT_3D('',#39901,#31247,#31248);
#27530=AXIS2_PLACEMENT_3D('',#39902,#31249,#31250);
#27531=AXIS2_PLACEMENT_3D('',#39911,#31255,#31256);
#27532=AXIS2_PLACEMENT_3D('',#39913,#31257,#31258);
#27533=AXIS2_PLACEMENT_3D('',#39917,#31261,#31262);
#27534=AXIS2_PLACEMENT_3D('',#39923,#31266,#31267);
#27535=AXIS2_PLACEMENT_3D('',#39924,#31268,#31269);
#27536=AXIS2_PLACEMENT_3D('',#39926,#31271,#31272);
#27537=AXIS2_PLACEMENT_3D('',#39927,#31273,#31274);
#27538=AXIS2_PLACEMENT_3D('',#39936,#31279,#31280);
#27539=AXIS2_PLACEMENT_3D('',#39938,#31281,#31282);
#27540=AXIS2_PLACEMENT_3D('',#39942,#31285,#31286);
#27541=AXIS2_PLACEMENT_3D('',#39948,#31290,#31291);
#27542=AXIS2_PLACEMENT_3D('',#39949,#31292,#31293);
#27543=AXIS2_PLACEMENT_3D('',#39951,#31295,#31296);
#27544=AXIS2_PLACEMENT_3D('',#39952,#31297,#31298);
#27545=AXIS2_PLACEMENT_3D('',#39961,#31303,#31304);
#27546=AXIS2_PLACEMENT_3D('',#39963,#31305,#31306);
#27547=AXIS2_PLACEMENT_3D('',#39967,#31309,#31310);
#27548=AXIS2_PLACEMENT_3D('',#39973,#31314,#31315);
#27549=AXIS2_PLACEMENT_3D('',#39974,#31316,#31317);
#27550=AXIS2_PLACEMENT_3D('',#39976,#31319,#31320);
#27551=AXIS2_PLACEMENT_3D('',#39977,#31321,#31322);
#27552=AXIS2_PLACEMENT_3D('',#39986,#31327,#31328);
#27553=AXIS2_PLACEMENT_3D('',#40007,#31329,#31330);
#27554=AXIS2_PLACEMENT_3D('',#40009,#31332,#31333);
#27555=AXIS2_PLACEMENT_3D('',#40015,#31337,#31338);
#27556=AXIS2_PLACEMENT_3D('',#40034,#31339,#31340);
#27557=AXIS2_PLACEMENT_3D('',#40035,#31341,#31342);
#27558=AXIS2_PLACEMENT_3D('',#40036,#31343,#31344);
#27559=AXIS2_PLACEMENT_3D('',#40038,#31345,#31346);
#27560=AXIS2_PLACEMENT_3D('',#40041,#31348,#31349);
#27561=AXIS2_PLACEMENT_3D('',#40042,#31350,#31351);
#27562=AXIS2_PLACEMENT_3D('',#40044,#31352,#31353);
#27563=AXIS2_PLACEMENT_3D('',#40045,#31354,#31355);
#27564=AXIS2_PLACEMENT_3D('',#40047,#31356,#31357);
#27565=AXIS2_PLACEMENT_3D('',#40049,#31359,#31360);
#27566=AXIS2_PLACEMENT_3D('',#40051,#31362,#31363);
#27567=AXIS2_PLACEMENT_3D('',#40054,#31365,#31366);
#27568=AXIS2_PLACEMENT_3D('',#40055,#31367,#31368);
#27569=AXIS2_PLACEMENT_3D('',#40058,#31370,#31371);
#27570=AXIS2_PLACEMENT_3D('',#40059,#31372,#31373);
#27571=AXIS2_PLACEMENT_3D('',#40061,#31374,#31375);
#27572=AXIS2_PLACEMENT_3D('',#40062,#31376,#31377);
#27573=AXIS2_PLACEMENT_3D('',#40065,#31379,#31380);
#27574=AXIS2_PLACEMENT_3D('',#40066,#31381,#31382);
#27575=AXIS2_PLACEMENT_3D('',#40067,#31383,#31384);
#27576=AXIS2_PLACEMENT_3D('',#40068,#31385,#31386);
#27577=AXIS2_PLACEMENT_3D('',#40071,#31387,#31388);
#27578=AXIS2_PLACEMENT_3D('',#40072,#31389,#31390);
#27579=AXIS2_PLACEMENT_3D('',#40076,#31392,#31393);
#27580=AXIS2_PLACEMENT_3D('',#40077,#31394,#31395);
#27581=AXIS2_PLACEMENT_3D('',#40078,#31396,#31397);
#27582=AXIS2_PLACEMENT_3D('',#40081,#31399,#31400);
#27583=AXIS2_PLACEMENT_3D('',#40082,#31401,#31402);
#27584=AXIS2_PLACEMENT_3D('',#40085,#31404,#31405);
#27585=AXIS2_PLACEMENT_3D('',#40087,#31406,#31407);
#27586=AXIS2_PLACEMENT_3D('',#40088,#31408,#31409);
#27587=AXIS2_PLACEMENT_3D('',#40090,#31410,#31411);
#27588=AXIS2_PLACEMENT_3D('',#40092,#31413,#31414);
#27589=AXIS2_PLACEMENT_3D('',#40094,#31416,#31417);
#27590=AXIS2_PLACEMENT_3D('',#40095,#31418,#31419);
#27591=AXIS2_PLACEMENT_3D('',#40123,#31421,#31422);
#27592=AXIS2_PLACEMENT_3D('',#40128,#31423,#31424);
#27593=AXIS2_PLACEMENT_3D('',#40212,#31426,#31427);
#27594=AXIS2_PLACEMENT_3D('',#40299,#31429,#31430);
#27595=AXIS2_PLACEMENT_3D('',#40383,#31432,#31433);
#27596=AXIS2_PLACEMENT_3D('',#40455,#31435,#31436);
#27597=AXIS2_PLACEMENT_3D('',#40524,#31438,#31439);
#27598=AXIS2_PLACEMENT_3D('',#40608,#31441,#31442);
#27599=AXIS2_PLACEMENT_3D('',#40692,#31444,#31445);
#27600=AXIS2_PLACEMENT_3D('',#40779,#31447,#31448);
#27601=AXIS2_PLACEMENT_3D('',#40863,#31450,#31451);
#27602=AXIS2_PLACEMENT_3D('',#40950,#31453,#31454);
#27603=AXIS2_PLACEMENT_3D('',#41034,#31456,#31457);
#27604=AXIS2_PLACEMENT_3D('',#41118,#31459,#31460);
#27605=AXIS2_PLACEMENT_3D('',#41205,#31462,#31463);
#27606=AXIS2_PLACEMENT_3D('',#41274,#31465,#31466);
#27607=AXIS2_PLACEMENT_3D('',#41346,#31468,#31469);
#27608=AXIS2_PLACEMENT_3D('',#41427,#31471,#31472);
#27609=AXIS2_PLACEMENT_3D('',#41514,#31474,#31475);
#27610=AXIS2_PLACEMENT_3D('',#41601,#31477,#31478);
#27611=AXIS2_PLACEMENT_3D('',#41685,#31480,#31481);
#27612=AXIS2_PLACEMENT_3D('',#41772,#31483,#31484);
#27613=AXIS2_PLACEMENT_3D('',#41844,#31486,#31487);
#27614=AXIS2_PLACEMENT_3D('',#41934,#31489,#31490);
#27615=AXIS2_PLACEMENT_3D('',#42018,#31492,#31493);
#27616=AXIS2_PLACEMENT_3D('',#42102,#31495,#31496);
#27617=AXIS2_PLACEMENT_3D('',#42189,#31498,#31499);
#27618=AXIS2_PLACEMENT_3D('',#42270,#31501,#31502);
#27619=AXIS2_PLACEMENT_3D('',#42342,#31504,#31505);
#27620=AXIS2_PLACEMENT_3D('',#42411,#31507,#31508);
#27621=AXIS2_PLACEMENT_3D('',#42495,#31510,#31511);
#27622=AXIS2_PLACEMENT_3D('',#42579,#31513,#31514);
#27623=AXIS2_PLACEMENT_3D('',#42663,#31516,#31517);
#27624=AXIS2_PLACEMENT_3D('',#42753,#31519,#31520);
#27625=AXIS2_PLACEMENT_3D('',#42837,#31522,#31523);
#27626=AXIS2_PLACEMENT_3D('',#42921,#31525,#31526);
#27627=AXIS2_PLACEMENT_3D('',#43005,#31528,#31529);
#27628=AXIS2_PLACEMENT_3D('',#43089,#31531,#31532);
#27629=AXIS2_PLACEMENT_3D('',#43158,#31534,#31535);
#27630=AXIS2_PLACEMENT_3D('',#43242,#31537,#31538);
#27631=AXIS2_PLACEMENT_3D('',#43329,#31540,#31541);
#27632=AXIS2_PLACEMENT_3D('',#43413,#31543,#31544);
#27633=AXIS2_PLACEMENT_3D('',#43497,#31546,#31547);
#27634=AXIS2_PLACEMENT_3D('',#43513,#31549,#31550);
#27635=AXIS2_PLACEMENT_3D('',#43519,#31551,#31552);
#27636=AXIS2_PLACEMENT_3D('',#43554,#31554,#31555);
#27637=AXIS2_PLACEMENT_3D('',#43591,#31557,#31558);
#27638=AXIS2_PLACEMENT_3D('',#43627,#31560,#31561);
#27639=AXIS2_PLACEMENT_3D('',#43663,#31563,#31564);
#27640=AXIS2_PLACEMENT_3D('',#43709,#31566,#31567);
#27641=AXIS2_PLACEMENT_3D('',#43744,#31569,#31570);
#27642=AXIS2_PLACEMENT_3D('',#43781,#31572,#31573);
#27643=AXIS2_PLACEMENT_3D('',#43816,#31575,#31576);
#27644=AXIS2_PLACEMENT_3D('',#43853,#31578,#31579);
#27645=AXIS2_PLACEMENT_3D('',#43890,#31581,#31582);
#27646=AXIS2_PLACEMENT_3D('',#43926,#31584,#31585);
#27647=AXIS2_PLACEMENT_3D('',#43963,#31587,#31588);
#27648=AXIS2_PLACEMENT_3D('',#43998,#31590,#31591);
#27649=AXIS2_PLACEMENT_3D('',#44035,#31593,#31594);
#27650=AXIS2_PLACEMENT_3D('',#44080,#31596,#31597);
#27651=AXIS2_PLACEMENT_3D('',#44116,#31599,#31600);
#27652=AXIS2_PLACEMENT_3D('',#44152,#31602,#31603);
#27653=AXIS2_PLACEMENT_3D('',#44188,#31605,#31606);
#27654=AXIS2_PLACEMENT_3D('',#44225,#31608,#31609);
#27655=AXIS2_PLACEMENT_3D('',#44262,#31611,#31612);
#27656=AXIS2_PLACEMENT_3D('',#44297,#31614,#31615);
#27657=AXIS2_PLACEMENT_3D('',#44331,#31617,#31618);
#27658=AXIS2_PLACEMENT_3D('',#44368,#31620,#31621);
#27659=AXIS2_PLACEMENT_3D('',#44404,#31623,#31624);
#27660=AXIS2_PLACEMENT_3D('',#44441,#31626,#31627);
#27661=AXIS2_PLACEMENT_3D('',#44477,#31629,#31630);
#27662=AXIS2_PLACEMENT_3D('',#44513,#31632,#31633);
#27663=AXIS2_PLACEMENT_3D('',#44549,#31635,#31636);
#27664=AXIS2_PLACEMENT_3D('',#44585,#31638,#31639);
#27665=AXIS2_PLACEMENT_3D('',#44622,#31641,#31642);
#27666=AXIS2_PLACEMENT_3D('',#44657,#31644,#31645);
#27667=AXIS2_PLACEMENT_3D('',#44694,#31647,#31648);
#27668=AXIS2_PLACEMENT_3D('',#44731,#31650,#31651);
#27669=AXIS2_PLACEMENT_3D('',#44767,#31653,#31654);
#27670=AXIS2_PLACEMENT_3D('',#44804,#31656,#31657);
#27671=AXIS2_PLACEMENT_3D('',#44839,#31659,#31660);
#27672=AXIS2_PLACEMENT_3D('',#44876,#31662,#31663);
#27673=AXIS2_PLACEMENT_3D('',#44911,#31665,#31666);
#27674=AXIS2_PLACEMENT_3D('',#44948,#31668,#31669);
#27675=AXIS2_PLACEMENT_3D('',#44984,#31671,#31672);
#27676=AXIS2_PLACEMENT_3D('',#45020,#31674,#31675);
#27677=AXIS2_PLACEMENT_3D('',#45022,#31676,#31677);
#27678=AXIS2_PLACEMENT_3D('',#45026,#31679,#31680);
#27679=AXIS2_PLACEMENT_3D('',#45027,#31681,#31682);
#27680=AXIS2_PLACEMENT_3D('',#45028,#31683,#31684);
#27681=AXIS2_PLACEMENT_3D('',#45032,#31686,#31687);
#27682=AXIS2_PLACEMENT_3D('',#45034,#31688,#31689);
#27683=AXIS2_PLACEMENT_3D('',#45035,#31690,#31691);
#27684=AXIS2_PLACEMENT_3D('',#45036,#31692,#31693);
#27685=AXIS2_PLACEMENT_3D('',#45037,#31694,#31695);
#27686=AXIS2_PLACEMENT_3D('',#45039,#31696,#31697);
#27687=AXIS2_PLACEMENT_3D('',#45042,#31699,#31700);
#27688=AXIS2_PLACEMENT_3D('',#45043,#31701,#31702);
#27689=AXIS2_PLACEMENT_3D('',#45045,#31703,#31704);
#27690=AXIS2_PLACEMENT_3D('',#45047,#31706,#31707);
#27691=AXIS2_PLACEMENT_3D('',#45049,#31708,#31709);
#27692=AXIS2_PLACEMENT_3D('',#45050,#31710,#31711);
#27693=AXIS2_PLACEMENT_3D('',#45163,#31712,#31713);
#27694=AXIS2_PLACEMENT_3D('',#47277,#31714,#31715);
#27695=AXIS2_PLACEMENT_3D('',#47298,#31716,#31717);
#27696=AXIS2_PLACEMENT_3D('',#47299,#31718,#31719);
#27697=AXIS2_PLACEMENT_3D('',#49540,#31720,#31721);
#27698=AXIS2_PLACEMENT_3D('',#49541,#31722,#31723);
#27699=AXIS2_PLACEMENT_3D('',#49542,#31724,#31725);
#27700=AXIS2_PLACEMENT_3D('',#49543,#31726,#31727);
#27701=AXIS2_PLACEMENT_3D('',#49546,#31729,#31730);
#27702=AXIS2_PLACEMENT_3D('',#49555,#31735,#31736);
#27703=AXIS2_PLACEMENT_3D('',#49576,#31737,#31738);
#27704=AXIS2_PLACEMENT_3D('',#49578,#31740,#31741);
#27705=AXIS2_PLACEMENT_3D('',#49584,#31745,#31746);
#27706=AXIS2_PLACEMENT_3D('',#49603,#31747,#31748);
#27707=AXIS2_PLACEMENT_3D('',#49604,#31749,#31750);
#27708=AXIS2_PLACEMENT_3D('',#49605,#31751,#31752);
#27709=AXIS2_PLACEMENT_3D('',#49607,#31753,#31754);
#27710=AXIS2_PLACEMENT_3D('',#49609,#31756,#31757);
#27711=AXIS2_PLACEMENT_3D('',#49611,#31758,#31759);
#27712=AXIS2_PLACEMENT_3D('',#49613,#31761,#31762);
#27713=AXIS2_PLACEMENT_3D('',#49615,#31763,#31764);
#27714=AXIS2_PLACEMENT_3D('',#49616,#31765,#31766);
#27715=AXIS2_PLACEMENT_3D('',#49618,#31767,#31768);
#27716=AXIS2_PLACEMENT_3D('',#49620,#31770,#31771);
#27717=AXIS2_PLACEMENT_3D('',#49622,#31772,#31773);
#27718=AXIS2_PLACEMENT_3D('',#49624,#31775,#31776);
#27719=AXIS2_PLACEMENT_3D('',#49626,#31777,#31778);
#27720=AXIS2_PLACEMENT_3D('',#49628,#31780,#31781);
#27721=AXIS2_PLACEMENT_3D('',#49629,#31782,#31783);
#27722=AXIS2_PLACEMENT_3D('',#49630,#31784,#31785);
#27723=AXIS2_PLACEMENT_3D('',#49632,#31786,#31787);
#27724=AXIS2_PLACEMENT_3D('',#49636,#31789,#31790);
#27725=AXIS2_PLACEMENT_3D('',#49637,#31791,#31792);
#27726=AXIS2_PLACEMENT_3D('',#49638,#31793,#31794);
#27727=AXIS2_PLACEMENT_3D('',#49641,#31795,#31796);
#27728=AXIS2_PLACEMENT_3D('',#49642,#31797,#31798);
#27729=AXIS2_PLACEMENT_3D('',#49644,#31800,#31801);
#27730=AXIS2_PLACEMENT_3D('',#49646,#31802,#31803);
#27731=AXIS2_PLACEMENT_3D('',#49647,#31804,#31805);
#27732=AXIS2_PLACEMENT_3D('',#49651,#31807,#31808);
#27733=AXIS2_PLACEMENT_3D('',#49652,#31809,#31810);
#27734=AXIS2_PLACEMENT_3D('',#49653,#31811,#31812);
#27735=AXIS2_PLACEMENT_3D('',#49655,#31813,#31814);
#27736=AXIS2_PLACEMENT_3D('',#49657,#31816,#31817);
#27737=AXIS2_PLACEMENT_3D('',#49659,#31818,#31819);
#27738=AXIS2_PLACEMENT_3D('',#49661,#31820,#31821);
#27739=AXIS2_PLACEMENT_3D('',#49662,#31822,#31823);
#27740=AXIS2_PLACEMENT_3D('',#49664,#31824,#31825);
#27741=AXIS2_PLACEMENT_3D('',#49666,#31827,#31828);
#27742=AXIS2_PLACEMENT_3D('',#49668,#31829,#31830);
#27743=AXIS2_PLACEMENT_3D('',#49669,#31831,#31832);
#27744=AXIS2_PLACEMENT_3D('',#49672,#31834,#31835);
#27745=AXIS2_PLACEMENT_3D('',#49673,#31836,#31837);
#27746=AXIS2_PLACEMENT_3D('',#49675,#31839,#31840);
#27747=AXIS2_PLACEMENT_3D('',#49677,#31841,#31842);
#27748=AXIS2_PLACEMENT_3D('',#49679,#31844,#31845);
#27749=AXIS2_PLACEMENT_3D('',#49681,#31846,#31847);
#27750=AXIS2_PLACEMENT_3D('',#49683,#31849,#31850);
#27751=AXIS2_PLACEMENT_3D('',#49685,#31851,#31852);
#27752=AXIS2_PLACEMENT_3D('',#49686,#31853,#31854);
#27753=AXIS2_PLACEMENT_3D('',#49688,#31856,#31857);
#27754=AXIS2_PLACEMENT_3D('',#49689,#31858,#31859);
#27755=AXIS2_PLACEMENT_3D('',#49692,#31860,#31861);
#27756=AXIS2_PLACEMENT_3D('',#49693,#31862,#31863);
#27757=AXIS2_PLACEMENT_3D('',#49696,#31865,#31866);
#27758=AXIS2_PLACEMENT_3D('',#49697,#31867,#31868);
#27759=AXIS2_PLACEMENT_3D('',#49699,#31869,#31870);
#27760=AXIS2_PLACEMENT_3D('',#49700,#31871,#31872);
#27761=AXIS2_PLACEMENT_3D('',#49703,#31874,#31875);
#27762=AXIS2_PLACEMENT_3D('',#49704,#31876,#31877);
#27763=AXIS2_PLACEMENT_3D('',#49706,#31878,#31879);
#27764=AXIS2_PLACEMENT_3D('',#49710,#31881,#31882);
#27765=AXIS2_PLACEMENT_3D('',#49711,#31883,#31884);
#27766=AXIS2_PLACEMENT_3D('',#49712,#31885,#31886);
#27767=AXIS2_PLACEMENT_3D('',#49716,#31888,#31889);
#27768=AXIS2_PLACEMENT_3D('',#49717,#31890,#31891);
#27769=AXIS2_PLACEMENT_3D('',#49718,#31892,#31893);
#27770=AXIS2_PLACEMENT_3D('',#49720,#31894,#31895);
#27771=AXIS2_PLACEMENT_3D('',#49722,#31896,#31897);
#27772=AXIS2_PLACEMENT_3D('',#49724,#31898,#31899);
#27773=AXIS2_PLACEMENT_3D('',#49726,#31900,#31901);
#27774=AXIS2_PLACEMENT_3D('',#49728,#31902,#31903);
#27775=AXIS2_PLACEMENT_3D('',#49729,#31904,#31905);
#27776=AXIS2_PLACEMENT_3D('',#49733,#31907,#31908);
#27777=AXIS2_PLACEMENT_3D('',#49734,#31909,#31910);
#27778=AXIS2_PLACEMENT_3D('',#49735,#31911,#31912);
#27779=AXIS2_PLACEMENT_3D('',#49739,#31914,#31915);
#27780=AXIS2_PLACEMENT_3D('',#49740,#31916,#31917);
#27781=AXIS2_PLACEMENT_3D('',#49741,#31918,#31919);
#27782=AXIS2_PLACEMENT_3D('',#49745,#31921,#31922);
#27783=AXIS2_PLACEMENT_3D('',#49746,#31923,#31924);
#27784=AXIS2_PLACEMENT_3D('',#49747,#31925,#31926);
#27785=AXIS2_PLACEMENT_3D('',#49751,#31928,#31929);
#27786=AXIS2_PLACEMENT_3D('',#49752,#31930,#31931);
#27787=AXIS2_PLACEMENT_3D('',#49753,#31932,#31933);
#27788=AXIS2_PLACEMENT_3D('',#49756,#31935,#31936);
#27789=AXIS2_PLACEMENT_3D('',#49757,#31937,#31938);
#27790=AXIS2_PLACEMENT_3D('',#49759,#31939,#31940);
#27791=AXIS2_PLACEMENT_3D('',#49761,#31941,#31942);
#27792=AXIS2_PLACEMENT_3D('',#49763,#31943,#31944);
#27793=AXIS2_PLACEMENT_3D('',#49765,#31945,#31946);
#27794=AXIS2_PLACEMENT_3D('',#49767,#31947,#31948);
#27795=AXIS2_PLACEMENT_3D('',#49768,#31949,#31950);
#27796=AXIS2_PLACEMENT_3D('',#49771,#31951,#31952);
#27797=AXIS2_PLACEMENT_3D('',#49772,#31953,#31954);
#27798=AXIS2_PLACEMENT_3D('',#49776,#31956,#31957);
#27799=AXIS2_PLACEMENT_3D('',#49777,#31958,#31959);
#27800=AXIS2_PLACEMENT_3D('',#49778,#31960,#31961);
#27801=AXIS2_PLACEMENT_3D('',#49782,#31963,#31964);
#27802=AXIS2_PLACEMENT_3D('',#49783,#31965,#31966);
#27803=AXIS2_PLACEMENT_3D('',#49784,#31967,#31968);
#27804=AXIS2_PLACEMENT_3D('',#49786,#31970,#31971);
#27805=AXIS2_PLACEMENT_3D('',#49789,#31973,#31974);
#27806=AXIS2_PLACEMENT_3D('',#49790,#31975,#31976);
#27807=AXIS2_PLACEMENT_3D('',#49792,#31977,#31978);
#27808=AXIS2_PLACEMENT_3D('',#49793,#31979,#31980);
#27809=AXIS2_PLACEMENT_3D('',#49797,#31982,#31983);
#27810=AXIS2_PLACEMENT_3D('',#49798,#31984,#31985);
#27811=AXIS2_PLACEMENT_3D('',#49799,#31986,#31987);
#27812=AXIS2_PLACEMENT_3D('',#49801,#31988,#31989);
#27813=AXIS2_PLACEMENT_3D('',#49803,#31991,#31992);
#27814=AXIS2_PLACEMENT_3D('',#49805,#31994,#31995);
#27815=AXIS2_PLACEMENT_3D('',#49807,#31997,#31998);
#27816=AXIS2_PLACEMENT_3D('',#49809,#32000,#32001);
#27817=AXIS2_PLACEMENT_3D('',#49811,#32003,#32004);
#27818=AXIS2_PLACEMENT_3D('',#49813,#32005,#32006);
#27819=AXIS2_PLACEMENT_3D('',#49815,#32008,#32009);
#27820=AXIS2_PLACEMENT_3D('',#49817,#32011,#32012);
#27821=AXIS2_PLACEMENT_3D('',#49819,#32013,#32014);
#27822=AXIS2_PLACEMENT_3D('',#49820,#32015,#32016);
#27823=AXIS2_PLACEMENT_3D('',#49823,#32018,#32019);
#27824=AXIS2_PLACEMENT_3D('',#49824,#32020,#32021);
#27825=AXIS2_PLACEMENT_3D('',#49825,#32022,#32023);
#27826=AXIS2_PLACEMENT_3D('',#49826,#32024,#32025);
#27827=AXIS2_PLACEMENT_3D('',#49829,#32026,#32027);
#27828=AXIS2_PLACEMENT_3D('',#49830,#32028,#32029);
#27829=AXIS2_PLACEMENT_3D('',#49834,#32031,#32032);
#27830=AXIS2_PLACEMENT_3D('',#49835,#32033,#32034);
#27831=AXIS2_PLACEMENT_3D('',#49836,#32035,#32036);
#27832=AXIS2_PLACEMENT_3D('',#49840,#32038,#32039);
#27833=AXIS2_PLACEMENT_3D('',#49841,#32040,#32041);
#27834=AXIS2_PLACEMENT_3D('',#49994,#32042,#32043);
#27835=AXIS2_PLACEMENT_3D('',#49997,#32044,#32045);
#27836=AXIS2_PLACEMENT_3D('',#49998,#32046,#32047);
#27837=AXIS2_PLACEMENT_3D('',#50000,#32049,#32050);
#27838=AXIS2_PLACEMENT_3D('',#50004,#32052,#32053);
#27839=AXIS2_PLACEMENT_3D('',#50005,#32054,#32055);
#27840=AXIS2_PLACEMENT_3D('',#50006,#32056,#32057);
#27841=AXIS2_PLACEMENT_3D('',#50010,#32059,#32060);
#27842=AXIS2_PLACEMENT_3D('',#50011,#32061,#32062);
#27843=AXIS2_PLACEMENT_3D('',#50012,#32063,#32064);
#27844=AXIS2_PLACEMENT_3D('',#50015,#32066,#32067);
#27845=AXIS2_PLACEMENT_3D('',#50016,#32068,#32069);
#27846=AXIS2_PLACEMENT_3D('',#50018,#32070,#32071);
#27847=AXIS2_PLACEMENT_3D('',#50019,#32072,#32073);
#27848=AXIS2_PLACEMENT_3D('',#50021,#32074,#32075);
#27849=AXIS2_PLACEMENT_3D('',#50023,#32077,#32078);
#27850=AXIS2_PLACEMENT_3D('',#50028,#32080,#32081);
#27851=AXIS2_PLACEMENT_3D('',#50032,#32084,#32085);
#27852=AXIS2_PLACEMENT_3D('',#50036,#32087,#32088);
#27853=AXIS2_PLACEMENT_3D('',#50038,#32090,#32091);
#27854=AXIS2_PLACEMENT_3D('',#50040,#32092,#32093);
#27855=AXIS2_PLACEMENT_3D('',#50044,#32096,#32097);
#27856=AXIS2_PLACEMENT_3D('',#50046,#32099,#32100);
#27857=AXIS2_PLACEMENT_3D('',#50052,#32104,#32105);
#27858=AXIS2_PLACEMENT_3D('',#50056,#32108,#32109);
#27859=AXIS2_PLACEMENT_3D('',#50060,#32112,#32113);
#27860=AXIS2_PLACEMENT_3D('',#50061,#32114,#32115);
#27861=AXIS2_PLACEMENT_3D('',#50062,#32116,#32117);
#27862=AXIS2_PLACEMENT_3D('',#50121,#32119,#32120);
#27863=AXIS2_PLACEMENT_3D('',#50180,#32122,#32123);
#27864=AXIS2_PLACEMENT_3D('',#50239,#32125,#32126);
#27865=AXIS2_PLACEMENT_3D('',#50298,#32128,#32129);
#27866=AXIS2_PLACEMENT_3D('',#50300,#32130,#32131);
#27867=AXIS2_PLACEMENT_3D('',#50301,#32132,#32133);
#27868=AXIS2_PLACEMENT_3D('',#50302,#32134,#32135);
#27869=AXIS2_PLACEMENT_3D('',#50303,#32136,#32137);
#27870=AXIS2_PLACEMENT_3D('',#50304,#32138,#32139);
#27871=AXIS2_PLACEMENT_3D('',#50305,#32140,#32141);
#27872=AXIS2_PLACEMENT_3D('',#50306,#32142,#32143);
#27873=AXIS2_PLACEMENT_3D('',#50308,#32144,#32145);
#27874=AXIS2_PLACEMENT_3D('',#50310,#32147,#32148);
#27875=AXIS2_PLACEMENT_3D('',#50311,#32149,#32150);
#27876=AXIS2_PLACEMENT_3D('',#50312,#32151,#32152);
#27877=AXIS2_PLACEMENT_3D('',#50328,#32154,#32155);
#27878=AXIS2_PLACEMENT_3D('',#50336,#32156,#32157);
#27879=AXIS2_PLACEMENT_3D('',#50384,#32159,#32160);
#27880=AXIS2_PLACEMENT_3D('',#50432,#32162,#32163);
#27881=AXIS2_PLACEMENT_3D('',#50486,#32165,#32166);
#27882=AXIS2_PLACEMENT_3D('',#50534,#32168,#32169);
#27883=AXIS2_PLACEMENT_3D('',#50582,#32171,#32172);
#27884=AXIS2_PLACEMENT_3D('',#50636,#32174,#32175);
#27885=AXIS2_PLACEMENT_3D('',#50684,#32177,#32178);
#27886=AXIS2_PLACEMENT_3D('',#50732,#32180,#32181);
#27887=AXIS2_PLACEMENT_3D('',#50786,#32183,#32184);
#27888=AXIS2_PLACEMENT_3D('',#50834,#32186,#32187);
#27889=AXIS2_PLACEMENT_3D('',#50882,#32189,#32190);
#27890=AXIS2_PLACEMENT_3D('',#50936,#32192,#32193);
#27891=AXIS2_PLACEMENT_3D('',#50984,#32195,#32196);
#27892=AXIS2_PLACEMENT_3D('',#51032,#32198,#32199);
#27893=AXIS2_PLACEMENT_3D('',#51086,#32201,#32202);
#27894=AXIS2_PLACEMENT_3D('',#51101,#32204,#32205);
#27895=AXIS2_PLACEMENT_3D('',#51109,#32206,#32207);
#27896=AXIS2_PLACEMENT_3D('',#51134,#32209,#32210);
#27897=AXIS2_PLACEMENT_3D('',#51158,#32212,#32213);
#27898=AXIS2_PLACEMENT_3D('',#51183,#32215,#32216);
#27899=AXIS2_PLACEMENT_3D('',#51208,#32218,#32219);
#27900=AXIS2_PLACEMENT_3D('',#51232,#32221,#32222);
#27901=AXIS2_PLACEMENT_3D('',#51257,#32224,#32225);
#27902=AXIS2_PLACEMENT_3D('',#51282,#32227,#32228);
#27903=AXIS2_PLACEMENT_3D('',#51306,#32230,#32231);
#27904=AXIS2_PLACEMENT_3D('',#51331,#32233,#32234);
#27905=AXIS2_PLACEMENT_3D('',#51356,#32236,#32237);
#27906=AXIS2_PLACEMENT_3D('',#51380,#32239,#32240);
#27907=AXIS2_PLACEMENT_3D('',#51405,#32242,#32243);
#27908=AXIS2_PLACEMENT_3D('',#51430,#32245,#32246);
#27909=AXIS2_PLACEMENT_3D('',#51454,#32248,#32249);
#27910=AXIS2_PLACEMENT_3D('',#51518,#32250,#32251);
#27911=AXIS2_PLACEMENT_3D('',#51520,#32252,#32253);
#27912=AXIS2_PLACEMENT_3D('',#52072,#32254,#32255);
#27913=AXIS2_PLACEMENT_3D('',#52074,#32256,#32257);
#27914=AXIS2_PLACEMENT_3D('',#52075,#32258,#32259);
#27915=AXIS2_PLACEMENT_3D('',#52138,#32260,#32261);
#27916=AXIS2_PLACEMENT_3D('',#52139,#32262,#32263);
#27917=AXIS2_PLACEMENT_3D('',#52564,#32264,#32265);
#27918=AXIS2_PLACEMENT_3D('',#52566,#32266,#32267);
#27919=AXIS2_PLACEMENT_3D('',#52567,#32268,#32269);
#27920=AXIS2_PLACEMENT_3D('',#52568,#32270,#32271);
#27921=AXIS2_PLACEMENT_3D('',#52569,#32272,#32273);
#27922=AXIS2_PLACEMENT_3D('',#52570,#32274,#32275);
#27923=AXIS2_PLACEMENT_3D('',#52572,#32276,#32277);
#27924=AXIS2_PLACEMENT_3D('',#52573,#32278,#32279);
#27925=AXIS2_PLACEMENT_3D('',#52577,#32281,#32282);
#27926=AXIS2_PLACEMENT_3D('',#52578,#32283,#32284);
#27927=AXIS2_PLACEMENT_3D('',#52581,#32286,#32287);
#27928=AXIS2_PLACEMENT_3D('',#52582,#32288,#32289);
#27929=AXIS2_PLACEMENT_3D('',#52585,#32291,#32292);
#27930=AXIS2_PLACEMENT_3D('',#52586,#32293,#32294);
#27931=AXIS2_PLACEMENT_3D('',#52589,#32296,#32297);
#27932=AXIS2_PLACEMENT_3D('',#52590,#32298,#32299);
#27933=AXIS2_PLACEMENT_3D('',#52593,#32301,#32302);
#27934=AXIS2_PLACEMENT_3D('',#52594,#32303,#32304);
#27935=AXIS2_PLACEMENT_3D('',#52596,#32306,#32307);
#27936=AXIS2_PLACEMENT_3D('',#52597,#32308,#32309);
#27937=AXIS2_PLACEMENT_3D('',#52600,#32311,#32312);
#27938=AXIS2_PLACEMENT_3D('',#52606,#32316,#32317);
#27939=AXIS2_PLACEMENT_3D('',#52610,#32320,#32321);
#27940=AXIS2_PLACEMENT_3D('',#52614,#32324,#32325);
#27941=AXIS2_PLACEMENT_3D('',#52618,#32328,#32329);
#27942=AXIS2_PLACEMENT_3D('',#52622,#32332,#32333);
#27943=AXIS2_PLACEMENT_3D('',#52624,#32335,#32336);
#27944=AXIS2_PLACEMENT_3D('',#52633,#32341,#32342);
#27945=AXIS2_PLACEMENT_3D('',#52635,#32343,#32344);
#27946=AXIS2_PLACEMENT_3D('',#52637,#32346,#32347);
#27947=AXIS2_PLACEMENT_3D('',#52641,#32350,#32351);
#27948=AXIS2_PLACEMENT_3D('',#52642,#32352,#32353);
#27949=AXIS2_PLACEMENT_3D('',#52643,#32354,#32355);
#27950=AXIS2_PLACEMENT_3D('',#52652,#32360,#32361);
#27951=AXIS2_PLACEMENT_3D('',#52654,#32362,#32363);
#27952=AXIS2_PLACEMENT_3D('',#52656,#32365,#32366);
#27953=AXIS2_PLACEMENT_3D('',#52660,#32369,#32370);
#27954=AXIS2_PLACEMENT_3D('',#52661,#32371,#32372);
#27955=AXIS2_PLACEMENT_3D('',#52662,#32373,#32374);
#27956=AXIS2_PLACEMENT_3D('',#52671,#32379,#32380);
#27957=AXIS2_PLACEMENT_3D('',#52673,#32381,#32382);
#27958=AXIS2_PLACEMENT_3D('',#52675,#32384,#32385);
#27959=AXIS2_PLACEMENT_3D('',#52679,#32388,#32389);
#27960=AXIS2_PLACEMENT_3D('',#52680,#32390,#32391);
#27961=AXIS2_PLACEMENT_3D('',#52681,#32392,#32393);
#27962=AXIS2_PLACEMENT_3D('',#52690,#32398,#32399);
#27963=AXIS2_PLACEMENT_3D('',#52692,#32400,#32401);
#27964=AXIS2_PLACEMENT_3D('',#52694,#32403,#32404);
#27965=AXIS2_PLACEMENT_3D('',#52698,#32407,#32408);
#27966=AXIS2_PLACEMENT_3D('',#52699,#32409,#32410);
#27967=AXIS2_PLACEMENT_3D('',#52700,#32411,#32412);
#27968=AXIS2_PLACEMENT_3D('',#52709,#32417,#32418);
#27969=AXIS2_PLACEMENT_3D('',#52711,#32419,#32420);
#27970=AXIS2_PLACEMENT_3D('',#52713,#32422,#32423);
#27971=AXIS2_PLACEMENT_3D('',#52717,#32426,#32427);
#27972=AXIS2_PLACEMENT_3D('',#52718,#32428,#32429);
#27973=AXIS2_PLACEMENT_3D('',#52719,#32430,#32431);
#27974=AXIS2_PLACEMENT_3D('',#52728,#32436,#32437);
#27975=AXIS2_PLACEMENT_3D('',#52730,#32438,#32439);
#27976=AXIS2_PLACEMENT_3D('',#52732,#32441,#32442);
#27977=AXIS2_PLACEMENT_3D('',#52736,#32445,#32446);
#27978=AXIS2_PLACEMENT_3D('',#52737,#32447,#32448);
#27979=AXIS2_PLACEMENT_3D('',#52738,#32449,#32450);
#27980=AXIS2_PLACEMENT_3D('',#52747,#32455,#32456);
#27981=AXIS2_PLACEMENT_3D('',#52749,#32457,#32458);
#27982=AXIS2_PLACEMENT_3D('',#52751,#32460,#32461);
#27983=AXIS2_PLACEMENT_3D('',#52755,#32464,#32465);
#27984=AXIS2_PLACEMENT_3D('',#52756,#32466,#32467);
#27985=AXIS2_PLACEMENT_3D('',#52757,#32468,#32469);
#27986=AXIS2_PLACEMENT_3D('',#52766,#32474,#32475);
#27987=AXIS2_PLACEMENT_3D('',#52768,#32476,#32477);
#27988=AXIS2_PLACEMENT_3D('',#52770,#32479,#32480);
#27989=AXIS2_PLACEMENT_3D('',#52774,#32483,#32484);
#27990=AXIS2_PLACEMENT_3D('',#52775,#32485,#32486);
#27991=AXIS2_PLACEMENT_3D('',#52776,#32487,#32488);
#27992=AXIS2_PLACEMENT_3D('',#52785,#32493,#32494);
#27993=AXIS2_PLACEMENT_3D('',#52787,#32495,#32496);
#27994=AXIS2_PLACEMENT_3D('',#52790,#32498,#32499);
#27995=AXIS2_PLACEMENT_3D('',#52791,#32500,#32501);
#27996=AXIS2_PLACEMENT_3D('',#52795,#32504,#32505);
#27997=AXIS2_PLACEMENT_3D('',#52797,#32506,#32507);
#27998=AXIS2_PLACEMENT_3D('',#52798,#32508,#32509);
#27999=AXIS2_PLACEMENT_3D('',#52799,#32510,#32511);
#28000=AXIS2_PLACEMENT_3D('',#52808,#32516,#32517);
#28001=AXIS2_PLACEMENT_3D('',#52810,#32518,#32519);
#28002=AXIS2_PLACEMENT_3D('',#52812,#32521,#32522);
#28003=AXIS2_PLACEMENT_3D('',#52816,#32525,#32526);
#28004=AXIS2_PLACEMENT_3D('',#52817,#32527,#32528);
#28005=AXIS2_PLACEMENT_3D('',#52818,#32529,#32530);
#28006=AXIS2_PLACEMENT_3D('',#52827,#32535,#32536);
#28007=AXIS2_PLACEMENT_3D('',#52829,#32537,#32538);
#28008=AXIS2_PLACEMENT_3D('',#52831,#32540,#32541);
#28009=AXIS2_PLACEMENT_3D('',#52835,#32544,#32545);
#28010=AXIS2_PLACEMENT_3D('',#52836,#32546,#32547);
#28011=AXIS2_PLACEMENT_3D('',#52837,#32548,#32549);
#28012=AXIS2_PLACEMENT_3D('',#52846,#32554,#32555);
#28013=AXIS2_PLACEMENT_3D('',#52848,#32556,#32557);
#28014=AXIS2_PLACEMENT_3D('',#52850,#32559,#32560);
#28015=AXIS2_PLACEMENT_3D('',#52854,#32563,#32564);
#28016=AXIS2_PLACEMENT_3D('',#52855,#32565,#32566);
#28017=AXIS2_PLACEMENT_3D('',#52856,#32567,#32568);
#28018=AXIS2_PLACEMENT_3D('',#52865,#32573,#32574);
#28019=AXIS2_PLACEMENT_3D('',#52867,#32575,#32576);
#28020=AXIS2_PLACEMENT_3D('',#52869,#32578,#32579);
#28021=AXIS2_PLACEMENT_3D('',#52873,#32582,#32583);
#28022=AXIS2_PLACEMENT_3D('',#52874,#32584,#32585);
#28023=AXIS2_PLACEMENT_3D('',#52875,#32586,#32587);
#28024=AXIS2_PLACEMENT_3D('',#52884,#32592,#32593);
#28025=AXIS2_PLACEMENT_3D('',#52886,#32594,#32595);
#28026=AXIS2_PLACEMENT_3D('',#52888,#32597,#32598);
#28027=AXIS2_PLACEMENT_3D('',#52892,#32601,#32602);
#28028=AXIS2_PLACEMENT_3D('',#52893,#32603,#32604);
#28029=AXIS2_PLACEMENT_3D('',#52894,#32605,#32606);
#28030=AXIS2_PLACEMENT_3D('',#52903,#32611,#32612);
#28031=AXIS2_PLACEMENT_3D('',#52905,#32613,#32614);
#28032=AXIS2_PLACEMENT_3D('',#52907,#32616,#32617);
#28033=AXIS2_PLACEMENT_3D('',#52911,#32620,#32621);
#28034=AXIS2_PLACEMENT_3D('',#52912,#32622,#32623);
#28035=AXIS2_PLACEMENT_3D('',#52913,#32624,#32625);
#28036=AXIS2_PLACEMENT_3D('',#52922,#32630,#32631);
#28037=AXIS2_PLACEMENT_3D('',#52924,#32632,#32633);
#28038=AXIS2_PLACEMENT_3D('',#52926,#32635,#32636);
#28039=AXIS2_PLACEMENT_3D('',#52930,#32639,#32640);
#28040=AXIS2_PLACEMENT_3D('',#52931,#32641,#32642);
#28041=AXIS2_PLACEMENT_3D('',#52932,#32643,#32644);
#28042=AXIS2_PLACEMENT_3D('',#52941,#32649,#32650);
#28043=AXIS2_PLACEMENT_3D('',#52943,#32651,#32652);
#28044=AXIS2_PLACEMENT_3D('',#52945,#32654,#32655);
#28045=AXIS2_PLACEMENT_3D('',#52949,#32658,#32659);
#28046=AXIS2_PLACEMENT_3D('',#52950,#32660,#32661);
#28047=AXIS2_PLACEMENT_3D('',#52951,#32662,#32663);
#28048=AXIS2_PLACEMENT_3D('',#52960,#32668,#32669);
#28049=AXIS2_PLACEMENT_3D('',#52962,#32670,#32671);
#28050=AXIS2_PLACEMENT_3D('',#52964,#32673,#32674);
#28051=AXIS2_PLACEMENT_3D('',#52968,#32677,#32678);
#28052=AXIS2_PLACEMENT_3D('',#52969,#32679,#32680);
#28053=AXIS2_PLACEMENT_3D('',#52970,#32681,#32682);
#28054=AXIS2_PLACEMENT_3D('',#52979,#32687,#32688);
#28055=AXIS2_PLACEMENT_3D('',#52981,#32689,#32690);
#28056=AXIS2_PLACEMENT_3D('',#52983,#32692,#32693);
#28057=AXIS2_PLACEMENT_3D('',#52987,#32696,#32697);
#28058=AXIS2_PLACEMENT_3D('',#52988,#32698,#32699);
#28059=AXIS2_PLACEMENT_3D('',#52989,#32700,#32701);
#28060=AXIS2_PLACEMENT_3D('',#52998,#32706,#32707);
#28061=AXIS2_PLACEMENT_3D('',#53000,#32708,#32709);
#28062=AXIS2_PLACEMENT_3D('',#53002,#32711,#32712);
#28063=AXIS2_PLACEMENT_3D('',#53006,#32715,#32716);
#28064=AXIS2_PLACEMENT_3D('',#53007,#32717,#32718);
#28065=AXIS2_PLACEMENT_3D('',#53008,#32719,#32720);
#28066=AXIS2_PLACEMENT_3D('',#53017,#32725,#32726);
#28067=AXIS2_PLACEMENT_3D('',#53019,#32727,#32728);
#28068=AXIS2_PLACEMENT_3D('',#53021,#32730,#32731);
#28069=AXIS2_PLACEMENT_3D('',#53025,#32734,#32735);
#28070=AXIS2_PLACEMENT_3D('',#53026,#32736,#32737);
#28071=AXIS2_PLACEMENT_3D('',#53027,#32738,#32739);
#28072=AXIS2_PLACEMENT_3D('',#53036,#32744,#32745);
#28073=AXIS2_PLACEMENT_3D('',#53038,#32746,#32747);
#28074=AXIS2_PLACEMENT_3D('',#53040,#32749,#32750);
#28075=AXIS2_PLACEMENT_3D('',#53044,#32753,#32754);
#28076=AXIS2_PLACEMENT_3D('',#53045,#32755,#32756);
#28077=AXIS2_PLACEMENT_3D('',#53046,#32757,#32758);
#28078=AXIS2_PLACEMENT_3D('',#53055,#32763,#32764);
#28079=AXIS2_PLACEMENT_3D('',#53057,#32765,#32766);
#28080=AXIS2_PLACEMENT_3D('',#53059,#32768,#32769);
#28081=AXIS2_PLACEMENT_3D('',#53063,#32772,#32773);
#28082=AXIS2_PLACEMENT_3D('',#53064,#32774,#32775);
#28083=AXIS2_PLACEMENT_3D('',#53065,#32776,#32777);
#28084=AXIS2_PLACEMENT_3D('',#53074,#32782,#32783);
#28085=AXIS2_PLACEMENT_3D('',#53076,#32784,#32785);
#28086=AXIS2_PLACEMENT_3D('',#53078,#32787,#32788);
#28087=AXIS2_PLACEMENT_3D('',#53082,#32791,#32792);
#28088=AXIS2_PLACEMENT_3D('',#53083,#32793,#32794);
#28089=AXIS2_PLACEMENT_3D('',#53084,#32795,#32796);
#28090=AXIS2_PLACEMENT_3D('',#53093,#32801,#32802);
#28091=AXIS2_PLACEMENT_3D('',#53095,#32803,#32804);
#28092=AXIS2_PLACEMENT_3D('',#53097,#32806,#32807);
#28093=AXIS2_PLACEMENT_3D('',#53101,#32810,#32811);
#28094=AXIS2_PLACEMENT_3D('',#53102,#32812,#32813);
#28095=AXIS2_PLACEMENT_3D('',#53103,#32814,#32815);
#28096=AXIS2_PLACEMENT_3D('',#53112,#32820,#32821);
#28097=AXIS2_PLACEMENT_3D('',#53114,#32822,#32823);
#28098=AXIS2_PLACEMENT_3D('',#53116,#32825,#32826);
#28099=AXIS2_PLACEMENT_3D('',#53120,#32829,#32830);
#28100=AXIS2_PLACEMENT_3D('',#53121,#32831,#32832);
#28101=AXIS2_PLACEMENT_3D('',#53122,#32833,#32834);
#28102=AXIS2_PLACEMENT_3D('',#53125,#32835,#32836);
#28103=AXIS2_PLACEMENT_3D('',#53129,#32839,#32840);
#28104=AXIS2_PLACEMENT_3D('',#53135,#32844,#32845);
#28105=AXIS2_PLACEMENT_3D('',#53139,#32848,#32849);
#28106=AXIS2_PLACEMENT_3D('',#53140,#32850,#32851);
#28107=AXIS2_PLACEMENT_3D('',#53141,#32852,#32853);
#28108=AXIS2_PLACEMENT_3D('',#53150,#32858,#32859);
#28109=AXIS2_PLACEMENT_3D('',#53152,#32860,#32861);
#28110=AXIS2_PLACEMENT_3D('',#53154,#32863,#32864);
#28111=AXIS2_PLACEMENT_3D('',#53158,#32867,#32868);
#28112=AXIS2_PLACEMENT_3D('',#53159,#32869,#32870);
#28113=AXIS2_PLACEMENT_3D('',#53160,#32871,#32872);
#28114=AXIS2_PLACEMENT_3D('',#53169,#32877,#32878);
#28115=AXIS2_PLACEMENT_3D('',#53171,#32879,#32880);
#28116=AXIS2_PLACEMENT_3D('',#53173,#32882,#32883);
#28117=AXIS2_PLACEMENT_3D('',#53177,#32886,#32887);
#28118=AXIS2_PLACEMENT_3D('',#53178,#32888,#32889);
#28119=AXIS2_PLACEMENT_3D('',#53179,#32890,#32891);
#28120=AXIS2_PLACEMENT_3D('',#53188,#32896,#32897);
#28121=AXIS2_PLACEMENT_3D('',#53190,#32898,#32899);
#28122=AXIS2_PLACEMENT_3D('',#53192,#32901,#32902);
#28123=AXIS2_PLACEMENT_3D('',#53196,#32905,#32906);
#28124=AXIS2_PLACEMENT_3D('',#53197,#32907,#32908);
#28125=AXIS2_PLACEMENT_3D('',#53198,#32909,#32910);
#28126=AXIS2_PLACEMENT_3D('',#53207,#32915,#32916);
#28127=AXIS2_PLACEMENT_3D('',#53209,#32917,#32918);
#28128=AXIS2_PLACEMENT_3D('',#53211,#32920,#32921);
#28129=AXIS2_PLACEMENT_3D('',#53215,#32924,#32925);
#28130=AXIS2_PLACEMENT_3D('',#53216,#32926,#32927);
#28131=AXIS2_PLACEMENT_3D('',#53217,#32928,#32929);
#28132=AXIS2_PLACEMENT_3D('',#53226,#32934,#32935);
#28133=AXIS2_PLACEMENT_3D('',#53228,#32936,#32937);
#28134=AXIS2_PLACEMENT_3D('',#53230,#32939,#32940);
#28135=AXIS2_PLACEMENT_3D('',#53234,#32943,#32944);
#28136=AXIS2_PLACEMENT_3D('',#53235,#32945,#32946);
#28137=AXIS2_PLACEMENT_3D('',#53236,#32947,#32948);
#28138=AXIS2_PLACEMENT_3D('',#53245,#32953,#32954);
#28139=AXIS2_PLACEMENT_3D('',#53247,#32955,#32956);
#28140=AXIS2_PLACEMENT_3D('',#53249,#32958,#32959);
#28141=AXIS2_PLACEMENT_3D('',#53253,#32962,#32963);
#28142=AXIS2_PLACEMENT_3D('',#53254,#32964,#32965);
#28143=AXIS2_PLACEMENT_3D('',#53255,#32966,#32967);
#28144=AXIS2_PLACEMENT_3D('',#53264,#32972,#32973);
#28145=AXIS2_PLACEMENT_3D('',#53266,#32974,#32975);
#28146=AXIS2_PLACEMENT_3D('',#53268,#32977,#32978);
#28147=AXIS2_PLACEMENT_3D('',#53272,#32981,#32982);
#28148=AXIS2_PLACEMENT_3D('',#53273,#32983,#32984);
#28149=AXIS2_PLACEMENT_3D('',#53274,#32985,#32986);
#28150=AXIS2_PLACEMENT_3D('',#53283,#32991,#32992);
#28151=AXIS2_PLACEMENT_3D('',#53285,#32993,#32994);
#28152=AXIS2_PLACEMENT_3D('',#53287,#32996,#32997);
#28153=AXIS2_PLACEMENT_3D('',#53291,#33000,#33001);
#28154=AXIS2_PLACEMENT_3D('',#53292,#33002,#33003);
#28155=AXIS2_PLACEMENT_3D('',#53293,#33004,#33005);
#28156=AXIS2_PLACEMENT_3D('',#53302,#33010,#33011);
#28157=AXIS2_PLACEMENT_3D('',#53304,#33012,#33013);
#28158=AXIS2_PLACEMENT_3D('',#53306,#33015,#33016);
#28159=AXIS2_PLACEMENT_3D('',#53310,#33019,#33020);
#28160=AXIS2_PLACEMENT_3D('',#53311,#33021,#33022);
#28161=AXIS2_PLACEMENT_3D('',#53312,#33023,#33024);
#28162=AXIS2_PLACEMENT_3D('',#53314,#33025,#33026);
#28163=AXIS2_PLACEMENT_3D('',#53315,#33027,#33028);
#28164=AXIS2_PLACEMENT_3D('',#53317,#33030,#33031);
#28165=AXIS2_PLACEMENT_3D('',#53319,#33032,#33033);
#28166=AXIS2_PLACEMENT_3D('',#53321,#33035,#33036);
#28167=AXIS2_PLACEMENT_3D('',#53322,#33037,#33038);
#28168=AXIS2_PLACEMENT_3D('',#53323,#33039,#33040);
#28169=AXIS2_PLACEMENT_3D('',#53324,#33041,#33042);
#28170=AXIS2_PLACEMENT_3D('',#53325,#33043,#33044);
#28171=AXIS2_PLACEMENT_3D('',#53326,#33045,#33046);
#28172=AXIS2_PLACEMENT_3D('',#53327,#33047,#33048);
#28173=AXIS2_PLACEMENT_3D('',#53328,#33049,#33050);
#28174=AXIS2_PLACEMENT_3D('',#53329,#33051,#33052);
#28175=AXIS2_PLACEMENT_3D('',#53330,#33053,#33054);
#28176=AXIS2_PLACEMENT_3D('',#53331,#33055,#33056);
#28177=AXIS2_PLACEMENT_3D('',#53332,#33057,#33058);
#28178=AXIS2_PLACEMENT_3D('',#53333,#33059,#33060);
#28179=AXIS2_PLACEMENT_3D('',#53334,#33061,#33062);
#28180=AXIS2_PLACEMENT_3D('',#53335,#33063,#33064);
#28181=AXIS2_PLACEMENT_3D('',#53336,#33065,#33066);
#28182=AXIS2_PLACEMENT_3D('',#53337,#33067,#33068);
#28183=AXIS2_PLACEMENT_3D('',#53339,#33070,#33071);
#28184=AXIS2_PLACEMENT_3D('',#53340,#33072,#33073);
#28185=AXIS2_PLACEMENT_3D('',#53341,#33074,#33075);
#28186=AXIS2_PLACEMENT_3D('',#53342,#33076,#33077);
#28187=AXIS2_PLACEMENT_3D('',#53343,#33078,#33079);
#28188=AXIS2_PLACEMENT_3D('',#53344,#33080,#33081);
#28189=AXIS2_PLACEMENT_3D('',#53345,#33082,#33083);
#28190=AXIS2_PLACEMENT_3D('',#53346,#33084,#33085);
#28191=AXIS2_PLACEMENT_3D('',#53347,#33086,#33087);
#28192=AXIS2_PLACEMENT_3D('',#53348,#33088,#33089);
#28193=AXIS2_PLACEMENT_3D('',#53349,#33090,#33091);
#28194=AXIS2_PLACEMENT_3D('',#53350,#33092,#33093);
#28195=AXIS2_PLACEMENT_3D('',#53351,#33094,#33095);
#28196=AXIS2_PLACEMENT_3D('',#53352,#33096,#33097);
#28197=AXIS2_PLACEMENT_3D('',#53353,#33098,#33099);
#28198=AXIS2_PLACEMENT_3D('',#53354,#33100,#33101);
#28199=AXIS2_PLACEMENT_3D('',#53355,#33102,#33103);
#28200=AXIS2_PLACEMENT_3D('',#53356,#33104,#33105);
#28201=AXIS2_PLACEMENT_3D('',#53357,#33106,#33107);
#28202=AXIS2_PLACEMENT_3D('',#53358,#33108,#33109);
#28203=AXIS2_PLACEMENT_3D('',#53359,#33110,#33111);
#28204=AXIS2_PLACEMENT_3D('',#53361,#33112,#33113);
#28205=AXIS2_PLACEMENT_3D('',#53363,#33115,#33116);
#28206=AXIS2_PLACEMENT_3D('',#53364,#33117,#33118);
#28207=AXIS2_PLACEMENT_3D('',#53365,#33119,#33120);
#28208=AXIS2_PLACEMENT_3D('',#53374,#33125,#33126);
#28209=AXIS2_PLACEMENT_3D('',#53378,#33128,#33129);
#28210=AXIS2_PLACEMENT_3D('',#53379,#33130,#33131);
#28211=AXIS2_PLACEMENT_3D('',#53380,#33132,#33133);
#28212=AXIS2_PLACEMENT_3D('',#53386,#33137,#33138);
#28213=AXIS2_PLACEMENT_3D('',#53387,#33139,#33140);
#28214=AXIS2_PLACEMENT_3D('',#53388,#33141,#33142);
#28215=AXIS2_PLACEMENT_3D('',#53389,#33143,#33144);
#28216=AXIS2_PLACEMENT_3D('',#53393,#33146,#33147);
#28217=AXIS2_PLACEMENT_3D('',#53395,#33149,#33150);
#28218=AXIS2_PLACEMENT_3D('',#53399,#33153,#33154);
#28219=AXIS2_PLACEMENT_3D('',#53400,#33155,#33156);
#28220=AXIS2_PLACEMENT_3D('',#53406,#33160,#33161);
#28221=AXIS2_PLACEMENT_3D('',#53410,#33163,#33164);
#28222=AXIS2_PLACEMENT_3D('',#53411,#33165,#33166);
#28223=AXIS2_PLACEMENT_3D('',#53412,#33167,#33168);
#28224=AXIS2_PLACEMENT_3D('',#53417,#33172,#33173);
#28225=AXIS2_PLACEMENT_3D('',#53418,#33174,#33175);
#28226=AXIS2_PLACEMENT_3D('',#53419,#33176,#33177);
#28227=AXIS2_PLACEMENT_3D('',#53421,#33179,#33180);
#28228=AXIS2_PLACEMENT_3D('',#53422,#33181,#33182);
#28229=AXIS2_PLACEMENT_3D('',#53423,#33183,#33184);
#28230=AXIS2_PLACEMENT_3D('',#53424,#33185,#33186);
#28231=AXIS2_PLACEMENT_3D('',#53446,#33188,#33189);
#28232=AXIS2_PLACEMENT_3D('',#53457,#33190,#33191);
#28233=AXIS2_PLACEMENT_3D('',#53541,#33193,#33194);
#28234=AXIS2_PLACEMENT_3D('',#53631,#33196,#33197);
#28235=AXIS2_PLACEMENT_3D('',#53721,#33199,#33200);
#28236=AXIS2_PLACEMENT_3D('',#53805,#33202,#33203);
#28237=AXIS2_PLACEMENT_3D('',#53895,#33205,#33206);
#28238=AXIS2_PLACEMENT_3D('',#53985,#33208,#33209);
#28239=AXIS2_PLACEMENT_3D('',#54069,#33211,#33212);
#28240=AXIS2_PLACEMENT_3D('',#54159,#33214,#33215);
#28241=AXIS2_PLACEMENT_3D('',#54249,#33217,#33218);
#28242=AXIS2_PLACEMENT_3D('',#54269,#33220,#33221);
#28243=AXIS2_PLACEMENT_3D('',#54281,#33222,#33223);
#28244=AXIS2_PLACEMENT_3D('',#54319,#33225,#33226);
#28245=AXIS2_PLACEMENT_3D('',#54356,#33228,#33229);
#28246=AXIS2_PLACEMENT_3D('',#54393,#33231,#33232);
#28247=AXIS2_PLACEMENT_3D('',#54431,#33234,#33235);
#28248=AXIS2_PLACEMENT_3D('',#54468,#33237,#33238);
#28249=AXIS2_PLACEMENT_3D('',#54505,#33240,#33241);
#28250=AXIS2_PLACEMENT_3D('',#54543,#33243,#33244);
#28251=AXIS2_PLACEMENT_3D('',#54580,#33246,#33247);
#28252=AXIS2_PLACEMENT_3D('',#54590,#33248,#33249);
#28253=AXIS2_PLACEMENT_3D('',#54598,#33250,#33251);
#28254=AXIS2_PLACEMENT_3D('',#54599,#33252,#33253);
#28255=AXIS2_PLACEMENT_3D('',#54608,#33254,#33255);
#28256=AXIS2_PLACEMENT_3D('',#54610,#33256,#33257);
#28257=AXIS2_PLACEMENT_3D('',#55297,#33258,#33259);
#28258=AXIS2_PLACEMENT_3D('',#55299,#33260,#33261);
#28259=AXIS2_PLACEMENT_3D('',#55300,#33262,#33263);
#28260=AXIS2_PLACEMENT_3D('',#55372,#33264,#33265);
#28261=AXIS2_PLACEMENT_3D('',#55373,#33266,#33267);
#28262=AXIS2_PLACEMENT_3D('',#55975,#33268,#33269);
#28263=AXIS2_PLACEMENT_3D('',#55995,#33271,#33272);
#28264=AXIS2_PLACEMENT_3D('',#55997,#33273,#33274);
#28265=AXIS2_PLACEMENT_3D('',#55998,#33275,#33276);
#28266=AXIS2_PLACEMENT_3D('',#56014,#33277,#33278);
#28267=AXIS2_PLACEMENT_3D('',#56016,#33279,#33280);
#28268=AXIS2_PLACEMENT_3D('',#56017,#33281,#33282);
#28269=AXIS2_PLACEMENT_3D('',#56018,#33283,#33284);
#28270=AXIS2_PLACEMENT_3D('',#56020,#33285,#33286);
#28271=AXIS2_PLACEMENT_3D('',#56022,#33287,#33288);
#28272=AXIS2_PLACEMENT_3D('',#56023,#33289,#33290);
#28273=AXIS2_PLACEMENT_3D('',#56025,#33292,#33293);
#28274=AXIS2_PLACEMENT_3D('',#56026,#33294,#33295);
#28275=AXIS2_PLACEMENT_3D('',#56028,#33296,#33297);
#28276=AXIS2_PLACEMENT_3D('',#56029,#33298,#33299);
#28277=AXIS2_PLACEMENT_3D('',#56031,#33301,#33302);
#28278=AXIS2_PLACEMENT_3D('',#56032,#33303,#33304);
#28279=AXIS2_PLACEMENT_3D('',#56033,#33305,#33306);
#28280=AXIS2_PLACEMENT_3D('',#56035,#33307,#33308);
#28281=AXIS2_PLACEMENT_3D('',#56036,#33309,#33310);
#28282=AXIS2_PLACEMENT_3D('',#56038,#33312,#33313);
#28283=AXIS2_PLACEMENT_3D('',#56039,#33314,#33315);
#28284=AXIS2_PLACEMENT_3D('',#56078,#33316,#33317);
#28285=AXIS2_PLACEMENT_3D('',#56080,#33318,#33319);
#28286=AXIS2_PLACEMENT_3D('',#56082,#33321,#33322);
#28287=AXIS2_PLACEMENT_3D('',#56084,#33323,#33324);
#28288=AXIS2_PLACEMENT_3D('',#56086,#33326,#33327);
#28289=AXIS2_PLACEMENT_3D('',#56087,#33328,#33329);
#28290=AXIS2_PLACEMENT_3D('',#56088,#33330,#33331);
#28291=AXIS2_PLACEMENT_3D('',#56104,#33333,#33334);
#28292=AXIS2_PLACEMENT_3D('',#56112,#33335,#33336);
#28293=AXIS2_PLACEMENT_3D('',#56160,#33338,#33339);
#28294=AXIS2_PLACEMENT_3D('',#56208,#33341,#33342);
#28295=AXIS2_PLACEMENT_3D('',#56256,#33344,#33345);
#28296=AXIS2_PLACEMENT_3D('',#56310,#33347,#33348);
#28297=AXIS2_PLACEMENT_3D('',#56358,#33350,#33351);
#28298=AXIS2_PLACEMENT_3D('',#56406,#33353,#33354);
#28299=AXIS2_PLACEMENT_3D('',#56460,#33356,#33357);
#28300=AXIS2_PLACEMENT_3D('',#56508,#33359,#33360);
#28301=AXIS2_PLACEMENT_3D('',#56556,#33362,#33363);
#28302=AXIS2_PLACEMENT_3D('',#56610,#33365,#33366);
#28303=AXIS2_PLACEMENT_3D('',#56658,#33368,#33369);
#28304=AXIS2_PLACEMENT_3D('',#56706,#33371,#33372);
#28305=AXIS2_PLACEMENT_3D('',#56754,#33374,#33375);
#28306=AXIS2_PLACEMENT_3D('',#56766,#33377,#33378);
#28307=AXIS2_PLACEMENT_3D('',#56771,#33379,#33380);
#28308=AXIS2_PLACEMENT_3D('',#56796,#33382,#33383);
#28309=AXIS2_PLACEMENT_3D('',#56820,#33385,#33386);
#28310=AXIS2_PLACEMENT_3D('',#56844,#33388,#33389);
#28311=AXIS2_PLACEMENT_3D('',#56869,#33391,#33392);
#28312=AXIS2_PLACEMENT_3D('',#56894,#33394,#33395);
#28313=AXIS2_PLACEMENT_3D('',#56918,#33397,#33398);
#28314=AXIS2_PLACEMENT_3D('',#56943,#33400,#33401);
#28315=AXIS2_PLACEMENT_3D('',#56968,#33403,#33404);
#28316=AXIS2_PLACEMENT_3D('',#56992,#33406,#33407);
#28317=AXIS2_PLACEMENT_3D('',#57017,#33409,#33410);
#28318=AXIS2_PLACEMENT_3D('',#57042,#33412,#33413);
#28319=AXIS2_PLACEMENT_3D('',#57066,#33415,#33416);
#28320=AXIS2_PLACEMENT_3D('',#57626,#33418,#33419);
#28321=AXIS2_PLACEMENT_3D('',#57628,#33420,#33421);
#28322=AXIS2_PLACEMENT_3D('',#57629,#33422,#33423);
#28323=AXIS2_PLACEMENT_3D('',#57692,#33424,#33425);
#28324=AXIS2_PLACEMENT_3D('',#57693,#33426,#33427);
#28325=AXIS2_PLACEMENT_3D('',#58155,#33428,#33429);
#28326=AXIS2_PLACEMENT_3D('',#58156,#33430,#33431);
#28327=AXIS2_PLACEMENT_3D('',#58158,#33432,#33433);
#28328=AXIS2_PLACEMENT_3D('',#58159,#33434,#33435);
#28329=AXIS2_PLACEMENT_3D('',#58168,#33440,#33441);
#28330=AXIS2_PLACEMENT_3D('',#58174,#33445,#33446);
#28331=AXIS2_PLACEMENT_3D('',#58180,#33450,#33451);
#28332=AXIS2_PLACEMENT_3D('',#58186,#33455,#33456);
#28333=AXIS2_PLACEMENT_3D('',#58192,#33460,#33461);
#28334=AXIS2_PLACEMENT_3D('',#58195,#33464,#33465);
#28335=AXIS2_PLACEMENT_3D('',#58196,#33466,#33467);
#28336=AXIS2_PLACEMENT_3D('',#58198,#33468,#33469);
#28337=AXIS2_PLACEMENT_3D('',#58199,#33470,#33471);
#28338=AXIS2_PLACEMENT_3D('',#58201,#33473,#33474);
#28339=AXIS2_PLACEMENT_3D('',#58202,#33475,#33476);
#28340=AXIS2_PLACEMENT_3D('',#58204,#33477,#33478);
#28341=AXIS2_PLACEMENT_3D('',#58206,#33480,#33481);
#28342=AXIS2_PLACEMENT_3D('',#58208,#33482,#33483);
#28343=AXIS2_PLACEMENT_3D('',#58210,#33485,#33486);
#28344=AXIS2_PLACEMENT_3D('',#58211,#33487,#33488);
#28345=AXIS2_PLACEMENT_3D('',#58212,#33489,#33490);
#28346=AXIS2_PLACEMENT_3D('',#58225,#33497,#33498);
#28347=AXIS2_PLACEMENT_3D('',#58231,#33502,#33503);
#28348=AXIS2_PLACEMENT_3D('',#58239,#33508,#33509);
#28349=AXIS2_PLACEMENT_3D('',#58247,#33514,#33515);
#28350=AXIS2_PLACEMENT_3D('',#58255,#33520,#33521);
#28351=AXIS2_PLACEMENT_3D('',#58265,#33527,#33528);
#28352=AXIS2_PLACEMENT_3D('',#58269,#33531,#33532);
#28353=AXIS2_PLACEMENT_3D('',#58275,#33536,#33537);
#28354=AXIS2_PLACEMENT_3D('',#58285,#33543,#33544);
#28355=AXIS2_PLACEMENT_3D('',#58291,#33548,#33549);
#28356=AXIS2_PLACEMENT_3D('',#58296,#33553,#33554);
#28357=AXIS2_PLACEMENT_3D('',#58301,#33558,#33559);
#28358=AXIS2_PLACEMENT_3D('',#58303,#33561,#33562);
#28359=AXIS2_PLACEMENT_3D('',#58305,#33564,#33565);
#28360=AXIS2_PLACEMENT_3D('',#58306,#33566,#33567);
#28361=AXIS2_PLACEMENT_3D('',#58308,#33569,#33570);
#28362=AXIS2_PLACEMENT_3D('',#58309,#33571,#33572);
#28363=AXIS2_PLACEMENT_3D('',#58310,#33573,#33574);
#28364=AXIS2_PLACEMENT_3D('',#58311,#33575,#33576);
#28365=AXIS2_PLACEMENT_3D('',#58333,#33578,#33579);
#28366=AXIS2_PLACEMENT_3D('',#58344,#33580,#33581);
#28367=AXIS2_PLACEMENT_3D('',#58428,#33583,#33584);
#28368=AXIS2_PLACEMENT_3D('',#58518,#33586,#33587);
#28369=AXIS2_PLACEMENT_3D('',#58608,#33589,#33590);
#28370=AXIS2_PLACEMENT_3D('',#58692,#33592,#33593);
#28371=AXIS2_PLACEMENT_3D('',#58782,#33595,#33596);
#28372=AXIS2_PLACEMENT_3D('',#58872,#33598,#33599);
#28373=AXIS2_PLACEMENT_3D('',#58956,#33601,#33602);
#28374=AXIS2_PLACEMENT_3D('',#59046,#33604,#33605);
#28375=AXIS2_PLACEMENT_3D('',#59136,#33607,#33608);
#28376=AXIS2_PLACEMENT_3D('',#59220,#33610,#33611);
#28377=AXIS2_PLACEMENT_3D('',#59310,#33613,#33614);
#28378=AXIS2_PLACEMENT_3D('',#59400,#33616,#33617);
#28379=AXIS2_PLACEMENT_3D('',#59484,#33619,#33620);
#28380=AXIS2_PLACEMENT_3D('',#59574,#33622,#33623);
#28381=AXIS2_PLACEMENT_3D('',#59664,#33625,#33626);
#28382=AXIS2_PLACEMENT_3D('',#59748,#33628,#33629);
#28383=AXIS2_PLACEMENT_3D('',#59838,#33631,#33632);
#28384=AXIS2_PLACEMENT_3D('',#59925,#33634,#33635);
#28385=AXIS2_PLACEMENT_3D('',#60012,#33637,#33638);
#28386=AXIS2_PLACEMENT_3D('',#60022,#33640,#33641);
#28387=AXIS2_PLACEMENT_3D('',#60023,#33642,#33643);
#28388=AXIS2_PLACEMENT_3D('',#60045,#33645,#33646);
#28389=AXIS2_PLACEMENT_3D('',#60061,#33647,#33648);
#28390=AXIS2_PLACEMENT_3D('',#60097,#33650,#33651);
#28391=AXIS2_PLACEMENT_3D('',#60135,#33653,#33654);
#28392=AXIS2_PLACEMENT_3D('',#60172,#33656,#33657);
#28393=AXIS2_PLACEMENT_3D('',#60209,#33659,#33660);
#28394=AXIS2_PLACEMENT_3D('',#60247,#33662,#33663);
#28395=AXIS2_PLACEMENT_3D('',#60284,#33665,#33666);
#28396=AXIS2_PLACEMENT_3D('',#60321,#33668,#33669);
#28397=AXIS2_PLACEMENT_3D('',#60359,#33671,#33672);
#28398=AXIS2_PLACEMENT_3D('',#60396,#33674,#33675);
#28399=AXIS2_PLACEMENT_3D('',#60433,#33677,#33678);
#28400=AXIS2_PLACEMENT_3D('',#60471,#33680,#33681);
#28401=AXIS2_PLACEMENT_3D('',#60508,#33683,#33684);
#28402=AXIS2_PLACEMENT_3D('',#60545,#33686,#33687);
#28403=AXIS2_PLACEMENT_3D('',#60583,#33689,#33690);
#28404=AXIS2_PLACEMENT_3D('',#60620,#33692,#33693);
#28405=AXIS2_PLACEMENT_3D('',#60657,#33695,#33696);
#28406=AXIS2_PLACEMENT_3D('',#60695,#33698,#33699);
#28407=AXIS2_PLACEMENT_3D('',#61950,#33701,#33702);
#28408=AXIS2_PLACEMENT_3D('',#61952,#33703,#33704);
#28409=AXIS2_PLACEMENT_3D('',#61953,#33705,#33706);
#28410=AXIS2_PLACEMENT_3D('',#62031,#33707,#33708);
#28411=AXIS2_PLACEMENT_3D('',#62032,#33709,#33710);
#28412=AXIS2_PLACEMENT_3D('',#63166,#33711,#33712);
#28413=AXIS2_PLACEMENT_3D('',#63190,#33714,#33715);
#28414=AXIS2_PLACEMENT_3D('',#63198,#33716,#33717);
#28415=AXIS2_PLACEMENT_3D('',#63204,#33721,#33722);
#28416=AXIS2_PLACEMENT_3D('',#63208,#33725,#33726);
#28417=AXIS2_PLACEMENT_3D('',#63212,#33729,#33730);
#28418=AXIS2_PLACEMENT_3D('',#63219,#33734,#33735);
#28419=AXIS2_PLACEMENT_3D('',#63220,#33736,#33737);
#28420=AXIS2_PLACEMENT_3D('',#63222,#33739,#33740);
#28421=AXIS2_PLACEMENT_3D('',#63224,#33742,#33743);
#28422=AXIS2_PLACEMENT_3D('',#63225,#33744,#33745);
#28423=AXIS2_PLACEMENT_3D('',#63226,#33746,#33747);
#28424=AXIS2_PLACEMENT_3D('',#63228,#33748,#33749);
#28425=AXIS2_PLACEMENT_3D('',#63229,#33750,#33751);
#28426=AXIS2_PLACEMENT_3D('',#63231,#33753,#33754);
#28427=AXIS2_PLACEMENT_3D('',#63232,#33755,#33756);
#28428=AXIS2_PLACEMENT_3D('',#63233,#33757,#33758);
#28429=AXIS2_PLACEMENT_3D('',#63235,#33759,#33760);
#28430=AXIS2_PLACEMENT_3D('',#63236,#33761,#33762);
#28431=AXIS2_PLACEMENT_3D('',#63238,#33764,#33765);
#28432=AXIS2_PLACEMENT_3D('',#63239,#33766,#33767);
#28433=AXIS2_PLACEMENT_3D('',#63241,#33768,#33769);
#28434=AXIS2_PLACEMENT_3D('',#63244,#33771,#33772);
#28435=AXIS2_PLACEMENT_3D('',#63245,#33773,#33774);
#28436=AXIS2_PLACEMENT_3D('',#63248,#33776,#33777);
#28437=AXIS2_PLACEMENT_3D('',#63249,#33778,#33779);
#28438=AXIS2_PLACEMENT_3D('',#63254,#33781,#33782);
#28439=AXIS2_PLACEMENT_3D('',#63258,#33784,#33785);
#28440=AXIS2_PLACEMENT_3D('',#63262,#33787,#33788);
#28441=AXIS2_PLACEMENT_3D('',#63265,#33790,#33791);
#28442=AXIS2_PLACEMENT_3D('',#63266,#33792,#33793);
#28443=AXIS2_PLACEMENT_3D('',#63269,#33795,#33796);
#28444=AXIS2_PLACEMENT_3D('',#63270,#33797,#33798);
#28445=AXIS2_PLACEMENT_3D('',#63272,#33799,#33800);
#28446=AXIS2_PLACEMENT_3D('',#63274,#33802,#33803);
#28447=AXIS2_PLACEMENT_3D('',#63276,#33804,#33805);
#28448=AXIS2_PLACEMENT_3D('',#63278,#33807,#33808);
#28449=AXIS2_PLACEMENT_3D('',#63280,#33809,#33810);
#28450=AXIS2_PLACEMENT_3D('',#63282,#33812,#33813);
#28451=AXIS2_PLACEMENT_3D('',#63285,#33815,#33816);
#28452=AXIS2_PLACEMENT_3D('',#63286,#33817,#33818);
#28453=AXIS2_PLACEMENT_3D('',#63291,#33820,#33821);
#28454=AXIS2_PLACEMENT_3D('',#63295,#33823,#33824);
#28455=AXIS2_PLACEMENT_3D('',#63299,#33826,#33827);
#28456=AXIS2_PLACEMENT_3D('',#63302,#33829,#33830);
#28457=AXIS2_PLACEMENT_3D('',#63303,#33831,#33832);
#28458=AXIS2_PLACEMENT_3D('',#63308,#33834,#33835);
#28459=AXIS2_PLACEMENT_3D('',#63311,#33837,#33838);
#28460=AXIS2_PLACEMENT_3D('',#63312,#33839,#33840);
#28461=AXIS2_PLACEMENT_3D('',#63318,#33844,#33845);
#28462=AXIS2_PLACEMENT_3D('',#63322,#33847,#33848);
#28463=AXIS2_PLACEMENT_3D('',#63323,#33849,#33850);
#28464=AXIS2_PLACEMENT_3D('',#63324,#33851,#33852);
#28465=AXIS2_PLACEMENT_3D('',#63330,#33856,#33857);
#28466=AXIS2_PLACEMENT_3D('',#63334,#33859,#33860);
#28467=AXIS2_PLACEMENT_3D('',#63335,#33861,#33862);
#28468=AXIS2_PLACEMENT_3D('',#63336,#33863,#33864);
#28469=AXIS2_PLACEMENT_3D('',#63342,#33868,#33869);
#28470=AXIS2_PLACEMENT_3D('',#63346,#33871,#33872);
#28471=AXIS2_PLACEMENT_3D('',#63347,#33873,#33874);
#28472=AXIS2_PLACEMENT_3D('',#63348,#33875,#33876);
#28473=AXIS2_PLACEMENT_3D('',#63351,#33879,#33880);
#28474=AXIS2_PLACEMENT_3D('',#63357,#33884,#33885);
#28475=AXIS2_PLACEMENT_3D('',#63360,#33887,#33888);
#28476=AXIS2_PLACEMENT_3D('',#63361,#33889,#33890);
#28477=AXIS2_PLACEMENT_3D('',#63365,#33893,#33894);
#28478=AXIS2_PLACEMENT_3D('',#63368,#33896,#33897);
#28479=AXIS2_PLACEMENT_3D('',#63369,#33898,#33899);
#28480=AXIS2_PLACEMENT_3D('',#63372,#33902,#33903);
#28481=AXIS2_PLACEMENT_3D('',#63374,#33905,#33906);
#28482=AXIS2_PLACEMENT_3D('',#63376,#33908,#33909);
#28483=AXIS2_PLACEMENT_3D('',#63378,#33911,#33912);
#28484=AXIS2_PLACEMENT_3D('',#63384,#33916,#33917);
#28485=AXIS2_PLACEMENT_3D('',#63387,#33919,#33920);
#28486=AXIS2_PLACEMENT_3D('',#63388,#33921,#33922);
#28487=AXIS2_PLACEMENT_3D('',#63392,#33925,#33926);
#28488=AXIS2_PLACEMENT_3D('',#63395,#33928,#33929);
#28489=AXIS2_PLACEMENT_3D('',#63396,#33930,#33931);
#28490=AXIS2_PLACEMENT_3D('',#63400,#33934,#33935);
#28491=AXIS2_PLACEMENT_3D('',#63403,#33937,#33938);
#28492=AXIS2_PLACEMENT_3D('',#63404,#33939,#33940);
#28493=AXIS2_PLACEMENT_3D('',#63408,#33943,#33944);
#28494=AXIS2_PLACEMENT_3D('',#63409,#33945,#33946);
#28495=AXIS2_PLACEMENT_3D('',#63410,#33947,#33948);
#28496=AXIS2_PLACEMENT_3D('',#63414,#33950,#33951);
#28497=AXIS2_PLACEMENT_3D('',#63416,#33953,#33954);
#28498=AXIS2_PLACEMENT_3D('',#63420,#33957,#33958);
#28499=AXIS2_PLACEMENT_3D('',#63423,#33960,#33961);
#28500=AXIS2_PLACEMENT_3D('',#63424,#33962,#33963);
#28501=AXIS2_PLACEMENT_3D('',#63428,#33966,#33967);
#28502=AXIS2_PLACEMENT_3D('',#63431,#33970,#33971);
#28503=AXIS2_PLACEMENT_3D('',#63433,#33973,#33974);
#28504=AXIS2_PLACEMENT_3D('',#63435,#33976,#33977);
#28505=AXIS2_PLACEMENT_3D('',#63437,#33979,#33980);
#28506=AXIS2_PLACEMENT_3D('',#63443,#33984,#33985);
#28507=AXIS2_PLACEMENT_3D('',#63447,#33987,#33988);
#28508=AXIS2_PLACEMENT_3D('',#63448,#33989,#33990);
#28509=AXIS2_PLACEMENT_3D('',#63449,#33991,#33992);
#28510=AXIS2_PLACEMENT_3D('',#63455,#33996,#33997);
#28511=AXIS2_PLACEMENT_3D('',#63456,#33998,#33999);
#28512=AXIS2_PLACEMENT_3D('',#63457,#34000,#34001);
#28513=AXIS2_PLACEMENT_3D('',#63458,#34002,#34003);
#28514=AXIS2_PLACEMENT_3D('',#63461,#34006,#34007);
#28515=AXIS2_PLACEMENT_3D('',#63463,#34009,#34010);
#28516=AXIS2_PLACEMENT_3D('',#63464,#34011,#34012);
#28517=AXIS2_PLACEMENT_3D('',#63465,#34013,#34014);
#28518=AXIS2_PLACEMENT_3D('',#63468,#34017,#34018);
#28519=AXIS2_PLACEMENT_3D('',#63469,#34019,#34020);
#28520=AXIS2_PLACEMENT_3D('',#63471,#34022,#34023);
#28521=AXIS2_PLACEMENT_3D('',#63472,#34024,#34025);
#28522=AXIS2_PLACEMENT_3D('',#63475,#34028,#34029);
#28523=AXIS2_PLACEMENT_3D('',#63477,#34031,#34032);
#28524=AXIS2_PLACEMENT_3D('',#63478,#34033,#34034);
#28525=AXIS2_PLACEMENT_3D('',#63479,#34035,#34036);
#28526=AXIS2_PLACEMENT_3D('',#63480,#34037,#34038);
#28527=AXIS2_PLACEMENT_3D('',#63482,#34039,#34040);
#28528=AXIS2_PLACEMENT_3D('',#63485,#34042,#34043);
#28529=AXIS2_PLACEMENT_3D('',#63486,#34044,#34045);
#28530=AXIS2_PLACEMENT_3D('',#63488,#34046,#34047);
#28531=AXIS2_PLACEMENT_3D('',#63490,#34049,#34050);
#28532=AXIS2_PLACEMENT_3D('',#63493,#34052,#34053);
#28533=AXIS2_PLACEMENT_3D('',#63494,#34054,#34055);
#28534=AXIS2_PLACEMENT_3D('',#63496,#34056,#34057);
#28535=AXIS2_PLACEMENT_3D('',#63499,#34059,#34060);
#28536=AXIS2_PLACEMENT_3D('',#63500,#34061,#34062);
#28537=AXIS2_PLACEMENT_3D('',#63502,#34063,#34064);
#28538=AXIS2_PLACEMENT_3D('',#63503,#34065,#34066);
#28539=AXIS2_PLACEMENT_3D('',#63505,#34067,#34068);
#28540=AXIS2_PLACEMENT_3D('',#63507,#34070,#34071);
#28541=AXIS2_PLACEMENT_3D('',#63509,#34072,#34073);
#28542=AXIS2_PLACEMENT_3D('',#63511,#34075,#34076);
#28543=AXIS2_PLACEMENT_3D('',#63512,#34077,#34078);
#28544=AXIS2_PLACEMENT_3D('',#63514,#34079,#34080);
#28545=AXIS2_PLACEMENT_3D('',#63516,#34082,#34083);
#28546=AXIS2_PLACEMENT_3D('',#63518,#34084,#34085);
#28547=AXIS2_PLACEMENT_3D('',#63519,#34086,#34087);
#28548=AXIS2_PLACEMENT_3D('',#63521,#34088,#34089);
#28549=AXIS2_PLACEMENT_3D('',#63523,#34091,#34092);
#28550=AXIS2_PLACEMENT_3D('',#63525,#34093,#34094);
#28551=AXIS2_PLACEMENT_3D('',#63527,#34096,#34097);
#28552=AXIS2_PLACEMENT_3D('',#63529,#34098,#34099);
#28553=AXIS2_PLACEMENT_3D('',#63530,#34100,#34101);
#28554=AXIS2_PLACEMENT_3D('',#63533,#34103,#34104);
#28555=AXIS2_PLACEMENT_3D('',#63534,#34105,#34106);
#28556=AXIS2_PLACEMENT_3D('',#63536,#34107,#34108);
#28557=AXIS2_PLACEMENT_3D('',#63537,#34109,#34110);
#28558=AXIS2_PLACEMENT_3D('',#63540,#34112,#34113);
#28559=AXIS2_PLACEMENT_3D('',#63541,#34114,#34115);
#28560=AXIS2_PLACEMENT_3D('',#63542,#34116,#34117);
#28561=AXIS2_PLACEMENT_3D('',#63543,#34118,#34119);
#28562=AXIS2_PLACEMENT_3D('',#63565,#34121,#34122);
#28563=AXIS2_PLACEMENT_3D('',#63576,#34123,#34124);
#28564=AXIS2_PLACEMENT_3D('',#63660,#34126,#34127);
#28565=AXIS2_PLACEMENT_3D('',#63750,#34129,#34130);
#28566=AXIS2_PLACEMENT_3D('',#63834,#34132,#34133);
#28567=AXIS2_PLACEMENT_3D('',#63924,#34135,#34136);
#28568=AXIS2_PLACEMENT_3D('',#64014,#34138,#34139);
#28569=AXIS2_PLACEMENT_3D('',#64098,#34141,#34142);
#28570=AXIS2_PLACEMENT_3D('',#64188,#34144,#34145);
#28571=AXIS2_PLACEMENT_3D('',#64272,#34147,#34148);
#28572=AXIS2_PLACEMENT_3D('',#64362,#34150,#34151);
#28573=AXIS2_PLACEMENT_3D('',#64452,#34153,#34154);
#28574=AXIS2_PLACEMENT_3D('',#64536,#34156,#34157);
#28575=AXIS2_PLACEMENT_3D('',#64626,#34159,#34160);
#28576=AXIS2_PLACEMENT_3D('',#64710,#34162,#34163);
#28577=AXIS2_PLACEMENT_3D('',#64800,#34165,#34166);
#28578=AXIS2_PLACEMENT_3D('',#64884,#34168,#34169);
#28579=AXIS2_PLACEMENT_3D('',#64974,#34171,#34172);
#28580=AXIS2_PLACEMENT_3D('',#65064,#34174,#34175);
#28581=AXIS2_PLACEMENT_3D('',#65148,#34177,#34178);
#28582=AXIS2_PLACEMENT_3D('',#65238,#34180,#34181);
#28583=AXIS2_PLACEMENT_3D('',#65322,#34183,#34184);
#28584=AXIS2_PLACEMENT_3D('',#65412,#34186,#34187);
#28585=AXIS2_PLACEMENT_3D('',#65499,#34189,#34190);
#28586=AXIS2_PLACEMENT_3D('',#65520,#34192,#34193);
#28587=AXIS2_PLACEMENT_3D('',#65533,#34194,#34195);
#28588=AXIS2_PLACEMENT_3D('',#65571,#34197,#34198);
#28589=AXIS2_PLACEMENT_3D('',#65608,#34200,#34201);
#28590=AXIS2_PLACEMENT_3D('',#65645,#34203,#34204);
#28591=AXIS2_PLACEMENT_3D('',#65682,#34206,#34207);
#28592=AXIS2_PLACEMENT_3D('',#65719,#34209,#34210);
#28593=AXIS2_PLACEMENT_3D('',#65757,#34212,#34213);
#28594=AXIS2_PLACEMENT_3D('',#65794,#34215,#34216);
#28595=AXIS2_PLACEMENT_3D('',#65831,#34218,#34219);
#28596=AXIS2_PLACEMENT_3D('',#65868,#34221,#34222);
#28597=AXIS2_PLACEMENT_3D('',#65905,#34224,#34225);
#28598=AXIS2_PLACEMENT_3D('',#65942,#34227,#34228);
#28599=AXIS2_PLACEMENT_3D('',#65979,#34230,#34231);
#28600=AXIS2_PLACEMENT_3D('',#66017,#34233,#34234);
#28601=AXIS2_PLACEMENT_3D('',#66054,#34236,#34237);
#28602=AXIS2_PLACEMENT_3D('',#66091,#34239,#34240);
#28603=AXIS2_PLACEMENT_3D('',#66128,#34242,#34243);
#28604=AXIS2_PLACEMENT_3D('',#66165,#34245,#34246);
#28605=AXIS2_PLACEMENT_3D('',#66203,#34248,#34249);
#28606=AXIS2_PLACEMENT_3D('',#66240,#34251,#34252);
#28607=AXIS2_PLACEMENT_3D('',#66277,#34254,#34255);
#28608=AXIS2_PLACEMENT_3D('',#67653,#34257,#34258);
#28609=AXIS2_PLACEMENT_3D('',#67655,#34259,#34260);
#28610=AXIS2_PLACEMENT_3D('',#67656,#34261,#34262);
#28611=AXIS2_PLACEMENT_3D('',#67728,#34263,#34264);
#28612=AXIS2_PLACEMENT_3D('',#67729,#34265,#34266);
#28613=AXIS2_PLACEMENT_3D('',#68993,#34267,#34268);
#28614=AXIS2_PLACEMENT_3D('',#69017,#34270,#34271);
#28615=AXIS2_PLACEMENT_3D('',#69025,#34272,#34273);
#28616=AXIS2_PLACEMENT_3D('',#69031,#34277,#34278);
#28617=AXIS2_PLACEMENT_3D('',#69035,#34281,#34282);
#28618=AXIS2_PLACEMENT_3D('',#69039,#34285,#34286);
#28619=AXIS2_PLACEMENT_3D('',#69046,#34290,#34291);
#28620=AXIS2_PLACEMENT_3D('',#69047,#34292,#34293);
#28621=AXIS2_PLACEMENT_3D('',#69049,#34295,#34296);
#28622=AXIS2_PLACEMENT_3D('',#69051,#34298,#34299);
#28623=AXIS2_PLACEMENT_3D('',#69052,#34300,#34301);
#28624=AXIS2_PLACEMENT_3D('',#69053,#34302,#34303);
#28625=AXIS2_PLACEMENT_3D('',#69055,#34304,#34305);
#28626=AXIS2_PLACEMENT_3D('',#69056,#34306,#34307);
#28627=AXIS2_PLACEMENT_3D('',#69058,#34309,#34310);
#28628=AXIS2_PLACEMENT_3D('',#69059,#34311,#34312);
#28629=AXIS2_PLACEMENT_3D('',#69060,#34313,#34314);
#28630=AXIS2_PLACEMENT_3D('',#69062,#34315,#34316);
#28631=AXIS2_PLACEMENT_3D('',#69063,#34317,#34318);
#28632=AXIS2_PLACEMENT_3D('',#69065,#34320,#34321);
#28633=AXIS2_PLACEMENT_3D('',#69066,#34322,#34323);
#28634=AXIS2_PLACEMENT_3D('',#69082,#34325,#34326);
#28635=AXIS2_PLACEMENT_3D('',#69093,#34327,#34328);
#28636=AXIS2_PLACEMENT_3D('',#69141,#34330,#34331);
#28637=AXIS2_PLACEMENT_3D('',#69189,#34333,#34334);
#28638=AXIS2_PLACEMENT_3D('',#69237,#34336,#34337);
#28639=AXIS2_PLACEMENT_3D('',#69291,#34339,#34340);
#28640=AXIS2_PLACEMENT_3D('',#69339,#34342,#34343);
#28641=AXIS2_PLACEMENT_3D('',#69387,#34345,#34346);
#28642=AXIS2_PLACEMENT_3D('',#69441,#34348,#34349);
#28643=AXIS2_PLACEMENT_3D('',#69489,#34351,#34352);
#28644=AXIS2_PLACEMENT_3D('',#69537,#34354,#34355);
#28645=AXIS2_PLACEMENT_3D('',#69588,#34357,#34358);
#28646=AXIS2_PLACEMENT_3D('',#69639,#34360,#34361);
#28647=AXIS2_PLACEMENT_3D('',#69687,#34363,#34364);
#28648=AXIS2_PLACEMENT_3D('',#69735,#34366,#34367);
#28649=AXIS2_PLACEMENT_3D('',#69789,#34369,#34370);
#28650=AXIS2_PLACEMENT_3D('',#69837,#34372,#34373);
#28651=AXIS2_PLACEMENT_3D('',#69885,#34375,#34376);
#28652=AXIS2_PLACEMENT_3D('',#69939,#34378,#34379);
#28653=AXIS2_PLACEMENT_3D('',#69987,#34381,#34382);
#28654=AXIS2_PLACEMENT_3D('',#70035,#34384,#34385);
#28655=AXIS2_PLACEMENT_3D('',#70083,#34387,#34388);
#28656=AXIS2_PLACEMENT_3D('',#70137,#34390,#34391);
#28657=AXIS2_PLACEMENT_3D('',#70185,#34393,#34394);
#28658=AXIS2_PLACEMENT_3D('',#70196,#34396,#34397);
#28659=AXIS2_PLACEMENT_3D('',#70201,#34398,#34399);
#28660=AXIS2_PLACEMENT_3D('',#70226,#34401,#34402);
#28661=AXIS2_PLACEMENT_3D('',#70251,#34404,#34405);
#28662=AXIS2_PLACEMENT_3D('',#70276,#34407,#34408);
#28663=AXIS2_PLACEMENT_3D('',#70300,#34410,#34411);
#28664=AXIS2_PLACEMENT_3D('',#70324,#34413,#34414);
#28665=AXIS2_PLACEMENT_3D('',#70349,#34416,#34417);
#28666=AXIS2_PLACEMENT_3D('',#70374,#34419,#34420);
#28667=AXIS2_PLACEMENT_3D('',#70398,#34422,#34423);
#28668=AXIS2_PLACEMENT_3D('',#70423,#34425,#34426);
#28669=AXIS2_PLACEMENT_3D('',#70448,#34428,#34429);
#28670=AXIS2_PLACEMENT_3D('',#70472,#34431,#34432);
#28671=AXIS2_PLACEMENT_3D('',#70497,#34434,#34435);
#28672=AXIS2_PLACEMENT_3D('',#70521,#34437,#34438);
#28673=AXIS2_PLACEMENT_3D('',#70546,#34440,#34441);
#28674=AXIS2_PLACEMENT_3D('',#70570,#34443,#34444);
#28675=AXIS2_PLACEMENT_3D('',#70595,#34446,#34447);
#28676=AXIS2_PLACEMENT_3D('',#70620,#34449,#34450);
#28677=AXIS2_PLACEMENT_3D('',#70644,#34452,#34453);
#28678=AXIS2_PLACEMENT_3D('',#70669,#34455,#34456);
#28679=AXIS2_PLACEMENT_3D('',#70694,#34458,#34459);
#28680=AXIS2_PLACEMENT_3D('',#70718,#34461,#34462);
#28681=AXIS2_PLACEMENT_3D('',#70742,#34464,#34465);
#28682=AXIS2_PLACEMENT_3D('',#70812,#34466,#34467);
#28683=AXIS2_PLACEMENT_3D('',#70814,#34468,#34469);
#28684=AXIS2_PLACEMENT_3D('',#71579,#34470,#34471);
#28685=AXIS2_PLACEMENT_3D('',#71581,#34472,#34473);
#28686=AXIS2_PLACEMENT_3D('',#71582,#34474,#34475);
#28687=AXIS2_PLACEMENT_3D('',#71651,#34476,#34477);
#28688=AXIS2_PLACEMENT_3D('',#71652,#34478,#34479);
#28689=AXIS2_PLACEMENT_3D('',#72282,#34480,#34481);
#28690=AXIS2_PLACEMENT_3D('',#72284,#34482,#34483);
#28691=AXIS2_PLACEMENT_3D('',#72285,#34484,#34485);
#28692=AXIS2_PLACEMENT_3D('',#72286,#34486,#34487);
#28693=AXIS2_PLACEMENT_3D('',#72287,#34488,#34489);
#28694=AXIS2_PLACEMENT_3D('',#72288,#34490,#34491);
#28695=AXIS2_PLACEMENT_3D('',#72290,#34492,#34493);
#28696=AXIS2_PLACEMENT_3D('',#72291,#34494,#34495);
#28697=AXIS2_PLACEMENT_3D('',#72295,#34497,#34498);
#28698=AXIS2_PLACEMENT_3D('',#72296,#34499,#34500);
#28699=AXIS2_PLACEMENT_3D('',#72299,#34502,#34503);
#28700=AXIS2_PLACEMENT_3D('',#72300,#34504,#34505);
#28701=AXIS2_PLACEMENT_3D('',#72303,#34507,#34508);
#28702=AXIS2_PLACEMENT_3D('',#72304,#34509,#34510);
#28703=AXIS2_PLACEMENT_3D('',#72307,#34512,#34513);
#28704=AXIS2_PLACEMENT_3D('',#72308,#34514,#34515);
#28705=AXIS2_PLACEMENT_3D('',#72311,#34517,#34518);
#28706=AXIS2_PLACEMENT_3D('',#72312,#34519,#34520);
#28707=AXIS2_PLACEMENT_3D('',#72314,#34522,#34523);
#28708=AXIS2_PLACEMENT_3D('',#72315,#34524,#34525);
#28709=AXIS2_PLACEMENT_3D('',#72318,#34527,#34528);
#28710=AXIS2_PLACEMENT_3D('',#72324,#34532,#34533);
#28711=AXIS2_PLACEMENT_3D('',#72328,#34536,#34537);
#28712=AXIS2_PLACEMENT_3D('',#72332,#34540,#34541);
#28713=AXIS2_PLACEMENT_3D('',#72336,#34544,#34545);
#28714=AXIS2_PLACEMENT_3D('',#72340,#34548,#34549);
#28715=AXIS2_PLACEMENT_3D('',#72342,#34551,#34552);
#28716=AXIS2_PLACEMENT_3D('',#72351,#34557,#34558);
#28717=AXIS2_PLACEMENT_3D('',#72353,#34559,#34560);
#28718=AXIS2_PLACEMENT_3D('',#72355,#34562,#34563);
#28719=AXIS2_PLACEMENT_3D('',#72359,#34566,#34567);
#28720=AXIS2_PLACEMENT_3D('',#72360,#34568,#34569);
#28721=AXIS2_PLACEMENT_3D('',#72361,#34570,#34571);
#28722=AXIS2_PLACEMENT_3D('',#72370,#34576,#34577);
#28723=AXIS2_PLACEMENT_3D('',#72372,#34578,#34579);
#28724=AXIS2_PLACEMENT_3D('',#72374,#34581,#34582);
#28725=AXIS2_PLACEMENT_3D('',#72378,#34585,#34586);
#28726=AXIS2_PLACEMENT_3D('',#72379,#34587,#34588);
#28727=AXIS2_PLACEMENT_3D('',#72380,#34589,#34590);
#28728=AXIS2_PLACEMENT_3D('',#72389,#34595,#34596);
#28729=AXIS2_PLACEMENT_3D('',#72391,#34597,#34598);
#28730=AXIS2_PLACEMENT_3D('',#72393,#34600,#34601);
#28731=AXIS2_PLACEMENT_3D('',#72397,#34604,#34605);
#28732=AXIS2_PLACEMENT_3D('',#72398,#34606,#34607);
#28733=AXIS2_PLACEMENT_3D('',#72399,#34608,#34609);
#28734=AXIS2_PLACEMENT_3D('',#72408,#34614,#34615);
#28735=AXIS2_PLACEMENT_3D('',#72410,#34616,#34617);
#28736=AXIS2_PLACEMENT_3D('',#72412,#34619,#34620);
#28737=AXIS2_PLACEMENT_3D('',#72416,#34623,#34624);
#28738=AXIS2_PLACEMENT_3D('',#72417,#34625,#34626);
#28739=AXIS2_PLACEMENT_3D('',#72418,#34627,#34628);
#28740=AXIS2_PLACEMENT_3D('',#72427,#34633,#34634);
#28741=AXIS2_PLACEMENT_3D('',#72429,#34635,#34636);
#28742=AXIS2_PLACEMENT_3D('',#72431,#34638,#34639);
#28743=AXIS2_PLACEMENT_3D('',#72435,#34642,#34643);
#28744=AXIS2_PLACEMENT_3D('',#72436,#34644,#34645);
#28745=AXIS2_PLACEMENT_3D('',#72437,#34646,#34647);
#28746=AXIS2_PLACEMENT_3D('',#72446,#34652,#34653);
#28747=AXIS2_PLACEMENT_3D('',#72448,#34654,#34655);
#28748=AXIS2_PLACEMENT_3D('',#72450,#34657,#34658);
#28749=AXIS2_PLACEMENT_3D('',#72454,#34661,#34662);
#28750=AXIS2_PLACEMENT_3D('',#72455,#34663,#34664);
#28751=AXIS2_PLACEMENT_3D('',#72456,#34665,#34666);
#28752=AXIS2_PLACEMENT_3D('',#72465,#34671,#34672);
#28753=AXIS2_PLACEMENT_3D('',#72467,#34673,#34674);
#28754=AXIS2_PLACEMENT_3D('',#72469,#34676,#34677);
#28755=AXIS2_PLACEMENT_3D('',#72473,#34680,#34681);
#28756=AXIS2_PLACEMENT_3D('',#72474,#34682,#34683);
#28757=AXIS2_PLACEMENT_3D('',#72475,#34684,#34685);
#28758=AXIS2_PLACEMENT_3D('',#72484,#34690,#34691);
#28759=AXIS2_PLACEMENT_3D('',#72486,#34692,#34693);
#28760=AXIS2_PLACEMENT_3D('',#72488,#34695,#34696);
#28761=AXIS2_PLACEMENT_3D('',#72492,#34699,#34700);
#28762=AXIS2_PLACEMENT_3D('',#72493,#34701,#34702);
#28763=AXIS2_PLACEMENT_3D('',#72494,#34703,#34704);
#28764=AXIS2_PLACEMENT_3D('',#72503,#34709,#34710);
#28765=AXIS2_PLACEMENT_3D('',#72505,#34711,#34712);
#28766=AXIS2_PLACEMENT_3D('',#72508,#34714,#34715);
#28767=AXIS2_PLACEMENT_3D('',#72509,#34716,#34717);
#28768=AXIS2_PLACEMENT_3D('',#72513,#34720,#34721);
#28769=AXIS2_PLACEMENT_3D('',#72515,#34722,#34723);
#28770=AXIS2_PLACEMENT_3D('',#72516,#34724,#34725);
#28771=AXIS2_PLACEMENT_3D('',#72517,#34726,#34727);
#28772=AXIS2_PLACEMENT_3D('',#72526,#34732,#34733);
#28773=AXIS2_PLACEMENT_3D('',#72528,#34734,#34735);
#28774=AXIS2_PLACEMENT_3D('',#72530,#34737,#34738);
#28775=AXIS2_PLACEMENT_3D('',#72534,#34741,#34742);
#28776=AXIS2_PLACEMENT_3D('',#72535,#34743,#34744);
#28777=AXIS2_PLACEMENT_3D('',#72536,#34745,#34746);
#28778=AXIS2_PLACEMENT_3D('',#72545,#34751,#34752);
#28779=AXIS2_PLACEMENT_3D('',#72547,#34753,#34754);
#28780=AXIS2_PLACEMENT_3D('',#72549,#34756,#34757);
#28781=AXIS2_PLACEMENT_3D('',#72553,#34760,#34761);
#28782=AXIS2_PLACEMENT_3D('',#72554,#34762,#34763);
#28783=AXIS2_PLACEMENT_3D('',#72555,#34764,#34765);
#28784=AXIS2_PLACEMENT_3D('',#72564,#34770,#34771);
#28785=AXIS2_PLACEMENT_3D('',#72566,#34772,#34773);
#28786=AXIS2_PLACEMENT_3D('',#72568,#34775,#34776);
#28787=AXIS2_PLACEMENT_3D('',#72572,#34779,#34780);
#28788=AXIS2_PLACEMENT_3D('',#72573,#34781,#34782);
#28789=AXIS2_PLACEMENT_3D('',#72574,#34783,#34784);
#28790=AXIS2_PLACEMENT_3D('',#72583,#34789,#34790);
#28791=AXIS2_PLACEMENT_3D('',#72585,#34791,#34792);
#28792=AXIS2_PLACEMENT_3D('',#72587,#34794,#34795);
#28793=AXIS2_PLACEMENT_3D('',#72591,#34798,#34799);
#28794=AXIS2_PLACEMENT_3D('',#72592,#34800,#34801);
#28795=AXIS2_PLACEMENT_3D('',#72593,#34802,#34803);
#28796=AXIS2_PLACEMENT_3D('',#72602,#34808,#34809);
#28797=AXIS2_PLACEMENT_3D('',#72604,#34810,#34811);
#28798=AXIS2_PLACEMENT_3D('',#72606,#34813,#34814);
#28799=AXIS2_PLACEMENT_3D('',#72610,#34817,#34818);
#28800=AXIS2_PLACEMENT_3D('',#72611,#34819,#34820);
#28801=AXIS2_PLACEMENT_3D('',#72612,#34821,#34822);
#28802=AXIS2_PLACEMENT_3D('',#72621,#34827,#34828);
#28803=AXIS2_PLACEMENT_3D('',#72623,#34829,#34830);
#28804=AXIS2_PLACEMENT_3D('',#72625,#34832,#34833);
#28805=AXIS2_PLACEMENT_3D('',#72629,#34836,#34837);
#28806=AXIS2_PLACEMENT_3D('',#72630,#34838,#34839);
#28807=AXIS2_PLACEMENT_3D('',#72631,#34840,#34841);
#28808=AXIS2_PLACEMENT_3D('',#72640,#34846,#34847);
#28809=AXIS2_PLACEMENT_3D('',#72642,#34848,#34849);
#28810=AXIS2_PLACEMENT_3D('',#72644,#34851,#34852);
#28811=AXIS2_PLACEMENT_3D('',#72648,#34855,#34856);
#28812=AXIS2_PLACEMENT_3D('',#72649,#34857,#34858);
#28813=AXIS2_PLACEMENT_3D('',#72650,#34859,#34860);
#28814=AXIS2_PLACEMENT_3D('',#72659,#34865,#34866);
#28815=AXIS2_PLACEMENT_3D('',#72661,#34867,#34868);
#28816=AXIS2_PLACEMENT_3D('',#72663,#34870,#34871);
#28817=AXIS2_PLACEMENT_3D('',#72667,#34874,#34875);
#28818=AXIS2_PLACEMENT_3D('',#72668,#34876,#34877);
#28819=AXIS2_PLACEMENT_3D('',#72669,#34878,#34879);
#28820=AXIS2_PLACEMENT_3D('',#72678,#34884,#34885);
#28821=AXIS2_PLACEMENT_3D('',#72680,#34886,#34887);
#28822=AXIS2_PLACEMENT_3D('',#72682,#34889,#34890);
#28823=AXIS2_PLACEMENT_3D('',#72686,#34893,#34894);
#28824=AXIS2_PLACEMENT_3D('',#72687,#34895,#34896);
#28825=AXIS2_PLACEMENT_3D('',#72688,#34897,#34898);
#28826=AXIS2_PLACEMENT_3D('',#72697,#34903,#34904);
#28827=AXIS2_PLACEMENT_3D('',#72699,#34905,#34906);
#28828=AXIS2_PLACEMENT_3D('',#72701,#34908,#34909);
#28829=AXIS2_PLACEMENT_3D('',#72705,#34912,#34913);
#28830=AXIS2_PLACEMENT_3D('',#72706,#34914,#34915);
#28831=AXIS2_PLACEMENT_3D('',#72707,#34916,#34917);
#28832=AXIS2_PLACEMENT_3D('',#72716,#34922,#34923);
#28833=AXIS2_PLACEMENT_3D('',#72718,#34924,#34925);
#28834=AXIS2_PLACEMENT_3D('',#72720,#34927,#34928);
#28835=AXIS2_PLACEMENT_3D('',#72724,#34931,#34932);
#28836=AXIS2_PLACEMENT_3D('',#72725,#34933,#34934);
#28837=AXIS2_PLACEMENT_3D('',#72726,#34935,#34936);
#28838=AXIS2_PLACEMENT_3D('',#72735,#34941,#34942);
#28839=AXIS2_PLACEMENT_3D('',#72737,#34943,#34944);
#28840=AXIS2_PLACEMENT_3D('',#72739,#34946,#34947);
#28841=AXIS2_PLACEMENT_3D('',#72743,#34950,#34951);
#28842=AXIS2_PLACEMENT_3D('',#72744,#34952,#34953);
#28843=AXIS2_PLACEMENT_3D('',#72745,#34954,#34955);
#28844=AXIS2_PLACEMENT_3D('',#72754,#34960,#34961);
#28845=AXIS2_PLACEMENT_3D('',#72756,#34962,#34963);
#28846=AXIS2_PLACEMENT_3D('',#72758,#34965,#34966);
#28847=AXIS2_PLACEMENT_3D('',#72762,#34969,#34970);
#28848=AXIS2_PLACEMENT_3D('',#72763,#34971,#34972);
#28849=AXIS2_PLACEMENT_3D('',#72764,#34973,#34974);
#28850=AXIS2_PLACEMENT_3D('',#72773,#34979,#34980);
#28851=AXIS2_PLACEMENT_3D('',#72775,#34981,#34982);
#28852=AXIS2_PLACEMENT_3D('',#72777,#34984,#34985);
#28853=AXIS2_PLACEMENT_3D('',#72781,#34988,#34989);
#28854=AXIS2_PLACEMENT_3D('',#72782,#34990,#34991);
#28855=AXIS2_PLACEMENT_3D('',#72783,#34992,#34993);
#28856=AXIS2_PLACEMENT_3D('',#72792,#34998,#34999);
#28857=AXIS2_PLACEMENT_3D('',#72794,#35000,#35001);
#28858=AXIS2_PLACEMENT_3D('',#72796,#35003,#35004);
#28859=AXIS2_PLACEMENT_3D('',#72800,#35007,#35008);
#28860=AXIS2_PLACEMENT_3D('',#72801,#35009,#35010);
#28861=AXIS2_PLACEMENT_3D('',#72802,#35011,#35012);
#28862=AXIS2_PLACEMENT_3D('',#72811,#35017,#35018);
#28863=AXIS2_PLACEMENT_3D('',#72813,#35019,#35020);
#28864=AXIS2_PLACEMENT_3D('',#72815,#35022,#35023);
#28865=AXIS2_PLACEMENT_3D('',#72819,#35026,#35027);
#28866=AXIS2_PLACEMENT_3D('',#72820,#35028,#35029);
#28867=AXIS2_PLACEMENT_3D('',#72821,#35030,#35031);
#28868=AXIS2_PLACEMENT_3D('',#72830,#35036,#35037);
#28869=AXIS2_PLACEMENT_3D('',#72832,#35038,#35039);
#28870=AXIS2_PLACEMENT_3D('',#72834,#35041,#35042);
#28871=AXIS2_PLACEMENT_3D('',#72838,#35045,#35046);
#28872=AXIS2_PLACEMENT_3D('',#72839,#35047,#35048);
#28873=AXIS2_PLACEMENT_3D('',#72840,#35049,#35050);
#28874=AXIS2_PLACEMENT_3D('',#72843,#35051,#35052);
#28875=AXIS2_PLACEMENT_3D('',#72847,#35055,#35056);
#28876=AXIS2_PLACEMENT_3D('',#72853,#35060,#35061);
#28877=AXIS2_PLACEMENT_3D('',#72857,#35064,#35065);
#28878=AXIS2_PLACEMENT_3D('',#72858,#35066,#35067);
#28879=AXIS2_PLACEMENT_3D('',#72859,#35068,#35069);
#28880=AXIS2_PLACEMENT_3D('',#72868,#35074,#35075);
#28881=AXIS2_PLACEMENT_3D('',#72870,#35076,#35077);
#28882=AXIS2_PLACEMENT_3D('',#72872,#35079,#35080);
#28883=AXIS2_PLACEMENT_3D('',#72876,#35083,#35084);
#28884=AXIS2_PLACEMENT_3D('',#72877,#35085,#35086);
#28885=AXIS2_PLACEMENT_3D('',#72878,#35087,#35088);
#28886=AXIS2_PLACEMENT_3D('',#72887,#35093,#35094);
#28887=AXIS2_PLACEMENT_3D('',#72889,#35095,#35096);
#28888=AXIS2_PLACEMENT_3D('',#72891,#35098,#35099);
#28889=AXIS2_PLACEMENT_3D('',#72895,#35102,#35103);
#28890=AXIS2_PLACEMENT_3D('',#72896,#35104,#35105);
#28891=AXIS2_PLACEMENT_3D('',#72897,#35106,#35107);
#28892=AXIS2_PLACEMENT_3D('',#72906,#35112,#35113);
#28893=AXIS2_PLACEMENT_3D('',#72908,#35114,#35115);
#28894=AXIS2_PLACEMENT_3D('',#72910,#35117,#35118);
#28895=AXIS2_PLACEMENT_3D('',#72914,#35121,#35122);
#28896=AXIS2_PLACEMENT_3D('',#72915,#35123,#35124);
#28897=AXIS2_PLACEMENT_3D('',#72916,#35125,#35126);
#28898=AXIS2_PLACEMENT_3D('',#72925,#35131,#35132);
#28899=AXIS2_PLACEMENT_3D('',#72927,#35133,#35134);
#28900=AXIS2_PLACEMENT_3D('',#72929,#35136,#35137);
#28901=AXIS2_PLACEMENT_3D('',#72933,#35140,#35141);
#28902=AXIS2_PLACEMENT_3D('',#72934,#35142,#35143);
#28903=AXIS2_PLACEMENT_3D('',#72935,#35144,#35145);
#28904=AXIS2_PLACEMENT_3D('',#72944,#35150,#35151);
#28905=AXIS2_PLACEMENT_3D('',#72946,#35152,#35153);
#28906=AXIS2_PLACEMENT_3D('',#72948,#35155,#35156);
#28907=AXIS2_PLACEMENT_3D('',#72952,#35159,#35160);
#28908=AXIS2_PLACEMENT_3D('',#72953,#35161,#35162);
#28909=AXIS2_PLACEMENT_3D('',#72954,#35163,#35164);
#28910=AXIS2_PLACEMENT_3D('',#72963,#35169,#35170);
#28911=AXIS2_PLACEMENT_3D('',#72965,#35171,#35172);
#28912=AXIS2_PLACEMENT_3D('',#72967,#35174,#35175);
#28913=AXIS2_PLACEMENT_3D('',#72971,#35178,#35179);
#28914=AXIS2_PLACEMENT_3D('',#72972,#35180,#35181);
#28915=AXIS2_PLACEMENT_3D('',#72973,#35182,#35183);
#28916=AXIS2_PLACEMENT_3D('',#72982,#35188,#35189);
#28917=AXIS2_PLACEMENT_3D('',#72984,#35190,#35191);
#28918=AXIS2_PLACEMENT_3D('',#72986,#35193,#35194);
#28919=AXIS2_PLACEMENT_3D('',#72990,#35197,#35198);
#28920=AXIS2_PLACEMENT_3D('',#72991,#35199,#35200);
#28921=AXIS2_PLACEMENT_3D('',#72992,#35201,#35202);
#28922=AXIS2_PLACEMENT_3D('',#73001,#35207,#35208);
#28923=AXIS2_PLACEMENT_3D('',#73003,#35209,#35210);
#28924=AXIS2_PLACEMENT_3D('',#73005,#35212,#35213);
#28925=AXIS2_PLACEMENT_3D('',#73009,#35216,#35217);
#28926=AXIS2_PLACEMENT_3D('',#73010,#35218,#35219);
#28927=AXIS2_PLACEMENT_3D('',#73011,#35220,#35221);
#28928=AXIS2_PLACEMENT_3D('',#73020,#35226,#35227);
#28929=AXIS2_PLACEMENT_3D('',#73022,#35228,#35229);
#28930=AXIS2_PLACEMENT_3D('',#73024,#35231,#35232);
#28931=AXIS2_PLACEMENT_3D('',#73028,#35235,#35236);
#28932=AXIS2_PLACEMENT_3D('',#73029,#35237,#35238);
#28933=AXIS2_PLACEMENT_3D('',#73030,#35239,#35240);
#28934=AXIS2_PLACEMENT_3D('',#73032,#35241,#35242);
#28935=AXIS2_PLACEMENT_3D('',#73033,#35243,#35244);
#28936=AXIS2_PLACEMENT_3D('',#73035,#35246,#35247);
#28937=AXIS2_PLACEMENT_3D('',#73037,#35248,#35249);
#28938=AXIS2_PLACEMENT_3D('',#73039,#35251,#35252);
#28939=AXIS2_PLACEMENT_3D('',#73040,#35253,#35254);
#28940=AXIS2_PLACEMENT_3D('',#73041,#35255,#35256);
#28941=AXIS2_PLACEMENT_3D('',#73042,#35257,#35258);
#28942=AXIS2_PLACEMENT_3D('',#73043,#35259,#35260);
#28943=AXIS2_PLACEMENT_3D('',#73044,#35261,#35262);
#28944=AXIS2_PLACEMENT_3D('',#73045,#35263,#35264);
#28945=AXIS2_PLACEMENT_3D('',#73046,#35265,#35266);
#28946=AXIS2_PLACEMENT_3D('',#73047,#35267,#35268);
#28947=AXIS2_PLACEMENT_3D('',#73048,#35269,#35270);
#28948=AXIS2_PLACEMENT_3D('',#73049,#35271,#35272);
#28949=AXIS2_PLACEMENT_3D('',#73050,#35273,#35274);
#28950=AXIS2_PLACEMENT_3D('',#73051,#35275,#35276);
#28951=AXIS2_PLACEMENT_3D('',#73052,#35277,#35278);
#28952=AXIS2_PLACEMENT_3D('',#73053,#35279,#35280);
#28953=AXIS2_PLACEMENT_3D('',#73054,#35281,#35282);
#28954=AXIS2_PLACEMENT_3D('',#73055,#35283,#35284);
#28955=AXIS2_PLACEMENT_3D('',#73057,#35286,#35287);
#28956=AXIS2_PLACEMENT_3D('',#73058,#35288,#35289);
#28957=AXIS2_PLACEMENT_3D('',#73059,#35290,#35291);
#28958=AXIS2_PLACEMENT_3D('',#73060,#35292,#35293);
#28959=AXIS2_PLACEMENT_3D('',#73061,#35294,#35295);
#28960=AXIS2_PLACEMENT_3D('',#73062,#35296,#35297);
#28961=AXIS2_PLACEMENT_3D('',#73063,#35298,#35299);
#28962=AXIS2_PLACEMENT_3D('',#73064,#35300,#35301);
#28963=AXIS2_PLACEMENT_3D('',#73065,#35302,#35303);
#28964=AXIS2_PLACEMENT_3D('',#73066,#35304,#35305);
#28965=AXIS2_PLACEMENT_3D('',#73067,#35306,#35307);
#28966=AXIS2_PLACEMENT_3D('',#73068,#35308,#35309);
#28967=AXIS2_PLACEMENT_3D('',#73069,#35310,#35311);
#28968=AXIS2_PLACEMENT_3D('',#73070,#35312,#35313);
#28969=AXIS2_PLACEMENT_3D('',#73071,#35314,#35315);
#28970=AXIS2_PLACEMENT_3D('',#73072,#35316,#35317);
#28971=AXIS2_PLACEMENT_3D('',#73073,#35318,#35319);
#28972=AXIS2_PLACEMENT_3D('',#73074,#35320,#35321);
#28973=AXIS2_PLACEMENT_3D('',#73075,#35322,#35323);
#28974=AXIS2_PLACEMENT_3D('',#73076,#35324,#35325);
#28975=AXIS2_PLACEMENT_3D('',#73077,#35326,#35327);
#28976=AXIS2_PLACEMENT_3D('',#73079,#35328,#35329);
#28977=AXIS2_PLACEMENT_3D('',#73081,#35331,#35332);
#28978=AXIS2_PLACEMENT_3D('',#73082,#35333,#35334);
#28979=AXIS2_PLACEMENT_3D('',#73083,#35335,#35336);
#28980=AXIS2_PLACEMENT_3D('',#73099,#35338,#35339);
#28981=AXIS2_PLACEMENT_3D('',#73107,#35340,#35341);
#28982=AXIS2_PLACEMENT_3D('',#73155,#35343,#35344);
#28983=AXIS2_PLACEMENT_3D('',#73203,#35346,#35347);
#28984=AXIS2_PLACEMENT_3D('',#73257,#35349,#35350);
#28985=AXIS2_PLACEMENT_3D('',#73305,#35352,#35353);
#28986=AXIS2_PLACEMENT_3D('',#73353,#35355,#35356);
#28987=AXIS2_PLACEMENT_3D('',#73404,#35358,#35359);
#28988=AXIS2_PLACEMENT_3D('',#73452,#35361,#35362);
#28989=AXIS2_PLACEMENT_3D('',#73500,#35364,#35365);
#28990=AXIS2_PLACEMENT_3D('',#73548,#35367,#35368);
#28991=AXIS2_PLACEMENT_3D('',#73602,#35370,#35371);
#28992=AXIS2_PLACEMENT_3D('',#73650,#35373,#35374);
#28993=AXIS2_PLACEMENT_3D('',#73698,#35376,#35377);
#28994=AXIS2_PLACEMENT_3D('',#73752,#35379,#35380);
#28995=AXIS2_PLACEMENT_3D('',#73800,#35382,#35383);
#28996=AXIS2_PLACEMENT_3D('',#73848,#35385,#35386);
#28997=AXIS2_PLACEMENT_3D('',#73902,#35388,#35389);
#28998=AXIS2_PLACEMENT_3D('',#73950,#35391,#35392);
#28999=AXIS2_PLACEMENT_3D('',#73998,#35394,#35395);
#29000=AXIS2_PLACEMENT_3D('',#74003,#35397,#35398);
#29001=AXIS2_PLACEMENT_3D('',#74051,#35399,#35400);
#29002=AXIS2_PLACEMENT_3D('',#74065,#35402,#35403);
#29003=AXIS2_PLACEMENT_3D('',#74072,#35404,#35405);
#29004=AXIS2_PLACEMENT_3D('',#74097,#35407,#35408);
#29005=AXIS2_PLACEMENT_3D('',#74121,#35410,#35411);
#29006=AXIS2_PLACEMENT_3D('',#74146,#35413,#35414);
#29007=AXIS2_PLACEMENT_3D('',#74171,#35416,#35417);
#29008=AXIS2_PLACEMENT_3D('',#74195,#35419,#35420);
#29009=AXIS2_PLACEMENT_3D('',#74220,#35422,#35423);
#29010=AXIS2_PLACEMENT_3D('',#74245,#35425,#35426);
#29011=AXIS2_PLACEMENT_3D('',#74269,#35428,#35429);
#29012=AXIS2_PLACEMENT_3D('',#74294,#35431,#35432);
#29013=AXIS2_PLACEMENT_3D('',#74319,#35434,#35435);
#29014=AXIS2_PLACEMENT_3D('',#74343,#35437,#35438);
#29015=AXIS2_PLACEMENT_3D('',#74367,#35440,#35441);
#29016=AXIS2_PLACEMENT_3D('',#74392,#35443,#35444);
#29017=AXIS2_PLACEMENT_3D('',#74417,#35446,#35447);
#29018=AXIS2_PLACEMENT_3D('',#74441,#35449,#35450);
#29019=AXIS2_PLACEMENT_3D('',#74466,#35452,#35453);
#29020=AXIS2_PLACEMENT_3D('',#74491,#35455,#35456);
#29021=AXIS2_PLACEMENT_3D('',#74515,#35458,#35459);
#29022=AXIS2_PLACEMENT_3D('',#74572,#35460,#35461);
#29023=AXIS2_PLACEMENT_3D('',#75208,#35462,#35463);
#29024=AXIS2_PLACEMENT_3D('',#75210,#35464,#35465);
#29025=AXIS2_PLACEMENT_3D('',#75211,#35466,#35467);
#29026=AXIS2_PLACEMENT_3D('',#75271,#35468,#35469);
#29027=AXIS2_PLACEMENT_3D('',#75272,#35470,#35471);
#29028=AXIS2_PLACEMENT_3D('',#75789,#35472,#35473);
#29029=AXIS2_PLACEMENT_3D('',#75791,#35474,#35475);
#29030=AXIS2_PLACEMENT_3D('',#75792,#35476,#35477);
#29031=AXIS2_PLACEMENT_3D('',#75793,#35478,#35479);
#29032=AXIS2_PLACEMENT_3D('',#75794,#35480,#35481);
#29033=AXIS2_PLACEMENT_3D('',#75795,#35482,#35483);
#29034=AXIS2_PLACEMENT_3D('',#75797,#35484,#35485);
#29035=AXIS2_PLACEMENT_3D('',#75798,#35486,#35487);
#29036=AXIS2_PLACEMENT_3D('',#75802,#35489,#35490);
#29037=AXIS2_PLACEMENT_3D('',#75803,#35491,#35492);
#29038=AXIS2_PLACEMENT_3D('',#75806,#35494,#35495);
#29039=AXIS2_PLACEMENT_3D('',#75807,#35496,#35497);
#29040=AXIS2_PLACEMENT_3D('',#75810,#35499,#35500);
#29041=AXIS2_PLACEMENT_3D('',#75811,#35501,#35502);
#29042=AXIS2_PLACEMENT_3D('',#75814,#35504,#35505);
#29043=AXIS2_PLACEMENT_3D('',#75815,#35506,#35507);
#29044=AXIS2_PLACEMENT_3D('',#75818,#35509,#35510);
#29045=AXIS2_PLACEMENT_3D('',#75819,#35511,#35512);
#29046=AXIS2_PLACEMENT_3D('',#75821,#35514,#35515);
#29047=AXIS2_PLACEMENT_3D('',#75822,#35516,#35517);
#29048=AXIS2_PLACEMENT_3D('',#75825,#35519,#35520);
#29049=AXIS2_PLACEMENT_3D('',#75831,#35524,#35525);
#29050=AXIS2_PLACEMENT_3D('',#75835,#35528,#35529);
#29051=AXIS2_PLACEMENT_3D('',#75839,#35532,#35533);
#29052=AXIS2_PLACEMENT_3D('',#75843,#35536,#35537);
#29053=AXIS2_PLACEMENT_3D('',#75847,#35540,#35541);
#29054=AXIS2_PLACEMENT_3D('',#75849,#35543,#35544);
#29055=AXIS2_PLACEMENT_3D('',#75858,#35549,#35550);
#29056=AXIS2_PLACEMENT_3D('',#75860,#35551,#35552);
#29057=AXIS2_PLACEMENT_3D('',#75862,#35554,#35555);
#29058=AXIS2_PLACEMENT_3D('',#75866,#35558,#35559);
#29059=AXIS2_PLACEMENT_3D('',#75867,#35560,#35561);
#29060=AXIS2_PLACEMENT_3D('',#75868,#35562,#35563);
#29061=AXIS2_PLACEMENT_3D('',#75877,#35568,#35569);
#29062=AXIS2_PLACEMENT_3D('',#75879,#35570,#35571);
#29063=AXIS2_PLACEMENT_3D('',#75881,#35573,#35574);
#29064=AXIS2_PLACEMENT_3D('',#75885,#35577,#35578);
#29065=AXIS2_PLACEMENT_3D('',#75886,#35579,#35580);
#29066=AXIS2_PLACEMENT_3D('',#75887,#35581,#35582);
#29067=AXIS2_PLACEMENT_3D('',#75896,#35587,#35588);
#29068=AXIS2_PLACEMENT_3D('',#75898,#35589,#35590);
#29069=AXIS2_PLACEMENT_3D('',#75900,#35592,#35593);
#29070=AXIS2_PLACEMENT_3D('',#75904,#35596,#35597);
#29071=AXIS2_PLACEMENT_3D('',#75905,#35598,#35599);
#29072=AXIS2_PLACEMENT_3D('',#75906,#35600,#35601);
#29073=AXIS2_PLACEMENT_3D('',#75915,#35606,#35607);
#29074=AXIS2_PLACEMENT_3D('',#75917,#35608,#35609);
#29075=AXIS2_PLACEMENT_3D('',#75919,#35611,#35612);
#29076=AXIS2_PLACEMENT_3D('',#75923,#35615,#35616);
#29077=AXIS2_PLACEMENT_3D('',#75924,#35617,#35618);
#29078=AXIS2_PLACEMENT_3D('',#75925,#35619,#35620);
#29079=AXIS2_PLACEMENT_3D('',#75934,#35625,#35626);
#29080=AXIS2_PLACEMENT_3D('',#75936,#35627,#35628);
#29081=AXIS2_PLACEMENT_3D('',#75938,#35630,#35631);
#29082=AXIS2_PLACEMENT_3D('',#75942,#35634,#35635);
#29083=AXIS2_PLACEMENT_3D('',#75943,#35636,#35637);
#29084=AXIS2_PLACEMENT_3D('',#75944,#35638,#35639);
#29085=AXIS2_PLACEMENT_3D('',#75953,#35644,#35645);
#29086=AXIS2_PLACEMENT_3D('',#75955,#35646,#35647);
#29087=AXIS2_PLACEMENT_3D('',#75957,#35649,#35650);
#29088=AXIS2_PLACEMENT_3D('',#75961,#35653,#35654);
#29089=AXIS2_PLACEMENT_3D('',#75962,#35655,#35656);
#29090=AXIS2_PLACEMENT_3D('',#75963,#35657,#35658);
#29091=AXIS2_PLACEMENT_3D('',#75972,#35663,#35664);
#29092=AXIS2_PLACEMENT_3D('',#75974,#35665,#35666);
#29093=AXIS2_PLACEMENT_3D('',#75976,#35668,#35669);
#29094=AXIS2_PLACEMENT_3D('',#75980,#35672,#35673);
#29095=AXIS2_PLACEMENT_3D('',#75981,#35674,#35675);
#29096=AXIS2_PLACEMENT_3D('',#75982,#35676,#35677);
#29097=AXIS2_PLACEMENT_3D('',#75991,#35682,#35683);
#29098=AXIS2_PLACEMENT_3D('',#75993,#35684,#35685);
#29099=AXIS2_PLACEMENT_3D('',#75995,#35687,#35688);
#29100=AXIS2_PLACEMENT_3D('',#75999,#35691,#35692);
#29101=AXIS2_PLACEMENT_3D('',#76000,#35693,#35694);
#29102=AXIS2_PLACEMENT_3D('',#76001,#35695,#35696);
#29103=AXIS2_PLACEMENT_3D('',#76010,#35701,#35702);
#29104=AXIS2_PLACEMENT_3D('',#76012,#35703,#35704);
#29105=AXIS2_PLACEMENT_3D('',#76015,#35706,#35707);
#29106=AXIS2_PLACEMENT_3D('',#76016,#35708,#35709);
#29107=AXIS2_PLACEMENT_3D('',#76020,#35712,#35713);
#29108=AXIS2_PLACEMENT_3D('',#76022,#35714,#35715);
#29109=AXIS2_PLACEMENT_3D('',#76023,#35716,#35717);
#29110=AXIS2_PLACEMENT_3D('',#76024,#35718,#35719);
#29111=AXIS2_PLACEMENT_3D('',#76033,#35724,#35725);
#29112=AXIS2_PLACEMENT_3D('',#76035,#35726,#35727);
#29113=AXIS2_PLACEMENT_3D('',#76037,#35729,#35730);
#29114=AXIS2_PLACEMENT_3D('',#76041,#35733,#35734);
#29115=AXIS2_PLACEMENT_3D('',#76042,#35735,#35736);
#29116=AXIS2_PLACEMENT_3D('',#76043,#35737,#35738);
#29117=AXIS2_PLACEMENT_3D('',#76052,#35743,#35744);
#29118=AXIS2_PLACEMENT_3D('',#76054,#35745,#35746);
#29119=AXIS2_PLACEMENT_3D('',#76056,#35748,#35749);
#29120=AXIS2_PLACEMENT_3D('',#76060,#35752,#35753);
#29121=AXIS2_PLACEMENT_3D('',#76061,#35754,#35755);
#29122=AXIS2_PLACEMENT_3D('',#76062,#35756,#35757);
#29123=AXIS2_PLACEMENT_3D('',#76071,#35762,#35763);
#29124=AXIS2_PLACEMENT_3D('',#76073,#35764,#35765);
#29125=AXIS2_PLACEMENT_3D('',#76075,#35767,#35768);
#29126=AXIS2_PLACEMENT_3D('',#76079,#35771,#35772);
#29127=AXIS2_PLACEMENT_3D('',#76080,#35773,#35774);
#29128=AXIS2_PLACEMENT_3D('',#76081,#35775,#35776);
#29129=AXIS2_PLACEMENT_3D('',#76090,#35781,#35782);
#29130=AXIS2_PLACEMENT_3D('',#76092,#35783,#35784);
#29131=AXIS2_PLACEMENT_3D('',#76094,#35786,#35787);
#29132=AXIS2_PLACEMENT_3D('',#76098,#35790,#35791);
#29133=AXIS2_PLACEMENT_3D('',#76099,#35792,#35793);
#29134=AXIS2_PLACEMENT_3D('',#76100,#35794,#35795);
#29135=AXIS2_PLACEMENT_3D('',#76109,#35800,#35801);
#29136=AXIS2_PLACEMENT_3D('',#76111,#35802,#35803);
#29137=AXIS2_PLACEMENT_3D('',#76113,#35805,#35806);
#29138=AXIS2_PLACEMENT_3D('',#76117,#35809,#35810);
#29139=AXIS2_PLACEMENT_3D('',#76118,#35811,#35812);
#29140=AXIS2_PLACEMENT_3D('',#76119,#35813,#35814);
#29141=AXIS2_PLACEMENT_3D('',#76128,#35819,#35820);
#29142=AXIS2_PLACEMENT_3D('',#76130,#35821,#35822);
#29143=AXIS2_PLACEMENT_3D('',#76132,#35824,#35825);
#29144=AXIS2_PLACEMENT_3D('',#76136,#35828,#35829);
#29145=AXIS2_PLACEMENT_3D('',#76137,#35830,#35831);
#29146=AXIS2_PLACEMENT_3D('',#76138,#35832,#35833);
#29147=AXIS2_PLACEMENT_3D('',#76147,#35838,#35839);
#29148=AXIS2_PLACEMENT_3D('',#76149,#35840,#35841);
#29149=AXIS2_PLACEMENT_3D('',#76151,#35843,#35844);
#29150=AXIS2_PLACEMENT_3D('',#76155,#35847,#35848);
#29151=AXIS2_PLACEMENT_3D('',#76156,#35849,#35850);
#29152=AXIS2_PLACEMENT_3D('',#76157,#35851,#35852);
#29153=AXIS2_PLACEMENT_3D('',#76166,#35857,#35858);
#29154=AXIS2_PLACEMENT_3D('',#76168,#35859,#35860);
#29155=AXIS2_PLACEMENT_3D('',#76170,#35862,#35863);
#29156=AXIS2_PLACEMENT_3D('',#76174,#35866,#35867);
#29157=AXIS2_PLACEMENT_3D('',#76175,#35868,#35869);
#29158=AXIS2_PLACEMENT_3D('',#76176,#35870,#35871);
#29159=AXIS2_PLACEMENT_3D('',#76185,#35876,#35877);
#29160=AXIS2_PLACEMENT_3D('',#76187,#35878,#35879);
#29161=AXIS2_PLACEMENT_3D('',#76189,#35881,#35882);
#29162=AXIS2_PLACEMENT_3D('',#76193,#35885,#35886);
#29163=AXIS2_PLACEMENT_3D('',#76194,#35887,#35888);
#29164=AXIS2_PLACEMENT_3D('',#76195,#35889,#35890);
#29165=AXIS2_PLACEMENT_3D('',#76204,#35895,#35896);
#29166=AXIS2_PLACEMENT_3D('',#76206,#35897,#35898);
#29167=AXIS2_PLACEMENT_3D('',#76208,#35900,#35901);
#29168=AXIS2_PLACEMENT_3D('',#76212,#35904,#35905);
#29169=AXIS2_PLACEMENT_3D('',#76213,#35906,#35907);
#29170=AXIS2_PLACEMENT_3D('',#76214,#35908,#35909);
#29171=AXIS2_PLACEMENT_3D('',#76223,#35914,#35915);
#29172=AXIS2_PLACEMENT_3D('',#76225,#35916,#35917);
#29173=AXIS2_PLACEMENT_3D('',#76227,#35919,#35920);
#29174=AXIS2_PLACEMENT_3D('',#76231,#35923,#35924);
#29175=AXIS2_PLACEMENT_3D('',#76232,#35925,#35926);
#29176=AXIS2_PLACEMENT_3D('',#76233,#35927,#35928);
#29177=AXIS2_PLACEMENT_3D('',#76242,#35933,#35934);
#29178=AXIS2_PLACEMENT_3D('',#76244,#35935,#35936);
#29179=AXIS2_PLACEMENT_3D('',#76246,#35938,#35939);
#29180=AXIS2_PLACEMENT_3D('',#76250,#35942,#35943);
#29181=AXIS2_PLACEMENT_3D('',#76251,#35944,#35945);
#29182=AXIS2_PLACEMENT_3D('',#76252,#35946,#35947);
#29183=AXIS2_PLACEMENT_3D('',#76261,#35952,#35953);
#29184=AXIS2_PLACEMENT_3D('',#76263,#35954,#35955);
#29185=AXIS2_PLACEMENT_3D('',#76265,#35957,#35958);
#29186=AXIS2_PLACEMENT_3D('',#76269,#35961,#35962);
#29187=AXIS2_PLACEMENT_3D('',#76270,#35963,#35964);
#29188=AXIS2_PLACEMENT_3D('',#76271,#35965,#35966);
#29189=AXIS2_PLACEMENT_3D('',#76280,#35971,#35972);
#29190=AXIS2_PLACEMENT_3D('',#76282,#35973,#35974);
#29191=AXIS2_PLACEMENT_3D('',#76284,#35976,#35977);
#29192=AXIS2_PLACEMENT_3D('',#76288,#35980,#35981);
#29193=AXIS2_PLACEMENT_3D('',#76289,#35982,#35983);
#29194=AXIS2_PLACEMENT_3D('',#76290,#35984,#35985);
#29195=AXIS2_PLACEMENT_3D('',#76299,#35990,#35991);
#29196=AXIS2_PLACEMENT_3D('',#76301,#35992,#35993);
#29197=AXIS2_PLACEMENT_3D('',#76303,#35995,#35996);
#29198=AXIS2_PLACEMENT_3D('',#76307,#35999,#36000);
#29199=AXIS2_PLACEMENT_3D('',#76308,#36001,#36002);
#29200=AXIS2_PLACEMENT_3D('',#76309,#36003,#36004);
#29201=AXIS2_PLACEMENT_3D('',#76318,#36009,#36010);
#29202=AXIS2_PLACEMENT_3D('',#76320,#36011,#36012);
#29203=AXIS2_PLACEMENT_3D('',#76322,#36014,#36015);
#29204=AXIS2_PLACEMENT_3D('',#76326,#36018,#36019);
#29205=AXIS2_PLACEMENT_3D('',#76327,#36020,#36021);
#29206=AXIS2_PLACEMENT_3D('',#76328,#36022,#36023);
#29207=AXIS2_PLACEMENT_3D('',#76337,#36028,#36029);
#29208=AXIS2_PLACEMENT_3D('',#76339,#36030,#36031);
#29209=AXIS2_PLACEMENT_3D('',#76341,#36033,#36034);
#29210=AXIS2_PLACEMENT_3D('',#76345,#36037,#36038);
#29211=AXIS2_PLACEMENT_3D('',#76346,#36039,#36040);
#29212=AXIS2_PLACEMENT_3D('',#76347,#36041,#36042);
#29213=AXIS2_PLACEMENT_3D('',#76350,#36043,#36044);
#29214=AXIS2_PLACEMENT_3D('',#76354,#36047,#36048);
#29215=AXIS2_PLACEMENT_3D('',#76360,#36052,#36053);
#29216=AXIS2_PLACEMENT_3D('',#76364,#36056,#36057);
#29217=AXIS2_PLACEMENT_3D('',#76365,#36058,#36059);
#29218=AXIS2_PLACEMENT_3D('',#76366,#36060,#36061);
#29219=AXIS2_PLACEMENT_3D('',#76375,#36066,#36067);
#29220=AXIS2_PLACEMENT_3D('',#76377,#36068,#36069);
#29221=AXIS2_PLACEMENT_3D('',#76379,#36071,#36072);
#29222=AXIS2_PLACEMENT_3D('',#76383,#36075,#36076);
#29223=AXIS2_PLACEMENT_3D('',#76384,#36077,#36078);
#29224=AXIS2_PLACEMENT_3D('',#76385,#36079,#36080);
#29225=AXIS2_PLACEMENT_3D('',#76394,#36085,#36086);
#29226=AXIS2_PLACEMENT_3D('',#76396,#36087,#36088);
#29227=AXIS2_PLACEMENT_3D('',#76398,#36090,#36091);
#29228=AXIS2_PLACEMENT_3D('',#76402,#36094,#36095);
#29229=AXIS2_PLACEMENT_3D('',#76403,#36096,#36097);
#29230=AXIS2_PLACEMENT_3D('',#76404,#36098,#36099);
#29231=AXIS2_PLACEMENT_3D('',#76413,#36104,#36105);
#29232=AXIS2_PLACEMENT_3D('',#76415,#36106,#36107);
#29233=AXIS2_PLACEMENT_3D('',#76417,#36109,#36110);
#29234=AXIS2_PLACEMENT_3D('',#76421,#36113,#36114);
#29235=AXIS2_PLACEMENT_3D('',#76422,#36115,#36116);
#29236=AXIS2_PLACEMENT_3D('',#76423,#36117,#36118);
#29237=AXIS2_PLACEMENT_3D('',#76432,#36123,#36124);
#29238=AXIS2_PLACEMENT_3D('',#76434,#36125,#36126);
#29239=AXIS2_PLACEMENT_3D('',#76436,#36128,#36129);
#29240=AXIS2_PLACEMENT_3D('',#76440,#36132,#36133);
#29241=AXIS2_PLACEMENT_3D('',#76441,#36134,#36135);
#29242=AXIS2_PLACEMENT_3D('',#76442,#36136,#36137);
#29243=AXIS2_PLACEMENT_3D('',#76451,#36142,#36143);
#29244=AXIS2_PLACEMENT_3D('',#76453,#36144,#36145);
#29245=AXIS2_PLACEMENT_3D('',#76455,#36147,#36148);
#29246=AXIS2_PLACEMENT_3D('',#76459,#36151,#36152);
#29247=AXIS2_PLACEMENT_3D('',#76460,#36153,#36154);
#29248=AXIS2_PLACEMENT_3D('',#76461,#36155,#36156);
#29249=AXIS2_PLACEMENT_3D('',#76470,#36161,#36162);
#29250=AXIS2_PLACEMENT_3D('',#76472,#36163,#36164);
#29251=AXIS2_PLACEMENT_3D('',#76474,#36166,#36167);
#29252=AXIS2_PLACEMENT_3D('',#76478,#36170,#36171);
#29253=AXIS2_PLACEMENT_3D('',#76479,#36172,#36173);
#29254=AXIS2_PLACEMENT_3D('',#76480,#36174,#36175);
#29255=AXIS2_PLACEMENT_3D('',#76489,#36180,#36181);
#29256=AXIS2_PLACEMENT_3D('',#76491,#36182,#36183);
#29257=AXIS2_PLACEMENT_3D('',#76493,#36185,#36186);
#29258=AXIS2_PLACEMENT_3D('',#76497,#36189,#36190);
#29259=AXIS2_PLACEMENT_3D('',#76498,#36191,#36192);
#29260=AXIS2_PLACEMENT_3D('',#76499,#36193,#36194);
#29261=AXIS2_PLACEMENT_3D('',#76508,#36199,#36200);
#29262=AXIS2_PLACEMENT_3D('',#76510,#36201,#36202);
#29263=AXIS2_PLACEMENT_3D('',#76512,#36204,#36205);
#29264=AXIS2_PLACEMENT_3D('',#76516,#36208,#36209);
#29265=AXIS2_PLACEMENT_3D('',#76517,#36210,#36211);
#29266=AXIS2_PLACEMENT_3D('',#76518,#36212,#36213);
#29267=AXIS2_PLACEMENT_3D('',#76527,#36218,#36219);
#29268=AXIS2_PLACEMENT_3D('',#76529,#36220,#36221);
#29269=AXIS2_PLACEMENT_3D('',#76531,#36223,#36224);
#29270=AXIS2_PLACEMENT_3D('',#76535,#36227,#36228);
#29271=AXIS2_PLACEMENT_3D('',#76536,#36229,#36230);
#29272=AXIS2_PLACEMENT_3D('',#76537,#36231,#36232);
#29273=AXIS2_PLACEMENT_3D('',#76539,#36233,#36234);
#29274=AXIS2_PLACEMENT_3D('',#76540,#36235,#36236);
#29275=AXIS2_PLACEMENT_3D('',#76542,#36238,#36239);
#29276=AXIS2_PLACEMENT_3D('',#76544,#36240,#36241);
#29277=AXIS2_PLACEMENT_3D('',#76546,#36243,#36244);
#29278=AXIS2_PLACEMENT_3D('',#76547,#36245,#36246);
#29279=AXIS2_PLACEMENT_3D('',#76548,#36247,#36248);
#29280=AXIS2_PLACEMENT_3D('',#76549,#36249,#36250);
#29281=AXIS2_PLACEMENT_3D('',#76550,#36251,#36252);
#29282=AXIS2_PLACEMENT_3D('',#76551,#36253,#36254);
#29283=AXIS2_PLACEMENT_3D('',#76552,#36255,#36256);
#29284=AXIS2_PLACEMENT_3D('',#76553,#36257,#36258);
#29285=AXIS2_PLACEMENT_3D('',#76554,#36259,#36260);
#29286=AXIS2_PLACEMENT_3D('',#76555,#36261,#36262);
#29287=AXIS2_PLACEMENT_3D('',#76556,#36263,#36264);
#29288=AXIS2_PLACEMENT_3D('',#76557,#36265,#36266);
#29289=AXIS2_PLACEMENT_3D('',#76558,#36267,#36268);
#29290=AXIS2_PLACEMENT_3D('',#76559,#36269,#36270);
#29291=AXIS2_PLACEMENT_3D('',#76560,#36271,#36272);
#29292=AXIS2_PLACEMENT_3D('',#76561,#36273,#36274);
#29293=AXIS2_PLACEMENT_3D('',#76562,#36275,#36276);
#29294=AXIS2_PLACEMENT_3D('',#76564,#36278,#36279);
#29295=AXIS2_PLACEMENT_3D('',#76565,#36280,#36281);
#29296=AXIS2_PLACEMENT_3D('',#76566,#36282,#36283);
#29297=AXIS2_PLACEMENT_3D('',#76567,#36284,#36285);
#29298=AXIS2_PLACEMENT_3D('',#76568,#36286,#36287);
#29299=AXIS2_PLACEMENT_3D('',#76569,#36288,#36289);
#29300=AXIS2_PLACEMENT_3D('',#76570,#36290,#36291);
#29301=AXIS2_PLACEMENT_3D('',#76571,#36292,#36293);
#29302=AXIS2_PLACEMENT_3D('',#76572,#36294,#36295);
#29303=AXIS2_PLACEMENT_3D('',#76573,#36296,#36297);
#29304=AXIS2_PLACEMENT_3D('',#76574,#36298,#36299);
#29305=AXIS2_PLACEMENT_3D('',#76575,#36300,#36301);
#29306=AXIS2_PLACEMENT_3D('',#76576,#36302,#36303);
#29307=AXIS2_PLACEMENT_3D('',#76577,#36304,#36305);
#29308=AXIS2_PLACEMENT_3D('',#76578,#36306,#36307);
#29309=AXIS2_PLACEMENT_3D('',#76579,#36308,#36309);
#29310=AXIS2_PLACEMENT_3D('',#76580,#36310,#36311);
#29311=AXIS2_PLACEMENT_3D('',#76581,#36312,#36313);
#29312=AXIS2_PLACEMENT_3D('',#76582,#36314,#36315);
#29313=AXIS2_PLACEMENT_3D('',#76583,#36316,#36317);
#29314=AXIS2_PLACEMENT_3D('',#76584,#36318,#36319);
#29315=AXIS2_PLACEMENT_3D('',#76586,#36320,#36321);
#29316=AXIS2_PLACEMENT_3D('',#76588,#36323,#36324);
#29317=AXIS2_PLACEMENT_3D('',#76589,#36325,#36326);
#29318=AXIS2_PLACEMENT_3D('',#76590,#36327,#36328);
#29319=AXIS2_PLACEMENT_3D('',#76591,#36329,#36330);
#29320=AXIS2_PLACEMENT_3D('',#76592,#36331,#36332);
#29321=AXIS2_PLACEMENT_3D('',#76593,#36333,#36334);
#29322=AXIS2_PLACEMENT_3D('',#76594,#36335,#36336);
#29323=AXIS2_PLACEMENT_3D('',#76595,#36337,#36338);
#29324=AXIS2_PLACEMENT_3D('',#76596,#36339,#36340);
#29325=AXIS2_PLACEMENT_3D('',#76597,#36341,#36342);
#29326=AXIS2_PLACEMENT_3D('',#76598,#36343,#36344);
#29327=AXIS2_PLACEMENT_3D('',#76599,#36345,#36346);
#29328=AXIS2_PLACEMENT_3D('',#76600,#36347,#36348);
#29329=AXIS2_PLACEMENT_3D('',#76601,#36349,#36350);
#29330=AXIS2_PLACEMENT_3D('',#76602,#36351,#36352);
#29331=AXIS2_PLACEMENT_3D('',#76603,#36353,#36354);
#29332=AXIS2_PLACEMENT_3D('',#76604,#36355,#36356);
#29333=AXIS2_PLACEMENT_3D('',#76605,#36357,#36358);
#29334=AXIS2_PLACEMENT_3D('',#76606,#36359,#36360);
#29335=AXIS2_PLACEMENT_3D('',#76607,#36361,#36362);
#29336=AXIS2_PLACEMENT_3D('',#76608,#36363,#36364);
#29337=AXIS2_PLACEMENT_3D('',#76609,#36365,#36366);
#29338=AXIS2_PLACEMENT_3D('',#76610,#36367,#36368);
#29339=AXIS2_PLACEMENT_3D('',#76611,#36369,#36370);
#29340=AXIS2_PLACEMENT_3D('',#76612,#36371,#36372);
#29341=AXIS2_PLACEMENT_3D('',#76613,#36373,#36374);
#29342=AXIS2_PLACEMENT_3D('',#76614,#36375,#36376);
#29343=AXIS2_PLACEMENT_3D('',#76615,#36377,#36378);
#29344=AXIS2_PLACEMENT_3D('',#76616,#36379,#36380);
#29345=DIRECTION('axis',(0.,0.,1.));
#29346=DIRECTION('refdir',(1.,0.,0.));
#29347=DIRECTION('axis',(0.,0.,1.));
#29348=DIRECTION('refdir',(1.,0.,0.));
#29349=DIRECTION('center_axis',(0.,0.,1.));
#29350=DIRECTION('ref_axis',(1.,1.68837364655892E-15,0.));
#29351=DIRECTION('',(0.,-0.923879532511291,-0.38268343236508));
#29352=DIRECTION('center_axis',(1.26986498732449E-30,-7.96826514156151E-16,
-1.));
#29353=DIRECTION('ref_axis',(1.,1.5936530283123E-15,0.));
#29354=DIRECTION('',(0.923879532511289,0.,0.382683432365085));
#29355=DIRECTION('center_axis',(0.,0.,1.));
#29356=DIRECTION('ref_axis',(1.,1.77635683940024E-15,0.));
#29357=DIRECTION('center_axis',(0.,-0.382683432365063,0.923879532511298));
#29358=DIRECTION('ref_axis',(1.,0.,0.));
#29359=DIRECTION('',(0.,-0.923879532511294,-0.382683432365072));
#29360=DIRECTION('',(1.,0.,0.));
#29361=DIRECTION('',(-1.,0.,0.));
#29362=DIRECTION('center_axis',(0.,0.,1.));
#29363=DIRECTION('ref_axis',(1.68837364655893E-15,1.,0.));
#29364=DIRECTION('',(0.923879532511285,0.,-0.382683432365095));
#29365=DIRECTION('center_axis',(0.,0.,-1.));
#29366=DIRECTION('ref_axis',(1.59365302831231E-15,1.,0.));
#29367=DIRECTION('center_axis',(0.,0.,1.));
#29368=DIRECTION('ref_axis',(1.77635683940025E-15,1.,0.));
#29369=DIRECTION('center_axis',(0.382683432365072,0.,0.923879532511294));
#29370=DIRECTION('ref_axis',(0.923879532511294,0.,-0.382683432365072));
#29371=DIRECTION('',(0.923879532511298,0.,-0.382683432365063));
#29372=DIRECTION('',(0.,1.,0.));
#29373=DIRECTION('',(0.,-1.,0.));
#29374=DIRECTION('center_axis',(0.,0.,1.));
#29375=DIRECTION('ref_axis',(-1.,0.,0.));
#29376=DIRECTION('',(0.,0.923879532511282,-0.382683432365102));
#29377=DIRECTION('center_axis',(0.,0.,-1.));
#29378=DIRECTION('ref_axis',(-1.,0.,0.));
#29379=DIRECTION('center_axis',(0.,0.,1.));
#29380=DIRECTION('ref_axis',(-1.,0.,0.));
#29381=DIRECTION('center_axis',(0.,0.382683432365063,0.923879532511298));
#29382=DIRECTION('ref_axis',(1.,0.,0.));
#29383=DIRECTION('',(0.,0.923879532511291,-0.382683432365078));
#29384=DIRECTION('',(-1.,0.,0.));
#29385=DIRECTION('',(1.,0.,0.));
#29386=DIRECTION('center_axis',(0.,0.,1.));
#29387=DIRECTION('ref_axis',(6.75349458623569E-15,-1.,0.));
#29388=DIRECTION('',(-0.923879532511281,-1.92271478790305E-14,-0.382683432365104));
#29389=DIRECTION('center_axis',(1.5936530283123E-15,1.01589198985959E-29,
-1.));
#29390=DIRECTION('ref_axis',(6.37461211324924E-15,-1.,0.));
#29391=DIRECTION('center_axis',(0.,0.,1.));
#29392=DIRECTION('ref_axis',(7.10542735760099E-15,-1.,0.));
#29393=DIRECTION('center_axis',(-0.382683432365085,0.,0.923879532511289));
#29394=DIRECTION('ref_axis',(0.923879532511289,0.,0.382683432365085));
#29395=DIRECTION('',(0.,-1.,0.));
#29396=DIRECTION('',(0.,1.,0.));
#29397=DIRECTION('center_axis',(0.,0.707106781186548,0.707106781186548));
#29398=DIRECTION('ref_axis',(1.,0.,0.));
#29399=DIRECTION('',(0.,0.707106781186548,-0.707106781186548));
#29400=DIRECTION('',(1.,0.,0.));
#29401=DIRECTION('',(8.3738264463134E-15,-0.707106781186552,0.707106781186543));
#29402=DIRECTION('center_axis',(0.,0.,1.));
#29403=DIRECTION('ref_axis',(7.10542735760099E-15,-1.,0.));
#29404=DIRECTION('',(0.707106781186543,0.,0.707106781186552));
#29405=DIRECTION('center_axis',(-1.71569776325697E-15,-1.17744752593799E-29,
1.));
#29406=DIRECTION('ref_axis',(6.86279105302788E-15,-1.,0.));
#29407=DIRECTION('center_axis',(-0.707106781186552,0.,0.707106781186543));
#29408=DIRECTION('ref_axis',(0.707106781186543,0.,0.707106781186552));
#29409=DIRECTION('',(0.707106781186543,0.,0.707106781186552));
#29410=DIRECTION('',(0.,1.,0.));
#29411=DIRECTION('center_axis',(0.,0.,1.));
#29412=DIRECTION('ref_axis',(1.,1.77635683940024E-15,0.));
#29413=DIRECTION('',(0.,0.707106781186548,0.707106781186548));
#29414=DIRECTION('center_axis',(2.94361881484495E-30,-1.71569776325696E-15,
1.));
#29415=DIRECTION('ref_axis',(1.,1.71569776325697E-15,0.));
#29416=DIRECTION('center_axis',(0.,0.,1.));
#29417=DIRECTION('ref_axis',(1.,0.,0.));
#29418=DIRECTION('center_axis',(0.,0.,-1.));
#29419=DIRECTION('ref_axis',(1.,1.77635683940025E-15,0.));
#29420=DIRECTION('',(1.,0.,0.));
#29421=DIRECTION('center_axis',(0.,0.,-1.));
#29422=DIRECTION('ref_axis',(8.88178419700126E-16,1.,0.));
#29423=DIRECTION('',(0.,1.,0.));
#29424=DIRECTION('center_axis',(0.,0.,-1.));
#29425=DIRECTION('ref_axis',(-1.,0.,0.));
#29426=DIRECTION('',(-1.,0.,0.));
#29427=DIRECTION('center_axis',(0.,0.,-1.));
#29428=DIRECTION('ref_axis',(0.,-1.,0.));
#29429=DIRECTION('',(0.,-1.,0.));
#29430=DIRECTION('center_axis',(0.,0.,1.));
#29431=DIRECTION('ref_axis',(1.,0.,0.));
#29432=DIRECTION('center_axis',(0.,0.,1.));
#29433=DIRECTION('ref_axis',(1.,0.,0.));
#29434=DIRECTION('',(0.707106781186554,8.65956056235501E-17,-0.707106781186541));
#29435=DIRECTION('center_axis',(0.,0.,-1.));
#29436=DIRECTION('ref_axis',(1.,0.,0.));
#29437=DIRECTION('center_axis',(0.,0.,1.));
#29438=DIRECTION('ref_axis',(1.,0.,0.));
#29439=DIRECTION('center_axis',(0.,0.,-1.));
#29440=DIRECTION('ref_axis',(-0.707106781186547,0.707106781186548,0.));
#29441=DIRECTION('',(0.,1.,0.));
#29442=DIRECTION('center_axis',(0.,0.,-1.));
#29443=DIRECTION('ref_axis',(-0.707106781186548,-0.707106781186548,0.));
#29444=DIRECTION('',(-1.,0.,0.));
#29445=DIRECTION('center_axis',(0.,0.,-1.));
#29446=DIRECTION('ref_axis',(0.707106781186551,-0.707106781186544,0.));
#29447=DIRECTION('',(0.,-1.,0.));
#29448=DIRECTION('center_axis',(0.,0.,-1.));
#29449=DIRECTION('ref_axis',(0.707106781186548,0.707106781186547,0.));
#29450=DIRECTION('',(1.,0.,0.));
#29451=DIRECTION('center_axis',(0.,0.,1.));
#29452=DIRECTION('ref_axis',(1.,0.,0.));
#29453=DIRECTION('center_axis',(0.,0.,1.));
#29454=DIRECTION('ref_axis',(1.,0.,0.));
#29455=DIRECTION('center_axis',(0.,0.,-1.));
#29456=DIRECTION('ref_axis',(1.,0.,0.));
#29457=DIRECTION('',(1.,0.,0.));
#29458=DIRECTION('',(0.,-1.,0.));
#29459=DIRECTION('',(-1.,0.,0.));
#29460=DIRECTION('',(0.,1.,0.));
#29461=DIRECTION('center_axis',(0.,0.,1.));
#29462=DIRECTION('ref_axis',(1.,0.,0.));
#29463=DIRECTION('center_axis',(0.,0.,1.));
#29464=DIRECTION('ref_axis',(1.,0.,0.));
#29465=DIRECTION('center_axis',(0.,0.,1.));
#29466=DIRECTION('ref_axis',(1.,0.,0.));
#29467=DIRECTION('',(0.,0.,1.));
#29468=DIRECTION('center_axis',(0.,0.,1.));
#29469=DIRECTION('ref_axis',(1.,0.,0.));
#29470=DIRECTION('',(0.707106781186554,8.65956056235501E-17,-0.707106781186541));
#29471=DIRECTION('center_axis',(0.,0.,-1.));
#29472=DIRECTION('ref_axis',(1.,0.,0.));
#29473=DIRECTION('center_axis',(0.,0.,1.));
#29474=DIRECTION('ref_axis',(1.,0.,0.));
#29475=DIRECTION('center_axis',(0.,0.,1.));
#29476=DIRECTION('ref_axis',(1.,0.,0.));
#29477=DIRECTION('',(0.,0.,1.));
#29478=DIRECTION('center_axis',(0.,0.,1.));
#29479=DIRECTION('ref_axis',(1.,0.,0.));
#29480=DIRECTION('',(0.707106781186554,8.65956056235501E-17,-0.707106781186541));
#29481=DIRECTION('center_axis',(0.,0.,-1.));
#29482=DIRECTION('ref_axis',(1.,0.,0.));
#29483=DIRECTION('center_axis',(0.,0.,1.));
#29484=DIRECTION('ref_axis',(1.,0.,0.));
#29485=DIRECTION('center_axis',(0.,0.,1.));
#29486=DIRECTION('ref_axis',(1.,0.,0.));
#29487=DIRECTION('',(0.,0.,1.));
#29488=DIRECTION('center_axis',(0.,0.,1.));
#29489=DIRECTION('ref_axis',(1.,0.,0.));
#29490=DIRECTION('',(0.707106781186554,8.65956056235501E-17,-0.707106781186541));
#29491=DIRECTION('center_axis',(0.,0.,-1.));
#29492=DIRECTION('ref_axis',(1.,0.,0.));
#29493=DIRECTION('center_axis',(0.,0.,1.));
#29494=DIRECTION('ref_axis',(1.,0.,0.));
#29495=DIRECTION('center_axis',(0.,0.,1.));
#29496=DIRECTION('ref_axis',(1.,0.,0.));
#29497=DIRECTION('',(0.,0.,1.));
#29498=DIRECTION('center_axis',(0.,-0.707106781186541,0.707106781186554));
#29499=DIRECTION('ref_axis',(1.,0.,0.));
#29500=DIRECTION('',(0.577350269189636,-0.577350269189616,-0.577350269189626));
#29501=DIRECTION('',(1.,0.,0.));
#29502=DIRECTION('',(-0.577350269189629,-0.577350269189629,-0.577350269189619));
#29503=DIRECTION('center_axis',(0.,0.707106781186541,0.707106781186554));
#29504=DIRECTION('ref_axis',(1.,0.,0.));
#29505=DIRECTION('',(-0.577350269189622,0.577350269189643,-0.577350269189612));
#29506=DIRECTION('',(-1.,0.,0.));
#29507=DIRECTION('',(-0.577350269189629,-0.577350269189629,0.577350269189619));
#29508=DIRECTION('center_axis',(-0.707106781186541,0.,0.707106781186554));
#29509=DIRECTION('ref_axis',(0.707106781186554,0.,0.707106781186541));
#29510=DIRECTION('',(0.,-1.,0.));
#29511=DIRECTION('center_axis',(0.707106781186541,0.,0.707106781186554));
#29512=DIRECTION('ref_axis',(0.707106781186554,0.,-0.707106781186541));
#29513=DIRECTION('',(0.,1.,0.));
#29514=DIRECTION('center_axis',(-1.,0.,0.));
#29515=DIRECTION('ref_axis',(0.,1.,0.));
#29516=DIRECTION('',(0.,0.,-1.));
#29517=DIRECTION('',(0.,1.,0.));
#29518=DIRECTION('',(0.,0.,-1.));
#29519=DIRECTION('center_axis',(0.,-1.,0.));
#29520=DIRECTION('ref_axis',(-1.,0.,0.));
#29521=DIRECTION('',(0.,0.,-1.));
#29522=DIRECTION('',(-1.,0.,0.));
#29523=DIRECTION('center_axis',(0.,0.923879532511296,0.382683432365067));
#29524=DIRECTION('ref_axis',(0.,-0.382683432365067,0.923879532511296));
#29525=DIRECTION('center_axis',(0.,-0.923879532511296,-0.382683432365067));
#29526=DIRECTION('ref_axis',(0.,-0.382683432365067,0.923879532511296));
#29527=DIRECTION('',(-1.,0.,0.));
#29528=DIRECTION('',(0.,-0.382683432365083,0.92387953251129));
#29529=DIRECTION('',(0.,0.38268343236507,-0.923879532511295));
#29530=DIRECTION('',(-1.,0.,0.));
#29531=DIRECTION('center_axis',(0.,0.,1.));
#29532=DIRECTION('ref_axis',(-1.,0.,0.));
#29533=DIRECTION('',(-0.38268343236509,0.,0.923879532511287));
#29534=DIRECTION('center_axis',(0.,0.,1.));
#29535=DIRECTION('ref_axis',(-1.,0.,0.));
#29536=DIRECTION('center_axis',(0.,0.,-1.));
#29537=DIRECTION('ref_axis',(-1.,0.,0.));
#29538=DIRECTION('center_axis',(0.923879532511287,0.,0.38268343236509));
#29539=DIRECTION('ref_axis',(0.38268343236509,0.,-0.923879532511287));
#29540=DIRECTION('',(-0.38268343236509,0.,0.923879532511287));
#29541=DIRECTION('',(0.,-1.,0.));
#29542=DIRECTION('',(0.,1.,0.));
#29543=DIRECTION('center_axis',(0.,0.,1.));
#29544=DIRECTION('ref_axis',(1.74550045912005E-15,1.,0.));
#29545=DIRECTION('',(0.,0.382683432365106,0.92387953251128));
#29546=DIRECTION('center_axis',(0.,0.,1.));
#29547=DIRECTION('ref_axis',(1.71569776325697E-15,1.,0.));
#29548=DIRECTION('center_axis',(0.,0.,-1.));
#29549=DIRECTION('ref_axis',(1.77635683940025E-15,1.,0.));
#29550=DIRECTION('center_axis',(0.,-0.923879532511296,0.382683432365067));
#29551=DIRECTION('ref_axis',(0.,-0.382683432365067,-0.923879532511296));
#29552=DIRECTION('center_axis',(0.,0.923879532511296,-0.382683432365067));
#29553=DIRECTION('ref_axis',(0.,0.382683432365067,0.923879532511296));
#29554=DIRECTION('',(1.,0.,0.));
#29555=DIRECTION('',(0.,0.38268343236507,0.923879532511295));
#29556=DIRECTION('',(-1.,0.,0.));
#29557=DIRECTION('',(1.,0.,0.));
#29558=DIRECTION('center_axis',(0.,0.,1.));
#29559=DIRECTION('ref_axis',(1.,1.74550045912004E-15,0.));
#29560=DIRECTION('',(0.382683432365103,0.,0.923879532511281));
#29561=DIRECTION('center_axis',(0.,0.,-1.));
#29562=DIRECTION('ref_axis',(1.,1.77635683940024E-15,0.));
#29563=DIRECTION('center_axis',(-0.923879532511286,0.,0.382683432365093));
#29564=DIRECTION('ref_axis',(0.382683432365093,0.,0.923879532511286));
#29565=DIRECTION('',(0.382683432365103,0.,0.923879532511281));
#29566=DIRECTION('',(0.,-1.,0.));
#29567=DIRECTION('center_axis',(0.,0.,1.));
#29568=DIRECTION('ref_axis',(6.98200183648019E-15,-1.,0.));
#29569=DIRECTION('center_axis',(0.,0.,-1.));
#29570=DIRECTION('ref_axis',(7.10542735760099E-15,-1.,0.));
#29571=DIRECTION('center_axis',(0.,-1.,0.));
#29572=DIRECTION('ref_axis',(-1.,0.,0.));
#29573=DIRECTION('',(0.,0.,-1.));
#29574=DIRECTION('',(1.,0.,0.));
#29575=DIRECTION('',(0.,0.,-1.));
#29576=DIRECTION('center_axis',(0.,-1.,0.));
#29577=DIRECTION('ref_axis',(0.,0.,1.));
#29578=DIRECTION('center_axis',(0.,-1.,0.));
#29579=DIRECTION('ref_axis',(0.,0.,1.));
#29580=DIRECTION('center_axis',(0.,0.,-1.));
#29581=DIRECTION('ref_axis',(7.10542735760099E-15,-1.,0.));
#29582=DIRECTION('',(0.,0.,-1.));
#29583=DIRECTION('center_axis',(0.,0.,1.));
#29584=DIRECTION('ref_axis',(0.707106781186551,-0.707106781186544,0.));
#29585=DIRECTION('center_axis',(1.,0.,0.));
#29586=DIRECTION('ref_axis',(0.,-1.,0.));
#29587=DIRECTION('',(0.,0.,-1.));
#29588=DIRECTION('',(0.,1.,0.));
#29589=DIRECTION('center_axis',(0.,0.,-1.));
#29590=DIRECTION('ref_axis',(1.,1.77635683940024E-15,0.));
#29591=DIRECTION('',(0.,0.,-1.));
#29592=DIRECTION('center_axis',(0.,0.,1.));
#29593=DIRECTION('ref_axis',(0.707106781186548,0.707106781186547,0.));
#29594=DIRECTION('center_axis',(0.,1.,0.));
#29595=DIRECTION('ref_axis',(1.,0.,0.));
#29596=DIRECTION('center_axis',(0.,1.,0.));
#29597=DIRECTION('ref_axis',(0.,0.,1.));
#29598=DIRECTION('center_axis',(0.,1.,0.));
#29599=DIRECTION('ref_axis',(0.,0.,1.));
#29600=DIRECTION('',(0.,0.,-1.));
#29601=DIRECTION('',(-1.,0.,0.));
#29602=DIRECTION('center_axis',(0.,1.,0.));
#29603=DIRECTION('ref_axis',(0.,0.,1.));
#29604=DIRECTION('',(0.,1.,0.));
#29605=DIRECTION('center_axis',(0.,-1.,0.));
#29606=DIRECTION('ref_axis',(0.,0.,1.));
#29607=DIRECTION('center_axis',(0.,-0.923879532511296,-0.382683432365067));
#29608=DIRECTION('ref_axis',(0.,-0.382683432365067,0.923879532511296));
#29609=DIRECTION('center_axis',(0.,-1.,0.));
#29610=DIRECTION('ref_axis',(0.,0.,1.));
#29611=DIRECTION('center_axis',(0.707106781186566,0.707106781186529,0.));
#29612=DIRECTION('ref_axis',(0.,0.,-1.));
#29613=DIRECTION('',(0.,0.,-1.));
#29614=DIRECTION('',(-0.357406744336602,0.357406744336621,-0.862856209461002));
#29615=DIRECTION('',(-0.357406744336583,0.357406744336602,0.862856209461017));
#29616=DIRECTION('',(0.,0.,1.));
#29617=DIRECTION('',(0.577350269189605,-0.577350269189636,0.577350269189636));
#29618=DIRECTION('center_axis',(0.707106781186566,0.,-0.707106781186529));
#29619=DIRECTION('ref_axis',(-0.707106781186529,0.,-0.707106781186566));
#29620=DIRECTION('',(0.,1.,0.));
#29621=DIRECTION('',(-0.577350269189602,-0.577350269189643,-0.577350269189633));
#29622=DIRECTION('',(0.,-1.,0.));
#29623=DIRECTION('center_axis',(0.923879532511281,0.,-0.382683432365103));
#29624=DIRECTION('ref_axis',(-0.382683432365103,0.,-0.923879532511281));
#29625=DIRECTION('',(0.,-1.,0.));
#29626=DIRECTION('',(-0.382683432365109,0.,-0.923879532511279));
#29627=DIRECTION('',(0.,1.,0.));
#29628=DIRECTION('',(-0.357406744336605,-0.357406744336599,-0.862856209461009));
#29629=DIRECTION('center_axis',(1.,0.,0.));
#29630=DIRECTION('ref_axis',(0.,1.,0.));
#29631=DIRECTION('',(0.,0.,1.));
#29632=DIRECTION('',(0.,-1.,0.));
#29633=DIRECTION('',(0.,0.,1.));
#29634=DIRECTION('',(0.,1.,0.));
#29635=DIRECTION('',(0.,0.,1.));
#29636=DIRECTION('center_axis',(0.,0.923879532511283,-0.382683432365098));
#29637=DIRECTION('ref_axis',(0.,0.382683432365098,0.923879532511283));
#29638=DIRECTION('',(-1.,0.,0.));
#29639=DIRECTION('',(-0.357406744336594,0.357406744336601,0.862856209461013));
#29640=DIRECTION('',(0.357406744336589,0.357406744336602,0.862856209461015));
#29641=DIRECTION('',(1.,0.,0.));
#29642=DIRECTION('center_axis',(-0.70710678118656,0.707106781186535,0.));
#29643=DIRECTION('ref_axis',(0.,0.,1.));
#29644=DIRECTION('',(0.357406744336593,0.357406744336606,-0.862856209461011));
#29645=DIRECTION('',(0.,0.,1.));
#29646=DIRECTION('',(0.577350269189616,0.577350269189636,-0.577350269189626));
#29647=DIRECTION('',(0.,0.,-1.));
#29648=DIRECTION('center_axis',(-0.923879532511286,0.,-0.382683432365092));
#29649=DIRECTION('ref_axis',(-0.382683432365092,0.,0.923879532511286));
#29650=DIRECTION('',(0.,-1.,0.));
#29651=DIRECTION('',(0.382683432365087,0.,-0.923879532511288));
#29652=DIRECTION('',(0.,1.,0.));
#29653=DIRECTION('center_axis',(0.,0.707106781186549,-0.707106781186546));
#29654=DIRECTION('ref_axis',(-1.,0.,0.));
#29655=DIRECTION('',(0.577350269189632,0.577350269189622,0.577350269189624));
#29656=DIRECTION('',(1.,0.,0.));
#29657=DIRECTION('',(0.577350269189629,-0.577350269189623,-0.577350269189626));
#29658=DIRECTION('center_axis',(0.,0.382683432365087,-0.923879532511288));
#29659=DIRECTION('ref_axis',(-1.,0.,0.));
#29660=DIRECTION('',(-0.357406744336593,0.862856209461018,0.357406744336591));
#29661=DIRECTION('',(-0.357406744336596,-0.862856209461017,-0.35740674433659));
#29662=DIRECTION('',(-1.,0.,0.));
#29663=DIRECTION('center_axis',(-0.707106781186546,0.,-0.707106781186549));
#29664=DIRECTION('ref_axis',(-0.707106781186549,0.,0.707106781186546));
#29665=DIRECTION('',(0.,-1.,0.));
#29666=DIRECTION('',(-0.707106781186549,-1.25607396694702E-14,0.707106781186546));
#29667=DIRECTION('center_axis',(0.,0.,-1.));
#29668=DIRECTION('ref_axis',(1.,1.83161605020261E-15,0.));
#29669=DIRECTION('',(0.923879532511282,0.,-0.382683432365102));
#29670=DIRECTION('center_axis',(1.77543178352399E-30,-9.42186760553338E-16,
1.));
#29671=DIRECTION('ref_axis',(1.,1.88437352110668E-15,0.));
#29672=DIRECTION('',(0.,-0.923879532511289,0.382683432365085));
#29673=DIRECTION('center_axis',(0.382683432365102,0.,0.923879532511282));
#29674=DIRECTION('ref_axis',(0.923879532511282,0.,-0.382683432365102));
#29675=DIRECTION('',(0.923879532511314,0.,-0.382683432365025));
#29676=DIRECTION('',(0.,1.,0.));
#29677=DIRECTION('center_axis',(0.,0.,-1.));
#29678=DIRECTION('ref_axis',(0.,-1.,0.));
#29679=DIRECTION('',(0.,-0.923879532511279,-0.38268343236511));
#29680=DIRECTION('center_axis',(4.71093380276669E-16,0.,1.));
#29681=DIRECTION('ref_axis',(0.,-1.,0.));
#29682=DIRECTION('center_axis',(0.,-0.382683432365087,0.923879532511288));
#29683=DIRECTION('ref_axis',(1.,0.,0.));
#29684=DIRECTION('',(0.,-0.923879532511279,-0.38268343236511));
#29685=DIRECTION('',(1.,0.,0.));
#29686=DIRECTION('center_axis',(0.,0.,-1.));
#29687=DIRECTION('ref_axis',(-1.,0.,0.));
#29688=DIRECTION('',(-0.923879532511282,0.,-0.382683432365102));
#29689=DIRECTION('center_axis',(0.,4.7109338027667E-16,1.));
#29690=DIRECTION('ref_axis',(-1.,0.,0.));
#29691=DIRECTION('center_axis',(-0.382683432365102,0.,0.923879532511282));
#29692=DIRECTION('ref_axis',(0.923879532511282,0.,0.382683432365102));
#29693=DIRECTION('',(-0.923879532511282,0.,-0.382683432365102));
#29694=DIRECTION('',(0.,-1.,0.));
#29695=DIRECTION('center_axis',(0.,0.,-1.));
#29696=DIRECTION('ref_axis',(9.15808025101306E-16,1.,0.));
#29697=DIRECTION('',(0.,0.923879532511285,-0.382683432365094));
#29698=DIRECTION('center_axis',(0.,0.,1.));
#29699=DIRECTION('ref_axis',(9.4218676055334E-16,1.,0.));
#29700=DIRECTION('center_axis',(0.,0.382683432365087,0.923879532511288));
#29701=DIRECTION('ref_axis',(1.,0.,0.));
#29702=DIRECTION('',(-1.,0.,0.));
#29703=DIRECTION('center_axis',(-0.707106781186548,0.,0.707106781186548));
#29704=DIRECTION('ref_axis',(0.707106781186548,0.,0.707106781186548));
#29705=DIRECTION('',(-0.707106781186548,0.,-0.707106781186548));
#29706=DIRECTION('',(0.,1.,0.));
#29707=DIRECTION('',(0.707106781186548,8.37382644631345E-15,0.707106781186548));
#29708=DIRECTION('center_axis',(0.,0.,-1.));
#29709=DIRECTION('ref_axis',(8.88178419700126E-16,1.,0.));
#29710=DIRECTION('',(0.,-0.707106781186548,0.707106781186548));
#29711=DIRECTION('center_axis',(0.,0.,-1.));
#29712=DIRECTION('ref_axis',(9.04161894879113E-16,1.,0.));
#29713=DIRECTION('center_axis',(0.,0.707106781186548,0.707106781186548));
#29714=DIRECTION('ref_axis',(1.,0.,0.));
#29715=DIRECTION('',(0.,-0.707106781186548,0.707106781186548));
#29716=DIRECTION('',(1.,0.,0.));
#29717=DIRECTION('center_axis',(0.,0.,-1.));
#29718=DIRECTION('ref_axis',(1.,1.77635683940025E-15,0.));
#29719=DIRECTION('',(-0.707106781186543,-8.3738264463135E-15,0.707106781186552));
#29720=DIRECTION('center_axis',(2.45252619645416E-30,-1.35624284231867E-15,
-1.));
#29721=DIRECTION('ref_axis',(1.,1.80832378975823E-15,0.));
#29722=DIRECTION('center_axis',(-0.923879532511287,0.,0.38268343236509));
#29723=DIRECTION('ref_axis',(0.38268343236509,0.,0.923879532511287));
#29724=DIRECTION('',(0.382683432365094,0.,0.923879532511285));
#29725=DIRECTION('',(-0.382683432365094,0.,-0.923879532511285));
#29726=DIRECTION('',(0.,-1.,0.));
#29727=DIRECTION('center_axis',(0.,0.,-1.));
#29728=DIRECTION('ref_axis',(-1.,0.,0.));
#29729=DIRECTION('',(0.,0.382683432365083,0.92387953251129));
#29730=DIRECTION('center_axis',(0.,0.,-1.));
#29731=DIRECTION('ref_axis',(-1.,0.,0.));
#29732=DIRECTION('center_axis',(0.,0.,1.));
#29733=DIRECTION('ref_axis',(-1.,0.,0.));
#29734=DIRECTION('center_axis',(0.,-0.923879532511296,0.382683432365067));
#29735=DIRECTION('ref_axis',(0.,-0.382683432365067,-0.923879532511296));
#29736=DIRECTION('center_axis',(0.,0.923879532511296,-0.382683432365067));
#29737=DIRECTION('ref_axis',(0.,0.382683432365067,0.923879532511296));
#29738=DIRECTION('',(1.,0.,0.));
#29739=DIRECTION('',(0.,0.38268343236507,0.923879532511295));
#29740=DIRECTION('',(-1.,0.,0.));
#29741=DIRECTION('',(1.,0.,0.));
#29742=DIRECTION('center_axis',(0.,0.,-1.));
#29743=DIRECTION('ref_axis',(0.,-1.,0.));
#29744=DIRECTION('',(-0.382683432365051,0.,0.923879532511303));
#29745=DIRECTION('center_axis',(-4.52080947439555E-16,0.,-1.));
#29746=DIRECTION('ref_axis',(0.,-1.,0.));
#29747=DIRECTION('center_axis',(0.,0.,1.));
#29748=DIRECTION('ref_axis',(0.,-1.,0.));
#29749=DIRECTION('center_axis',(0.923879532511273,0.,0.382683432365124));
#29750=DIRECTION('ref_axis',(0.382683432365124,0.,-0.923879532511273));
#29751=DIRECTION('',(-0.382683432365124,0.,0.923879532511273));
#29752=DIRECTION('',(0.,-1.,0.));
#29753=DIRECTION('center_axis',(0.,0.,-1.));
#29754=DIRECTION('ref_axis',(1.,1.79219777943861E-15,0.));
#29755=DIRECTION('',(0.,-0.382683432365097,0.923879532511284));
#29756=DIRECTION('center_axis',(0.,0.,1.));
#29757=DIRECTION('ref_axis',(1.,1.77635683940025E-15,0.));
#29758=DIRECTION('center_axis',(0.,0.923879532511296,0.382683432365067));
#29759=DIRECTION('ref_axis',(0.,-0.382683432365067,0.923879532511296));
#29760=DIRECTION('',(-1.,0.,0.));
#29761=DIRECTION('',(0.,-0.38268343236507,0.923879532511295));
#29762=DIRECTION('',(-1.,0.,0.));
#29763=DIRECTION('center_axis',(0.,0.,-1.));
#29764=DIRECTION('ref_axis',(8.96098889719304E-16,1.,0.));
#29765=DIRECTION('center_axis',(0.,0.,1.));
#29766=DIRECTION('ref_axis',(8.88178419700126E-16,1.,0.));
#29767=DIRECTION('center_axis',(0.,-1.,0.));
#29768=DIRECTION('ref_axis',(1.,0.,0.));
#29769=DIRECTION('',(0.,0.,1.));
#29770=DIRECTION('',(-1.,0.,0.));
#29771=DIRECTION('',(0.,0.,1.));
#29772=DIRECTION('center_axis',(0.,1.,0.));
#29773=DIRECTION('ref_axis',(0.,0.,1.));
#29774=DIRECTION('center_axis',(0.,1.,0.));
#29775=DIRECTION('ref_axis',(0.,0.,1.));
#29776=DIRECTION('center_axis',(0.,0.,1.));
#29777=DIRECTION('ref_axis',(-1.,0.,0.));
#29778=DIRECTION('',(0.,0.,1.));
#29779=DIRECTION('center_axis',(0.,0.,-1.));
#29780=DIRECTION('ref_axis',(-1.,0.,0.));
#29781=DIRECTION('center_axis',(-1.,0.,0.));
#29782=DIRECTION('ref_axis',(0.,-1.,0.));
#29783=DIRECTION('',(0.,0.,1.));
#29784=DIRECTION('',(0.,1.,0.));
#29785=DIRECTION('',(0.,0.,-1.));
#29786=DIRECTION('',(0.,1.,0.));
#29787=DIRECTION('center_axis',(0.,0.,1.));
#29788=DIRECTION('ref_axis',(8.88178419700126E-16,1.,0.));
#29789=DIRECTION('',(0.,0.,1.));
#29790=DIRECTION('center_axis',(0.,0.,-1.));
#29791=DIRECTION('ref_axis',(8.88178419700126E-16,1.,0.));
#29792=DIRECTION('center_axis',(0.,1.,0.));
#29793=DIRECTION('ref_axis',(-1.,0.,0.));
#29794=DIRECTION('',(0.,0.,1.));
#29795=DIRECTION('',(1.,0.,0.));
#29796=DIRECTION('center_axis',(0.,0.,1.));
#29797=DIRECTION('ref_axis',(0.,-1.,0.));
#29798=DIRECTION('',(0.,0.382683432365078,-0.923879532511292));
#29799=DIRECTION('center_axis',(-9.0416189487911E-16,0.,1.));
#29800=DIRECTION('ref_axis',(0.,-1.,0.));
#29801=DIRECTION('center_axis',(0.,0.,-1.));
#29802=DIRECTION('ref_axis',(0.,-1.,0.));
#29803=DIRECTION('center_axis',(0.,-0.923879532511287,-0.382683432365089));
#29804=DIRECTION('ref_axis',(0.,0.382683432365089,-0.923879532511287));
#29805=DIRECTION('',(0.,0.382683432365074,-0.923879532511293));
#29806=DIRECTION('',(1.,0.,0.));
#29807=DIRECTION('center_axis',(0.,0.,1.));
#29808=DIRECTION('ref_axis',(-1.,0.,-5.95065668954225E-17));
#29809=DIRECTION('center_axis',(-1.20084001663632E-16,3.6731576979464E-16,
1.));
#29810=DIRECTION('ref_axis',(-1.,0.,-1.20084001663632E-16));
#29811=DIRECTION('center_axis',(0.707106781186543,0.,-0.707106781186553));
#29812=DIRECTION('ref_axis',(-0.707106781186553,0.,-0.707106781186543));
#29813=DIRECTION('',(0.707106781186553,0.,0.707106781186543));
#29814=DIRECTION('',(0.,1.,0.));
#29815=DIRECTION('center_axis',(0.,0.,1.));
#29816=DIRECTION('ref_axis',(0.,-1.,0.));
#29817=DIRECTION('',(0.,-0.707106781186546,0.707106781186549));
#29818=DIRECTION('center_axis',(0.,0.,1.));
#29819=DIRECTION('ref_axis',(0.,-1.,0.));
#29820=DIRECTION('center_axis',(0.,-0.707106781186549,-0.707106781186546));
#29821=DIRECTION('ref_axis',(-1.,0.,0.));
#29822=DIRECTION('',(0.,-0.707106781186546,0.707106781186549));
#29823=DIRECTION('',(1.,0.,0.));
#29824=DIRECTION('center_axis',(0.,0.,1.));
#29825=DIRECTION('ref_axis',(-1.,0.,0.));
#29826=DIRECTION('center_axis',(0.,0.,1.));
#29827=DIRECTION('ref_axis',(-1.,0.,0.));
#29828=DIRECTION('center_axis',(0.293767845955579,-0.29376784595556,-0.909615800965028));
#29829=DIRECTION('ref_axis',(-0.951603598919524,0.,-0.307328147951679));
#29830=DIRECTION('',(0.252587513646048,-0.893921863713326,0.37027455965189));
#29831=DIRECTION('',(-0.893921863713342,0.252587513646,-0.370274559651883));
#29832=DIRECTION('',(0.707106781186522,0.707106781186573,-2.56395024851135E-15));
#29833=DIRECTION('center_axis',(-0.293767845955583,-0.293767845955567,-0.909615800965025));
#29834=DIRECTION('ref_axis',(-0.951603598919523,0.,0.307328147951684));
#29835=DIRECTION('',(0.707106781186537,-0.707106781186558,-2.05116019880918E-14));
#29836=DIRECTION('',(-0.893921863713315,-0.252587513646067,0.370274559651903));
#29837=DIRECTION('',(0.252587513646048,0.893921863713326,-0.37027455965189));
#29838=DIRECTION('center_axis',(0.382683432365075,0.,-0.923879532511293));
#29839=DIRECTION('ref_axis',(-0.923879532511293,0.,-0.382683432365075));
#29840=DIRECTION('',(0.923879532511287,1.92271478790291E-14,0.38268343236509));
#29841=DIRECTION('',(0.,-1.,0.));
#29842=DIRECTION('',(0.,1.,0.));
#29843=DIRECTION('center_axis',(0.,0.,1.));
#29844=DIRECTION('ref_axis',(1.,1.80669269305388E-15,0.));
#29845=DIRECTION('',(0.,0.923879532511307,0.382683432365042));
#29846=DIRECTION('center_axis',(6.58156273757651E-32,-3.58533327904521E-17,
-1.));
#29847=DIRECTION('ref_axis',(1.,1.83569063887115E-15,0.));
#29848=DIRECTION('center_axis',(0.,0.,1.));
#29849=DIRECTION('ref_axis',(1.,1.77635683940025E-15,0.));
#29850=DIRECTION('center_axis',(0.,0.382683432365087,-0.923879532511288));
#29851=DIRECTION('ref_axis',(-1.,0.,0.));
#29852=DIRECTION('',(0.,0.923879532511291,0.382683432365079));
#29853=DIRECTION('',(1.,0.,0.));
#29854=DIRECTION('',(-1.,0.,0.));
#29855=DIRECTION('center_axis',(0.,0.,1.));
#29856=DIRECTION('ref_axis',(9.03346346526939E-16,1.,0.));
#29857=DIRECTION('',(-0.923879532511288,0.,0.382683432365088));
#29858=DIRECTION('center_axis',(2.40217329696029E-16,-2.20482351708812E-31,
-1.));
#29859=DIRECTION('ref_axis',(9.17845319435574E-16,1.,0.));
#29860=DIRECTION('center_axis',(0.,0.,1.));
#29861=DIRECTION('ref_axis',(8.88178419700126E-16,1.,0.));
#29862=DIRECTION('center_axis',(-0.382683432365103,0.,-0.923879532511281));
#29863=DIRECTION('ref_axis',(-0.923879532511281,0.,0.382683432365103));
#29864=DIRECTION('',(0.,-1.,0.));
#29865=DIRECTION('',(0.,1.,0.));
#29866=DIRECTION('center_axis',(0.,-0.382683432365087,-0.923879532511288));
#29867=DIRECTION('ref_axis',(-1.,0.,0.));
#29868=DIRECTION('',(-1.,0.,0.));
#29869=DIRECTION('',(1.,0.,0.));
#29870=DIRECTION('center_axis',(0.585030164998638,-0.585030164998597,-0.56167553986566));
#29871=DIRECTION('ref_axis',(-0.692561717404368,0.,-0.721358626194982));
#29872=DIRECTION('',(0.707106781186527,0.707106781186568,5.12790049702273E-15));
#29873=DIRECTION('',(0.341690748410332,-0.450292794593974,0.824914438949602));
#29874=DIRECTION('',(-0.707106781186522,-0.707106781186573,-2.70840949122957E-14));
#29875=DIRECTION('',(-0.450292794593978,0.341690748410326,-0.824914438949602));
#29876=DIRECTION('center_axis',(-0.585030164998638,-0.585030164998608,-0.561675539865649));
#29877=DIRECTION('ref_axis',(-0.692561717404361,0.,0.721358626194989));
#29878=DIRECTION('',(-0.450292794593951,-0.341690748410332,0.824914438949615));
#29879=DIRECTION('',(-0.707106781186541,0.707106781186554,1.37383090134832E-14));
#29880=DIRECTION('',(0.341690748410326,0.450292794593954,-0.824914438949615));
#29881=DIRECTION('',(0.707106781186553,-0.707106781186542,-2.5639502485115E-14));
#29882=DIRECTION('center_axis',(-0.707106781186554,-0.707106781186541,0.));
#29883=DIRECTION('ref_axis',(0.,0.,1.));
#29884=DIRECTION('',(0.,0.,1.));
#29885=DIRECTION('',(-0.577350269189605,0.577350269189636,0.577350269189636));
#29886=DIRECTION('center_axis',(-0.707106781186541,0.,-0.707106781186554));
#29887=DIRECTION('ref_axis',(-0.707106781186554,0.,0.707106781186541));
#29888=DIRECTION('',(0.,-1.,0.));
#29889=DIRECTION('center_axis',(-0.923879532511286,0.,-0.382683432365092));
#29890=DIRECTION('ref_axis',(-0.382683432365092,0.,0.923879532511286));
#29891=DIRECTION('',(0.382683432365091,0.,-0.923879532511286));
#29892=DIRECTION('',(0.,-1.,0.));
#29893=DIRECTION('center_axis',(0.,0.,1.));
#29894=DIRECTION('ref_axis',(8.96098889719304E-16,1.,0.));
#29895=DIRECTION('',(0.,-0.382683432365091,-0.923879532511287));
#29896=DIRECTION('center_axis',(0.,0.,1.));
#29897=DIRECTION('ref_axis',(9.04161894879114E-16,1.,0.));
#29898=DIRECTION('center_axis',(0.,0.923879532511287,-0.382683432365089));
#29899=DIRECTION('ref_axis',(0.,0.382683432365089,0.923879532511287));
#29900=DIRECTION('',(0.,-0.382683432365091,-0.923879532511286));
#29901=DIRECTION('',(-1.,0.,0.));
#29902=DIRECTION('center_axis',(0.,0.,1.));
#29903=DIRECTION('ref_axis',(1.,1.79219777943861E-15,0.));
#29904=DIRECTION('',(-0.382683432365101,0.,-0.923879532511282));
#29905=DIRECTION('center_axis',(1.72443248188183E-30,-9.53608248505313E-16,
1.));
#29906=DIRECTION('ref_axis',(1.,1.80832378975823E-15,0.));
#29907=DIRECTION('center_axis',(0.,0.,-1.));
#29908=DIRECTION('ref_axis',(1.,1.77635683940025E-15,0.));
#29909=DIRECTION('center_axis',(0.923879532511281,0.,-0.382683432365103));
#29910=DIRECTION('ref_axis',(-0.382683432365103,0.,-0.923879532511281));
#29911=DIRECTION('',(0.,1.,0.));
#29912=DIRECTION('center_axis',(-0.408248290463875,-0.408248290463851,-0.816496580927726));
#29913=DIRECTION('ref_axis',(-0.894427190999911,0.,0.447213595499968));
#29914=DIRECTION('',(-0.577350269189629,-0.577350269189623,0.577350269189626));
#29915=DIRECTION('',(0.577350269189629,0.577350269189623,-0.577350269189626));
#29916=DIRECTION('center_axis',(0.,-0.923879532511283,-0.382683432365098));
#29917=DIRECTION('ref_axis',(0.,0.382683432365098,-0.923879532511283));
#29918=DIRECTION('',(1.,0.,0.));
#29919=DIRECTION('',(-1.,0.,0.));
#29920=DIRECTION('center_axis',(0.707106781186573,-0.707106781186522,0.));
#29921=DIRECTION('ref_axis',(0.,0.,-1.));
#29922=DIRECTION('',(0.,0.,-1.));
#29923=DIRECTION('center_axis',(0.408248290463882,-0.408248290463841,-0.816496580927727));
#29924=DIRECTION('ref_axis',(-0.894427190999908,0.,-0.447213595499974));
#29925=DIRECTION('',(0.577350269189632,-0.577350269189622,0.577350269189624));
#29926=DIRECTION('',(-0.577350269189632,0.577350269189622,-0.577350269189624));
#29927=DIRECTION('center_axis',(0.,0.,1.));
#29928=DIRECTION('ref_axis',(1.,1.77635683940025E-15,0.));
#29929=DIRECTION('',(0.,0.707106781186565,0.70710678118653));
#29930=DIRECTION('',(0.707106781186553,1.25607396694701E-14,0.707106781186543));
#29931=DIRECTION('center_axis',(-0.707106781186546,0.,-0.707106781186549));
#29932=DIRECTION('ref_axis',(-0.707106781186549,0.,0.707106781186546));
#29933=DIRECTION('',(-0.707106781186546,0.,0.707106781186549));
#29934=DIRECTION('center_axis',(0.,0.707106781186549,-0.707106781186546));
#29935=DIRECTION('ref_axis',(-1.,0.,0.));
#29936=DIRECTION('',(0.,0.707106781186546,0.707106781186549));
#29937=DIRECTION('center_axis',(0.,0.,1.));
#29938=DIRECTION('ref_axis',(8.88178419700126E-16,1.,0.));
#29939=DIRECTION('center_axis',(0.,-1.,0.));
#29940=DIRECTION('ref_axis',(1.,0.,0.));
#29941=DIRECTION('',(1.,0.,0.));
#29942=DIRECTION('center_axis',(0.,0.,1.));
#29943=DIRECTION('ref_axis',(1.,0.,0.));
#29944=DIRECTION('',(-1.,0.,0.));
#29945=DIRECTION('center_axis',(0.,0.,1.));
#29946=DIRECTION('ref_axis',(1.,0.,0.));
#29947=DIRECTION('center_axis',(0.,1.,0.));
#29948=DIRECTION('ref_axis',(-1.,0.,0.));
#29949=DIRECTION('center_axis',(0.,0.,1.));
#29950=DIRECTION('ref_axis',(1.,0.,0.));
#29951=DIRECTION('center_axis',(0.,-0.707106781186549,-0.707106781186546));
#29952=DIRECTION('ref_axis',(-1.,0.,0.));
#29953=DIRECTION('center_axis',(0.707106781186543,0.,-0.707106781186553));
#29954=DIRECTION('ref_axis',(-0.707106781186553,0.,-0.707106781186543));
#29955=DIRECTION('center_axis',(0.,0.,1.));
#29956=DIRECTION('ref_axis',(1.,0.,0.));
#29957=DIRECTION('center_axis',(0.,0.,-1.));
#29958=DIRECTION('ref_axis',(-1.,0.,0.));
#29959=DIRECTION('center_axis',(0.,-1.,0.));
#29960=DIRECTION('ref_axis',(-1.,0.,0.));
#29961=DIRECTION('center_axis',(1.,0.,0.));
#29962=DIRECTION('ref_axis',(0.,0.,-1.));
#29963=DIRECTION('center_axis',(0.,0.,1.));
#29964=DIRECTION('ref_axis',(-0.707106781186547,0.707106781186548,0.));
#29965=DIRECTION('center_axis',(1.,0.,0.));
#29966=DIRECTION('ref_axis',(0.,0.707106781186547,-0.707106781186547));
#29967=DIRECTION('center_axis',(1.,0.,0.));
#29968=DIRECTION('ref_axis',(0.,0.,-1.));
#29969=DIRECTION('center_axis',(0.,0.,-1.));
#29970=DIRECTION('ref_axis',(-1.,0.,0.));
#29971=DIRECTION('center_axis',(0.,-1.,0.));
#29972=DIRECTION('ref_axis',(0.,0.,-1.));
#29973=DIRECTION('center_axis',(0.,-1.,0.));
#29974=DIRECTION('ref_axis',(0.707106781186543,0.,-0.707106781186552));
#29975=DIRECTION('center_axis',(-5.92118946466756E-15,-1.,0.));
#29976=DIRECTION('ref_axis',(0.,0.,-1.));
#29977=DIRECTION('center_axis',(0.,0.,-1.));
#29978=DIRECTION('ref_axis',(-1.,0.,0.));
#29979=DIRECTION('center_axis',(-1.,-2.368475785867E-14,0.));
#29980=DIRECTION('ref_axis',(0.,0.,-1.));
#29981=DIRECTION('center_axis',(-1.,0.,0.));
#29982=DIRECTION('ref_axis',(0.,-0.707106781186547,-0.707106781186547));
#29983=DIRECTION('center_axis',(-1.,5.92118946466752E-15,0.));
#29984=DIRECTION('ref_axis',(0.,0.,-1.));
#29985=DIRECTION('center_axis',(0.,0.,-1.));
#29986=DIRECTION('ref_axis',(-1.,0.,0.));
#29987=DIRECTION('center_axis',(0.,1.,0.));
#29988=DIRECTION('ref_axis',(0.,0.,-1.));
#29989=DIRECTION('center_axis',(0.,0.,1.));
#29990=DIRECTION('ref_axis',(-0.707106781186548,-0.707106781186548,0.));
#29991=DIRECTION('center_axis',(0.,1.,0.));
#29992=DIRECTION('ref_axis',(-0.707106781186552,0.,-0.707106781186543));
#29993=DIRECTION('',(0.,-1.,0.));
#29994=DIRECTION('center_axis',(0.,0.,-1.));
#29995=DIRECTION('ref_axis',(-1.,0.,0.));
#29996=DIRECTION('',(0.,0.,-1.));
#29997=DIRECTION('center_axis',(-1.,0.,0.));
#29998=DIRECTION('ref_axis',(0.,1.,0.));
#29999=DIRECTION('',(0.,0.,-1.));
#30000=DIRECTION('center_axis',(0.,0.,-1.));
#30001=DIRECTION('ref_axis',(1.77635683940025E-15,1.,0.));
#30002=DIRECTION('center_axis',(0.,0.,1.));
#30003=DIRECTION('ref_axis',(-1.,0.,0.));
#30004=DIRECTION('',(-0.707106781186548,0.,0.707106781186548));
#30005=DIRECTION('center_axis',(0.707106781186543,0.,0.707106781186552));
#30006=DIRECTION('ref_axis',(0.707106781186552,0.,-0.707106781186543));
#30007=DIRECTION('',(-0.707106781186552,0.,0.707106781186543));
#30008=DIRECTION('center_axis',(0.,0.,1.));
#30009=DIRECTION('ref_axis',(1.77635683940025E-15,1.,0.));
#30010=DIRECTION('',(0.,0.707106781186548,0.707106781186548));
#30011=DIRECTION('center_axis',(0.,-0.707106781186548,0.707106781186548));
#30012=DIRECTION('ref_axis',(1.,0.,0.));
#30013=DIRECTION('center_axis',(0.,0.,-1.));
#30014=DIRECTION('ref_axis',(-1.,0.,0.));
#30015=DIRECTION('',(0.,0.707106781186548,0.707106781186548));
#30016=DIRECTION('center_axis',(0.,-0.707106781186548,0.707106781186548));
#30017=DIRECTION('ref_axis',(1.,0.,0.));
#30018=DIRECTION('',(0.,0.707106781186548,0.707106781186548));
#30019=DIRECTION('center_axis',(0.,0.,-1.));
#30020=DIRECTION('ref_axis',(0.,-1.,0.));
#30021=DIRECTION('',(-0.707106781186527,0.,0.707106781186568));
#30022=DIRECTION('center_axis',(0.707106781186552,0.,0.707106781186543));
#30023=DIRECTION('ref_axis',(0.707106781186543,0.,-0.707106781186552));
#30024=DIRECTION('center_axis',(0.,0.,1.));
#30025=DIRECTION('ref_axis',(0.,-1.,0.));
#30026=DIRECTION('center_axis',(0.,1.,0.));
#30027=DIRECTION('ref_axis',(0.,0.,1.));
#30028=DIRECTION('',(0.,1.,0.));
#30029=DIRECTION('center_axis',(0.,0.,1.));
#30030=DIRECTION('ref_axis',(1.,0.,0.));
#30031=DIRECTION('',(0.,0.,1.));
#30032=DIRECTION('center_axis',(0.,0.,1.));
#30033=DIRECTION('ref_axis',(1.,0.,0.));
#30034=DIRECTION('',(-0.857167300702113,-1.04972719113862E-16,0.515038074910052));
#30035=DIRECTION('center_axis',(0.,0.,1.));
#30036=DIRECTION('ref_axis',(1.,0.,0.));
#30037=DIRECTION('',(-0.857167300702113,-1.04972719113862E-16,0.515038074910052));
#30038=DIRECTION('center_axis',(0.,0.,1.));
#30039=DIRECTION('ref_axis',(1.,0.,0.));
#30040=DIRECTION('',(-0.857167300702112,-1.04972719113862E-16,0.515038074910055));
#30041=DIRECTION('center_axis',(0.,0.,1.));
#30042=DIRECTION('ref_axis',(1.,0.,0.));
#30043=DIRECTION('',(-0.857167300702112,-1.04972719113862E-16,0.515038074910055));
#30044=DIRECTION('center_axis',(1.,0.,0.));
#30045=DIRECTION('ref_axis',(0.,-1.,0.));
#30046=DIRECTION('',(0.,0.,-1.));
#30047=DIRECTION('',(0.,-1.,0.));
#30048=DIRECTION('center_axis',(0.,1.,0.));
#30049=DIRECTION('ref_axis',(1.,0.,0.));
#30050=DIRECTION('',(1.,0.,0.));
#30051=DIRECTION('center_axis',(0.,0.,-1.));
#30052=DIRECTION('ref_axis',(-1.,0.,0.));
#30053=DIRECTION('center_axis',(0.,0.,1.));
#30054=DIRECTION('ref_axis',(1.,1.77635683940025E-15,0.));
#30055=DIRECTION('axis',(0.,0.,1.));
#30056=DIRECTION('refdir',(1.,0.,0.));
#30057=DIRECTION('center_axis',(0.,-3.00548293115791E-15,-1.));
#30058=DIRECTION('ref_axis',(-1.,-3.13880988628035E-17,0.));
#30059=DIRECTION('center_axis',(0.,0.,-1.));
#30060=DIRECTION('ref_axis',(-1.,0.,0.));
#30061=DIRECTION('',(0.923879532511284,-1.00800709067767E-15,-0.382683432365096));
#30062=DIRECTION('center_axis',(0.,0.,1.));
#30063=DIRECTION('ref_axis',(-1.,-6.12323399573677E-17,0.));
#30064=DIRECTION('center_axis',(0.,0.,1.));
#30065=DIRECTION('ref_axis',(-1.,-6.12323399573677E-17,0.));
#30066=DIRECTION('center_axis',(0.,0.,-1.));
#30067=DIRECTION('ref_axis',(1.,0.,0.));
#30068=DIRECTION('',(-0.707106781186522,-8.65956056235463E-17,-0.707106781186573));
#30069=DIRECTION('center_axis',(0.,0.,-1.));
#30070=DIRECTION('ref_axis',(-1.,-6.12323399573677E-17,0.));
#30071=DIRECTION('center_axis',(0.,0.,-1.));
#30072=DIRECTION('ref_axis',(-1.,-6.12323399573677E-17,0.));
#30073=DIRECTION('center_axis',(0.,0.,1.));
#30074=DIRECTION('ref_axis',(1.,0.,0.));
#30075=DIRECTION('center_axis',(0.,0.,-1.));
#30076=DIRECTION('ref_axis',(1.,0.,0.));
#30077=DIRECTION('center_axis',(0.,1.26592340881653E-15,-1.));
#30078=DIRECTION('ref_axis',(-1.,-3.0312508555666E-17,0.));
#30079=DIRECTION('',(0.382683432365077,1.22802602600346E-15,-0.923879532511292));
#30080=DIRECTION('center_axis',(0.,0.,1.));
#30081=DIRECTION('ref_axis',(-1.,0.,0.));
#30082=DIRECTION('center_axis',(0.,0.,1.));
#30083=DIRECTION('ref_axis',(-1.,0.,0.));
#30084=DIRECTION('center_axis',(0.,0.,1.));
#30085=DIRECTION('ref_axis',(1.,0.,0.));
#30086=DIRECTION('',(0.,0.,-1.));
#30087=DIRECTION('center_axis',(-1.,0.,0.));
#30088=DIRECTION('ref_axis',(0.,0.,-1.));
#30089=DIRECTION('center_axis',(-1.,0.,0.));
#30090=DIRECTION('ref_axis',(0.,0.,-1.));
#30091=DIRECTION('',(0.707106781186538,-8.65956056235505E-17,-0.707106781186557));
#30092=DIRECTION('center_axis',(1.,0.,0.));
#30093=DIRECTION('ref_axis',(0.,0.,-1.));
#30094=DIRECTION('center_axis',(1.,0.,0.));
#30095=DIRECTION('ref_axis',(0.,0.,-1.));
#30096=DIRECTION('center_axis',(-1.,0.,0.));
#30097=DIRECTION('ref_axis',(0.,0.,-1.));
#30098=DIRECTION('center_axis',(1.,0.,0.));
#30099=DIRECTION('ref_axis',(0.,-1.,0.));
#30100=DIRECTION('center_axis',(-1.,0.,0.));
#30101=DIRECTION('ref_axis',(0.,-1.,0.));
#30102=DIRECTION('center_axis',(-1.,0.,0.));
#30103=DIRECTION('ref_axis',(0.,-1.,0.));
#30104=DIRECTION('',(-0.707106781186546,-0.707106781186549,-8.65956056235495E-17));
#30105=DIRECTION('center_axis',(1.,0.,0.));
#30106=DIRECTION('ref_axis',(0.,-1.,0.));
#30107=DIRECTION('center_axis',(1.,0.,0.));
#30108=DIRECTION('ref_axis',(0.,-1.,0.));
#30109=DIRECTION('center_axis',(1.,0.,0.));
#30110=DIRECTION('ref_axis',(0.,-1.,0.));
#30111=DIRECTION('center_axis',(1.,0.,0.));
#30112=DIRECTION('ref_axis',(0.,-1.,0.));
#30113=DIRECTION('center_axis',(1.,0.,0.));
#30114=DIRECTION('ref_axis',(0.,-1.,0.));
#30115=DIRECTION('center_axis',(-1.,0.,0.));
#30116=DIRECTION('ref_axis',(0.,0.,1.));
#30117=DIRECTION('center_axis',(-1.,0.,0.));
#30118=DIRECTION('ref_axis',(0.,0.,1.));
#30119=DIRECTION('',(-1.,0.,0.));
#30120=DIRECTION('center_axis',(-1.,0.,0.));
#30121=DIRECTION('ref_axis',(0.,0.,1.));
#30122=DIRECTION('center_axis',(-1.,0.,0.));
#30123=DIRECTION('ref_axis',(0.,0.,1.));
#30124=DIRECTION('',(0.707106781186562,8.65956056235476E-17,0.707106781186533));
#30125=DIRECTION('center_axis',(1.,0.,0.));
#30126=DIRECTION('ref_axis',(0.,0.,1.));
#30127=DIRECTION('center_axis',(-1.,0.,0.));
#30128=DIRECTION('ref_axis',(0.,0.,1.));
#30129=DIRECTION('center_axis',(-1.,0.,0.));
#30130=DIRECTION('ref_axis',(0.,0.,1.));
#30131=DIRECTION('center_axis',(-1.,0.,0.));
#30132=DIRECTION('ref_axis',(0.,0.,1.));
#30133=DIRECTION('',(-1.,0.,0.));
#30134=DIRECTION('center_axis',(-0.707106781186541,0.,-0.707106781186554));
#30135=DIRECTION('ref_axis',(-0.707106781186554,0.,0.707106781186541));
#30136=DIRECTION('',(0.577350269189629,-0.577350269189629,-0.577350269189619));
#30137=DIRECTION('',(0.,-1.,0.));
#30138=DIRECTION('',(-0.577350269189629,-0.577350269189629,0.577350269189619));
#30139=DIRECTION('',(-0.577350269189629,0.577350269189629,0.577350269189619));
#30140=DIRECTION('',(0.,1.,0.));
#30141=DIRECTION('',(0.577350269189629,0.577350269189629,-0.577350269189619));
#30142=DIRECTION('center_axis',(0.,0.,1.));
#30143=DIRECTION('ref_axis',(1.,0.,0.));
#30144=DIRECTION('',(-1.,0.,0.));
#30145=DIRECTION('center_axis',(0.,0.,1.));
#30146=DIRECTION('ref_axis',(1.,1.77635683940025E-15,0.));
#30147=DIRECTION('',(0.,1.,0.));
#30148=DIRECTION('center_axis',(0.,0.,1.));
#30149=DIRECTION('ref_axis',(0.,-1.,0.));
#30150=DIRECTION('',(1.,0.,0.));
#30151=DIRECTION('',(0.,1.,0.));
#30152=DIRECTION('center_axis',(0.,0.,-1.));
#30153=DIRECTION('ref_axis',(-1.,3.22973970800045E-15,0.));
#30154=DIRECTION('',(0.,-1.,0.));
#30155=DIRECTION('center_axis',(0.,0.,-1.));
#30156=DIRECTION('ref_axis',(1.,-3.22973970800045E-15,0.));
#30157=DIRECTION('',(0.,1.,0.));
#30158=DIRECTION('center_axis',(0.,0.,-1.));
#30159=DIRECTION('ref_axis',(-1.,3.22973970800045E-15,0.));
#30160=DIRECTION('',(0.,-1.,0.));
#30161=DIRECTION('center_axis',(0.,0.,-1.));
#30162=DIRECTION('ref_axis',(1.,-3.22973970800045E-15,0.));
#30163=DIRECTION('center_axis',(0.,0.707106781186541,-0.707106781186554));
#30164=DIRECTION('ref_axis',(-1.,0.,0.));
#30165=DIRECTION('',(-0.577350269189629,-0.577350269189629,-0.577350269189619));
#30166=DIRECTION('',(1.,0.,0.));
#30167=DIRECTION('',(0.,-0.707106781186554,-0.707106781186541));
#30168=DIRECTION('center_axis',(-0.707106781186548,0.707106781186548,0.));
#30169=DIRECTION('ref_axis',(0.,0.,1.));
#30170=DIRECTION('',(0.,0.,1.));
#30171=DIRECTION('',(0.577350269189622,0.577350269189643,0.577350269189612));
#30172=DIRECTION('',(0.,0.,-1.));
#30173=DIRECTION('center_axis',(-1.,0.,0.));
#30174=DIRECTION('ref_axis',(0.,-1.,0.));
#30175=DIRECTION('center_axis',(1.,0.,0.));
#30176=DIRECTION('ref_axis',(0.,-1.,0.));
#30177=DIRECTION('',(0.382683432365096,-0.923879532511284,1.1314261122877E-16));
#30178=DIRECTION('center_axis',(-1.,0.,0.));
#30179=DIRECTION('ref_axis',(0.,-1.,0.));
#30180=DIRECTION('center_axis',(-1.,0.,0.));
#30181=DIRECTION('ref_axis',(0.,-1.,0.));
#30182=DIRECTION('',(-0.707106781186552,0.707106781186543,8.65956056235488E-17));
#30183=DIRECTION('center_axis',(-1.,0.,0.));
#30184=DIRECTION('ref_axis',(0.,-1.,0.));
#30185=DIRECTION('center_axis',(1.,0.,0.));
#30186=DIRECTION('ref_axis',(0.,0.,-1.));
#30187=DIRECTION('center_axis',(-1.,0.,0.));
#30188=DIRECTION('ref_axis',(0.,1.,0.));
#30189=DIRECTION('',(0.,0.75225657268058,0.658870282270242));
#30190=DIRECTION('center_axis',(1.,0.,0.));
#30191=DIRECTION('ref_axis',(0.,1.,0.));
#30192=DIRECTION('center_axis',(1.,0.,0.));
#30193=DIRECTION('ref_axis',(0.,-1.,0.));
#30194=DIRECTION('center_axis',(1.,0.,0.));
#30195=DIRECTION('ref_axis',(0.,-1.,0.));
#30196=DIRECTION('',(-1.,0.,0.));
#30197=DIRECTION('',(-1.,0.,0.));
#30198=DIRECTION('',(1.,0.,0.));
#30199=DIRECTION('center_axis',(-1.,0.,0.));
#30200=DIRECTION('ref_axis',(0.,2.83276944882399E-16,-1.));
#30201=DIRECTION('center_axis',(0.,0.,1.));
#30202=DIRECTION('ref_axis',(1.,0.,0.));
#30203=DIRECTION('',(0.,0.,1.));
#30204=DIRECTION('center_axis',(0.,0.,1.));
#30205=DIRECTION('ref_axis',(1.,0.,0.));
#30206=DIRECTION('center_axis',(-1.,0.,0.));
#30207=DIRECTION('ref_axis',(0.,-1.,0.));
#30208=DIRECTION('',(-0.923879532511285,0.382683432365094,4.68652040532634E-17));
#30209=DIRECTION('center_axis',(-0.707106781186541,-0.707106781186554,0.));
#30210=DIRECTION('ref_axis',(0.,0.,1.));
#30211=DIRECTION('',(-0.706643908451704,0.706643908451754,0.0361769719037954));
#30212=DIRECTION('',(0.,0.,-1.));
#30213=DIRECTION('',(-0.707106781186554,0.707106781186541,0.));
#30214=DIRECTION('',(0.,0.,1.));
#30215=DIRECTION('center_axis',(1.,0.,0.));
#30216=DIRECTION('ref_axis',(0.,0.,-1.));
#30217=DIRECTION('',(0.,1.,0.));
#30218=DIRECTION('',(0.,-0.256212647338981,0.966620442233429));
#30219=DIRECTION('',(0.,-1.,0.));
#30220=DIRECTION('center_axis',(0.,1.,0.));
#30221=DIRECTION('ref_axis',(-0.999937018558663,0.,0.0112231419848006));
#30222=DIRECTION('center_axis',(0.,1.,0.));
#30223=DIRECTION('ref_axis',(-0.999937018558664,0.,0.0112231419848006));
#30224=DIRECTION('',(-0.659148681788774,0.707106781186549,0.255974637993922));
#30225=DIRECTION('center_axis',(0.,-1.,0.));
#30226=DIRECTION('ref_axis',(-0.999937018558664,0.,0.0112231419848006));
#30227=DIRECTION('',(-2.99369449574795E-14,-0.877058019307039,0.480384461415243));
#30228=DIRECTION('',(2.99369449574799E-14,-0.877058019307036,-0.480384461415249));
#30229=DIRECTION('',(0.468387297258231,0.511424326802648,0.720457144958386));
#30230=DIRECTION('center_axis',(0.,-0.707106781186541,-0.707106781186554));
#30231=DIRECTION('ref_axis',(-1.,0.,0.));
#30232=DIRECTION('',(0.,-0.707106781186554,0.707106781186541));
#30233=DIRECTION('',(-1.,0.,0.));
#30234=DIRECTION('',(-0.577350269189629,0.577350269189629,-0.577350269189619));
#30235=DIRECTION('center_axis',(-0.707106781186548,-0.707106781186548,0.));
#30236=DIRECTION('ref_axis',(0.,0.,1.));
#30237=DIRECTION('',(0.,0.,1.));
#30238=DIRECTION('',(-0.577350269189629,0.577350269189629,-0.577350269189619));
#30239=DIRECTION('',(0.,0.,-1.));
#30240=DIRECTION('center_axis',(0.577350269189622,-0.577350269189622,-0.577350269189633));
#30241=DIRECTION('ref_axis',(-0.707106781186554,0.,-0.707106781186541));
#30242=DIRECTION('',(-0.707106781186554,0.,-0.707106781186541));
#30243=DIRECTION('',(0.707106781186548,0.707106781186548,0.));
#30244=DIRECTION('',(0.,-0.707106781186554,0.707106781186541));
#30245=DIRECTION('center_axis',(0.707106781186548,-0.707106781186548,0.));
#30246=DIRECTION('ref_axis',(0.,0.,-1.));
#30247=DIRECTION('',(0.,0.,-1.));
#30248=DIRECTION('',(0.,0.,1.));
#30249=DIRECTION('',(-0.577350269189622,-0.577350269189643,0.577350269189612));
#30250=DIRECTION('center_axis',(0.577350269189622,0.577350269189622,-0.577350269189633));
#30251=DIRECTION('ref_axis',(-0.707106781186554,0.,-0.707106781186541));
#30252=DIRECTION('',(0.707106781186554,0.,0.707106781186541));
#30253=DIRECTION('',(0.,-0.707106781186554,-0.707106781186541));
#30254=DIRECTION('',(-0.707106781186548,0.707106781186548,0.));
#30255=DIRECTION('center_axis',(0.,0.707106781186541,-0.707106781186554));
#30256=DIRECTION('ref_axis',(-1.,0.,0.));
#30257=DIRECTION('',(0.,0.707106781186554,0.707106781186541));
#30258=DIRECTION('',(1.,0.,0.));
#30259=DIRECTION('',(-1.,0.,0.));
#30260=DIRECTION('center_axis',(0.,0.,1.));
#30261=DIRECTION('ref_axis',(0.,1.,0.));
#30262=DIRECTION('',(-0.707106781186554,0.,0.707106781186541));
#30263=DIRECTION('center_axis',(0.,0.,-1.));
#30264=DIRECTION('ref_axis',(0.,1.,0.));
#30265=DIRECTION('center_axis',(0.,0.,1.));
#30266=DIRECTION('ref_axis',(0.,1.,0.));
#30267=DIRECTION('center_axis',(-0.707106781186541,0.,-0.707106781186554));
#30268=DIRECTION('ref_axis',(-0.707106781186554,0.,0.707106781186541));
#30269=DIRECTION('',(-0.707106781186554,0.,0.707106781186541));
#30270=DIRECTION('',(0.,1.,0.));
#30271=DIRECTION('',(0.,-1.,0.));
#30272=DIRECTION('center_axis',(0.,0.,1.));
#30273=DIRECTION('ref_axis',(-1.,0.,0.));
#30274=DIRECTION('',(0.,-0.707106781186554,0.707106781186541));
#30275=DIRECTION('center_axis',(0.,0.,-1.));
#30276=DIRECTION('ref_axis',(-1.,0.,0.));
#30277=DIRECTION('center_axis',(0.,0.,1.));
#30278=DIRECTION('ref_axis',(-1.,0.,0.));
#30279=DIRECTION('center_axis',(0.,-0.707106781186541,-0.707106781186554));
#30280=DIRECTION('ref_axis',(-1.,0.,0.));
#30281=DIRECTION('',(1.,0.,0.));
#30282=DIRECTION('',(-1.,0.,0.));
#30283=DIRECTION('center_axis',(0.707106781186548,0.707106781186548,0.));
#30284=DIRECTION('ref_axis',(0.,0.,-1.));
#30285=DIRECTION('',(0.,0.,-1.));
#30286=DIRECTION('',(0.,0.,1.));
#30287=DIRECTION('',(0.577350269189629,-0.577350269189629,-0.577350269189619));
#30288=DIRECTION('center_axis',(0.707106781186541,0.,-0.707106781186554));
#30289=DIRECTION('ref_axis',(-0.707106781186554,0.,-0.707106781186541));
#30290=DIRECTION('',(0.,1.,0.));
#30291=DIRECTION('',(0.,-1.,0.));
#30292=DIRECTION('center_axis',(0.,0.707106781186541,-0.707106781186554));
#30293=DIRECTION('ref_axis',(-1.,0.,0.));
#30294=DIRECTION('',(-1.,0.,0.));
#30295=DIRECTION('',(1.,0.,0.));
#30296=DIRECTION('center_axis',(0.,-0.707106781186541,-0.707106781186554));
#30297=DIRECTION('ref_axis',(-1.,0.,0.));
#30298=DIRECTION('',(-1.,0.,0.));
#30299=DIRECTION('',(1.,0.,0.));
#30300=DIRECTION('center_axis',(0.,0.,1.));
#30301=DIRECTION('ref_axis',(1.,1.77635683940025E-15,0.));
#30302=DIRECTION('center_axis',(0.,0.,-1.));
#30303=DIRECTION('ref_axis',(1.,1.77635683940025E-15,0.));
#30304=DIRECTION('',(-0.49497474683058,-0.50497524691812,-0.707106781186538));
#30305=DIRECTION('center_axis',(0.,0.,1.));
#30306=DIRECTION('ref_axis',(0.,-1.,0.));
#30307=DIRECTION('',(0.494974746830587,-0.504975246918101,0.707106781186547));
#30308=DIRECTION('center_axis',(0.,0.,-1.));
#30309=DIRECTION('ref_axis',(0.,-1.,0.));
#30310=DIRECTION('',(-0.468387297258238,0.511424326802607,-0.72045714495841));
#30311=DIRECTION('center_axis',(0.,-1.,0.));
#30312=DIRECTION('ref_axis',(1.,0.,0.));
#30313=DIRECTION('',(0.,0.,1.));
#30314=DIRECTION('',(1.,0.,0.));
#30315=DIRECTION('',(0.,0.,1.));
#30316=DIRECTION('center_axis',(0.,0.,1.));
#30317=DIRECTION('ref_axis',(0.,-1.,0.));
#30318=DIRECTION('',(0.,0.,1.));
#30319=DIRECTION('center_axis',(0.,0.,1.));
#30320=DIRECTION('ref_axis',(0.,-1.,0.));
#30321=DIRECTION('center_axis',(1.,0.,0.));
#30322=DIRECTION('ref_axis',(0.,0.,-1.));
#30323=DIRECTION('',(0.,-1.,0.));
#30324=DIRECTION('',(0.,0.,1.));
#30325=DIRECTION('',(0.,0.877058019307042,-0.480384461415237));
#30326=DIRECTION('',(0.,1.,0.));
#30327=DIRECTION('',(0.,0.256212647338981,-0.966620442233429));
#30328=DIRECTION('center_axis',(1.,0.,0.));
#30329=DIRECTION('ref_axis',(0.,2.83276944882399E-16,-1.));
#30330=DIRECTION('',(0.,0.256212647338981,0.966620442233429));
#30331=DIRECTION('',(0.,1.,0.));
#30332=DIRECTION('',(0.,0.877058019307039,0.480384461415243));
#30333=DIRECTION('',(0.,0.,-1.));
#30334=DIRECTION('center_axis',(1.,0.,0.));
#30335=DIRECTION('ref_axis',(0.,6.12323399573677E-17,1.));
#30336=DIRECTION('',(0.,0.,1.));
#30337=DIRECTION('',(0.,1.,0.));
#30338=DIRECTION('center_axis',(0.,1.,0.));
#30339=DIRECTION('ref_axis',(0.707106781186543,0.,-0.707106781186552));
#30340=DIRECTION('center_axis',(-1.,0.,0.));
#30341=DIRECTION('ref_axis',(0.,-1.,0.));
#30342=DIRECTION('',(0.,-1.,0.));
#30343=DIRECTION('center_axis',(1.,0.,0.));
#30344=DIRECTION('ref_axis',(0.,1.,0.));
#30345=DIRECTION('',(0.,1.,0.));
#30346=DIRECTION('center_axis',(0.,0.,1.));
#30347=DIRECTION('ref_axis',(1.,0.,0.));
#30348=DIRECTION('center_axis',(0.,0.,1.));
#30349=DIRECTION('ref_axis',(1.,0.,0.));
#30350=DIRECTION('',(0.,1.,0.));
#30351=DIRECTION('center_axis',(0.,0.,-1.));
#30352=DIRECTION('ref_axis',(-1.,0.,0.));
#30353=DIRECTION('',(0.,-1.,0.));
#30354=DIRECTION('center_axis',(0.,0.,-1.));
#30355=DIRECTION('ref_axis',(1.,0.,0.));
#30356=DIRECTION('',(0.,1.,0.));
#30357=DIRECTION('center_axis',(0.,0.,-1.));
#30358=DIRECTION('ref_axis',(-1.,0.,0.));
#30359=DIRECTION('',(0.,-1.,0.));
#30360=DIRECTION('center_axis',(0.,0.,-1.));
#30361=DIRECTION('ref_axis',(1.,0.,0.));
#30362=DIRECTION('center_axis',(0.707106781186566,0.,-0.707106781186529));
#30363=DIRECTION('ref_axis',(-0.707106781186529,0.,-0.707106781186566));
#30364=DIRECTION('',(-0.707106781186529,0.,-0.707106781186566));
#30365=DIRECTION('',(0.707106781186529,0.,0.707106781186566));
#30366=DIRECTION('',(0.,-1.,0.));
#30367=DIRECTION('center_axis',(0.,0.,-1.));
#30368=DIRECTION('ref_axis',(-1.,3.22973970800045E-15,0.));
#30369=DIRECTION('',(0.707106781186554,0.,-0.707106781186541));
#30370=DIRECTION('center_axis',(0.,0.,1.));
#30371=DIRECTION('ref_axis',(-1.,3.22973970800045E-15,0.));
#30372=DIRECTION('center_axis',(-0.707106781186566,0.,-0.707106781186529));
#30373=DIRECTION('ref_axis',(-0.707106781186529,0.,0.707106781186566));
#30374=DIRECTION('',(0.707106781186529,0.,-0.707106781186566));
#30375=DIRECTION('',(0.,1.,0.));
#30376=DIRECTION('center_axis',(0.,0.,-1.));
#30377=DIRECTION('ref_axis',(1.,-3.22973970800045E-15,0.));
#30378=DIRECTION('center_axis',(0.,0.,1.));
#30379=DIRECTION('ref_axis',(1.,-3.22973970800045E-15,0.));
#30380=DIRECTION('center_axis',(0.,0.,-1.));
#30381=DIRECTION('ref_axis',(-1.,3.22973970800045E-15,0.));
#30382=DIRECTION('',(0.,0.,-1.));
#30383=DIRECTION('center_axis',(0.,0.,-1.));
#30384=DIRECTION('ref_axis',(-1.,3.22973970800045E-15,0.));
#30385=DIRECTION('',(0.,0.,-1.));
#30386=DIRECTION('center_axis',(-1.,0.,0.));
#30387=DIRECTION('ref_axis',(0.,1.,0.));
#30388=DIRECTION('',(0.,0.,-1.));
#30389=DIRECTION('',(0.,1.,0.));
#30390=DIRECTION('center_axis',(0.707106781186541,0.,-0.707106781186554));
#30391=DIRECTION('ref_axis',(-0.707106781186554,0.,-0.707106781186541));
#30392=DIRECTION('',(-0.707106781186554,0.,-0.707106781186541));
#30393=DIRECTION('',(0.707106781186554,0.,0.707106781186541));
#30394=DIRECTION('',(0.,-1.,0.));
#30395=DIRECTION('center_axis',(0.,0.,-1.));
#30396=DIRECTION('ref_axis',(-1.,0.,0.));
#30397=DIRECTION('',(0.707106781186554,0.,-0.707106781186541));
#30398=DIRECTION('center_axis',(0.,0.,1.));
#30399=DIRECTION('ref_axis',(-1.,0.,0.));
#30400=DIRECTION('center_axis',(-0.707106781186541,0.,-0.707106781186554));
#30401=DIRECTION('ref_axis',(-0.707106781186554,0.,0.707106781186541));
#30402=DIRECTION('',(0.707106781186554,0.,-0.707106781186541));
#30403=DIRECTION('',(0.,1.,0.));
#30404=DIRECTION('center_axis',(0.,0.,-1.));
#30405=DIRECTION('ref_axis',(1.,0.,0.));
#30406=DIRECTION('center_axis',(0.,0.,1.));
#30407=DIRECTION('ref_axis',(1.,0.,0.));
#30408=DIRECTION('center_axis',(0.,0.,-1.));
#30409=DIRECTION('ref_axis',(-1.,0.,0.));
#30410=DIRECTION('',(0.,0.,-1.));
#30411=DIRECTION('center_axis',(0.,0.,-1.));
#30412=DIRECTION('ref_axis',(-1.,0.,0.));
#30413=DIRECTION('',(0.,0.,-1.));
#30414=DIRECTION('center_axis',(-1.,0.,0.));
#30415=DIRECTION('ref_axis',(0.,1.,0.));
#30416=DIRECTION('',(0.,0.,-1.));
#30417=DIRECTION('',(0.,1.,0.));
#30418=DIRECTION('center_axis',(0.707106781186541,0.,-0.707106781186554));
#30419=DIRECTION('ref_axis',(-0.707106781186554,0.,-0.707106781186541));
#30420=DIRECTION('',(-0.707106781186554,0.,-0.707106781186541));
#30421=DIRECTION('',(0.707106781186554,0.,0.707106781186541));
#30422=DIRECTION('',(0.,-1.,0.));
#30423=DIRECTION('center_axis',(0.,0.,-1.));
#30424=DIRECTION('ref_axis',(-1.,0.,0.));
#30425=DIRECTION('',(0.707106781186554,0.,-0.707106781186541));
#30426=DIRECTION('center_axis',(0.,0.,1.));
#30427=DIRECTION('ref_axis',(-1.,0.,0.));
#30428=DIRECTION('center_axis',(-0.707106781186541,0.,-0.707106781186554));
#30429=DIRECTION('ref_axis',(-0.707106781186554,0.,0.707106781186541));
#30430=DIRECTION('',(0.707106781186554,0.,-0.707106781186541));
#30431=DIRECTION('',(0.,1.,0.));
#30432=DIRECTION('center_axis',(0.,0.,-1.));
#30433=DIRECTION('ref_axis',(1.,0.,0.));
#30434=DIRECTION('center_axis',(0.,0.,1.));
#30435=DIRECTION('ref_axis',(1.,0.,0.));
#30436=DIRECTION('center_axis',(0.,0.,-1.));
#30437=DIRECTION('ref_axis',(-1.,0.,0.));
#30438=DIRECTION('',(0.,0.,-1.));
#30439=DIRECTION('center_axis',(0.,0.,-1.));
#30440=DIRECTION('ref_axis',(-1.,0.,0.));
#30441=DIRECTION('',(0.,0.,-1.));
#30442=DIRECTION('center_axis',(-1.,0.,0.));
#30443=DIRECTION('ref_axis',(0.,1.,0.));
#30444=DIRECTION('',(0.,0.,-1.));
#30445=DIRECTION('',(0.,1.,0.));
#30446=DIRECTION('center_axis',(0.707106781186566,0.,-0.707106781186529));
#30447=DIRECTION('ref_axis',(-0.707106781186529,0.,-0.707106781186566));
#30448=DIRECTION('',(-0.707106781186529,0.,-0.707106781186566));
#30449=DIRECTION('',(0.707106781186529,0.,0.707106781186566));
#30450=DIRECTION('',(0.,-1.,0.));
#30451=DIRECTION('center_axis',(0.,0.,-1.));
#30452=DIRECTION('ref_axis',(-1.,3.22973970800045E-15,0.));
#30453=DIRECTION('',(0.707106781186554,0.,-0.707106781186541));
#30454=DIRECTION('center_axis',(0.,0.,1.));
#30455=DIRECTION('ref_axis',(-1.,3.22973970800045E-15,0.));
#30456=DIRECTION('center_axis',(-0.707106781186566,0.,-0.707106781186529));
#30457=DIRECTION('ref_axis',(-0.707106781186529,0.,0.707106781186566));
#30458=DIRECTION('',(0.707106781186529,0.,-0.707106781186566));
#30459=DIRECTION('',(0.,1.,0.));
#30460=DIRECTION('center_axis',(0.,0.,-1.));
#30461=DIRECTION('ref_axis',(1.,-3.22973970800045E-15,0.));
#30462=DIRECTION('center_axis',(0.,0.,1.));
#30463=DIRECTION('ref_axis',(1.,-3.22973970800045E-15,0.));
#30464=DIRECTION('center_axis',(0.,0.,-1.));
#30465=DIRECTION('ref_axis',(-1.,3.22973970800045E-15,0.));
#30466=DIRECTION('',(0.,0.,-1.));
#30467=DIRECTION('center_axis',(0.,0.,-1.));
#30468=DIRECTION('ref_axis',(-1.,3.22973970800045E-15,0.));
#30469=DIRECTION('',(0.,0.,-1.));
#30470=DIRECTION('center_axis',(-1.,0.,0.));
#30471=DIRECTION('ref_axis',(0.,1.,0.));
#30472=DIRECTION('',(0.,0.,-1.));
#30473=DIRECTION('',(0.,1.,0.));
#30474=DIRECTION('center_axis',(-1.,0.,0.));
#30475=DIRECTION('ref_axis',(0.,0.,-1.));
#30476=DIRECTION('center_axis',(-1.,0.,0.));
#30477=DIRECTION('ref_axis',(0.,0.,-1.));
#30478=DIRECTION('',(0.707106781186538,-8.65956056235505E-17,-0.707106781186557));
#30479=DIRECTION('center_axis',(1.,0.,0.));
#30480=DIRECTION('ref_axis',(0.,0.,-1.));
#30481=DIRECTION('center_axis',(1.,0.,0.));
#30482=DIRECTION('ref_axis',(0.,0.,-1.));
#30483=DIRECTION('center_axis',(-1.,0.,0.));
#30484=DIRECTION('ref_axis',(0.,0.,-1.));
#30485=DIRECTION('center_axis',(-1.,0.,0.));
#30486=DIRECTION('ref_axis',(0.,0.,1.));
#30487=DIRECTION('center_axis',(-1.,0.,0.));
#30488=DIRECTION('ref_axis',(0.,0.,1.));
#30489=DIRECTION('',(-1.,0.,0.));
#30490=DIRECTION('center_axis',(-1.,0.,0.));
#30491=DIRECTION('ref_axis',(0.,0.,1.));
#30492=DIRECTION('center_axis',(-1.,0.,0.));
#30493=DIRECTION('ref_axis',(0.,0.,1.));
#30494=DIRECTION('',(0.707106781186542,8.659560562355E-17,0.707106781186553));
#30495=DIRECTION('center_axis',(1.,0.,0.));
#30496=DIRECTION('ref_axis',(0.,0.,1.));
#30497=DIRECTION('center_axis',(-1.,0.,0.));
#30498=DIRECTION('ref_axis',(0.,0.,1.));
#30499=DIRECTION('center_axis',(-1.,0.,0.));
#30500=DIRECTION('ref_axis',(0.,0.,1.));
#30501=DIRECTION('center_axis',(-1.,0.,0.));
#30502=DIRECTION('ref_axis',(0.,0.,1.));
#30503=DIRECTION('',(-1.,0.,0.));
#30504=DIRECTION('center_axis',(0.707106781186566,0.,0.707106781186529));
#30505=DIRECTION('ref_axis',(0.707106781186529,0.,-0.707106781186566));
#30506=DIRECTION('',(-0.707106781186529,0.,0.707106781186566));
#30507=DIRECTION('',(0.,-1.,0.));
#30508=DIRECTION('',(0.707106781186529,0.,-0.707106781186566));
#30509=DIRECTION('center_axis',(0.,0.,1.));
#30510=DIRECTION('ref_axis',(1.,-3.22973970800045E-15,0.));
#30511=DIRECTION('',(0.707106781186554,0.,0.707106781186541));
#30512=DIRECTION('center_axis',(0.,0.,1.));
#30513=DIRECTION('ref_axis',(1.,-3.22973970800045E-15,0.));
#30514=DIRECTION('center_axis',(0.,0.,-1.));
#30515=DIRECTION('ref_axis',(1.,-3.22973970800045E-15,0.));
#30516=DIRECTION('center_axis',(-0.707106781186566,0.,0.707106781186529));
#30517=DIRECTION('ref_axis',(0.707106781186529,0.,0.707106781186566));
#30518=DIRECTION('',(0.707106781186529,0.,0.707106781186566));
#30519=DIRECTION('',(0.,1.,0.));
#30520=DIRECTION('',(0.,-1.,0.));
#30521=DIRECTION('center_axis',(0.,0.,1.));
#30522=DIRECTION('ref_axis',(-1.,3.22973970800045E-15,0.));
#30523=DIRECTION('center_axis',(0.,0.,1.));
#30524=DIRECTION('ref_axis',(-1.,3.22973970800045E-15,0.));
#30525=DIRECTION('center_axis',(0.,0.,-1.));
#30526=DIRECTION('ref_axis',(1.,-3.22973970800045E-15,0.));
#30527=DIRECTION('',(0.,0.,-1.));
#30528=DIRECTION('center_axis',(0.,0.,1.));
#30529=DIRECTION('ref_axis',(1.,0.,0.));
#30530=DIRECTION('',(0.,-1.,0.));
#30531=DIRECTION('',(1.,0.,0.));
#30532=DIRECTION('',(-0.695004915696666,0.719004984097795,0.));
#30533=DIRECTION('',(0.,-1.,0.));
#30534=DIRECTION('',(0.707106781186554,0.707106781186541,0.));
#30535=DIRECTION('',(1.,0.,0.));
#30536=DIRECTION('',(0.,-1.,0.));
#30537=DIRECTION('',(1.,0.,0.));
#30538=DIRECTION('',(0.69500491569666,0.719004984097801,0.));
#30539=DIRECTION('',(1.,0.,0.));
#30540=DIRECTION('',(0.,-1.,0.));
#30541=DIRECTION('center_axis',(0.,0.,-1.));
#30542=DIRECTION('ref_axis',(1.,1.77635683940025E-15,0.));
#30543=DIRECTION('',(1.,0.,0.));
#30544=DIRECTION('center_axis',(0.,0.,-1.));
#30545=DIRECTION('ref_axis',(0.,1.,0.));
#30546=DIRECTION('',(0.,1.,0.));
#30547=DIRECTION('center_axis',(0.,0.,-1.));
#30548=DIRECTION('ref_axis',(-1.,0.,0.));
#30549=DIRECTION('',(-1.,0.,0.));
#30550=DIRECTION('center_axis',(0.,0.,-1.));
#30551=DIRECTION('ref_axis',(0.,-1.,0.));
#30552=DIRECTION('',(0.,-1.,0.));
#30553=DIRECTION('center_axis',(0.,0.,1.));
#30554=DIRECTION('ref_axis',(1.,0.,0.));
#30555=DIRECTION('',(0.,1.,0.));
#30556=DIRECTION('center_axis',(0.,0.,1.));
#30557=DIRECTION('ref_axis',(-1.,0.,0.));
#30558=DIRECTION('',(0.,-1.,0.));
#30559=DIRECTION('center_axis',(0.,0.,1.));
#30560=DIRECTION('ref_axis',(1.,-3.22973970800045E-15,0.));
#30561=DIRECTION('',(0.,1.,0.));
#30562=DIRECTION('center_axis',(0.,0.,1.));
#30563=DIRECTION('ref_axis',(-1.,3.22973970800045E-15,0.));
#30564=DIRECTION('',(0.,-1.,0.));
#30565=DIRECTION('center_axis',(0.,0.,1.));
#30566=DIRECTION('ref_axis',(1.,0.,0.));
#30567=DIRECTION('',(0.,1.,0.));
#30568=DIRECTION('center_axis',(0.,0.,1.));
#30569=DIRECTION('ref_axis',(-1.,0.,0.));
#30570=DIRECTION('center_axis',(0.707106781186541,0.,0.707106781186554));
#30571=DIRECTION('ref_axis',(0.707106781186554,0.,-0.707106781186541));
#30572=DIRECTION('',(-0.707106781186554,0.,0.707106781186541));
#30573=DIRECTION('',(0.707106781186554,0.,-0.707106781186541));
#30574=DIRECTION('center_axis',(0.,0.,1.));
#30575=DIRECTION('ref_axis',(1.,0.,0.));
#30576=DIRECTION('',(0.707106781186554,0.,0.707106781186541));
#30577=DIRECTION('center_axis',(0.,0.,-1.));
#30578=DIRECTION('ref_axis',(1.,0.,0.));
#30579=DIRECTION('center_axis',(-0.707106781186541,0.,0.707106781186554));
#30580=DIRECTION('ref_axis',(0.707106781186554,0.,0.707106781186541));
#30581=DIRECTION('',(0.707106781186554,0.,0.707106781186541));
#30582=DIRECTION('',(0.,-1.,0.));
#30583=DIRECTION('center_axis',(0.,0.,1.));
#30584=DIRECTION('ref_axis',(-1.,0.,0.));
#30585=DIRECTION('center_axis',(0.,0.,-1.));
#30586=DIRECTION('ref_axis',(1.,0.,0.));
#30587=DIRECTION('',(0.,0.,-1.));
#30588=DIRECTION('center_axis',(0.707106781186541,0.,0.707106781186554));
#30589=DIRECTION('ref_axis',(0.707106781186554,0.,-0.707106781186541));
#30590=DIRECTION('',(-0.707106781186554,0.,0.707106781186541));
#30591=DIRECTION('',(0.707106781186554,0.,-0.707106781186541));
#30592=DIRECTION('center_axis',(0.,0.,1.));
#30593=DIRECTION('ref_axis',(1.,0.,0.));
#30594=DIRECTION('',(0.707106781186554,0.,0.707106781186541));
#30595=DIRECTION('center_axis',(0.,0.,-1.));
#30596=DIRECTION('ref_axis',(1.,0.,0.));
#30597=DIRECTION('center_axis',(-0.707106781186541,0.,0.707106781186554));
#30598=DIRECTION('ref_axis',(0.707106781186554,0.,0.707106781186541));
#30599=DIRECTION('',(0.707106781186554,0.,0.707106781186541));
#30600=DIRECTION('',(0.,-1.,0.));
#30601=DIRECTION('center_axis',(0.,0.,1.));
#30602=DIRECTION('ref_axis',(-1.,0.,0.));
#30603=DIRECTION('center_axis',(0.,0.,-1.));
#30604=DIRECTION('ref_axis',(1.,0.,0.));
#30605=DIRECTION('',(0.,0.,-1.));
#30606=DIRECTION('center_axis',(0.707106781186566,0.,0.707106781186529));
#30607=DIRECTION('ref_axis',(0.707106781186529,0.,-0.707106781186566));
#30608=DIRECTION('',(-0.707106781186529,0.,0.707106781186566));
#30609=DIRECTION('',(0.707106781186529,0.,-0.707106781186566));
#30610=DIRECTION('center_axis',(0.,0.,1.));
#30611=DIRECTION('ref_axis',(1.,-3.22973970800045E-15,0.));
#30612=DIRECTION('',(0.707106781186554,0.,0.707106781186541));
#30613=DIRECTION('center_axis',(0.,0.,-1.));
#30614=DIRECTION('ref_axis',(1.,-3.22973970800045E-15,0.));
#30615=DIRECTION('center_axis',(-0.707106781186566,0.,0.707106781186529));
#30616=DIRECTION('ref_axis',(0.707106781186529,0.,0.707106781186566));
#30617=DIRECTION('',(0.707106781186529,0.,0.707106781186566));
#30618=DIRECTION('',(0.,-1.,0.));
#30619=DIRECTION('center_axis',(0.,0.,1.));
#30620=DIRECTION('ref_axis',(-1.,3.22973970800045E-15,0.));
#30621=DIRECTION('center_axis',(0.,0.,-1.));
#30622=DIRECTION('ref_axis',(1.,-3.22973970800045E-15,0.));
#30623=DIRECTION('',(0.,0.,-1.));
#30624=DIRECTION('',(-0.468387297256998,-0.511424326801133,0.720457144960262));
#30625=DIRECTION('center_axis',(0.,0.,-1.));
#30626=DIRECTION('ref_axis',(1.,1.77635683940025E-15,0.));
#30627=DIRECTION('',(0.,-0.707106781186566,0.707106781186529));
#30628=DIRECTION('',(0.494974746830587,0.504975246918101,-0.707106781186547));
#30629=DIRECTION('center_axis',(0.,0.,1.));
#30630=DIRECTION('ref_axis',(1.,1.77635683940025E-15,0.));
#30631=DIRECTION('center_axis',(0.,0.707106781186541,0.707106781186554));
#30632=DIRECTION('ref_axis',(1.,0.,0.));
#30633=DIRECTION('',(0.,-0.707106781186554,0.707106781186541));
#30634=DIRECTION('',(-1.,0.,0.));
#30635=DIRECTION('center_axis',(0.,0.,-1.));
#30636=DIRECTION('ref_axis',(0.,1.,0.));
#30637=DIRECTION('',(0.707106781186554,0.,0.707106781186541));
#30638=DIRECTION('center_axis',(0.,0.,1.));
#30639=DIRECTION('ref_axis',(0.,1.,0.));
#30640=DIRECTION('center_axis',(-0.707106781186541,0.,0.707106781186554));
#30641=DIRECTION('ref_axis',(0.707106781186554,0.,0.707106781186541));
#30642=DIRECTION('',(0.707106781186554,0.,0.707106781186541));
#30643=DIRECTION('',(0.,-1.,0.));
#30644=DIRECTION('center_axis',(0.,0.,-1.));
#30645=DIRECTION('ref_axis',(-1.,0.,0.));
#30646=DIRECTION('',(0.,0.707106781186554,0.707106781186541));
#30647=DIRECTION('center_axis',(0.,0.,1.));
#30648=DIRECTION('ref_axis',(-1.,0.,0.));
#30649=DIRECTION('center_axis',(0.,-0.707106781186541,0.707106781186554));
#30650=DIRECTION('ref_axis',(1.,0.,0.));
#30651=DIRECTION('',(0.,0.707106781186554,0.707106781186541));
#30652=DIRECTION('center_axis',(0.,0.,-1.));
#30653=DIRECTION('ref_axis',(0.,-1.,0.));
#30654=DIRECTION('',(-0.494974746830587,0.504975246918101,0.707106781186547));
#30655=DIRECTION('',(0.468387297257005,-0.511424326801092,-0.720457144960286));
#30656=DIRECTION('center_axis',(0.,1.,0.));
#30657=DIRECTION('ref_axis',(0.707106781186552,0.,0.707106781186543));
#30658=DIRECTION('center_axis',(0.,-0.792531591590824,-0.609830858788332));
#30659=DIRECTION('ref_axis',(7.33239017272468E-17,-0.609830858788332,0.792531591590824));
#30660=DIRECTION('center_axis',(0.,0.,1.));
#30661=DIRECTION('ref_axis',(-1.,0.,0.));
#30662=DIRECTION('',(0.,0.,1.));
#30663=DIRECTION('center_axis',(-1.,0.,0.));
#30664=DIRECTION('ref_axis',(0.,-1.,0.));
#30665=DIRECTION('',(0.,0.,1.));
#30666=DIRECTION('center_axis',(0.,0.,1.));
#30667=DIRECTION('ref_axis',(0.,1.,0.));
#30668=DIRECTION('',(0.,0.,1.));
#30669=DIRECTION('center_axis',(0.,1.,0.));
#30670=DIRECTION('ref_axis',(-1.,0.,0.));
#30671=DIRECTION('',(0.,0.,1.));
#30672=DIRECTION('center_axis',(-0.707106781186541,0.707106781186554,0.));
#30673=DIRECTION('ref_axis',(0.,0.,1.));
#30674=DIRECTION('',(0.,0.,-1.));
#30675=DIRECTION('',(0.,0.,1.));
#30676=DIRECTION('center_axis',(0.,-1.,0.));
#30677=DIRECTION('ref_axis',(-0.999937018558663,0.,0.0112231419848006));
#30678=DIRECTION('center_axis',(0.,1.,0.));
#30679=DIRECTION('ref_axis',(-0.999937018558664,0.,0.0112231419848006));
#30680=DIRECTION('',(0.659148681788774,0.707106781186549,-0.255974637993922));
#30681=DIRECTION('center_axis',(0.,-1.,0.));
#30682=DIRECTION('ref_axis',(-0.999937018558664,0.,0.0112231419848006));
#30683=DIRECTION('',(-0.658168284632395,-0.706843019174437,0.259205430784961));
#30684=DIRECTION('',(0.658168284632367,-0.70684301917446,-0.259205430784969));
#30685=DIRECTION('center_axis',(0.,1.,0.));
#30686=DIRECTION('ref_axis',(0.,0.,1.));
#30687=DIRECTION('',(1.,0.,0.));
#30688=DIRECTION('',(0.,0.,1.));
#30689=DIRECTION('center_axis',(1.,0.,0.));
#30690=DIRECTION('ref_axis',(0.,1.,0.));
#30691=DIRECTION('',(1.,0.,0.));
#30692=DIRECTION('center_axis',(-1.,0.,0.));
#30693=DIRECTION('ref_axis',(0.,6.12323399573677E-17,1.));
#30694=DIRECTION('center_axis',(0.,-1.,0.));
#30695=DIRECTION('ref_axis',(0.,0.,-1.));
#30696=DIRECTION('',(0.,0.,-1.));
#30697=DIRECTION('center_axis',(-0.70710678118654,-0.683503869536805,0.181169700359153));
#30698=DIRECTION('ref_axis',(0.24819572925489,0.,0.968709904966205));
#30699=DIRECTION('',(0.,-0.256212647338981,-0.966620442233429));
#30700=DIRECTION('',(0.,0.256212647338981,0.966620442233429));
#30701=DIRECTION('center_axis',(-0.70710678118654,-0.683503869536805,0.181169700359153));
#30702=DIRECTION('ref_axis',(-0.662116968503032,0.729946888703702,0.169642741348226));
#30703=DIRECTION('center_axis',(1.,0.,0.));
#30704=DIRECTION('ref_axis',(0.,0.,-1.));
#30705=DIRECTION('',(0.,1.,0.));
#30706=DIRECTION('center_axis',(0.,1.,0.));
#30707=DIRECTION('ref_axis',(-0.999937018558664,0.,0.0112231419848006));
#30708=DIRECTION('center_axis',(-0.707106781186546,0.683503869536799,0.181169700359152));
#30709=DIRECTION('ref_axis',(-0.662116968503027,-0.729946888703707,0.169642741348222));
#30710=DIRECTION('center_axis',(-0.707106781186546,0.683503869536799,0.181169700359152));
#30711=DIRECTION('ref_axis',(0.248195729254886,0.,0.968709904966206));
#30712=DIRECTION('',(0.,0.256212647338981,-0.966620442233429));
#30713=DIRECTION('center_axis',(0.,0.966620442233429,0.256212647338981));
#30714=DIRECTION('ref_axis',(0.,-0.256212647338981,0.966620442233429));
#30715=DIRECTION('',(0.,-0.256212647338981,0.966620442233429));
#30716=DIRECTION('center_axis',(0.,-0.256212647338981,0.966620442233429));
#30717=DIRECTION('ref_axis',(0.707106781186545,0.683503869536801,0.181169700359147));
#30718=DIRECTION('center_axis',(0.,0.256212647338975,-0.966620442233431));
#30719=DIRECTION('ref_axis',(0.,0.966620442233431,0.256212647338975));
#30720=DIRECTION('center_axis',(0.,0.792531591590825,-0.609830858788332));
#30721=DIRECTION('ref_axis',(1.46647803454493E-16,0.609830858788331,0.792531591590825));
#30722=DIRECTION('center_axis',(-1.22056273718388E-14,0.256212647338986,
0.966620442233428));
#30723=DIRECTION('ref_axis',(0.,-0.966620442233428,0.256212647338986));
#30724=DIRECTION('center_axis',(0.,-0.256212647338981,-0.966620442233429));
#30725=DIRECTION('ref_axis',(0.707106781186543,-0.683503869536803,0.181169700359147));
#30726=DIRECTION('',(0.,-0.256212647338981,-0.966620442233429));
#30727=DIRECTION('center_axis',(0.,-0.966620442233429,0.256212647338981));
#30728=DIRECTION('ref_axis',(0.,-0.256212647338981,-0.966620442233429));
#30729=DIRECTION('center_axis',(0.,0.,1.));
#30730=DIRECTION('ref_axis',(0.707106781186545,0.70710678118655,0.));
#30731=DIRECTION('center_axis',(0.,0.,-1.));
#30732=DIRECTION('ref_axis',(0.,1.,0.));
#30733=DIRECTION('center_axis',(0.,-0.707106781186549,0.707106781186546));
#30734=DIRECTION('ref_axis',(0.,-0.707106781186546,-0.707106781186549));
#30735=DIRECTION('center_axis',(0.,1.,0.));
#30736=DIRECTION('ref_axis',(0.707106781186552,0.,0.707106781186543));
#30737=DIRECTION('center_axis',(-2.09345661157836E-15,-0.707106781186549,
-0.707106781186546));
#30738=DIRECTION('ref_axis',(2.09345661157836E-15,-0.707106781186546,0.707106781186549));
#30739=DIRECTION('center_axis',(-1.,0.,0.));
#30740=DIRECTION('ref_axis',(0.,0.,1.));
#30741=DIRECTION('center_axis',(0.,0.,1.));
#30742=DIRECTION('ref_axis',(0.,-1.,0.));
#30743=DIRECTION('center_axis',(0.,0.,-1.));
#30744=DIRECTION('ref_axis',(0.707106781186545,-0.70710678118655,0.));
#30745=DIRECTION('center_axis',(0.,1.,0.));
#30746=DIRECTION('ref_axis',(0.707106781186552,0.,0.707106781186543));
#30747=DIRECTION('center_axis',(0.,0.,1.));
#30748=DIRECTION('ref_axis',(1.,1.77635683940025E-15,0.));
#30749=DIRECTION('center_axis',(1.,0.,0.));
#30750=DIRECTION('ref_axis',(0.,0.,-1.));
#30751=DIRECTION('center_axis',(1.,0.,0.));
#30752=DIRECTION('ref_axis',(0.,-1.,0.));
#30753=DIRECTION('center_axis',(1.,0.,0.));
#30754=DIRECTION('ref_axis',(0.,-1.,0.));
#30755=DIRECTION('center_axis',(1.,0.,0.));
#30756=DIRECTION('ref_axis',(0.,-1.,0.));
#30757=DIRECTION('center_axis',(1.,0.,0.));
#30758=DIRECTION('ref_axis',(0.,-1.,0.));
#30759=DIRECTION('center_axis',(-1.,0.,0.));
#30760=DIRECTION('ref_axis',(0.,0.,1.));
#30761=DIRECTION('',(-0.515038074910054,-1.04972719113862E-16,-0.857167300702112));
#30762=DIRECTION('center_axis',(-1.,0.,0.));
#30763=DIRECTION('ref_axis',(0.,0.,1.));
#30764=DIRECTION('',(-0.515038074910054,-1.04972719113862E-16,-0.857167300702112));
#30765=DIRECTION('center_axis',(-1.,0.,0.));
#30766=DIRECTION('ref_axis',(0.,0.,1.));
#30767=DIRECTION('',(-0.515038074910054,-1.04972719113862E-16,-0.857167300702112));
#30768=DIRECTION('center_axis',(-1.,0.,0.));
#30769=DIRECTION('ref_axis',(0.,0.,1.));
#30770=DIRECTION('',(-0.515038074910054,-1.04972719113862E-16,-0.857167300702112));
#30771=DIRECTION('center_axis',(0.,0.,1.));
#30772=DIRECTION('ref_axis',(1.,0.,0.));
#30773=DIRECTION('center_axis',(0.,0.,1.));
#30774=DIRECTION('ref_axis',(1.,0.,0.));
#30775=DIRECTION('center_axis',(0.,0.,1.));
#30776=DIRECTION('ref_axis',(1.,0.,0.));
#30777=DIRECTION('',(0.,0.,1.));
#30778=DIRECTION('center_axis',(0.,0.,1.));
#30779=DIRECTION('ref_axis',(1.,0.,0.));
#30780=DIRECTION('',(0.,0.,1.));
#30781=DIRECTION('center_axis',(0.,0.,1.));
#30782=DIRECTION('ref_axis',(1.,0.,0.));
#30783=DIRECTION('center_axis',(0.,0.,1.));
#30784=DIRECTION('ref_axis',(1.,0.,0.));
#30785=DIRECTION('center_axis',(0.,0.,1.));
#30786=DIRECTION('ref_axis',(1.,0.,0.));
#30787=DIRECTION('center_axis',(0.,0.,1.));
#30788=DIRECTION('ref_axis',(1.,0.,0.));
#30789=DIRECTION('',(0.,0.,1.));
#30790=DIRECTION('center_axis',(1.,0.,0.));
#30791=DIRECTION('ref_axis',(0.,1.,0.));
#30792=DIRECTION('center_axis',(1.,0.,0.));
#30793=DIRECTION('ref_axis',(0.,1.,0.));
#30794=DIRECTION('',(1.,0.,0.));
#30795=DIRECTION('center_axis',(-1.,0.,0.));
#30796=DIRECTION('ref_axis',(0.,0.,1.));
#30797=DIRECTION('axis',(0.,0.,1.));
#30798=DIRECTION('refdir',(1.,0.,0.));
#30799=DIRECTION('center_axis',(-1.,0.,0.));
#30800=DIRECTION('ref_axis',(0.,-1.,0.));
#30801=DIRECTION('center_axis',(-1.,0.,0.));
#30802=DIRECTION('ref_axis',(0.,-1.,0.));
#30803=DIRECTION('',(-0.561700222361827,0.827340836776884,1.0132003075627E-16));
#30804=DIRECTION('center_axis',(1.,0.,0.));
#30805=DIRECTION('ref_axis',(0.,-1.,0.));
#30806=DIRECTION('center_axis',(1.,0.,0.));
#30807=DIRECTION('ref_axis',(0.,-1.,0.));
#30808=DIRECTION('center_axis',(-1.,0.,0.));
#30809=DIRECTION('ref_axis',(0.,1.,0.));
#30810=DIRECTION('',(-0.929435063973188,-0.368985720397356,-4.51877181415702E-17));
#30811=DIRECTION('center_axis',(1.,0.,0.));
#30812=DIRECTION('ref_axis',(0.,0.,-1.));
#30813=DIRECTION('center_axis',(1.,0.,0.));
#30814=DIRECTION('ref_axis',(0.,0.,-1.));
#30815=DIRECTION('center_axis',(1.,0.,0.));
#30816=DIRECTION('ref_axis',(0.,0.,-1.));
#30817=DIRECTION('center_axis',(0.,1.,0.));
#30818=DIRECTION('ref_axis',(1.,0.,0.));
#30819=DIRECTION('',(1.,0.,0.));
#30820=DIRECTION('',(0.,0.,-1.));
#30821=DIRECTION('',(1.,0.,0.));
#30822=DIRECTION('',(0.,0.,-1.));
#30823=DIRECTION('center_axis',(1.,0.,0.));
#30824=DIRECTION('ref_axis',(0.,-1.,0.));
#30825=DIRECTION('center_axis',(1.,0.,0.));
#30826=DIRECTION('ref_axis',(0.,1.,0.));
#30827=DIRECTION('',(0.,-1.,0.));
#30828=DIRECTION('',(0.,0.,-1.));
#30829=DIRECTION('center_axis',(0.,-1.,0.));
#30830=DIRECTION('ref_axis',(-1.,0.,0.));
#30831=DIRECTION('',(-1.,0.,0.));
#30832=DIRECTION('',(-1.,0.,0.));
#30833=DIRECTION('',(0.,0.,-1.));
#30834=DIRECTION('center_axis',(-1.,0.,0.));
#30835=DIRECTION('ref_axis',(0.,1.,0.));
#30836=DIRECTION('center_axis',(-1.,0.,0.));
#30837=DIRECTION('ref_axis',(0.,1.,0.));
#30838=DIRECTION('',(0.,1.,0.));
#30839=DIRECTION('center_axis',(0.,0.,-1.));
#30840=DIRECTION('ref_axis',(-1.,0.,0.));
#30841=DIRECTION('center_axis',(0.,1.,0.));
#30842=DIRECTION('ref_axis',(1.,0.,0.));
#30843=DIRECTION('',(1.,0.,0.));
#30844=DIRECTION('',(0.,0.,-1.));
#30845=DIRECTION('',(1.,0.,0.));
#30846=DIRECTION('',(0.,0.,-1.));
#30847=DIRECTION('center_axis',(1.,0.,0.));
#30848=DIRECTION('ref_axis',(0.,-1.,0.));
#30849=DIRECTION('center_axis',(1.,0.,0.));
#30850=DIRECTION('ref_axis',(0.,1.,0.));
#30851=DIRECTION('',(0.,-1.,0.));
#30852=DIRECTION('',(0.,0.,-1.));
#30853=DIRECTION('center_axis',(0.,-1.,0.));
#30854=DIRECTION('ref_axis',(-1.,0.,0.));
#30855=DIRECTION('',(-1.,0.,0.));
#30856=DIRECTION('',(-1.,0.,0.));
#30857=DIRECTION('',(0.,0.,-1.));
#30858=DIRECTION('center_axis',(-1.,0.,0.));
#30859=DIRECTION('ref_axis',(0.,1.,0.));
#30860=DIRECTION('center_axis',(-1.,0.,0.));
#30861=DIRECTION('ref_axis',(0.,1.,0.));
#30862=DIRECTION('',(0.,1.,0.));
#30863=DIRECTION('center_axis',(0.,0.,-1.));
#30864=DIRECTION('ref_axis',(-1.,0.,0.));
#30865=DIRECTION('center_axis',(0.,1.,0.));
#30866=DIRECTION('ref_axis',(1.,0.,0.));
#30867=DIRECTION('',(1.,0.,0.));
#30868=DIRECTION('',(0.,0.,-1.));
#30869=DIRECTION('',(1.,0.,0.));
#30870=DIRECTION('',(0.,0.,-1.));
#30871=DIRECTION('center_axis',(1.,0.,0.));
#30872=DIRECTION('ref_axis',(0.,-1.,0.));
#30873=DIRECTION('center_axis',(1.,0.,0.));
#30874=DIRECTION('ref_axis',(0.,1.,0.));
#30875=DIRECTION('',(0.,-1.,0.));
#30876=DIRECTION('',(0.,0.,-1.));
#30877=DIRECTION('center_axis',(0.,-1.,0.));
#30878=DIRECTION('ref_axis',(-1.,0.,0.));
#30879=DIRECTION('',(-1.,0.,0.));
#30880=DIRECTION('',(-1.,0.,0.));
#30881=DIRECTION('',(0.,0.,-1.));
#30882=DIRECTION('center_axis',(-1.,0.,0.));
#30883=DIRECTION('ref_axis',(0.,1.,0.));
#30884=DIRECTION('center_axis',(-1.,0.,0.));
#30885=DIRECTION('ref_axis',(0.,1.,0.));
#30886=DIRECTION('',(0.,1.,0.));
#30887=DIRECTION('center_axis',(0.,0.,-1.));
#30888=DIRECTION('ref_axis',(-1.,0.,0.));
#30889=DIRECTION('center_axis',(0.,1.,0.));
#30890=DIRECTION('ref_axis',(1.,0.,0.));
#30891=DIRECTION('',(1.,0.,0.));
#30892=DIRECTION('',(0.,0.,-1.));
#30893=DIRECTION('',(1.,0.,0.));
#30894=DIRECTION('',(0.,0.,-1.));
#30895=DIRECTION('center_axis',(1.,0.,0.));
#30896=DIRECTION('ref_axis',(0.,-1.,0.));
#30897=DIRECTION('center_axis',(1.,0.,0.));
#30898=DIRECTION('ref_axis',(0.,1.,0.));
#30899=DIRECTION('',(0.,-1.,0.));
#30900=DIRECTION('',(0.,0.,-1.));
#30901=DIRECTION('center_axis',(0.,-1.,0.));
#30902=DIRECTION('ref_axis',(-1.,0.,0.));
#30903=DIRECTION('',(-1.,0.,0.));
#30904=DIRECTION('',(-1.,0.,0.));
#30905=DIRECTION('',(0.,0.,-1.));
#30906=DIRECTION('center_axis',(-1.,0.,0.));
#30907=DIRECTION('ref_axis',(0.,1.,0.));
#30908=DIRECTION('center_axis',(-1.,0.,0.));
#30909=DIRECTION('ref_axis',(0.,1.,0.));
#30910=DIRECTION('',(0.,1.,0.));
#30911=DIRECTION('center_axis',(0.,0.,-1.));
#30912=DIRECTION('ref_axis',(-1.,0.,0.));
#30913=DIRECTION('center_axis',(0.,1.,0.));
#30914=DIRECTION('ref_axis',(1.,0.,0.));
#30915=DIRECTION('',(1.,0.,0.));
#30916=DIRECTION('',(0.,0.,-1.));
#30917=DIRECTION('',(1.,0.,0.));
#30918=DIRECTION('',(0.,0.,-1.));
#30919=DIRECTION('center_axis',(1.,0.,0.));
#30920=DIRECTION('ref_axis',(0.,-1.,0.));
#30921=DIRECTION('center_axis',(1.,0.,0.));
#30922=DIRECTION('ref_axis',(0.,1.,0.));
#30923=DIRECTION('',(0.,-1.,0.));
#30924=DIRECTION('',(0.,0.,-1.));
#30925=DIRECTION('center_axis',(0.,-1.,0.));
#30926=DIRECTION('ref_axis',(-1.,0.,0.));
#30927=DIRECTION('',(-1.,0.,0.));
#30928=DIRECTION('',(-1.,0.,0.));
#30929=DIRECTION('',(0.,0.,-1.));
#30930=DIRECTION('center_axis',(-1.,0.,0.));
#30931=DIRECTION('ref_axis',(0.,1.,0.));
#30932=DIRECTION('center_axis',(-1.,0.,0.));
#30933=DIRECTION('ref_axis',(0.,1.,0.));
#30934=DIRECTION('',(0.,1.,0.));
#30935=DIRECTION('center_axis',(0.,0.,-1.));
#30936=DIRECTION('ref_axis',(-1.,0.,0.));
#30937=DIRECTION('center_axis',(0.,1.,0.));
#30938=DIRECTION('ref_axis',(1.,0.,0.));
#30939=DIRECTION('',(1.,0.,0.));
#30940=DIRECTION('',(0.,0.,-1.));
#30941=DIRECTION('',(1.,0.,0.));
#30942=DIRECTION('',(0.,0.,-1.));
#30943=DIRECTION('center_axis',(1.,0.,0.));
#30944=DIRECTION('ref_axis',(0.,-1.,0.));
#30945=DIRECTION('center_axis',(1.,0.,0.));
#30946=DIRECTION('ref_axis',(0.,1.,0.));
#30947=DIRECTION('',(0.,-1.,0.));
#30948=DIRECTION('',(0.,0.,-1.));
#30949=DIRECTION('center_axis',(0.,-1.,0.));
#30950=DIRECTION('ref_axis',(-1.,0.,0.));
#30951=DIRECTION('',(-1.,0.,0.));
#30952=DIRECTION('',(-1.,0.,0.));
#30953=DIRECTION('',(0.,0.,-1.));
#30954=DIRECTION('center_axis',(-1.,0.,0.));
#30955=DIRECTION('ref_axis',(0.,1.,0.));
#30956=DIRECTION('center_axis',(-1.,0.,0.));
#30957=DIRECTION('ref_axis',(0.,1.,0.));
#30958=DIRECTION('',(0.,1.,0.));
#30959=DIRECTION('center_axis',(0.,0.,-1.));
#30960=DIRECTION('ref_axis',(-1.,0.,0.));
#30961=DIRECTION('center_axis',(0.,1.,0.));
#30962=DIRECTION('ref_axis',(1.,0.,0.));
#30963=DIRECTION('',(1.,0.,0.));
#30964=DIRECTION('',(0.,0.,-1.));
#30965=DIRECTION('',(1.,0.,0.));
#30966=DIRECTION('',(0.,0.,-1.));
#30967=DIRECTION('center_axis',(1.,0.,0.));
#30968=DIRECTION('ref_axis',(0.,-1.,0.));
#30969=DIRECTION('center_axis',(1.,0.,0.));
#30970=DIRECTION('ref_axis',(0.,1.,0.));
#30971=DIRECTION('',(0.,-1.,0.));
#30972=DIRECTION('',(0.,0.,-1.));
#30973=DIRECTION('center_axis',(0.,-1.,0.));
#30974=DIRECTION('ref_axis',(-1.,0.,0.));
#30975=DIRECTION('',(-1.,0.,0.));
#30976=DIRECTION('',(-1.,0.,0.));
#30977=DIRECTION('',(0.,0.,-1.));
#30978=DIRECTION('center_axis',(-1.,0.,0.));
#30979=DIRECTION('ref_axis',(0.,1.,0.));
#30980=DIRECTION('center_axis',(-1.,0.,0.));
#30981=DIRECTION('ref_axis',(0.,1.,0.));
#30982=DIRECTION('',(0.,1.,0.));
#30983=DIRECTION('center_axis',(0.,0.,-1.));
#30984=DIRECTION('ref_axis',(-1.,0.,0.));
#30985=DIRECTION('center_axis',(0.,1.,0.));
#30986=DIRECTION('ref_axis',(1.,0.,0.));
#30987=DIRECTION('',(1.,0.,0.));
#30988=DIRECTION('',(0.,0.,-1.));
#30989=DIRECTION('',(1.,0.,0.));
#30990=DIRECTION('',(0.,0.,-1.));
#30991=DIRECTION('center_axis',(1.,0.,0.));
#30992=DIRECTION('ref_axis',(0.,-1.,0.));
#30993=DIRECTION('center_axis',(1.,0.,0.));
#30994=DIRECTION('ref_axis',(0.,1.,0.));
#30995=DIRECTION('',(0.,-1.,0.));
#30996=DIRECTION('',(0.,0.,-1.));
#30997=DIRECTION('center_axis',(0.,-1.,0.));
#30998=DIRECTION('ref_axis',(-1.,0.,0.));
#30999=DIRECTION('',(-1.,0.,0.));
#31000=DIRECTION('',(-1.,0.,0.));
#31001=DIRECTION('',(0.,0.,-1.));
#31002=DIRECTION('center_axis',(-1.,0.,0.));
#31003=DIRECTION('ref_axis',(0.,1.,0.));
#31004=DIRECTION('center_axis',(-1.,0.,0.));
#31005=DIRECTION('ref_axis',(0.,1.,0.));
#31006=DIRECTION('',(0.,1.,0.));
#31007=DIRECTION('center_axis',(0.,0.,-1.));
#31008=DIRECTION('ref_axis',(-1.,0.,0.));
#31009=DIRECTION('center_axis',(0.,1.,0.));
#31010=DIRECTION('ref_axis',(1.,0.,0.));
#31011=DIRECTION('',(1.,0.,0.));
#31012=DIRECTION('',(0.,0.,-1.));
#31013=DIRECTION('',(1.,0.,0.));
#31014=DIRECTION('',(0.,0.,-1.));
#31015=DIRECTION('center_axis',(1.,0.,0.));
#31016=DIRECTION('ref_axis',(0.,-1.,0.));
#31017=DIRECTION('center_axis',(1.,0.,0.));
#31018=DIRECTION('ref_axis',(0.,1.,0.));
#31019=DIRECTION('',(0.,-1.,0.));
#31020=DIRECTION('',(0.,0.,-1.));
#31021=DIRECTION('center_axis',(0.,-1.,0.));
#31022=DIRECTION('ref_axis',(-1.,0.,0.));
#31023=DIRECTION('',(-1.,0.,0.));
#31024=DIRECTION('',(-1.,0.,0.));
#31025=DIRECTION('',(0.,0.,-1.));
#31026=DIRECTION('center_axis',(-1.,0.,0.));
#31027=DIRECTION('ref_axis',(0.,1.,0.));
#31028=DIRECTION('center_axis',(-1.,0.,0.));
#31029=DIRECTION('ref_axis',(0.,1.,0.));
#31030=DIRECTION('',(0.,1.,0.));
#31031=DIRECTION('center_axis',(0.,0.,-1.));
#31032=DIRECTION('ref_axis',(-1.,0.,0.));
#31033=DIRECTION('center_axis',(0.,1.,0.));
#31034=DIRECTION('ref_axis',(1.,0.,0.));
#31035=DIRECTION('',(1.,0.,0.));
#31036=DIRECTION('',(0.,0.,-1.));
#31037=DIRECTION('',(1.,0.,0.));
#31038=DIRECTION('',(0.,0.,-1.));
#31039=DIRECTION('center_axis',(1.,0.,0.));
#31040=DIRECTION('ref_axis',(0.,-1.,0.));
#31041=DIRECTION('center_axis',(1.,0.,0.));
#31042=DIRECTION('ref_axis',(0.,1.,0.));
#31043=DIRECTION('',(0.,-1.,0.));
#31044=DIRECTION('',(0.,0.,-1.));
#31045=DIRECTION('center_axis',(0.,-1.,0.));
#31046=DIRECTION('ref_axis',(-1.,0.,0.));
#31047=DIRECTION('',(-1.,0.,0.));
#31048=DIRECTION('',(-1.,0.,0.));
#31049=DIRECTION('',(0.,0.,-1.));
#31050=DIRECTION('center_axis',(-1.,0.,0.));
#31051=DIRECTION('ref_axis',(0.,1.,0.));
#31052=DIRECTION('center_axis',(-1.,0.,0.));
#31053=DIRECTION('ref_axis',(0.,1.,0.));
#31054=DIRECTION('',(0.,1.,0.));
#31055=DIRECTION('center_axis',(0.,0.,-1.));
#31056=DIRECTION('ref_axis',(-1.,0.,0.));
#31057=DIRECTION('center_axis',(0.,1.,0.));
#31058=DIRECTION('ref_axis',(1.,0.,0.));
#31059=DIRECTION('',(1.,0.,0.));
#31060=DIRECTION('',(0.,0.,-1.));
#31061=DIRECTION('',(1.,0.,0.));
#31062=DIRECTION('',(0.,0.,-1.));
#31063=DIRECTION('center_axis',(1.,0.,0.));
#31064=DIRECTION('ref_axis',(0.,-1.,0.));
#31065=DIRECTION('center_axis',(1.,0.,0.));
#31066=DIRECTION('ref_axis',(0.,1.,0.));
#31067=DIRECTION('',(0.,-1.,0.));
#31068=DIRECTION('',(0.,0.,-1.));
#31069=DIRECTION('center_axis',(0.,-1.,0.));
#31070=DIRECTION('ref_axis',(-1.,0.,0.));
#31071=DIRECTION('',(-1.,0.,0.));
#31072=DIRECTION('',(-1.,0.,0.));
#31073=DIRECTION('',(0.,0.,-1.));
#31074=DIRECTION('center_axis',(-1.,0.,0.));
#31075=DIRECTION('ref_axis',(0.,1.,0.));
#31076=DIRECTION('center_axis',(-1.,0.,0.));
#31077=DIRECTION('ref_axis',(0.,1.,0.));
#31078=DIRECTION('',(0.,1.,0.));
#31079=DIRECTION('center_axis',(0.,0.,-1.));
#31080=DIRECTION('ref_axis',(-1.,0.,0.));
#31081=DIRECTION('center_axis',(0.,1.,0.));
#31082=DIRECTION('ref_axis',(1.,0.,0.));
#31083=DIRECTION('',(1.,0.,0.));
#31084=DIRECTION('',(0.,0.,-1.));
#31085=DIRECTION('',(1.,0.,0.));
#31086=DIRECTION('',(0.,0.,-1.));
#31087=DIRECTION('center_axis',(1.,0.,0.));
#31088=DIRECTION('ref_axis',(0.,-1.,0.));
#31089=DIRECTION('center_axis',(1.,0.,0.));
#31090=DIRECTION('ref_axis',(0.,1.,0.));
#31091=DIRECTION('',(0.,-1.,0.));
#31092=DIRECTION('',(0.,0.,-1.));
#31093=DIRECTION('center_axis',(0.,-1.,0.));
#31094=DIRECTION('ref_axis',(-1.,0.,0.));
#31095=DIRECTION('',(-1.,0.,0.));
#31096=DIRECTION('',(-1.,0.,0.));
#31097=DIRECTION('',(0.,0.,-1.));
#31098=DIRECTION('center_axis',(-1.,0.,0.));
#31099=DIRECTION('ref_axis',(0.,1.,0.));
#31100=DIRECTION('center_axis',(-1.,0.,0.));
#31101=DIRECTION('ref_axis',(0.,1.,0.));
#31102=DIRECTION('',(0.,1.,0.));
#31103=DIRECTION('center_axis',(0.,0.,-1.));
#31104=DIRECTION('ref_axis',(-1.,0.,0.));
#31105=DIRECTION('center_axis',(0.,1.,0.));
#31106=DIRECTION('ref_axis',(1.,0.,0.));
#31107=DIRECTION('',(1.,0.,0.));
#31108=DIRECTION('',(0.,0.,-1.));
#31109=DIRECTION('',(1.,0.,0.));
#31110=DIRECTION('',(0.,0.,-1.));
#31111=DIRECTION('center_axis',(1.,0.,0.));
#31112=DIRECTION('ref_axis',(0.,-1.,0.));
#31113=DIRECTION('center_axis',(1.,0.,0.));
#31114=DIRECTION('ref_axis',(0.,1.,0.));
#31115=DIRECTION('',(0.,-1.,0.));
#31116=DIRECTION('',(0.,0.,-1.));
#31117=DIRECTION('center_axis',(0.,-1.,0.));
#31118=DIRECTION('ref_axis',(-1.,0.,0.));
#31119=DIRECTION('',(-1.,0.,0.));
#31120=DIRECTION('',(-1.,0.,0.));
#31121=DIRECTION('',(0.,0.,-1.));
#31122=DIRECTION('center_axis',(-1.,0.,0.));
#31123=DIRECTION('ref_axis',(0.,1.,0.));
#31124=DIRECTION('center_axis',(-1.,0.,0.));
#31125=DIRECTION('ref_axis',(0.,1.,0.));
#31126=DIRECTION('',(0.,1.,0.));
#31127=DIRECTION('center_axis',(0.,0.,-1.));
#31128=DIRECTION('ref_axis',(-1.,0.,0.));
#31129=DIRECTION('center_axis',(0.,1.,0.));
#31130=DIRECTION('ref_axis',(1.,0.,0.));
#31131=DIRECTION('',(1.,0.,0.));
#31132=DIRECTION('',(0.,0.,-1.));
#31133=DIRECTION('',(1.,0.,0.));
#31134=DIRECTION('',(0.,0.,-1.));
#31135=DIRECTION('center_axis',(1.,0.,0.));
#31136=DIRECTION('ref_axis',(0.,-1.,0.));
#31137=DIRECTION('center_axis',(1.,0.,0.));
#31138=DIRECTION('ref_axis',(0.,1.,0.));
#31139=DIRECTION('',(0.,-1.,0.));
#31140=DIRECTION('',(0.,0.,-1.));
#31141=DIRECTION('center_axis',(0.,-1.,0.));
#31142=DIRECTION('ref_axis',(-1.,0.,0.));
#31143=DIRECTION('',(-1.,0.,0.));
#31144=DIRECTION('',(-1.,0.,0.));
#31145=DIRECTION('',(0.,0.,-1.));
#31146=DIRECTION('center_axis',(-1.,0.,0.));
#31147=DIRECTION('ref_axis',(0.,1.,0.));
#31148=DIRECTION('center_axis',(-1.,0.,0.));
#31149=DIRECTION('ref_axis',(0.,1.,0.));
#31150=DIRECTION('',(0.,1.,0.));
#31151=DIRECTION('center_axis',(0.,0.,-1.));
#31152=DIRECTION('ref_axis',(-1.,0.,0.));
#31153=DIRECTION('center_axis',(0.,1.,0.));
#31154=DIRECTION('ref_axis',(1.,0.,0.));
#31155=DIRECTION('',(1.,0.,0.));
#31156=DIRECTION('',(0.,0.,-1.));
#31157=DIRECTION('',(1.,0.,0.));
#31158=DIRECTION('',(0.,0.,-1.));
#31159=DIRECTION('center_axis',(1.,0.,0.));
#31160=DIRECTION('ref_axis',(0.,-1.,0.));
#31161=DIRECTION('center_axis',(1.,0.,0.));
#31162=DIRECTION('ref_axis',(0.,1.,0.));
#31163=DIRECTION('',(0.,-1.,0.));
#31164=DIRECTION('',(0.,0.,-1.));
#31165=DIRECTION('center_axis',(0.,-1.,0.));
#31166=DIRECTION('ref_axis',(-1.,0.,0.));
#31167=DIRECTION('',(-1.,0.,0.));
#31168=DIRECTION('',(-1.,0.,0.));
#31169=DIRECTION('',(0.,0.,-1.));
#31170=DIRECTION('center_axis',(-1.,0.,0.));
#31171=DIRECTION('ref_axis',(0.,1.,0.));
#31172=DIRECTION('center_axis',(-1.,0.,0.));
#31173=DIRECTION('ref_axis',(0.,1.,0.));
#31174=DIRECTION('',(0.,1.,0.));
#31175=DIRECTION('center_axis',(0.,0.,-1.));
#31176=DIRECTION('ref_axis',(-1.,0.,0.));
#31177=DIRECTION('center_axis',(0.,1.,0.));
#31178=DIRECTION('ref_axis',(1.,0.,0.));
#31179=DIRECTION('',(1.,0.,0.));
#31180=DIRECTION('',(0.,0.,-1.));
#31181=DIRECTION('',(1.,0.,0.));
#31182=DIRECTION('',(0.,0.,-1.));
#31183=DIRECTION('center_axis',(1.,0.,0.));
#31184=DIRECTION('ref_axis',(0.,-1.,0.));
#31185=DIRECTION('center_axis',(1.,0.,0.));
#31186=DIRECTION('ref_axis',(0.,1.,0.));
#31187=DIRECTION('',(0.,-1.,0.));
#31188=DIRECTION('',(0.,0.,-1.));
#31189=DIRECTION('center_axis',(0.,-1.,0.));
#31190=DIRECTION('ref_axis',(-1.,0.,0.));
#31191=DIRECTION('',(-1.,0.,0.));
#31192=DIRECTION('',(-1.,0.,0.));
#31193=DIRECTION('',(0.,0.,-1.));
#31194=DIRECTION('center_axis',(-1.,0.,0.));
#31195=DIRECTION('ref_axis',(0.,1.,0.));
#31196=DIRECTION('center_axis',(-1.,0.,0.));
#31197=DIRECTION('ref_axis',(0.,1.,0.));
#31198=DIRECTION('',(0.,1.,0.));
#31199=DIRECTION('center_axis',(0.,0.,-1.));
#31200=DIRECTION('ref_axis',(-1.,0.,0.));
#31201=DIRECTION('center_axis',(0.,1.,0.));
#31202=DIRECTION('ref_axis',(1.,0.,0.));
#31203=DIRECTION('',(1.,0.,0.));
#31204=DIRECTION('',(0.,0.,-1.));
#31205=DIRECTION('',(1.,0.,0.));
#31206=DIRECTION('',(0.,0.,-1.));
#31207=DIRECTION('center_axis',(1.,0.,0.));
#31208=DIRECTION('ref_axis',(0.,-1.,0.));
#31209=DIRECTION('center_axis',(1.,0.,0.));
#31210=DIRECTION('ref_axis',(0.,1.,0.));
#31211=DIRECTION('',(0.,-1.,0.));
#31212=DIRECTION('',(0.,0.,-1.));
#31213=DIRECTION('center_axis',(0.,-1.,0.));
#31214=DIRECTION('ref_axis',(-1.,0.,0.));
#31215=DIRECTION('',(-1.,0.,0.));
#31216=DIRECTION('',(-1.,0.,0.));
#31217=DIRECTION('',(0.,0.,-1.));
#31218=DIRECTION('center_axis',(-1.,0.,0.));
#31219=DIRECTION('ref_axis',(0.,1.,0.));
#31220=DIRECTION('center_axis',(-1.,0.,0.));
#31221=DIRECTION('ref_axis',(0.,1.,0.));
#31222=DIRECTION('',(0.,1.,0.));
#31223=DIRECTION('center_axis',(0.,0.,-1.));
#31224=DIRECTION('ref_axis',(-1.,0.,0.));
#31225=DIRECTION('center_axis',(0.,1.,0.));
#31226=DIRECTION('ref_axis',(1.,0.,0.));
#31227=DIRECTION('',(1.,0.,0.));
#31228=DIRECTION('',(0.,0.,-1.));
#31229=DIRECTION('',(1.,0.,0.));
#31230=DIRECTION('',(0.,0.,-1.));
#31231=DIRECTION('center_axis',(1.,0.,0.));
#31232=DIRECTION('ref_axis',(0.,-1.,0.));
#31233=DIRECTION('center_axis',(1.,0.,0.));
#31234=DIRECTION('ref_axis',(0.,1.,0.));
#31235=DIRECTION('',(0.,-1.,0.));
#31236=DIRECTION('',(0.,0.,-1.));
#31237=DIRECTION('center_axis',(0.,-1.,0.));
#31238=DIRECTION('ref_axis',(-1.,0.,0.));
#31239=DIRECTION('',(-1.,0.,0.));
#31240=DIRECTION('',(-1.,0.,0.));
#31241=DIRECTION('',(0.,0.,-1.));
#31242=DIRECTION('center_axis',(-1.,0.,0.));
#31243=DIRECTION('ref_axis',(0.,1.,0.));
#31244=DIRECTION('center_axis',(-1.,0.,0.));
#31245=DIRECTION('ref_axis',(0.,1.,0.));
#31246=DIRECTION('',(0.,1.,0.));
#31247=DIRECTION('center_axis',(0.,0.,-1.));
#31248=DIRECTION('ref_axis',(-1.,0.,0.));
#31249=DIRECTION('center_axis',(0.,1.,0.));
#31250=DIRECTION('ref_axis',(1.,0.,0.));
#31251=DIRECTION('',(1.,0.,0.));
#31252=DIRECTION('',(0.,0.,-1.));
#31253=DIRECTION('',(1.,0.,0.));
#31254=DIRECTION('',(0.,0.,-1.));
#31255=DIRECTION('center_axis',(1.,0.,0.));
#31256=DIRECTION('ref_axis',(0.,-1.,0.));
#31257=DIRECTION('center_axis',(1.,0.,0.));
#31258=DIRECTION('ref_axis',(0.,1.,0.));
#31259=DIRECTION('',(0.,-1.,0.));
#31260=DIRECTION('',(0.,0.,-1.));
#31261=DIRECTION('center_axis',(0.,-1.,0.));
#31262=DIRECTION('ref_axis',(-1.,0.,0.));
#31263=DIRECTION('',(-1.,0.,0.));
#31264=DIRECTION('',(-1.,0.,0.));
#31265=DIRECTION('',(0.,0.,-1.));
#31266=DIRECTION('center_axis',(-1.,0.,0.));
#31267=DIRECTION('ref_axis',(0.,1.,0.));
#31268=DIRECTION('center_axis',(-1.,0.,0.));
#31269=DIRECTION('ref_axis',(0.,1.,0.));
#31270=DIRECTION('',(0.,1.,0.));
#31271=DIRECTION('center_axis',(0.,0.,-1.));
#31272=DIRECTION('ref_axis',(-1.,0.,0.));
#31273=DIRECTION('center_axis',(0.,1.,0.));
#31274=DIRECTION('ref_axis',(1.,0.,0.));
#31275=DIRECTION('',(1.,0.,0.));
#31276=DIRECTION('',(0.,0.,-1.));
#31277=DIRECTION('',(1.,0.,0.));
#31278=DIRECTION('',(0.,0.,-1.));
#31279=DIRECTION('center_axis',(1.,0.,0.));
#31280=DIRECTION('ref_axis',(0.,-1.,0.));
#31281=DIRECTION('center_axis',(1.,0.,0.));
#31282=DIRECTION('ref_axis',(0.,1.,0.));
#31283=DIRECTION('',(0.,-1.,0.));
#31284=DIRECTION('',(0.,0.,-1.));
#31285=DIRECTION('center_axis',(0.,-1.,0.));
#31286=DIRECTION('ref_axis',(-1.,0.,0.));
#31287=DIRECTION('',(-1.,0.,0.));
#31288=DIRECTION('',(-1.,0.,0.));
#31289=DIRECTION('',(0.,0.,-1.));
#31290=DIRECTION('center_axis',(-1.,0.,0.));
#31291=DIRECTION('ref_axis',(0.,1.,0.));
#31292=DIRECTION('center_axis',(-1.,0.,0.));
#31293=DIRECTION('ref_axis',(0.,1.,0.));
#31294=DIRECTION('',(0.,1.,0.));
#31295=DIRECTION('center_axis',(0.,0.,-1.));
#31296=DIRECTION('ref_axis',(-1.,0.,0.));
#31297=DIRECTION('center_axis',(0.,1.,0.));
#31298=DIRECTION('ref_axis',(1.,0.,0.));
#31299=DIRECTION('',(1.,0.,0.));
#31300=DIRECTION('',(0.,0.,-1.));
#31301=DIRECTION('',(1.,0.,0.));
#31302=DIRECTION('',(0.,0.,-1.));
#31303=DIRECTION('center_axis',(1.,0.,0.));
#31304=DIRECTION('ref_axis',(0.,-1.,0.));
#31305=DIRECTION('center_axis',(1.,0.,0.));
#31306=DIRECTION('ref_axis',(0.,1.,0.));
#31307=DIRECTION('',(0.,-1.,0.));
#31308=DIRECTION('',(0.,0.,-1.));
#31309=DIRECTION('center_axis',(0.,-1.,0.));
#31310=DIRECTION('ref_axis',(-1.,0.,0.));
#31311=DIRECTION('',(-1.,0.,0.));
#31312=DIRECTION('',(-1.,0.,0.));
#31313=DIRECTION('',(0.,0.,-1.));
#31314=DIRECTION('center_axis',(-1.,0.,0.));
#31315=DIRECTION('ref_axis',(0.,1.,0.));
#31316=DIRECTION('center_axis',(-1.,0.,0.));
#31317=DIRECTION('ref_axis',(0.,1.,0.));
#31318=DIRECTION('',(0.,1.,0.));
#31319=DIRECTION('center_axis',(0.,0.,-1.));
#31320=DIRECTION('ref_axis',(-1.,0.,0.));
#31321=DIRECTION('center_axis',(0.,1.,0.));
#31322=DIRECTION('ref_axis',(1.,0.,0.));
#31323=DIRECTION('',(-1.,0.,0.));
#31324=DIRECTION('',(0.,0.,-1.));
#31325=DIRECTION('',(-1.,0.,0.));
#31326=DIRECTION('',(0.,0.,-1.));
#31327=DIRECTION('center_axis',(0.,0.,-1.));
#31328=DIRECTION('ref_axis',(1.1842378929335E-14,1.,0.));
#31329=DIRECTION('center_axis',(0.,0.,1.));
#31330=DIRECTION('ref_axis',(1.1842378929335E-14,1.,0.));
#31331=DIRECTION('',(0.,0.,-1.));
#31332=DIRECTION('center_axis',(0.,-1.,0.));
#31333=DIRECTION('ref_axis',(-1.,0.,0.));
#31334=DIRECTION('',(1.,0.,0.));
#31335=DIRECTION('',(1.,0.,0.));
#31336=DIRECTION('',(0.,0.,-1.));
#31337=DIRECTION('center_axis',(0.,0.,-1.));
#31338=DIRECTION('ref_axis',(0.,-1.,0.));
#31339=DIRECTION('center_axis',(0.,0.,1.));
#31340=DIRECTION('ref_axis',(0.,-1.,0.));
#31341=DIRECTION('center_axis',(0.,0.,1.));
#31342=DIRECTION('ref_axis',(1.,0.,0.));
#31343=DIRECTION('center_axis',(1.,0.,0.));
#31344=DIRECTION('ref_axis',(0.,1.,0.));
#31345=DIRECTION('center_axis',(1.,0.,0.));
#31346=DIRECTION('ref_axis',(0.,0.,-1.));
#31347=DIRECTION('',(-1.,0.,0.));
#31348=DIRECTION('center_axis',(1.,0.,0.));
#31349=DIRECTION('ref_axis',(0.,0.,-1.));
#31350=DIRECTION('center_axis',(-1.,0.,0.));
#31351=DIRECTION('ref_axis',(0.,0.,1.));
#31352=DIRECTION('center_axis',(1.,0.,0.));
#31353=DIRECTION('ref_axis',(0.,0.,-1.));
#31354=DIRECTION('center_axis',(1.,0.,0.));
#31355=DIRECTION('ref_axis',(0.,1.,0.));
#31356=DIRECTION('center_axis',(1.,0.,0.));
#31357=DIRECTION('ref_axis',(0.,0.,-1.));
#31358=DIRECTION('',(-0.707106781186546,0.707106781186549,8.65956056235495E-17));
#31359=DIRECTION('center_axis',(1.,0.,0.));
#31360=DIRECTION('ref_axis',(0.,1.,0.));
#31361=DIRECTION('',(-1.,0.,0.));
#31362=DIRECTION('center_axis',(1.,0.,0.));
#31363=DIRECTION('ref_axis',(0.,1.,0.));
#31364=DIRECTION('',(-0.697985354304537,0.71611203395584,8.7698431021492E-17));
#31365=DIRECTION('center_axis',(1.,0.,0.));
#31366=DIRECTION('ref_axis',(0.,0.,-1.));
#31367=DIRECTION('center_axis',(1.,0.,0.));
#31368=DIRECTION('ref_axis',(0.,1.,0.));
#31369=DIRECTION('',(-0.999662950030635,0.0259612468122956,3.17933578105522E-18));
#31370=DIRECTION('center_axis',(1.,0.,0.));
#31371=DIRECTION('ref_axis',(0.,0.,-1.));
#31372=DIRECTION('center_axis',(1.,0.,0.));
#31373=DIRECTION('ref_axis',(0.,0.,-1.));
#31374=DIRECTION('center_axis',(1.,0.,0.));
#31375=DIRECTION('ref_axis',(0.,0.,-1.));
#31376=DIRECTION('center_axis',(1.,0.,0.));
#31377=DIRECTION('ref_axis',(0.,1.,0.));
#31378=DIRECTION('',(-1.,0.,0.));
#31379=DIRECTION('center_axis',(1.,0.,0.));
#31380=DIRECTION('ref_axis',(0.,0.,-1.));
#31381=DIRECTION('center_axis',(-1.,0.,0.));
#31382=DIRECTION('ref_axis',(0.,0.,1.));
#31383=DIRECTION('axis',(0.,0.,1.));
#31384=DIRECTION('refdir',(1.,0.,0.));
#31385=DIRECTION('center_axis',(-1.,0.,0.));
#31386=DIRECTION('ref_axis',(0.,-1.,0.));
#31387=DIRECTION('center_axis',(-1.,0.,0.));
#31388=DIRECTION('ref_axis',(0.,-1.,0.));
#31389=DIRECTION('center_axis',(-1.,0.,0.));
#31390=DIRECTION('ref_axis',(0.,-1.,0.));
#31391=DIRECTION('',(-0.969243390898598,0.246104142995171,3.01390650975938E-17));
#31392=DIRECTION('center_axis',(1.,0.,0.));
#31393=DIRECTION('ref_axis',(0.,-1.,0.));
#31394=DIRECTION('center_axis',(1.,0.,0.));
#31395=DIRECTION('ref_axis',(0.,-1.,0.));
#31396=DIRECTION('center_axis',(1.,0.,0.));
#31397=DIRECTION('ref_axis',(0.,1.,0.));
#31398=DIRECTION('',(-0.999654664967248,0.0262783334558961,3.218167695369E-18));
#31399=DIRECTION('center_axis',(1.,0.,0.));
#31400=DIRECTION('ref_axis',(0.,0.,-1.));
#31401=DIRECTION('center_axis',(-1.,0.,0.));
#31402=DIRECTION('ref_axis',(0.,1.,0.));
#31403=DIRECTION('',(-0.866025403784439,-0.5,-6.12323399573677E-17));
#31404=DIRECTION('center_axis',(-1.,0.,0.));
#31405=DIRECTION('ref_axis',(0.,0.,1.));
#31406=DIRECTION('center_axis',(1.,0.,0.));
#31407=DIRECTION('ref_axis',(0.,0.,-1.));
#31408=DIRECTION('center_axis',(1.,0.,0.));
#31409=DIRECTION('ref_axis',(0.,1.,0.));
#31410=DIRECTION('center_axis',(1.,0.,0.));
#31411=DIRECTION('ref_axis',(0.,0.,-1.));
#31412=DIRECTION('',(-0.707106781186555,0.70710678118654,8.65956056235484E-17));
#31413=DIRECTION('center_axis',(1.,0.,0.));
#31414=DIRECTION('ref_axis',(0.,1.,0.));
#31415=DIRECTION('',(-0.999662950030635,0.0259612468122956,3.17933578105522E-18));
#31416=DIRECTION('axis',(0.,0.,1.));
#31417=DIRECTION('refdir',(1.,0.,0.));
#31418=DIRECTION('center_axis',(1.,0.,0.));
#31419=DIRECTION('ref_axis',(0.,-0.216887865424076,0.976196524185468));
#31420=DIRECTION('',(-1.,0.,0.));
#31421=DIRECTION('center_axis',(-1.,0.,0.));
#31422=DIRECTION('ref_axis',(0.,1.,0.));
#31423=DIRECTION('center_axis',(1.,0.,0.));
#31424=DIRECTION('ref_axis',(0.,1.,0.));
#31425=DIRECTION('',(-1.,0.,0.));
#31426=DIRECTION('center_axis',(1.,0.,0.));
#31427=DIRECTION('ref_axis',(0.,1.,0.));
#31428=DIRECTION('',(-1.,0.,0.));
#31429=DIRECTION('center_axis',(1.,0.,0.));
#31430=DIRECTION('ref_axis',(0.,1.,0.));
#31431=DIRECTION('',(-1.,0.,0.));
#31432=DIRECTION('center_axis',(1.,0.,0.));
#31433=DIRECTION('ref_axis',(0.,1.,0.));
#31434=DIRECTION('',(-1.,0.,0.));
#31435=DIRECTION('center_axis',(1.,0.,0.));
#31436=DIRECTION('ref_axis',(0.,1.,0.));
#31437=DIRECTION('',(-1.,0.,0.));
#31438=DIRECTION('center_axis',(1.,0.,0.));
#31439=DIRECTION('ref_axis',(0.,1.,0.));
#31440=DIRECTION('',(-1.,0.,0.));
#31441=DIRECTION('center_axis',(1.,0.,0.));
#31442=DIRECTION('ref_axis',(0.,1.,0.));
#31443=DIRECTION('',(-1.,0.,0.));
#31444=DIRECTION('center_axis',(1.,0.,0.));
#31445=DIRECTION('ref_axis',(0.,1.,0.));
#31446=DIRECTION('',(-1.,0.,0.));
#31447=DIRECTION('center_axis',(1.,0.,0.));
#31448=DIRECTION('ref_axis',(0.,1.,0.));
#31449=DIRECTION('',(-1.,0.,0.));
#31450=DIRECTION('center_axis',(1.,0.,0.));
#31451=DIRECTION('ref_axis',(0.,1.,0.));
#31452=DIRECTION('',(-1.,0.,0.));
#31453=DIRECTION('center_axis',(1.,0.,0.));
#31454=DIRECTION('ref_axis',(0.,1.,0.));
#31455=DIRECTION('',(-1.,0.,0.));
#31456=DIRECTION('center_axis',(1.,0.,0.));
#31457=DIRECTION('ref_axis',(0.,1.,0.));
#31458=DIRECTION('',(-1.,0.,0.));
#31459=DIRECTION('center_axis',(1.,0.,0.));
#31460=DIRECTION('ref_axis',(0.,1.,0.));
#31461=DIRECTION('',(-1.,0.,0.));
#31462=DIRECTION('center_axis',(1.,0.,0.));
#31463=DIRECTION('ref_axis',(0.,1.,0.));
#31464=DIRECTION('',(-1.,0.,0.));
#31465=DIRECTION('center_axis',(1.,0.,0.));
#31466=DIRECTION('ref_axis',(0.,1.,0.));
#31467=DIRECTION('',(-1.,0.,0.));
#31468=DIRECTION('center_axis',(1.,0.,0.));
#31469=DIRECTION('ref_axis',(0.,1.,0.));
#31470=DIRECTION('',(-1.,0.,0.));
#31471=DIRECTION('center_axis',(1.,0.,0.));
#31472=DIRECTION('ref_axis',(0.,1.,0.));
#31473=DIRECTION('',(-1.,0.,0.));
#31474=DIRECTION('center_axis',(1.,0.,0.));
#31475=DIRECTION('ref_axis',(0.,1.,0.));
#31476=DIRECTION('',(-1.,0.,0.));
#31477=DIRECTION('center_axis',(1.,0.,0.));
#31478=DIRECTION('ref_axis',(0.,1.,0.));
#31479=DIRECTION('',(-1.,0.,0.));
#31480=DIRECTION('center_axis',(1.,0.,0.));
#31481=DIRECTION('ref_axis',(0.,1.,0.));
#31482=DIRECTION('',(-1.,0.,0.));
#31483=DIRECTION('center_axis',(1.,0.,0.));
#31484=DIRECTION('ref_axis',(0.,1.,0.));
#31485=DIRECTION('',(-1.,0.,0.));
#31486=DIRECTION('center_axis',(1.,0.,0.));
#31487=DIRECTION('ref_axis',(0.,1.,0.));
#31488=DIRECTION('',(-1.,0.,0.));
#31489=DIRECTION('center_axis',(1.,0.,0.));
#31490=DIRECTION('ref_axis',(0.,1.,0.));
#31491=DIRECTION('',(-1.,0.,0.));
#31492=DIRECTION('center_axis',(1.,0.,0.));
#31493=DIRECTION('ref_axis',(0.,1.,0.));
#31494=DIRECTION('',(-1.,0.,0.));
#31495=DIRECTION('center_axis',(1.,0.,0.));
#31496=DIRECTION('ref_axis',(0.,1.,0.));
#31497=DIRECTION('',(-1.,0.,0.));
#31498=DIRECTION('center_axis',(1.,0.,0.));
#31499=DIRECTION('ref_axis',(0.,1.,0.));
#31500=DIRECTION('',(-1.,0.,0.));
#31501=DIRECTION('center_axis',(1.,0.,0.));
#31502=DIRECTION('ref_axis',(0.,1.,0.));
#31503=DIRECTION('',(-1.,0.,0.));
#31504=DIRECTION('center_axis',(1.,0.,0.));
#31505=DIRECTION('ref_axis',(0.,1.,0.));
#31506=DIRECTION('',(-1.,0.,0.));
#31507=DIRECTION('center_axis',(1.,0.,0.));
#31508=DIRECTION('ref_axis',(0.,1.,0.));
#31509=DIRECTION('',(-1.,0.,0.));
#31510=DIRECTION('center_axis',(1.,0.,0.));
#31511=DIRECTION('ref_axis',(0.,1.,0.));
#31512=DIRECTION('',(-1.,0.,0.));
#31513=DIRECTION('center_axis',(1.,0.,0.));
#31514=DIRECTION('ref_axis',(0.,1.,0.));
#31515=DIRECTION('',(-1.,0.,0.));
#31516=DIRECTION('center_axis',(1.,0.,0.));
#31517=DIRECTION('ref_axis',(0.,1.,0.));
#31518=DIRECTION('',(-1.,0.,0.));
#31519=DIRECTION('center_axis',(1.,0.,0.));
#31520=DIRECTION('ref_axis',(0.,1.,0.));
#31521=DIRECTION('',(-1.,0.,0.));
#31522=DIRECTION('center_axis',(1.,0.,0.));
#31523=DIRECTION('ref_axis',(0.,1.,0.));
#31524=DIRECTION('',(-1.,0.,0.));
#31525=DIRECTION('center_axis',(1.,0.,0.));
#31526=DIRECTION('ref_axis',(0.,1.,0.));
#31527=DIRECTION('',(-1.,0.,0.));
#31528=DIRECTION('center_axis',(1.,0.,0.));
#31529=DIRECTION('ref_axis',(0.,1.,0.));
#31530=DIRECTION('',(-1.,0.,0.));
#31531=DIRECTION('center_axis',(1.,0.,0.));
#31532=DIRECTION('ref_axis',(0.,1.,0.));
#31533=DIRECTION('',(-1.,0.,0.));
#31534=DIRECTION('center_axis',(1.,0.,0.));
#31535=DIRECTION('ref_axis',(0.,1.,0.));
#31536=DIRECTION('',(-1.,0.,0.));
#31537=DIRECTION('center_axis',(1.,0.,0.));
#31538=DIRECTION('ref_axis',(0.,1.,0.));
#31539=DIRECTION('',(-1.,0.,0.));
#31540=DIRECTION('center_axis',(1.,0.,0.));
#31541=DIRECTION('ref_axis',(0.,1.,0.));
#31542=DIRECTION('',(-1.,0.,0.));
#31543=DIRECTION('center_axis',(1.,0.,0.));
#31544=DIRECTION('ref_axis',(0.,1.,0.));
#31545=DIRECTION('',(-1.,0.,0.));
#31546=DIRECTION('center_axis',(1.,0.,0.));
#31547=DIRECTION('ref_axis',(0.,-0.201340086992588,-0.979521398117375));
#31548=DIRECTION('',(1.,0.,0.));
#31549=DIRECTION('center_axis',(1.,0.,0.));
#31550=DIRECTION('ref_axis',(0.,1.,-4.88042043924972E-13));
#31551=DIRECTION('center_axis',(1.,0.,0.));
#31552=DIRECTION('ref_axis',(0.,1.,-4.88042043924972E-13));
#31553=DIRECTION('',(1.,0.,0.));
#31554=DIRECTION('center_axis',(1.,0.,0.));
#31555=DIRECTION('ref_axis',(0.,1.,-4.88042043924972E-13));
#31556=DIRECTION('',(1.,0.,0.));
#31557=DIRECTION('center_axis',(1.,0.,0.));
#31558=DIRECTION('ref_axis',(0.,1.,-4.88042043924972E-13));
#31559=DIRECTION('',(1.,0.,0.));
#31560=DIRECTION('center_axis',(1.,0.,0.));
#31561=DIRECTION('ref_axis',(0.,1.,-4.88042043924972E-13));
#31562=DIRECTION('',(1.,0.,0.));
#31563=DIRECTION('center_axis',(1.,0.,0.));
#31564=DIRECTION('ref_axis',(0.,1.,-4.88042043924972E-13));
#31565=DIRECTION('',(1.,0.,0.));
#31566=DIRECTION('center_axis',(1.,0.,0.));
#31567=DIRECTION('ref_axis',(0.,1.,-4.88042043924972E-13));
#31568=DIRECTION('',(1.,0.,0.));
#31569=DIRECTION('center_axis',(1.,0.,0.));
#31570=DIRECTION('ref_axis',(0.,1.,-4.88042043924972E-13));
#31571=DIRECTION('',(1.,0.,0.));
#31572=DIRECTION('center_axis',(1.,0.,0.));
#31573=DIRECTION('ref_axis',(0.,1.,-4.88042043924972E-13));
#31574=DIRECTION('',(1.,0.,0.));
#31575=DIRECTION('center_axis',(1.,0.,0.));
#31576=DIRECTION('ref_axis',(0.,1.,-4.88042043924972E-13));
#31577=DIRECTION('',(1.,0.,0.));
#31578=DIRECTION('center_axis',(1.,0.,0.));
#31579=DIRECTION('ref_axis',(0.,1.,-4.88042043924972E-13));
#31580=DIRECTION('',(1.,0.,0.));
#31581=DIRECTION('center_axis',(1.,0.,0.));
#31582=DIRECTION('ref_axis',(0.,1.,-4.88042043924972E-13));
#31583=DIRECTION('',(1.,0.,0.));
#31584=DIRECTION('center_axis',(1.,0.,0.));
#31585=DIRECTION('ref_axis',(0.,1.,-4.88042043924972E-13));
#31586=DIRECTION('',(1.,0.,0.));
#31587=DIRECTION('center_axis',(1.,0.,0.));
#31588=DIRECTION('ref_axis',(0.,1.,-4.88042043924972E-13));
#31589=DIRECTION('',(1.,0.,0.));
#31590=DIRECTION('center_axis',(1.,0.,0.));
#31591=DIRECTION('ref_axis',(0.,1.,-4.88042043924972E-13));
#31592=DIRECTION('',(1.,0.,0.));
#31593=DIRECTION('center_axis',(1.,0.,0.));
#31594=DIRECTION('ref_axis',(0.,1.,-4.88042043924972E-13));
#31595=DIRECTION('',(1.,0.,0.));
#31596=DIRECTION('center_axis',(1.,0.,0.));
#31597=DIRECTION('ref_axis',(0.,1.,-4.88042043924972E-13));
#31598=DIRECTION('',(1.,0.,0.));
#31599=DIRECTION('center_axis',(1.,0.,0.));
#31600=DIRECTION('ref_axis',(0.,1.,-4.88042043924972E-13));
#31601=DIRECTION('',(1.,0.,0.));
#31602=DIRECTION('center_axis',(1.,0.,0.));
#31603=DIRECTION('ref_axis',(0.,1.,-4.88042043924972E-13));
#31604=DIRECTION('',(1.,0.,0.));
#31605=DIRECTION('center_axis',(1.,0.,0.));
#31606=DIRECTION('ref_axis',(0.,1.,-4.88042043924972E-13));
#31607=DIRECTION('',(1.,0.,0.));
#31608=DIRECTION('center_axis',(1.,0.,0.));
#31609=DIRECTION('ref_axis',(0.,1.,-4.88042043924972E-13));
#31610=DIRECTION('',(1.,0.,0.));
#31611=DIRECTION('center_axis',(1.,0.,0.));
#31612=DIRECTION('ref_axis',(0.,1.,-4.88042043924972E-13));
#31613=DIRECTION('',(1.,0.,0.));
#31614=DIRECTION('center_axis',(1.,0.,0.));
#31615=DIRECTION('ref_axis',(0.,1.,-4.88042043924972E-13));
#31616=DIRECTION('',(1.,0.,0.));
#31617=DIRECTION('center_axis',(1.,0.,0.));
#31618=DIRECTION('ref_axis',(0.,1.,-4.88042043924972E-13));
#31619=DIRECTION('',(1.,0.,0.));
#31620=DIRECTION('center_axis',(1.,0.,0.));
#31621=DIRECTION('ref_axis',(0.,1.,-4.88042043924972E-13));
#31622=DIRECTION('',(1.,0.,0.));
#31623=DIRECTION('center_axis',(1.,0.,0.));
#31624=DIRECTION('ref_axis',(0.,1.,-4.88042043924972E-13));
#31625=DIRECTION('',(1.,0.,0.));
#31626=DIRECTION('center_axis',(1.,0.,0.));
#31627=DIRECTION('ref_axis',(0.,1.,-4.88042043924972E-13));
#31628=DIRECTION('',(1.,0.,0.));
#31629=DIRECTION('center_axis',(1.,0.,0.));
#31630=DIRECTION('ref_axis',(0.,1.,-4.88042043924972E-13));
#31631=DIRECTION('',(1.,0.,0.));
#31632=DIRECTION('center_axis',(1.,0.,0.));
#31633=DIRECTION('ref_axis',(0.,1.,-4.88042043924972E-13));
#31634=DIRECTION('',(1.,0.,0.));
#31635=DIRECTION('center_axis',(1.,0.,0.));
#31636=DIRECTION('ref_axis',(0.,1.,-4.88042043924972E-13));
#31637=DIRECTION('',(1.,0.,0.));
#31638=DIRECTION('center_axis',(1.,0.,0.));
#31639=DIRECTION('ref_axis',(0.,1.,-4.88042043924972E-13));
#31640=DIRECTION('',(1.,0.,0.));
#31641=DIRECTION('center_axis',(1.,0.,0.));
#31642=DIRECTION('ref_axis',(0.,1.,-4.88042043924972E-13));
#31643=DIRECTION('',(1.,0.,0.));
#31644=DIRECTION('center_axis',(1.,0.,0.));
#31645=DIRECTION('ref_axis',(0.,1.,-4.88042043924972E-13));
#31646=DIRECTION('',(1.,0.,0.));
#31647=DIRECTION('center_axis',(1.,0.,0.));
#31648=DIRECTION('ref_axis',(0.,1.,-4.88042043924972E-13));
#31649=DIRECTION('',(1.,0.,0.));
#31650=DIRECTION('center_axis',(1.,0.,0.));
#31651=DIRECTION('ref_axis',(0.,1.,-4.88042043924972E-13));
#31652=DIRECTION('',(1.,0.,0.));
#31653=DIRECTION('center_axis',(1.,0.,0.));
#31654=DIRECTION('ref_axis',(0.,1.,-4.88042043924972E-13));
#31655=DIRECTION('',(1.,0.,0.));
#31656=DIRECTION('center_axis',(1.,0.,0.));
#31657=DIRECTION('ref_axis',(0.,1.,-4.88042043924972E-13));
#31658=DIRECTION('',(1.,0.,0.));
#31659=DIRECTION('center_axis',(1.,0.,0.));
#31660=DIRECTION('ref_axis',(0.,1.,-4.88042043924972E-13));
#31661=DIRECTION('',(1.,0.,0.));
#31662=DIRECTION('center_axis',(1.,0.,0.));
#31663=DIRECTION('ref_axis',(0.,1.,-4.88042043924972E-13));
#31664=DIRECTION('',(1.,0.,0.));
#31665=DIRECTION('center_axis',(1.,0.,0.));
#31666=DIRECTION('ref_axis',(0.,1.,-4.88042043924972E-13));
#31667=DIRECTION('',(1.,0.,0.));
#31668=DIRECTION('center_axis',(1.,0.,0.));
#31669=DIRECTION('ref_axis',(0.,1.,-4.88042043924972E-13));
#31670=DIRECTION('',(1.,0.,0.));
#31671=DIRECTION('center_axis',(1.,0.,0.));
#31672=DIRECTION('ref_axis',(0.,1.,-4.88042043924972E-13));
#31673=DIRECTION('',(1.,0.,0.));
#31674=DIRECTION('center_axis',(-1.,0.,0.));
#31675=DIRECTION('ref_axis',(0.,-1.,0.));
#31676=DIRECTION('center_axis',(-1.,0.,0.));
#31677=DIRECTION('ref_axis',(0.,-1.,0.));
#31678=DIRECTION('',(-0.382683432365103,0.923879532511281,1.13142611228769E-16));
#31679=DIRECTION('center_axis',(1.,0.,0.));
#31680=DIRECTION('ref_axis',(0.,-1.,0.));
#31681=DIRECTION('center_axis',(1.,0.,0.));
#31682=DIRECTION('ref_axis',(0.,-1.,0.));
#31683=DIRECTION('center_axis',(-1.,0.,0.));
#31684=DIRECTION('ref_axis',(0.,1.,0.));
#31685=DIRECTION('',(-0.707106781186553,-0.707106781186542,-8.65956056235487E-17));
#31686=DIRECTION('center_axis',(-1.,0.,0.));
#31687=DIRECTION('ref_axis',(0.,-1.,0.));
#31688=DIRECTION('center_axis',(-1.,0.,0.));
#31689=DIRECTION('ref_axis',(0.,1.,0.));
#31690=DIRECTION('center_axis',(-1.,0.,0.));
#31691=DIRECTION('ref_axis',(0.,-1.,0.));
#31692=DIRECTION('center_axis',(1.,0.,0.));
#31693=DIRECTION('ref_axis',(0.,0.,-1.));
#31694=DIRECTION('center_axis',(-1.,0.,0.));
#31695=DIRECTION('ref_axis',(0.,0.,1.));
#31696=DIRECTION('center_axis',(-1.,0.,0.));
#31697=DIRECTION('ref_axis',(0.,0.,1.));
#31698=DIRECTION('',(0.707106781186543,8.65956056235499E-17,0.707106781186552));
#31699=DIRECTION('center_axis',(1.,0.,0.));
#31700=DIRECTION('ref_axis',(0.,0.,1.));
#31701=DIRECTION('center_axis',(-1.,0.,0.));
#31702=DIRECTION('ref_axis',(0.,0.,1.));
#31703=DIRECTION('center_axis',(-1.,0.,0.));
#31704=DIRECTION('ref_axis',(0.,0.,1.));
#31705=DIRECTION('',(-1.,0.,0.));
#31706=DIRECTION('center_axis',(-1.,0.,0.));
#31707=DIRECTION('ref_axis',(0.,0.,1.));
#31708=DIRECTION('center_axis',(1.,0.,0.));
#31709=DIRECTION('ref_axis',(0.,0.,-1.));
#31710=DIRECTION('center_axis',(-1.,0.,0.));
#31711=DIRECTION('ref_axis',(0.,-0.0771183618471287,0.997021944726401));
#31712=DIRECTION('center_axis',(1.,0.,0.));
#31713=DIRECTION('ref_axis',(0.,-1.,0.));
#31714=DIRECTION('center_axis',(1.,0.,0.));
#31715=DIRECTION('ref_axis',(0.,0.413513095306714,-0.91049817133801));
#31716=DIRECTION('center_axis',(1.,0.,0.));
#31717=DIRECTION('ref_axis',(0.,1.,0.));
#31718=DIRECTION('center_axis',(1.,0.,0.));
#31719=DIRECTION('ref_axis',(0.,0.,-1.));
#31720=DIRECTION('center_axis',(1.,0.,0.));
#31721=DIRECTION('ref_axis',(0.,0.965988671445919,0.258584389780489));
#31722=DIRECTION('center_axis',(-1.,0.,0.));
#31723=DIRECTION('ref_axis',(0.,1.,-4.88042043924972E-13));
#31724=DIRECTION('center_axis',(1.,0.,0.));
#31725=DIRECTION('ref_axis',(0.,0.851219542641563,-0.524809765748589));
#31726=DIRECTION('center_axis',(-1.,0.,0.));
#31727=DIRECTION('ref_axis',(0.,0.,1.));
#31728=DIRECTION('',(-0.515038074910053,-1.04972719113862E-16,-0.857167300702113));
#31729=DIRECTION('center_axis',(0.,-1.,0.));
#31730=DIRECTION('ref_axis',(1.,0.,0.));
#31731=DIRECTION('',(-1.,0.,0.));
#31732=DIRECTION('',(0.,0.,1.));
#31733=DIRECTION('',(1.,0.,0.));
#31734=DIRECTION('',(0.,0.,1.));
#31735=DIRECTION('center_axis',(0.,0.,1.));
#31736=DIRECTION('ref_axis',(0.,1.,0.));
#31737=DIRECTION('center_axis',(0.,0.,1.));
#31738=DIRECTION('ref_axis',(0.,1.,0.));
#31739=DIRECTION('',(0.,0.,1.));
#31740=DIRECTION('center_axis',(0.,1.,0.));
#31741=DIRECTION('ref_axis',(-1.,0.,0.));
#31742=DIRECTION('',(1.,0.,0.));
#31743=DIRECTION('',(-1.,0.,0.));
#31744=DIRECTION('',(0.,0.,1.));
#31745=DIRECTION('center_axis',(0.,0.,1.));
#31746=DIRECTION('ref_axis',(0.,-1.,0.));
#31747=DIRECTION('center_axis',(0.,0.,1.));
#31748=DIRECTION('ref_axis',(0.,-1.,0.));
#31749=DIRECTION('center_axis',(0.,0.,1.));
#31750=DIRECTION('ref_axis',(1.,0.,0.));
#31751=DIRECTION('center_axis',(1.,0.,0.));
#31752=DIRECTION('ref_axis',(0.,1.,0.));
#31753=DIRECTION('center_axis',(1.,0.,0.));
#31754=DIRECTION('ref_axis',(0.,0.,-1.));
#31755=DIRECTION('',(-0.707106781186546,0.707106781186549,8.65956056235495E-17));
#31756=DIRECTION('center_axis',(1.,0.,0.));
#31757=DIRECTION('ref_axis',(0.,1.,0.));
#31758=DIRECTION('center_axis',(1.,0.,0.));
#31759=DIRECTION('ref_axis',(0.,0.,-1.));
#31760=DIRECTION('',(-1.,0.,0.));
#31761=DIRECTION('center_axis',(-1.,0.,0.));
#31762=DIRECTION('ref_axis',(0.,0.,1.));
#31763=DIRECTION('center_axis',(1.,0.,0.));
#31764=DIRECTION('ref_axis',(0.,0.,-1.));
#31765=DIRECTION('center_axis',(1.,0.,0.));
#31766=DIRECTION('ref_axis',(0.,1.,0.));
#31767=DIRECTION('center_axis',(1.,0.,0.));
#31768=DIRECTION('ref_axis',(0.,0.,-1.));
#31769=DIRECTION('',(-0.70710678118654,0.707106781186555,8.65956056235503E-17));
#31770=DIRECTION('center_axis',(1.,0.,0.));
#31771=DIRECTION('ref_axis',(0.,1.,0.));
#31772=DIRECTION('center_axis',(1.,0.,0.));
#31773=DIRECTION('ref_axis',(0.,0.,-1.));
#31774=DIRECTION('',(-1.,0.,0.));
#31775=DIRECTION('center_axis',(-1.,0.,0.));
#31776=DIRECTION('ref_axis',(0.,1.,0.));
#31777=DIRECTION('center_axis',(1.,0.,0.));
#31778=DIRECTION('ref_axis',(0.,0.,-1.));
#31779=DIRECTION('',(-0.70710678118654,-0.707106781186555,-8.65956056235503E-17));
#31780=DIRECTION('center_axis',(1.,0.,0.));
#31781=DIRECTION('ref_axis',(0.,0.,-1.));
#31782=DIRECTION('axis',(0.,0.,1.));
#31783=DIRECTION('refdir',(1.,0.,0.));
#31784=DIRECTION('center_axis',(-1.,0.,0.));
#31785=DIRECTION('ref_axis',(0.,-1.,0.));
#31786=DIRECTION('center_axis',(-1.,0.,0.));
#31787=DIRECTION('ref_axis',(0.,-1.,0.));
#31788=DIRECTION('',(0.382683432365091,-0.923879532511286,1.1314261122877E-16));
#31789=DIRECTION('center_axis',(1.,0.,-1.66069808438821E-15));
#31790=DIRECTION('ref_axis',(0.,-1.,0.));
#31791=DIRECTION('center_axis',(1.,0.,-1.66069808438821E-15));
#31792=DIRECTION('ref_axis',(0.,-1.,0.));
#31793=DIRECTION('center_axis',(-1.,0.,0.));
#31794=DIRECTION('ref_axis',(0.,1.,0.));
#31795=DIRECTION('center_axis',(-1.,0.,0.));
#31796=DIRECTION('ref_axis',(0.,-1.,0.));
#31797=DIRECTION('center_axis',(-1.,0.,0.));
#31798=DIRECTION('ref_axis',(0.,-1.,0.));
#31799=DIRECTION('',(-0.707106781186547,-0.707106781186548,-8.65956056235494E-17));
#31800=DIRECTION('center_axis',(-1.,0.,0.));
#31801=DIRECTION('ref_axis',(0.,0.,1.));
#31802=DIRECTION('center_axis',(1.,0.,0.));
#31803=DIRECTION('ref_axis',(0.,0.,-1.));
#31804=DIRECTION('center_axis',(-1.,0.,0.));
#31805=DIRECTION('ref_axis',(0.,-1.,0.));
#31806=DIRECTION('',(0.923879532511285,-0.382683432365095,4.68652040532636E-17));
#31807=DIRECTION('center_axis',(1.,0.,0.));
#31808=DIRECTION('ref_axis',(0.,-1.,0.));
#31809=DIRECTION('center_axis',(1.,0.,0.));
#31810=DIRECTION('ref_axis',(0.,-1.,0.));
#31811=DIRECTION('center_axis',(1.,0.,0.));
#31812=DIRECTION('ref_axis',(0.,1.,0.));
#31813=DIRECTION('center_axis',(1.,0.,0.));
#31814=DIRECTION('ref_axis',(0.,0.,-1.));
#31815=DIRECTION('',(-1.,0.,0.));
#31816=DIRECTION('center_axis',(1.,0.,0.));
#31817=DIRECTION('ref_axis',(0.,0.,-1.));
#31818=DIRECTION('center_axis',(1.,0.,0.));
#31819=DIRECTION('ref_axis',(0.,1.,0.));
#31820=DIRECTION('center_axis',(1.,0.,0.));
#31821=DIRECTION('ref_axis',(0.,0.,-1.));
#31822=DIRECTION('center_axis',(1.,0.,0.));
#31823=DIRECTION('ref_axis',(0.,1.,0.));
#31824=DIRECTION('center_axis',(1.,0.,0.));
#31825=DIRECTION('ref_axis',(0.,0.,-1.));
#31826=DIRECTION('',(1.,0.,0.));
#31827=DIRECTION('center_axis',(-1.,0.,0.));
#31828=DIRECTION('ref_axis',(0.,0.,1.));
#31829=DIRECTION('center_axis',(-1.,0.,0.));
#31830=DIRECTION('ref_axis',(0.,1.,0.));
#31831=DIRECTION('center_axis',(1.,0.,0.));
#31832=DIRECTION('ref_axis',(0.,1.,0.));
#31833=DIRECTION('',(-1.,0.,0.));
#31834=DIRECTION('center_axis',(1.,0.,0.));
#31835=DIRECTION('ref_axis',(0.,0.,-1.));
#31836=DIRECTION('center_axis',(1.,0.,0.));
#31837=DIRECTION('ref_axis',(0.,1.,0.));
#31838=DIRECTION('',(-0.707106781186552,0.707106781186543,8.65956056235488E-17));
#31839=DIRECTION('center_axis',(1.,0.,0.));
#31840=DIRECTION('ref_axis',(0.,1.,0.));
#31841=DIRECTION('center_axis',(1.,0.,0.));
#31842=DIRECTION('ref_axis',(0.,0.,-1.));
#31843=DIRECTION('',(-1.,0.,0.));
#31844=DIRECTION('center_axis',(-1.,0.,0.));
#31845=DIRECTION('ref_axis',(0.,1.,0.));
#31846=DIRECTION('center_axis',(1.,0.,0.));
#31847=DIRECTION('ref_axis',(0.,0.,-1.));
#31848=DIRECTION('',(-0.707106781186552,-0.707106781186543,-8.65956056235488E-17));
#31849=DIRECTION('center_axis',(1.,0.,0.));
#31850=DIRECTION('ref_axis',(0.,0.,-1.));
#31851=DIRECTION('center_axis',(1.,0.,0.));
#31852=DIRECTION('ref_axis',(0.,0.,-1.));
#31853=DIRECTION('center_axis',(1.,0.,0.));
#31854=DIRECTION('ref_axis',(0.,1.,0.));
#31855=DIRECTION('',(-0.707106781186547,0.707106781186548,8.65956056235494E-17));
#31856=DIRECTION('axis',(0.,0.,1.));
#31857=DIRECTION('refdir',(1.,0.,0.));
#31858=DIRECTION('center_axis',(1.,0.,0.));
#31859=DIRECTION('ref_axis',(0.,-1.,0.));
#31860=DIRECTION('center_axis',(-1.,0.,0.));
#31861=DIRECTION('ref_axis',(0.,-1.,0.));
#31862=DIRECTION('center_axis',(-1.,0.,0.));
#31863=DIRECTION('ref_axis',(0.,-1.,0.));
#31864=DIRECTION('',(0.707106781186552,0.707106781186543,-8.65956056235487E-17));
#31865=DIRECTION('center_axis',(1.,0.,0.));
#31866=DIRECTION('ref_axis',(0.,-1.,0.));
#31867=DIRECTION('center_axis',(1.,0.,0.));
#31868=DIRECTION('ref_axis',(0.,0.,-1.));
#31869=DIRECTION('center_axis',(1.,0.,0.));
#31870=DIRECTION('ref_axis',(0.,0.,-1.));
#31871=DIRECTION('center_axis',(1.,0.,0.));
#31872=DIRECTION('ref_axis',(0.,1.,0.));
#31873=DIRECTION('',(-1.,0.,0.));
#31874=DIRECTION('center_axis',(1.,0.,0.));
#31875=DIRECTION('ref_axis',(0.,0.,-1.));
#31876=DIRECTION('center_axis',(-1.,0.,0.));
#31877=DIRECTION('ref_axis',(0.,-1.,0.));
#31878=DIRECTION('center_axis',(-1.,0.,0.));
#31879=DIRECTION('ref_axis',(0.,-1.,0.));
#31880=DIRECTION('',(-0.38268343236509,0.923879532511287,1.1314261122877E-16));
#31881=DIRECTION('center_axis',(1.,0.,-1.4359375832322E-16));
#31882=DIRECTION('ref_axis',(0.,-1.,0.));
#31883=DIRECTION('center_axis',(1.,0.,-1.4359375832322E-16));
#31884=DIRECTION('ref_axis',(0.,-1.,0.));
#31885=DIRECTION('center_axis',(-1.,0.,0.));
#31886=DIRECTION('ref_axis',(0.,1.,0.));
#31887=DIRECTION('',(-0.707106781186548,-0.707106781186548,-8.65956056235493E-17));
#31888=DIRECTION('center_axis',(-1.,0.,0.));
#31889=DIRECTION('ref_axis',(0.,-1.,0.));
#31890=DIRECTION('center_axis',(-1.,0.,0.));
#31891=DIRECTION('ref_axis',(0.,-1.,0.));
#31892=DIRECTION('center_axis',(1.,0.,0.));
#31893=DIRECTION('ref_axis',(0.,0.,-1.));
#31894=DIRECTION('center_axis',(1.,0.,0.));
#31895=DIRECTION('ref_axis',(0.,0.,-1.));
#31896=DIRECTION('center_axis',(-1.,0.,0.));
#31897=DIRECTION('ref_axis',(0.,0.,1.));
#31898=DIRECTION('center_axis',(-1.,0.,0.));
#31899=DIRECTION('ref_axis',(0.,0.,1.));
#31900=DIRECTION('center_axis',(-1.,0.,0.));
#31901=DIRECTION('ref_axis',(0.,0.,1.));
#31902=DIRECTION('center_axis',(-1.,0.,0.));
#31903=DIRECTION('ref_axis',(0.,0.,1.));
#31904=DIRECTION('center_axis',(-1.,0.,0.));
#31905=DIRECTION('ref_axis',(0.,-1.,0.));
#31906=DIRECTION('',(-0.923879532511287,0.38268343236509,4.6865204053263E-17));
#31907=DIRECTION('center_axis',(1.,0.,0.));
#31908=DIRECTION('ref_axis',(0.,-1.,0.));
#31909=DIRECTION('center_axis',(1.,0.,0.));
#31910=DIRECTION('ref_axis',(0.,-1.,0.));
#31911=DIRECTION('center_axis',(1.,0.,0.));
#31912=DIRECTION('ref_axis',(0.,1.,0.));
#31913=DIRECTION('',(-1.,0.,0.));
#31914=DIRECTION('center_axis',(-1.,0.,0.));
#31915=DIRECTION('ref_axis',(0.,-1.,0.));
#31916=DIRECTION('center_axis',(-1.,0.,0.));
#31917=DIRECTION('ref_axis',(0.,-1.,0.));
#31918=DIRECTION('center_axis',(1.,0.,0.));
#31919=DIRECTION('ref_axis',(0.,-1.,0.));
#31920=DIRECTION('',(-0.923879532511287,-0.38268343236509,-4.6865204053263E-17));
#31921=DIRECTION('center_axis',(1.,0.,0.));
#31922=DIRECTION('ref_axis',(0.,-1.,0.));
#31923=DIRECTION('center_axis',(1.,0.,0.));
#31924=DIRECTION('ref_axis',(0.,-1.,0.));
#31925=DIRECTION('center_axis',(1.,0.,0.));
#31926=DIRECTION('ref_axis',(0.,1.,0.));
#31927=DIRECTION('',(-0.707106781186551,0.707106781186545,8.6595605623549E-17));
#31928=DIRECTION('center_axis',(-1.,0.,-1.4359375832322E-16));
#31929=DIRECTION('ref_axis',(0.,-1.,0.));
#31930=DIRECTION('center_axis',(-1.,0.,-1.4359375832322E-16));
#31931=DIRECTION('ref_axis',(0.,-1.,0.));
#31932=DIRECTION('center_axis',(1.,0.,0.));
#31933=DIRECTION('ref_axis',(0.,-1.,0.));
#31934=DIRECTION('',(-0.38268343236509,-0.923879532511287,-1.1314261122877E-16));
#31935=DIRECTION('center_axis',(1.,0.,0.));
#31936=DIRECTION('ref_axis',(0.,-1.,0.));
#31937=DIRECTION('center_axis',(-1.,0.,0.));
#31938=DIRECTION('ref_axis',(0.,0.,1.));
#31939=DIRECTION('center_axis',(1.,0.,0.));
#31940=DIRECTION('ref_axis',(0.,0.,-1.));
#31941=DIRECTION('center_axis',(1.,0.,0.));
#31942=DIRECTION('ref_axis',(0.,0.,1.));
#31943=DIRECTION('center_axis',(1.,0.,0.));
#31944=DIRECTION('ref_axis',(0.,0.,1.));
#31945=DIRECTION('center_axis',(1.,0.,0.));
#31946=DIRECTION('ref_axis',(0.,0.,1.));
#31947=DIRECTION('center_axis',(1.,0.,0.));
#31948=DIRECTION('ref_axis',(0.,0.,1.));
#31949=DIRECTION('center_axis',(1.,0.,0.));
#31950=DIRECTION('ref_axis',(0.,-1.,0.));
#31951=DIRECTION('center_axis',(-1.,0.,0.));
#31952=DIRECTION('ref_axis',(0.,-1.,0.));
#31953=DIRECTION('center_axis',(-1.,0.,0.));
#31954=DIRECTION('ref_axis',(0.,-1.,0.));
#31955=DIRECTION('',(-0.923879532511288,-0.382683432365086,-4.68652040532625E-17));
#31956=DIRECTION('center_axis',(1.,0.,0.));
#31957=DIRECTION('ref_axis',(0.,-1.,0.));
#31958=DIRECTION('center_axis',(1.,0.,0.));
#31959=DIRECTION('ref_axis',(0.,-1.,0.));
#31960=DIRECTION('center_axis',(1.,0.,0.));
#31961=DIRECTION('ref_axis',(0.,1.,0.));
#31962=DIRECTION('',(-0.707106781186551,0.707106781186544,8.6595605623549E-17));
#31963=DIRECTION('center_axis',(-1.,0.,3.24703122485565E-16));
#31964=DIRECTION('ref_axis',(0.,-1.,0.));
#31965=DIRECTION('center_axis',(-1.,0.,3.24703122485565E-16));
#31966=DIRECTION('ref_axis',(0.,-1.,0.));
#31967=DIRECTION('center_axis',(1.,0.,0.));
#31968=DIRECTION('ref_axis',(0.,1.,0.));
#31969=DIRECTION('',(-1.,0.,0.));
#31970=DIRECTION('center_axis',(1.,0.,0.));
#31971=DIRECTION('ref_axis',(0.,-1.,0.));
#31972=DIRECTION('',(-0.38268343236509,-0.923879532511287,-1.1314261122877E-16));
#31973=DIRECTION('center_axis',(1.,0.,0.));
#31974=DIRECTION('ref_axis',(0.,-1.,0.));
#31975=DIRECTION('center_axis',(-1.,0.,0.));
#31976=DIRECTION('ref_axis',(0.,0.,1.));
#31977=DIRECTION('center_axis',(-1.,0.,0.));
#31978=DIRECTION('ref_axis',(0.,-1.,0.));
#31979=DIRECTION('center_axis',(-1.,0.,0.));
#31980=DIRECTION('ref_axis',(0.,-1.,0.));
#31981=DIRECTION('',(0.707106781186546,-0.707106781186549,8.65956056235495E-17));
#31982=DIRECTION('center_axis',(1.,0.,0.));
#31983=DIRECTION('ref_axis',(0.,-1.,0.));
#31984=DIRECTION('center_axis',(1.,0.,0.));
#31985=DIRECTION('ref_axis',(0.,-1.,0.));
#31986=DIRECTION('center_axis',(1.,0.,0.));
#31987=DIRECTION('ref_axis',(0.,1.,0.));
#31988=DIRECTION('center_axis',(1.,0.,0.));
#31989=DIRECTION('ref_axis',(0.,0.,-1.));
#31990=DIRECTION('',(-1.,0.,0.));
#31991=DIRECTION('center_axis',(-1.,0.,0.));
#31992=DIRECTION('ref_axis',(0.,0.,1.));
#31993=DIRECTION('',(-1.,0.,0.));
#31994=DIRECTION('center_axis',(-1.,0.,0.));
#31995=DIRECTION('ref_axis',(0.,0.,1.));
#31996=DIRECTION('',(-1.,0.,0.));
#31997=DIRECTION('center_axis',(-1.,0.,0.));
#31998=DIRECTION('ref_axis',(0.,0.,1.));
#31999=DIRECTION('',(-1.,0.,0.));
#32000=DIRECTION('center_axis',(-1.,0.,0.));
#32001=DIRECTION('ref_axis',(0.,0.,1.));
#32002=DIRECTION('',(-1.,0.,0.));
#32003=DIRECTION('center_axis',(1.,0.,0.));
#32004=DIRECTION('ref_axis',(0.,1.,0.));
#32005=DIRECTION('center_axis',(1.,0.,0.));
#32006=DIRECTION('ref_axis',(0.,0.,-1.));
#32007=DIRECTION('',(-1.,0.,0.));
#32008=DIRECTION('center_axis',(-1.,0.,0.));
#32009=DIRECTION('ref_axis',(0.,1.,0.));
#32010=DIRECTION('',(-0.707106781186554,-0.707106781186541,-8.65956056235486E-17));
#32011=DIRECTION('center_axis',(1.,0.,0.));
#32012=DIRECTION('ref_axis',(0.,0.,-1.));
#32013=DIRECTION('center_axis',(1.,0.,0.));
#32014=DIRECTION('ref_axis',(0.,0.,-1.));
#32015=DIRECTION('center_axis',(1.,0.,0.));
#32016=DIRECTION('ref_axis',(0.,1.,0.));
#32017=DIRECTION('',(-1.,0.,0.));
#32018=DIRECTION('center_axis',(1.,0.,0.));
#32019=DIRECTION('ref_axis',(0.,0.,-1.));
#32020=DIRECTION('center_axis',(-1.,0.,0.));
#32021=DIRECTION('ref_axis',(0.,0.,1.));
#32022=DIRECTION('axis',(0.,0.,1.));
#32023=DIRECTION('refdir',(1.,0.,0.));
#32024=DIRECTION('center_axis',(-1.,0.,0.));
#32025=DIRECTION('ref_axis',(0.,-1.,0.));
#32026=DIRECTION('center_axis',(-1.,0.,0.));
#32027=DIRECTION('ref_axis',(0.,-1.,0.));
#32028=DIRECTION('center_axis',(-1.,0.,0.));
#32029=DIRECTION('ref_axis',(0.,-1.,0.));
#32030=DIRECTION('',(-0.923879532511287,0.38268343236509,4.6865204053263E-17));
#32031=DIRECTION('center_axis',(1.,0.,0.));
#32032=DIRECTION('ref_axis',(0.,-1.,0.));
#32033=DIRECTION('center_axis',(1.,0.,0.));
#32034=DIRECTION('ref_axis',(0.,-1.,0.));
#32035=DIRECTION('center_axis',(1.,0.,0.));
#32036=DIRECTION('ref_axis',(0.,1.,0.));
#32037=DIRECTION('',(-1.,0.,0.));
#32038=DIRECTION('center_axis',(-1.,0.,0.));
#32039=DIRECTION('ref_axis',(0.,-1.,0.));
#32040=DIRECTION('center_axis',(-1.,0.,0.));
#32041=DIRECTION('ref_axis',(0.,-1.,0.));
#32042=DIRECTION('center_axis',(-1.,0.,0.));
#32043=DIRECTION('ref_axis',(0.,1.,0.));
#32044=DIRECTION('center_axis',(1.,0.,-3.64701776966638E-16));
#32045=DIRECTION('ref_axis',(0.,-1.,0.));
#32046=DIRECTION('center_axis',(1.,0.,-3.64701776966638E-16));
#32047=DIRECTION('ref_axis',(0.,-1.,0.));
#32048=DIRECTION('',(-0.707106781186546,-0.707106781186549,-8.65956056235495E-17));
#32049=DIRECTION('center_axis',(1.,0.,0.));
#32050=DIRECTION('ref_axis',(0.,-1.,0.));
#32051=DIRECTION('',(-0.923879532511287,-0.382683432365088,-4.68652040532628E-17));
#32052=DIRECTION('center_axis',(1.,0.,1.35137901485737E-16));
#32053=DIRECTION('ref_axis',(0.,-1.,0.));
#32054=DIRECTION('center_axis',(1.,0.,1.35137901485737E-16));
#32055=DIRECTION('ref_axis',(0.,-1.,0.));
#32056=DIRECTION('center_axis',(1.,0.,0.));
#32057=DIRECTION('ref_axis',(0.,1.,0.));
#32058=DIRECTION('',(-0.707106781186547,0.707106781186548,8.65956056235494E-17));
#32059=DIRECTION('center_axis',(-1.,0.,-4.55877221208297E-16));
#32060=DIRECTION('ref_axis',(0.,-1.,0.));
#32061=DIRECTION('center_axis',(-1.,0.,-4.55877221208297E-16));
#32062=DIRECTION('ref_axis',(0.,-1.,0.));
#32063=DIRECTION('center_axis',(1.,0.,0.));
#32064=DIRECTION('ref_axis',(0.,-1.,0.));
#32065=DIRECTION('',(-0.382683432365089,-0.923879532511287,-1.1314261122877E-16));
#32066=DIRECTION('center_axis',(1.,0.,0.));
#32067=DIRECTION('ref_axis',(0.,-1.,0.));
#32068=DIRECTION('center_axis',(-1.,0.,0.));
#32069=DIRECTION('ref_axis',(0.,0.,1.));
#32070=DIRECTION('center_axis',(1.,0.,0.));
#32071=DIRECTION('ref_axis',(0.,0.,-1.));
#32072=DIRECTION('center_axis',(-1.,0.,0.));
#32073=DIRECTION('ref_axis',(0.,-1.,0.));
#32074=DIRECTION('center_axis',(-1.,0.,0.));
#32075=DIRECTION('ref_axis',(0.,-1.,0.));
#32076=DIRECTION('',(-0.38268343236509,0.923879532511287,1.1314261122877E-16));
#32077=DIRECTION('center_axis',(1.,0.,0.));
#32078=DIRECTION('ref_axis',(0.,0.,-1.));
#32079=DIRECTION('',(0.,0.,1.));
#32080=DIRECTION('center_axis',(1.,0.,0.));
#32081=DIRECTION('ref_axis',(0.,0.,-1.));
#32082=DIRECTION('',(0.,0.,-1.));
#32083=DIRECTION('',(0.,-1.,0.));
#32084=DIRECTION('center_axis',(0.707106781186548,-0.707106781186547,0.));
#32085=DIRECTION('ref_axis',(0.,0.,-1.));
#32086=DIRECTION('',(0.,0.,-1.));
#32087=DIRECTION('center_axis',(-0.707106781186548,0.707106781186547,0.));
#32088=DIRECTION('ref_axis',(0.707106781186547,0.707106781186548,0.));
#32089=DIRECTION('',(-0.577350269189608,-0.57735026918961,-0.57735026918966));
#32090=DIRECTION('center_axis',(0.707106781186554,0.707106781186541,0.));
#32091=DIRECTION('ref_axis',(0.,0.,-1.));
#32092=DIRECTION('center_axis',(-0.707106781186554,-0.707106781186541,0.));
#32093=DIRECTION('ref_axis',(-0.707106781186541,0.707106781186554,0.));
#32094=DIRECTION('',(0.,0.,1.));
#32095=DIRECTION('',(0.577350269189602,-0.577350269189613,0.577350269189663));
#32096=DIRECTION('center_axis',(0.707106781186579,0.,-0.707106781186516));
#32097=DIRECTION('ref_axis',(-0.707106781186516,0.,-0.707106781186579));
#32098=DIRECTION('',(0.,1.,0.));
#32099=DIRECTION('center_axis',(0.,0.,1.));
#32100=DIRECTION('ref_axis',(1.,0.,0.));
#32101=DIRECTION('',(1.,0.,0.));
#32102=DIRECTION('',(0.,-1.,0.));
#32103=DIRECTION('',(-1.,0.,0.));
#32104=DIRECTION('center_axis',(0.,-1.,0.));
#32105=DIRECTION('ref_axis',(-1.,0.,0.));
#32106=DIRECTION('',(1.,0.,0.));
#32107=DIRECTION('',(0.,0.,-1.));
#32108=DIRECTION('center_axis',(0.,1.,0.));
#32109=DIRECTION('ref_axis',(1.,0.,0.));
#32110=DIRECTION('',(0.,0.,-1.));
#32111=DIRECTION('',(-1.,0.,0.));
#32112=DIRECTION('center_axis',(1.,0.,0.));
#32113=DIRECTION('ref_axis',(0.,6.12323399573677E-17,-1.));
#32114=DIRECTION('center_axis',(1.,0.,0.));
#32115=DIRECTION('ref_axis',(0.,0.,-1.));
#32116=DIRECTION('center_axis',(0.,-0.707106781186547,0.707106781186548));
#32117=DIRECTION('ref_axis',(0.,0.707106781186548,0.707106781186547));
#32118=DIRECTION('',(-3.92313542605626E-18,-0.729395907617851,0.684091813976992));
#32119=DIRECTION('center_axis',(0.,0.707106781186548,0.707106781186547));
#32120=DIRECTION('ref_axis',(0.,0.707106781186548,-0.707106781186547));
#32121=DIRECTION('',(-3.92313542605626E-18,0.684091813976992,0.729395907617851));
#32122=DIRECTION('center_axis',(0.,0.707106781186547,-0.707106781186548));
#32123=DIRECTION('ref_axis',(0.,-0.707106781186546,-0.707106781186549));
#32124=DIRECTION('',(-3.92313542605623E-18,0.729395907617851,-0.684091813976992));
#32125=DIRECTION('center_axis',(0.,-0.707106781186547,-0.707106781186548));
#32126=DIRECTION('ref_axis',(0.,-0.707106781186548,0.707106781186547));
#32127=DIRECTION('',(-3.92313542605642E-18,-0.68409181397699,-0.729395907617853));
#32128=DIRECTION('center_axis',(1.,0.,0.));
#32129=DIRECTION('ref_axis',(0.,0.,-1.));
#32130=DIRECTION('center_axis',(0.,-1.,-1.22464679914735E-16));
#32131=DIRECTION('ref_axis',(0.,-1.22464679914735E-16,1.));
#32132=DIRECTION('center_axis',(-1.,0.,0.));
#32133=DIRECTION('ref_axis',(0.,0.,-1.));
#32134=DIRECTION('center_axis',(-1.,0.,0.));
#32135=DIRECTION('ref_axis',(0.,0.,-1.));
#32136=DIRECTION('center_axis',(-1.,0.,0.));
#32137=DIRECTION('ref_axis',(0.,0.,-1.));
#32138=DIRECTION('center_axis',(-1.,0.,0.));
#32139=DIRECTION('ref_axis',(0.,0.,-1.));
#32140=DIRECTION('center_axis',(-1.,0.,0.));
#32141=DIRECTION('ref_axis',(0.,0.,-1.));
#32142=DIRECTION('center_axis',(1.,0.,0.));
#32143=DIRECTION('ref_axis',(0.,1.,0.));
#32144=DIRECTION('center_axis',(1.,0.,0.));
#32145=DIRECTION('ref_axis',(0.,0.,-1.));
#32146=DIRECTION('',(-1.,0.,0.));
#32147=DIRECTION('center_axis',(1.,0.,0.));
#32148=DIRECTION('ref_axis',(0.,0.,-1.));
#32149=DIRECTION('axis',(0.,0.,1.));
#32150=DIRECTION('refdir',(1.,0.,0.));
#32151=DIRECTION('center_axis',(0.,0.,1.));
#32152=DIRECTION('ref_axis',(1.,0.,0.));
#32153=DIRECTION('',(0.,0.,-1.));
#32154=DIRECTION('center_axis',(0.,0.,1.));
#32155=DIRECTION('ref_axis',(1.,0.,0.));
#32156=DIRECTION('center_axis',(0.,0.,1.));
#32157=DIRECTION('ref_axis',(1.,0.,0.));
#32158=DIRECTION('',(0.,0.,-1.));
#32159=DIRECTION('center_axis',(0.,0.,1.));
#32160=DIRECTION('ref_axis',(1.,0.,0.));
#32161=DIRECTION('',(0.,0.,-1.));
#32162=DIRECTION('center_axis',(0.,0.,1.));
#32163=DIRECTION('ref_axis',(1.,0.,0.));
#32164=DIRECTION('',(0.,0.,-1.));
#32165=DIRECTION('center_axis',(0.,0.,1.));
#32166=DIRECTION('ref_axis',(1.,0.,0.));
#32167=DIRECTION('',(0.,0.,-1.));
#32168=DIRECTION('center_axis',(0.,0.,1.));
#32169=DIRECTION('ref_axis',(1.,0.,0.));
#32170=DIRECTION('',(0.,0.,-1.));
#32171=DIRECTION('center_axis',(0.,0.,1.));
#32172=DIRECTION('ref_axis',(1.,0.,0.));
#32173=DIRECTION('',(0.,0.,-1.));
#32174=DIRECTION('center_axis',(0.,0.,1.));
#32175=DIRECTION('ref_axis',(1.,0.,0.));
#32176=DIRECTION('',(0.,0.,-1.));
#32177=DIRECTION('center_axis',(0.,0.,1.));
#32178=DIRECTION('ref_axis',(1.,0.,0.));
#32179=DIRECTION('',(0.,0.,-1.));
#32180=DIRECTION('center_axis',(0.,0.,1.));
#32181=DIRECTION('ref_axis',(1.,0.,0.));
#32182=DIRECTION('',(0.,0.,-1.));
#32183=DIRECTION('center_axis',(0.,0.,1.));
#32184=DIRECTION('ref_axis',(1.,0.,0.));
#32185=DIRECTION('',(0.,0.,-1.));
#32186=DIRECTION('center_axis',(0.,0.,1.));
#32187=DIRECTION('ref_axis',(1.,0.,0.));
#32188=DIRECTION('',(0.,0.,-1.));
#32189=DIRECTION('center_axis',(0.,0.,1.));
#32190=DIRECTION('ref_axis',(1.,0.,0.));
#32191=DIRECTION('',(0.,0.,-1.));
#32192=DIRECTION('center_axis',(0.,0.,1.));
#32193=DIRECTION('ref_axis',(1.,0.,0.));
#32194=DIRECTION('',(0.,0.,-1.));
#32195=DIRECTION('center_axis',(0.,0.,1.));
#32196=DIRECTION('ref_axis',(1.,0.,0.));
#32197=DIRECTION('',(0.,0.,-1.));
#32198=DIRECTION('center_axis',(0.,0.,1.));
#32199=DIRECTION('ref_axis',(1.,0.,0.));
#32200=DIRECTION('',(0.,0.,-1.));
#32201=DIRECTION('center_axis',(0.,0.,1.));
#32202=DIRECTION('ref_axis',(0.812982922164426,-0.582287530580031,0.));
#32203=DIRECTION('',(0.,0.,1.));
#32204=DIRECTION('center_axis',(0.,0.,1.));
#32205=DIRECTION('ref_axis',(1.,9.56839379238543E-14,0.));
#32206=DIRECTION('center_axis',(0.,0.,1.));
#32207=DIRECTION('ref_axis',(1.,9.56839379238543E-14,0.));
#32208=DIRECTION('',(0.,0.,1.));
#32209=DIRECTION('center_axis',(0.,0.,1.));
#32210=DIRECTION('ref_axis',(1.,9.56839379238543E-14,0.));
#32211=DIRECTION('',(0.,0.,1.));
#32212=DIRECTION('center_axis',(0.,0.,1.));
#32213=DIRECTION('ref_axis',(1.,9.56839379238543E-14,0.));
#32214=DIRECTION('',(0.,0.,1.));
#32215=DIRECTION('center_axis',(0.,0.,1.));
#32216=DIRECTION('ref_axis',(1.,9.56839379238543E-14,0.));
#32217=DIRECTION('',(0.,0.,1.));
#32218=DIRECTION('center_axis',(0.,0.,1.));
#32219=DIRECTION('ref_axis',(1.,9.56839379238543E-14,0.));
#32220=DIRECTION('',(0.,0.,1.));
#32221=DIRECTION('center_axis',(0.,0.,1.));
#32222=DIRECTION('ref_axis',(1.,9.56839379238543E-14,0.));
#32223=DIRECTION('',(0.,0.,1.));
#32224=DIRECTION('center_axis',(0.,0.,1.));
#32225=DIRECTION('ref_axis',(1.,9.56839379238543E-14,0.));
#32226=DIRECTION('',(0.,0.,1.));
#32227=DIRECTION('center_axis',(0.,0.,1.));
#32228=DIRECTION('ref_axis',(1.,9.56839379238543E-14,0.));
#32229=DIRECTION('',(0.,0.,1.));
#32230=DIRECTION('center_axis',(0.,0.,1.));
#32231=DIRECTION('ref_axis',(1.,9.56839379238543E-14,0.));
#32232=DIRECTION('',(0.,0.,1.));
#32233=DIRECTION('center_axis',(0.,0.,1.));
#32234=DIRECTION('ref_axis',(1.,9.56839379238543E-14,0.));
#32235=DIRECTION('',(0.,0.,1.));
#32236=DIRECTION('center_axis',(0.,0.,1.));
#32237=DIRECTION('ref_axis',(1.,9.56839379238543E-14,0.));
#32238=DIRECTION('',(0.,0.,1.));
#32239=DIRECTION('center_axis',(0.,0.,1.));
#32240=DIRECTION('ref_axis',(1.,9.56839379238543E-14,0.));
#32241=DIRECTION('',(0.,0.,1.));
#32242=DIRECTION('center_axis',(0.,0.,1.));
#32243=DIRECTION('ref_axis',(1.,9.56839379238543E-14,0.));
#32244=DIRECTION('',(0.,0.,1.));
#32245=DIRECTION('center_axis',(0.,0.,1.));
#32246=DIRECTION('ref_axis',(1.,9.56839379238543E-14,0.));
#32247=DIRECTION('',(0.,0.,1.));
#32248=DIRECTION('center_axis',(0.,0.,1.));
#32249=DIRECTION('ref_axis',(1.,0.,0.));
#32250=DIRECTION('center_axis',(0.,0.,1.));
#32251=DIRECTION('ref_axis',(1.,0.,0.));
#32252=DIRECTION('center_axis',(0.,0.,1.));
#32253=DIRECTION('ref_axis',(1.,0.,0.));
#32254=DIRECTION('center_axis',(0.,0.,1.));
#32255=DIRECTION('ref_axis',(1.,0.,0.));
#32256=DIRECTION('center_axis',(0.,0.,1.));
#32257=DIRECTION('ref_axis',(1.,0.,0.));
#32258=DIRECTION('center_axis',(0.,0.,1.));
#32259=DIRECTION('ref_axis',(1.,0.,0.));
#32260=DIRECTION('center_axis',(0.,0.,-1.));
#32261=DIRECTION('ref_axis',(1.,9.56839379238543E-14,0.));
#32262=DIRECTION('center_axis',(0.,0.,1.));
#32263=DIRECTION('ref_axis',(1.,9.56839379238543E-14,0.));
#32264=DIRECTION('center_axis',(0.,0.,1.));
#32265=DIRECTION('ref_axis',(1.,0.,0.));
#32266=DIRECTION('center_axis',(1.22464679914735E-16,-1.,0.));
#32267=DIRECTION('ref_axis',(-1.,-1.22464679914735E-16,0.));
#32268=DIRECTION('center_axis',(0.,0.,-1.));
#32269=DIRECTION('ref_axis',(1.,0.,0.));
#32270=DIRECTION('center_axis',(0.,0.,1.));
#32271=DIRECTION('ref_axis',(1.,0.,0.));
#32272=DIRECTION('center_axis',(0.,0.,1.));
#32273=DIRECTION('ref_axis',(-0.645026930002996,-0.764159839019894,0.));
#32274=DIRECTION('center_axis',(0.,0.,-1.));
#32275=DIRECTION('ref_axis',(-1.,0.,0.));
#32276=DIRECTION('center_axis',(0.,0.,1.));
#32277=DIRECTION('ref_axis',(1.,0.,0.));
#32278=DIRECTION('center_axis',(0.,0.,1.));
#32279=DIRECTION('ref_axis',(1.,0.,0.));
#32280=DIRECTION('',(0.5,-0.866025403784439,0.));
#32281=DIRECTION('center_axis',(0.,0.,1.));
#32282=DIRECTION('ref_axis',(1.,0.,0.));
#32283=DIRECTION('center_axis',(0.,0.,1.));
#32284=DIRECTION('ref_axis',(1.,0.,0.));
#32285=DIRECTION('',(-0.5,-0.866025403784439,0.));
#32286=DIRECTION('center_axis',(0.,0.,1.));
#32287=DIRECTION('ref_axis',(1.,0.,0.));
#32288=DIRECTION('center_axis',(0.,0.,1.));
#32289=DIRECTION('ref_axis',(1.,0.,0.));
#32290=DIRECTION('',(-1.,1.60246890531964E-16,0.));
#32291=DIRECTION('center_axis',(0.,0.,1.));
#32292=DIRECTION('ref_axis',(1.,0.,0.));
#32293=DIRECTION('center_axis',(0.,0.,1.));
#32294=DIRECTION('ref_axis',(1.,0.,0.));
#32295=DIRECTION('',(-0.5,0.866025403784439,0.));
#32296=DIRECTION('center_axis',(0.,0.,1.));
#32297=DIRECTION('ref_axis',(1.,0.,0.));
#32298=DIRECTION('center_axis',(0.,0.,1.));
#32299=DIRECTION('ref_axis',(1.,0.,0.));
#32300=DIRECTION('',(0.5,0.866025403784439,0.));
#32301=DIRECTION('center_axis',(0.,0.,1.));
#32302=DIRECTION('ref_axis',(1.,0.,0.));
#32303=DIRECTION('center_axis',(0.,0.,1.));
#32304=DIRECTION('ref_axis',(1.,0.,0.));
#32305=DIRECTION('',(1.,-1.60246890531964E-16,0.));
#32306=DIRECTION('center_axis',(0.,0.,1.));
#32307=DIRECTION('ref_axis',(1.,0.,0.));
#32308=DIRECTION('center_axis',(0.,0.,1.));
#32309=DIRECTION('ref_axis',(1.,0.,0.));
#32310=DIRECTION('',(-0.857492925712544,-1.05012596676537E-16,0.514495755427527));
#32311=DIRECTION('center_axis',(0.866025403784439,0.5,0.));
#32312=DIRECTION('ref_axis',(0.5,-0.866025403784439,0.));
#32313=DIRECTION('',(0.5,-0.866025403784439,0.));
#32314=DIRECTION('',(0.,0.,-1.));
#32315=DIRECTION('',(0.,0.,-1.));
#32316=DIRECTION('center_axis',(1.60246890531964E-16,1.,0.));
#32317=DIRECTION('ref_axis',(1.,-1.60246890531964E-16,0.));
#32318=DIRECTION('',(1.,-1.60246890531964E-16,0.));
#32319=DIRECTION('',(0.,0.,-1.));
#32320=DIRECTION('center_axis',(-0.866025403784439,0.5,0.));
#32321=DIRECTION('ref_axis',(0.5,0.866025403784439,0.));
#32322=DIRECTION('',(0.5,0.866025403784439,0.));
#32323=DIRECTION('',(0.,0.,-1.));
#32324=DIRECTION('center_axis',(-0.866025403784439,-0.5,0.));
#32325=DIRECTION('ref_axis',(-0.5,0.866025403784439,0.));
#32326=DIRECTION('',(-0.5,0.866025403784439,0.));
#32327=DIRECTION('',(0.,0.,-1.));
#32328=DIRECTION('center_axis',(-1.60246890531964E-16,-1.,0.));
#32329=DIRECTION('ref_axis',(-1.,1.60246890531964E-16,0.));
#32330=DIRECTION('',(-1.,1.60246890531964E-16,0.));
#32331=DIRECTION('',(0.,0.,-1.));
#32332=DIRECTION('center_axis',(0.866025403784439,-0.5,0.));
#32333=DIRECTION('ref_axis',(-0.5,-0.866025403784439,0.));
#32334=DIRECTION('',(-0.5,-0.866025403784439,0.));
#32335=DIRECTION('center_axis',(-0.782019212317096,-0.623254323343969,0.));
#32336=DIRECTION('ref_axis',(-0.623254323343969,0.782019212317096,0.));
#32337=DIRECTION('',(0.,0.,1.));
#32338=DIRECTION('',(-0.623254323343969,0.782019212317096,0.));
#32339=DIRECTION('',(0.,0.,-1.));
#32340=DIRECTION('',(-0.623254323343969,0.782019212317096,0.));
#32341=DIRECTION('center_axis',(0.,0.,1.));
#32342=DIRECTION('ref_axis',(1.,0.,0.));
#32343=DIRECTION('center_axis',(0.,0.,1.));
#32344=DIRECTION('ref_axis',(1.,0.,0.));
#32345=DIRECTION('',(0.980112771261784,0.198441315278714,0.));
#32346=DIRECTION('center_axis',(-0.198441315278714,0.980112771261784,0.));
#32347=DIRECTION('ref_axis',(0.980112771261784,0.198441315278714,0.));
#32348=DIRECTION('',(0.,0.,-1.));
#32349=DIRECTION('',(0.980112771261784,0.198441315278714,0.));
#32350=DIRECTION('center_axis',(0.,0.,-1.));
#32351=DIRECTION('ref_axis',(-1.,0.,0.));
#32352=DIRECTION('center_axis',(0.,0.,-1.));
#32353=DIRECTION('ref_axis',(1.,0.,0.));
#32354=DIRECTION('center_axis',(-0.948023216125629,-0.318201165439129,0.));
#32355=DIRECTION('ref_axis',(-0.318201165439129,0.948023216125629,0.));
#32356=DIRECTION('',(0.,0.,1.));
#32357=DIRECTION('',(-0.318201165439129,0.948023216125629,0.));
#32358=DIRECTION('',(0.,0.,-1.));
#32359=DIRECTION('',(-0.318201165439129,0.948023216125629,0.));
#32360=DIRECTION('center_axis',(0.,0.,1.));
#32361=DIRECTION('ref_axis',(1.,0.,0.));
#32362=DIRECTION('center_axis',(0.,0.,1.));
#32363=DIRECTION('ref_axis',(1.,0.,0.));
#32364=DIRECTION('',(0.988875665786086,-0.148744470875809,0.));
#32365=DIRECTION('center_axis',(0.148744470875809,0.988875665786086,0.));
#32366=DIRECTION('ref_axis',(0.988875665786086,-0.148744470875809,0.));
#32367=DIRECTION('',(0.,0.,-1.));
#32368=DIRECTION('',(0.988875665786086,-0.148744470875809,0.));
#32369=DIRECTION('center_axis',(0.,0.,-1.));
#32370=DIRECTION('ref_axis',(-1.,0.,0.));
#32371=DIRECTION('center_axis',(0.,0.,-1.));
#32372=DIRECTION('ref_axis',(1.,0.,0.));
#32373=DIRECTION('center_axis',(-0.999681628736863,0.0252317491667324,0.));
#32374=DIRECTION('ref_axis',(0.0252317491667324,0.999681628736863,0.));
#32375=DIRECTION('',(0.,0.,1.));
#32376=DIRECTION('',(0.0252317491667324,0.999681628736863,0.));
#32377=DIRECTION('',(0.,0.,-1.));
#32378=DIRECTION('',(0.0252317491667324,0.999681628736863,0.));
#32379=DIRECTION('center_axis',(0.,0.,1.));
#32380=DIRECTION('ref_axis',(1.,0.,0.));
#32381=DIRECTION('center_axis',(0.,0.,1.));
#32382=DIRECTION('ref_axis',(1.,0.,0.));
#32383=DIRECTION('',(0.87836556076609,-0.477989478608131,0.));
#32384=DIRECTION('center_axis',(0.477989478608131,0.87836556076609,0.));
#32385=DIRECTION('ref_axis',(0.87836556076609,-0.477989478608131,0.));
#32386=DIRECTION('',(0.,0.,-1.));
#32387=DIRECTION('',(0.87836556076609,-0.477989478608131,0.));
#32388=DIRECTION('center_axis',(0.,0.,-1.));
#32389=DIRECTION('ref_axis',(-1.,0.,0.));
#32390=DIRECTION('center_axis',(0.,0.,-1.));
#32391=DIRECTION('ref_axis',(1.,0.,0.));
#32392=DIRECTION('center_axis',(-0.930763683192908,0.365621342442113,0.));
#32393=DIRECTION('ref_axis',(0.365621342442113,0.930763683192908,0.));
#32394=DIRECTION('',(0.,0.,1.));
#32395=DIRECTION('',(0.365621342442113,0.930763683192908,0.));
#32396=DIRECTION('',(0.,0.,-1.));
#32397=DIRECTION('',(0.365621342442113,0.930763683192908,0.));
#32398=DIRECTION('center_axis',(0.,0.,1.));
#32399=DIRECTION('ref_axis',(1.,0.,0.));
#32400=DIRECTION('center_axis',(0.,0.,1.));
#32401=DIRECTION('ref_axis',(1.,0.,0.));
#32402=DIRECTION('',(0.661911605822662,-0.749581900846909,0.));
#32403=DIRECTION('center_axis',(0.749581900846909,0.661911605822662,0.));
#32404=DIRECTION('ref_axis',(0.661911605822662,-0.749581900846909,0.));
#32405=DIRECTION('',(0.,0.,-1.));
#32406=DIRECTION('',(0.661911605822662,-0.749581900846909,0.));
#32407=DIRECTION('center_axis',(0.,0.,-1.));
#32408=DIRECTION('ref_axis',(-1.,0.,0.));
#32409=DIRECTION('center_axis',(0.,0.,-1.));
#32410=DIRECTION('ref_axis',(1.,0.,0.));
#32411=DIRECTION('center_axis',(-0.749581900846909,0.661911605822661,0.));
#32412=DIRECTION('ref_axis',(0.661911605822661,0.749581900846909,0.));
#32413=DIRECTION('',(0.,0.,1.));
#32414=DIRECTION('',(0.661911605822661,0.749581900846909,0.));
#32415=DIRECTION('',(0.,0.,-1.));
#32416=DIRECTION('',(0.661911605822661,0.749581900846909,0.));
#32417=DIRECTION('center_axis',(0.,0.,1.));
#32418=DIRECTION('ref_axis',(1.,0.,0.));
#32419=DIRECTION('center_axis',(0.,0.,1.));
#32420=DIRECTION('ref_axis',(1.,0.,0.));
#32421=DIRECTION('',(0.365621342442119,-0.930763683192905,0.));
#32422=DIRECTION('center_axis',(0.930763683192905,0.365621342442119,0.));
#32423=DIRECTION('ref_axis',(0.365621342442119,-0.930763683192905,0.));
#32424=DIRECTION('',(0.,0.,-1.));
#32425=DIRECTION('',(0.365621342442119,-0.930763683192905,0.));
#32426=DIRECTION('center_axis',(0.,0.,-1.));
#32427=DIRECTION('ref_axis',(-1.,0.,0.));
#32428=DIRECTION('center_axis',(0.,0.,-1.));
#32429=DIRECTION('ref_axis',(1.,0.,0.));
#32430=DIRECTION('center_axis',(-0.477989478608131,0.87836556076609,0.));
#32431=DIRECTION('ref_axis',(0.87836556076609,0.477989478608131,0.));
#32432=DIRECTION('',(0.,0.,1.));
#32433=DIRECTION('',(0.87836556076609,0.477989478608131,0.));
#32434=DIRECTION('',(0.,0.,-1.));
#32435=DIRECTION('',(0.87836556076609,0.477989478608131,0.));
#32436=DIRECTION('center_axis',(0.,0.,1.));
#32437=DIRECTION('ref_axis',(1.,0.,0.));
#32438=DIRECTION('center_axis',(0.,0.,1.));
#32439=DIRECTION('ref_axis',(1.,0.,0.));
#32440=DIRECTION('',(0.0252317491667324,-0.999681628736863,0.));
#32441=DIRECTION('center_axis',(0.999681628736863,0.0252317491667324,0.));
#32442=DIRECTION('ref_axis',(0.0252317491667324,-0.999681628736863,0.));
#32443=DIRECTION('',(0.,0.,-1.));
#32444=DIRECTION('',(0.0252317491667324,-0.999681628736863,0.));
#32445=DIRECTION('center_axis',(0.,0.,-1.));
#32446=DIRECTION('ref_axis',(-1.,0.,0.));
#32447=DIRECTION('center_axis',(0.,0.,-1.));
#32448=DIRECTION('ref_axis',(1.,0.,0.));
#32449=DIRECTION('center_axis',(-0.148744470875812,0.988875665786086,0.));
#32450=DIRECTION('ref_axis',(0.988875665786086,0.148744470875812,0.));
#32451=DIRECTION('',(0.,0.,1.));
#32452=DIRECTION('',(0.988875665786086,0.148744470875812,0.));
#32453=DIRECTION('',(0.,0.,-1.));
#32454=DIRECTION('',(0.988875665786086,0.148744470875812,0.));
#32455=DIRECTION('center_axis',(0.,0.,1.));
#32456=DIRECTION('ref_axis',(1.,0.,0.));
#32457=DIRECTION('center_axis',(0.,0.,1.));
#32458=DIRECTION('ref_axis',(1.,0.,0.));
#32459=DIRECTION('',(-0.318201165439124,-0.94802321612563,0.));
#32460=DIRECTION('center_axis',(0.94802321612563,-0.318201165439124,0.));
#32461=DIRECTION('ref_axis',(-0.318201165439124,-0.94802321612563,0.));
#32462=DIRECTION('',(0.,0.,-1.));
#32463=DIRECTION('',(-0.318201165439124,-0.94802321612563,0.));
#32464=DIRECTION('center_axis',(0.,0.,-1.));
#32465=DIRECTION('ref_axis',(-1.,0.,0.));
#32466=DIRECTION('center_axis',(0.,0.,-1.));
#32467=DIRECTION('ref_axis',(1.,0.,0.));
#32468=DIRECTION('center_axis',(0.198441315278718,0.980112771261783,0.));
#32469=DIRECTION('ref_axis',(0.980112771261783,-0.198441315278718,0.));
#32470=DIRECTION('',(0.,0.,1.));
#32471=DIRECTION('',(0.980112771261783,-0.198441315278718,0.));
#32472=DIRECTION('',(0.,0.,-1.));
#32473=DIRECTION('',(0.980112771261783,-0.198441315278718,0.));
#32474=DIRECTION('center_axis',(0.,0.,1.));
#32475=DIRECTION('ref_axis',(1.,0.,0.));
#32476=DIRECTION('center_axis',(0.,0.,1.));
#32477=DIRECTION('ref_axis',(1.,0.,0.));
#32478=DIRECTION('',(-0.623254323343971,-0.782019212317094,0.));
#32479=DIRECTION('center_axis',(0.782019212317094,-0.623254323343971,0.));
#32480=DIRECTION('ref_axis',(-0.623254323343971,-0.782019212317094,0.));
#32481=DIRECTION('',(0.,0.,-1.));
#32482=DIRECTION('',(-0.623254323343971,-0.782019212317094,0.));
#32483=DIRECTION('center_axis',(0.,0.,-1.));
#32484=DIRECTION('ref_axis',(-1.,0.,0.));
#32485=DIRECTION('center_axis',(0.,0.,-1.));
#32486=DIRECTION('ref_axis',(1.,0.,0.));
#32487=DIRECTION('center_axis',(0.521692150128735,0.853133811599363,0.));
#32488=DIRECTION('ref_axis',(0.853133811599363,-0.521692150128735,0.));
#32489=DIRECTION('',(0.,0.,1.));
#32490=DIRECTION('',(0.853133811599363,-0.521692150128735,0.));
#32491=DIRECTION('',(0.,0.,-1.));
#32492=DIRECTION('',(0.853133811599363,-0.521692150128735,0.));
#32493=DIRECTION('center_axis',(0.,0.,1.));
#32494=DIRECTION('ref_axis',(1.,0.,0.));
#32495=DIRECTION('center_axis',(0.,0.,1.));
#32496=DIRECTION('ref_axis',(1.,0.,0.));
#32497=DIRECTION('',(-0.853133811599363,-0.521692150128735,0.));
#32498=DIRECTION('center_axis',(0.,0.,1.));
#32499=DIRECTION('ref_axis',(1.,0.,0.));
#32500=DIRECTION('center_axis',(0.521692150128735,-0.853133811599363,0.));
#32501=DIRECTION('ref_axis',(-0.853133811599363,-0.521692150128735,0.));
#32502=DIRECTION('',(0.,0.,-1.));
#32503=DIRECTION('',(-0.853133811599363,-0.521692150128735,0.));
#32504=DIRECTION('center_axis',(0.,0.,-1.));
#32505=DIRECTION('ref_axis',(-1.,0.,0.));
#32506=DIRECTION('center_axis',(0.,0.,-1.));
#32507=DIRECTION('ref_axis',(1.,0.,0.));
#32508=DIRECTION('center_axis',(0.,0.,-1.));
#32509=DIRECTION('ref_axis',(1.,0.,0.));
#32510=DIRECTION('center_axis',(0.661911605822661,0.749581900846909,0.));
#32511=DIRECTION('ref_axis',(0.749581900846909,-0.661911605822661,0.));
#32512=DIRECTION('',(0.,0.,1.));
#32513=DIRECTION('',(0.749581900846909,-0.661911605822661,0.));
#32514=DIRECTION('',(0.,0.,-1.));
#32515=DIRECTION('',(0.749581900846909,-0.661911605822661,0.));
#32516=DIRECTION('center_axis',(0.,0.,1.));
#32517=DIRECTION('ref_axis',(1.,0.,0.));
#32518=DIRECTION('center_axis',(0.,0.,1.));
#32519=DIRECTION('ref_axis',(1.,0.,0.));
#32520=DIRECTION('',(-0.930763683192906,-0.365621342442116,0.));
#32521=DIRECTION('center_axis',(0.365621342442116,-0.930763683192906,0.));
#32522=DIRECTION('ref_axis',(-0.930763683192906,-0.365621342442116,0.));
#32523=DIRECTION('',(0.,0.,-1.));
#32524=DIRECTION('',(-0.930763683192906,-0.365621342442116,0.));
#32525=DIRECTION('center_axis',(0.,0.,-1.));
#32526=DIRECTION('ref_axis',(-1.,0.,0.));
#32527=DIRECTION('center_axis',(0.,0.,-1.));
#32528=DIRECTION('ref_axis',(1.,0.,0.));
#32529=DIRECTION('center_axis',(0.878365560766093,0.477989478608124,0.));
#32530=DIRECTION('ref_axis',(0.477989478608124,-0.878365560766093,0.));
#32531=DIRECTION('',(0.,0.,1.));
#32532=DIRECTION('',(0.477989478608124,-0.878365560766093,0.));
#32533=DIRECTION('',(0.,0.,-1.));
#32534=DIRECTION('',(0.477989478608124,-0.878365560766093,0.));
#32535=DIRECTION('center_axis',(0.,0.,1.));
#32536=DIRECTION('ref_axis',(1.,0.,0.));
#32537=DIRECTION('center_axis',(0.,0.,1.));
#32538=DIRECTION('ref_axis',(1.,0.,0.));
#32539=DIRECTION('',(-0.999681628736863,-0.0252317491667277,0.));
#32540=DIRECTION('center_axis',(0.0252317491667277,-0.999681628736863,0.));
#32541=DIRECTION('ref_axis',(-0.999681628736863,-0.0252317491667277,0.));
#32542=DIRECTION('',(0.,0.,-1.));
#32543=DIRECTION('',(-0.999681628736863,-0.0252317491667277,0.));
#32544=DIRECTION('center_axis',(0.,0.,-1.));
#32545=DIRECTION('ref_axis',(-1.,0.,0.));
#32546=DIRECTION('center_axis',(0.,0.,-1.));
#32547=DIRECTION('ref_axis',(1.,0.,0.));
#32548=DIRECTION('center_axis',(0.988875665786086,0.148744470875811,0.));
#32549=DIRECTION('ref_axis',(0.148744470875811,-0.988875665786086,0.));
#32550=DIRECTION('',(0.,0.,1.));
#32551=DIRECTION('',(0.148744470875811,-0.988875665786086,0.));
#32552=DIRECTION('',(0.,0.,-1.));
#32553=DIRECTION('',(0.148744470875811,-0.988875665786086,0.));
#32554=DIRECTION('center_axis',(0.,0.,1.));
#32555=DIRECTION('ref_axis',(1.,0.,0.));
#32556=DIRECTION('center_axis',(0.,0.,1.));
#32557=DIRECTION('ref_axis',(1.,0.,0.));
#32558=DIRECTION('',(-0.94802321612563,0.318201165439124,0.));
#32559=DIRECTION('center_axis',(-0.318201165439124,-0.94802321612563,0.));
#32560=DIRECTION('ref_axis',(-0.94802321612563,0.318201165439124,0.));
#32561=DIRECTION('',(0.,0.,-1.));
#32562=DIRECTION('',(-0.94802321612563,0.318201165439124,0.));
#32563=DIRECTION('center_axis',(0.,0.,-1.));
#32564=DIRECTION('ref_axis',(-1.,0.,0.));
#32565=DIRECTION('center_axis',(0.,0.,-1.));
#32566=DIRECTION('ref_axis',(1.,0.,0.));
#32567=DIRECTION('center_axis',(0.980112771261783,-0.19844131527872,0.));
#32568=DIRECTION('ref_axis',(-0.19844131527872,-0.980112771261783,0.));
#32569=DIRECTION('',(0.,0.,1.));
#32570=DIRECTION('',(-0.19844131527872,-0.980112771261783,0.));
#32571=DIRECTION('',(0.,0.,-1.));
#32572=DIRECTION('',(-0.19844131527872,-0.980112771261783,0.));
#32573=DIRECTION('center_axis',(0.,0.,1.));
#32574=DIRECTION('ref_axis',(1.,0.,0.));
#32575=DIRECTION('center_axis',(0.,0.,1.));
#32576=DIRECTION('ref_axis',(1.,0.,0.));
#32577=DIRECTION('',(-0.782019212317096,0.623254323343969,0.));
#32578=DIRECTION('center_axis',(-0.623254323343969,-0.782019212317096,0.));
#32579=DIRECTION('ref_axis',(-0.782019212317096,0.623254323343969,0.));
#32580=DIRECTION('',(0.,0.,-1.));
#32581=DIRECTION('',(-0.782019212317096,0.623254323343969,0.));
#32582=DIRECTION('center_axis',(0.,0.,-1.));
#32583=DIRECTION('ref_axis',(-1.,0.,0.));
#32584=DIRECTION('center_axis',(0.,0.,-1.));
#32585=DIRECTION('ref_axis',(1.,0.,0.));
#32586=DIRECTION('center_axis',(0.853133811599362,-0.521692150128737,0.));
#32587=DIRECTION('ref_axis',(-0.521692150128737,-0.853133811599362,0.));
#32588=DIRECTION('',(0.,0.,1.));
#32589=DIRECTION('',(-0.521692150128737,-0.853133811599362,0.));
#32590=DIRECTION('',(0.,0.,-1.));
#32591=DIRECTION('',(-0.521692150128737,-0.853133811599362,0.));
#32592=DIRECTION('center_axis',(0.,0.,1.));
#32593=DIRECTION('ref_axis',(1.,0.,0.));
#32594=DIRECTION('center_axis',(0.,0.,1.));
#32595=DIRECTION('ref_axis',(1.,0.,0.));
#32596=DIRECTION('',(-0.521692150128737,0.853133811599362,0.));
#32597=DIRECTION('center_axis',(-0.853133811599362,-0.521692150128737,0.));
#32598=DIRECTION('ref_axis',(-0.521692150128737,0.853133811599362,0.));
#32599=DIRECTION('',(0.,0.,-1.));
#32600=DIRECTION('',(-0.521692150128737,0.853133811599362,0.));
#32601=DIRECTION('center_axis',(0.,0.,-1.));
#32602=DIRECTION('ref_axis',(-1.,0.,0.));
#32603=DIRECTION('center_axis',(0.,0.,-1.));
#32604=DIRECTION('ref_axis',(1.,0.,0.));
#32605=DIRECTION('center_axis',(0.62325432334397,-0.782019212317095,0.));
#32606=DIRECTION('ref_axis',(-0.782019212317095,-0.62325432334397,0.));
#32607=DIRECTION('',(0.,0.,1.));
#32608=DIRECTION('',(-0.782019212317095,-0.62325432334397,0.));
#32609=DIRECTION('',(0.,0.,-1.));
#32610=DIRECTION('',(-0.782019212317095,-0.62325432334397,0.));
#32611=DIRECTION('center_axis',(0.,0.,1.));
#32612=DIRECTION('ref_axis',(1.,0.,0.));
#32613=DIRECTION('center_axis',(0.,0.,1.));
#32614=DIRECTION('ref_axis',(1.,0.,0.));
#32615=DIRECTION('',(-0.19844131527872,0.980112771261783,0.));
#32616=DIRECTION('center_axis',(-0.980112771261783,-0.19844131527872,0.));
#32617=DIRECTION('ref_axis',(-0.19844131527872,0.980112771261783,0.));
#32618=DIRECTION('',(0.,0.,-1.));
#32619=DIRECTION('',(-0.19844131527872,0.980112771261783,0.));
#32620=DIRECTION('center_axis',(0.,0.,-1.));
#32621=DIRECTION('ref_axis',(-1.,0.,0.));
#32622=DIRECTION('center_axis',(0.,0.,-1.));
#32623=DIRECTION('ref_axis',(1.,0.,0.));
#32624=DIRECTION('center_axis',(0.318201165439123,-0.948023216125631,0.));
#32625=DIRECTION('ref_axis',(-0.948023216125631,-0.318201165439123,0.));
#32626=DIRECTION('',(0.,0.,1.));
#32627=DIRECTION('',(-0.948023216125631,-0.318201165439123,0.));
#32628=DIRECTION('',(0.,0.,-1.));
#32629=DIRECTION('',(-0.948023216125631,-0.318201165439123,0.));
#32630=DIRECTION('center_axis',(0.,0.,1.));
#32631=DIRECTION('ref_axis',(1.,0.,0.));
#32632=DIRECTION('center_axis',(0.,0.,1.));
#32633=DIRECTION('ref_axis',(1.,0.,0.));
#32634=DIRECTION('',(0.148744470875811,0.988875665786086,0.));
#32635=DIRECTION('center_axis',(-0.988875665786086,0.148744470875811,0.));
#32636=DIRECTION('ref_axis',(0.148744470875811,0.988875665786086,0.));
#32637=DIRECTION('',(0.,0.,-1.));
#32638=DIRECTION('',(0.148744470875811,0.988875665786086,0.));
#32639=DIRECTION('center_axis',(0.,0.,-1.));
#32640=DIRECTION('ref_axis',(-1.,0.,0.));
#32641=DIRECTION('center_axis',(0.,0.,-1.));
#32642=DIRECTION('ref_axis',(1.,0.,0.));
#32643=DIRECTION('center_axis',(-0.0252317491667293,-0.999681628736863,
0.));
#32644=DIRECTION('ref_axis',(-0.999681628736863,0.0252317491667293,0.));
#32645=DIRECTION('',(0.,0.,1.));
#32646=DIRECTION('',(-0.999681628736863,0.0252317491667293,0.));
#32647=DIRECTION('',(0.,0.,-1.));
#32648=DIRECTION('',(-0.999681628736863,0.0252317491667293,0.));
#32649=DIRECTION('center_axis',(0.,0.,1.));
#32650=DIRECTION('ref_axis',(1.,0.,0.));
#32651=DIRECTION('center_axis',(0.,0.,1.));
#32652=DIRECTION('ref_axis',(1.,0.,0.));
#32653=DIRECTION('',(0.477989478608125,0.878365560766093,0.));
#32654=DIRECTION('center_axis',(-0.878365560766093,0.477989478608125,0.));
#32655=DIRECTION('ref_axis',(0.477989478608125,0.878365560766093,0.));
#32656=DIRECTION('',(0.,0.,-1.));
#32657=DIRECTION('',(0.477989478608125,0.878365560766093,0.));
#32658=DIRECTION('center_axis',(0.,0.,-1.));
#32659=DIRECTION('ref_axis',(-1.,0.,0.));
#32660=DIRECTION('center_axis',(0.,0.,-1.));
#32661=DIRECTION('ref_axis',(1.,0.,0.));
#32662=DIRECTION('center_axis',(-0.365621342442117,-0.930763683192906,0.));
#32663=DIRECTION('ref_axis',(-0.930763683192906,0.365621342442117,0.));
#32664=DIRECTION('',(0.,0.,1.));
#32665=DIRECTION('',(-0.930763683192906,0.365621342442117,0.));
#32666=DIRECTION('',(0.,0.,-1.));
#32667=DIRECTION('',(-0.930763683192906,0.365621342442117,0.));
#32668=DIRECTION('center_axis',(0.,0.,1.));
#32669=DIRECTION('ref_axis',(1.,0.,0.));
#32670=DIRECTION('center_axis',(0.,0.,1.));
#32671=DIRECTION('ref_axis',(1.,0.,0.));
#32672=DIRECTION('',(0.749581900846911,0.661911605822659,0.));
#32673=DIRECTION('center_axis',(-0.661911605822659,0.749581900846911,0.));
#32674=DIRECTION('ref_axis',(0.749581900846911,0.661911605822659,0.));
#32675=DIRECTION('',(0.,0.,-1.));
#32676=DIRECTION('',(0.749581900846911,0.661911605822659,0.));
#32677=DIRECTION('center_axis',(0.,0.,-1.));
#32678=DIRECTION('ref_axis',(-1.,0.,0.));
#32679=DIRECTION('center_axis',(0.,0.,-1.));
#32680=DIRECTION('ref_axis',(1.,0.,0.));
#32681=DIRECTION('center_axis',(-0.198441315278718,-0.980112771261783,0.));
#32682=DIRECTION('ref_axis',(-0.980112771261783,0.198441315278718,0.));
#32683=DIRECTION('',(0.,0.,1.));
#32684=DIRECTION('',(-0.980112771261783,0.198441315278718,0.));
#32685=DIRECTION('',(0.,0.,-1.));
#32686=DIRECTION('',(-0.980112771261783,0.198441315278718,0.));
#32687=DIRECTION('center_axis',(0.,0.,1.));
#32688=DIRECTION('ref_axis',(1.,0.,0.));
#32689=DIRECTION('center_axis',(0.,0.,1.));
#32690=DIRECTION('ref_axis',(1.,0.,0.));
#32691=DIRECTION('',(0.623254323343969,0.782019212317096,0.));
#32692=DIRECTION('center_axis',(-0.782019212317096,0.623254323343969,0.));
#32693=DIRECTION('ref_axis',(0.623254323343969,0.782019212317096,0.));
#32694=DIRECTION('',(0.,0.,-1.));
#32695=DIRECTION('',(0.623254323343969,0.782019212317096,0.));
#32696=DIRECTION('center_axis',(0.,0.,-1.));
#32697=DIRECTION('ref_axis',(-1.,0.,0.));
#32698=DIRECTION('center_axis',(0.,0.,-1.));
#32699=DIRECTION('ref_axis',(1.,0.,0.));
#32700=DIRECTION('center_axis',(0.148744470875811,-0.988875665786086,0.));
#32701=DIRECTION('ref_axis',(-0.988875665786086,-0.148744470875811,0.));
#32702=DIRECTION('',(0.,0.,1.));
#32703=DIRECTION('',(-0.988875665786086,-0.148744470875811,0.));
#32704=DIRECTION('',(0.,0.,-1.));
#32705=DIRECTION('',(-0.988875665786086,-0.148744470875811,0.));
#32706=DIRECTION('center_axis',(0.,0.,1.));
#32707=DIRECTION('ref_axis',(1.,0.,0.));
#32708=DIRECTION('center_axis',(0.,0.,1.));
#32709=DIRECTION('ref_axis',(1.,0.,0.));
#32710=DIRECTION('',(0.318201165439122,0.948023216125631,0.));
#32711=DIRECTION('center_axis',(-0.948023216125631,0.318201165439122,0.));
#32712=DIRECTION('ref_axis',(0.318201165439122,0.948023216125631,0.));
#32713=DIRECTION('',(0.,0.,-1.));
#32714=DIRECTION('',(0.318201165439122,0.948023216125631,0.));
#32715=DIRECTION('center_axis',(0.,0.,-1.));
#32716=DIRECTION('ref_axis',(-1.,0.,0.));
#32717=DIRECTION('center_axis',(0.,0.,-1.));
#32718=DIRECTION('ref_axis',(1.,0.,0.));
#32719=DIRECTION('center_axis',(0.477989478608127,-0.878365560766092,0.));
#32720=DIRECTION('ref_axis',(-0.878365560766092,-0.477989478608127,0.));
#32721=DIRECTION('',(0.,0.,1.));
#32722=DIRECTION('',(-0.878365560766092,-0.477989478608127,0.));
#32723=DIRECTION('',(0.,0.,-1.));
#32724=DIRECTION('',(-0.878365560766092,-0.477989478608127,0.));
#32725=DIRECTION('center_axis',(0.,0.,1.));
#32726=DIRECTION('ref_axis',(1.,0.,0.));
#32727=DIRECTION('center_axis',(0.,0.,1.));
#32728=DIRECTION('ref_axis',(1.,0.,0.));
#32729=DIRECTION('',(-0.0252317491667292,0.999681628736863,0.));
#32730=DIRECTION('center_axis',(-0.999681628736863,-0.0252317491667292,
0.));
#32731=DIRECTION('ref_axis',(-0.0252317491667292,0.999681628736863,0.));
#32732=DIRECTION('',(0.,0.,-1.));
#32733=DIRECTION('',(-0.0252317491667292,0.999681628736863,0.));
#32734=DIRECTION('center_axis',(0.,0.,-1.));
#32735=DIRECTION('ref_axis',(-1.,0.,0.));
#32736=DIRECTION('center_axis',(0.,0.,-1.));
#32737=DIRECTION('ref_axis',(1.,0.,0.));
#32738=DIRECTION('center_axis',(0.749581900846912,-0.661911605822658,0.));
#32739=DIRECTION('ref_axis',(-0.661911605822658,-0.749581900846912,0.));
#32740=DIRECTION('',(0.,0.,1.));
#32741=DIRECTION('',(-0.661911605822658,-0.749581900846912,0.));
#32742=DIRECTION('',(0.,0.,-1.));
#32743=DIRECTION('',(-0.661911605822658,-0.749581900846912,0.));
#32744=DIRECTION('center_axis',(0.,0.,1.));
#32745=DIRECTION('ref_axis',(1.,0.,0.));
#32746=DIRECTION('center_axis',(0.,0.,1.));
#32747=DIRECTION('ref_axis',(1.,0.,0.));
#32748=DIRECTION('',(-0.365621342442117,0.930763683192906,0.));
#32749=DIRECTION('center_axis',(-0.930763683192906,-0.365621342442117,0.));
#32750=DIRECTION('ref_axis',(-0.365621342442117,0.930763683192906,0.));
#32751=DIRECTION('',(0.,0.,-1.));
#32752=DIRECTION('',(-0.365621342442117,0.930763683192906,0.));
#32753=DIRECTION('center_axis',(0.,0.,-1.));
#32754=DIRECTION('ref_axis',(-1.,0.,0.));
#32755=DIRECTION('center_axis',(0.,0.,-1.));
#32756=DIRECTION('ref_axis',(1.,0.,0.));
#32757=DIRECTION('center_axis',(0.930763683192906,-0.365621342442117,0.));
#32758=DIRECTION('ref_axis',(-0.365621342442117,-0.930763683192906,0.));
#32759=DIRECTION('',(0.,0.,1.));
#32760=DIRECTION('',(-0.365621342442117,-0.930763683192906,0.));
#32761=DIRECTION('',(0.,0.,-1.));
#32762=DIRECTION('',(-0.365621342442117,-0.930763683192906,0.));
#32763=DIRECTION('center_axis',(0.,0.,1.));
#32764=DIRECTION('ref_axis',(1.,0.,0.));
#32765=DIRECTION('center_axis',(0.,0.,1.));
#32766=DIRECTION('ref_axis',(1.,0.,0.));
#32767=DIRECTION('',(-0.66191160582266,0.749581900846911,0.));
#32768=DIRECTION('center_axis',(-0.749581900846911,-0.66191160582266,0.));
#32769=DIRECTION('ref_axis',(-0.66191160582266,0.749581900846911,0.));
#32770=DIRECTION('',(0.,0.,-1.));
#32771=DIRECTION('',(-0.66191160582266,0.749581900846911,0.));
#32772=DIRECTION('center_axis',(0.,0.,-1.));
#32773=DIRECTION('ref_axis',(-1.,0.,0.));
#32774=DIRECTION('center_axis',(0.,0.,-1.));
#32775=DIRECTION('ref_axis',(1.,0.,0.));
#32776=DIRECTION('center_axis',(0.999681628736863,-0.0252317491667285,0.));
#32777=DIRECTION('ref_axis',(-0.0252317491667285,-0.999681628736863,0.));
#32778=DIRECTION('',(0.,0.,1.));
#32779=DIRECTION('',(-0.0252317491667285,-0.999681628736863,0.));
#32780=DIRECTION('',(0.,0.,-1.));
#32781=DIRECTION('',(-0.0252317491667285,-0.999681628736863,0.));
#32782=DIRECTION('center_axis',(0.,0.,1.));
#32783=DIRECTION('ref_axis',(1.,0.,0.));
#32784=DIRECTION('center_axis',(0.,0.,1.));
#32785=DIRECTION('ref_axis',(1.,0.,0.));
#32786=DIRECTION('',(-0.878365560766093,0.477989478608125,0.));
#32787=DIRECTION('center_axis',(-0.477989478608125,-0.878365560766093,0.));
#32788=DIRECTION('ref_axis',(-0.878365560766093,0.477989478608125,0.));
#32789=DIRECTION('',(0.,0.,-1.));
#32790=DIRECTION('',(-0.878365560766093,0.477989478608125,0.));
#32791=DIRECTION('center_axis',(0.,0.,-1.));
#32792=DIRECTION('ref_axis',(-1.,0.,0.));
#32793=DIRECTION('center_axis',(0.,0.,-1.));
#32794=DIRECTION('ref_axis',(1.,0.,0.));
#32795=DIRECTION('center_axis',(0.94802321612563,0.318201165439124,0.));
#32796=DIRECTION('ref_axis',(0.318201165439124,-0.94802321612563,0.));
#32797=DIRECTION('',(0.,0.,1.));
#32798=DIRECTION('',(0.318201165439124,-0.94802321612563,0.));
#32799=DIRECTION('',(0.,0.,-1.));
#32800=DIRECTION('',(0.318201165439124,-0.94802321612563,0.));
#32801=DIRECTION('center_axis',(0.,0.,1.));
#32802=DIRECTION('ref_axis',(1.,0.,0.));
#32803=DIRECTION('center_axis',(0.,0.,1.));
#32804=DIRECTION('ref_axis',(1.,0.,0.));
#32805=DIRECTION('',(-0.988875665786087,0.148744470875807,0.));
#32806=DIRECTION('center_axis',(-0.148744470875807,-0.988875665786087,0.));
#32807=DIRECTION('ref_axis',(-0.988875665786087,0.148744470875807,0.));
#32808=DIRECTION('',(0.,0.,-1.));
#32809=DIRECTION('',(-0.988875665786087,0.148744470875807,0.));
#32810=DIRECTION('center_axis',(0.,0.,-1.));
#32811=DIRECTION('ref_axis',(-1.,0.,0.));
#32812=DIRECTION('center_axis',(0.,0.,-1.));
#32813=DIRECTION('ref_axis',(1.,0.,0.));
#32814=DIRECTION('center_axis',(0.782019212317095,0.62325432334397,0.));
#32815=DIRECTION('ref_axis',(0.62325432334397,-0.782019212317095,0.));
#32816=DIRECTION('',(0.,0.,1.));
#32817=DIRECTION('',(0.62325432334397,-0.782019212317095,0.));
#32818=DIRECTION('',(0.,0.,-1.));
#32819=DIRECTION('',(0.62325432334397,-0.782019212317095,0.));
#32820=DIRECTION('center_axis',(0.,0.,1.));
#32821=DIRECTION('ref_axis',(1.,0.,0.));
#32822=DIRECTION('center_axis',(0.,0.,1.));
#32823=DIRECTION('ref_axis',(1.,0.,0.));
#32824=DIRECTION('',(-0.980112771261782,-0.198441315278722,0.));
#32825=DIRECTION('center_axis',(0.198441315278722,-0.980112771261782,0.));
#32826=DIRECTION('ref_axis',(-0.980112771261782,-0.198441315278722,0.));
#32827=DIRECTION('',(0.,0.,-1.));
#32828=DIRECTION('',(-0.980112771261782,-0.198441315278722,0.));
#32829=DIRECTION('center_axis',(0.,0.,-1.));
#32830=DIRECTION('ref_axis',(-1.,0.,0.));
#32831=DIRECTION('center_axis',(0.,0.,-1.));
#32832=DIRECTION('ref_axis',(1.,0.,0.));
#32833=DIRECTION('center_axis',(0.,0.,1.));
#32834=DIRECTION('ref_axis',(1.,0.,0.));
#32835=DIRECTION('center_axis',(0.,0.,1.));
#32836=DIRECTION('ref_axis',(1.,0.,0.));
#32837=DIRECTION('',(-0.853133811599362,0.521692150128736,0.));
#32838=DIRECTION('',(0.853133811599362,0.521692150128736,0.));
#32839=DIRECTION('center_axis',(-0.521692150128736,-0.853133811599362,0.));
#32840=DIRECTION('ref_axis',(-0.853133811599362,0.521692150128736,0.));
#32841=DIRECTION('',(0.,0.,1.));
#32842=DIRECTION('',(-0.853133811599362,0.521692150128736,0.));
#32843=DIRECTION('',(0.,0.,-1.));
#32844=DIRECTION('center_axis',(-0.521692150128736,0.853133811599362,0.));
#32845=DIRECTION('ref_axis',(0.853133811599362,0.521692150128736,0.));
#32846=DIRECTION('',(0.,0.,-1.));
#32847=DIRECTION('',(0.853133811599362,0.521692150128736,0.));
#32848=DIRECTION('center_axis',(0.,0.,-1.));
#32849=DIRECTION('ref_axis',(-1.,0.,0.));
#32850=DIRECTION('center_axis',(0.,0.,-1.));
#32851=DIRECTION('ref_axis',(1.,0.,0.));
#32852=DIRECTION('center_axis',(0.365621342442119,0.930763683192905,0.));
#32853=DIRECTION('ref_axis',(0.930763683192905,-0.365621342442119,0.));
#32854=DIRECTION('',(0.,0.,1.));
#32855=DIRECTION('',(0.930763683192905,-0.365621342442119,0.));
#32856=DIRECTION('',(0.,0.,-1.));
#32857=DIRECTION('',(0.930763683192905,-0.365621342442119,0.));
#32858=DIRECTION('center_axis',(0.,0.,1.));
#32859=DIRECTION('ref_axis',(1.,0.,0.));
#32860=DIRECTION('center_axis',(0.,0.,1.));
#32861=DIRECTION('ref_axis',(1.,0.,0.));
#32862=DIRECTION('',(-0.749581900846912,-0.661911605822659,0.));
#32863=DIRECTION('center_axis',(0.661911605822659,-0.749581900846912,0.));
#32864=DIRECTION('ref_axis',(-0.749581900846912,-0.661911605822659,0.));
#32865=DIRECTION('',(0.,0.,-1.));
#32866=DIRECTION('',(-0.749581900846912,-0.661911605822659,0.));
#32867=DIRECTION('center_axis',(0.,0.,-1.));
#32868=DIRECTION('ref_axis',(-1.,0.,0.));
#32869=DIRECTION('center_axis',(0.,0.,-1.));
#32870=DIRECTION('ref_axis',(1.,0.,0.));
#32871=DIRECTION('center_axis',(0.0252317491667325,0.999681628736863,0.));
#32872=DIRECTION('ref_axis',(0.999681628736863,-0.0252317491667325,0.));
#32873=DIRECTION('',(0.,0.,1.));
#32874=DIRECTION('',(0.999681628736863,-0.0252317491667325,0.));
#32875=DIRECTION('',(0.,0.,-1.));
#32876=DIRECTION('',(0.999681628736863,-0.0252317491667325,0.));
#32877=DIRECTION('center_axis',(0.,0.,1.));
#32878=DIRECTION('ref_axis',(1.,0.,0.));
#32879=DIRECTION('center_axis',(0.,0.,1.));
#32880=DIRECTION('ref_axis',(1.,0.,0.));
#32881=DIRECTION('',(-0.477989478608127,-0.878365560766092,0.));
#32882=DIRECTION('center_axis',(0.878365560766092,-0.477989478608127,0.));
#32883=DIRECTION('ref_axis',(-0.477989478608127,-0.878365560766092,0.));
#32884=DIRECTION('',(0.,0.,-1.));
#32885=DIRECTION('',(-0.477989478608127,-0.878365560766092,0.));
#32886=DIRECTION('center_axis',(0.,0.,-1.));
#32887=DIRECTION('ref_axis',(-1.,0.,0.));
#32888=DIRECTION('center_axis',(0.,0.,-1.));
#32889=DIRECTION('ref_axis',(1.,0.,0.));
#32890=DIRECTION('center_axis',(-0.318201165439124,0.94802321612563,0.));
#32891=DIRECTION('ref_axis',(0.94802321612563,0.318201165439124,0.));
#32892=DIRECTION('',(0.,0.,1.));
#32893=DIRECTION('',(0.94802321612563,0.318201165439124,0.));
#32894=DIRECTION('',(0.,0.,-1.));
#32895=DIRECTION('',(0.94802321612563,0.318201165439124,0.));
#32896=DIRECTION('center_axis',(0.,0.,1.));
#32897=DIRECTION('ref_axis',(1.,0.,0.));
#32898=DIRECTION('center_axis',(0.,0.,1.));
#32899=DIRECTION('ref_axis',(1.,0.,0.));
#32900=DIRECTION('',(-0.148744470875809,-0.988875665786086,0.));
#32901=DIRECTION('center_axis',(0.988875665786086,-0.148744470875809,0.));
#32902=DIRECTION('ref_axis',(-0.148744470875809,-0.988875665786086,0.));
#32903=DIRECTION('',(0.,0.,-1.));
#32904=DIRECTION('',(-0.148744470875809,-0.988875665786086,0.));
#32905=DIRECTION('center_axis',(0.,0.,-1.));
#32906=DIRECTION('ref_axis',(-1.,0.,0.));
#32907=DIRECTION('center_axis',(0.,0.,-1.));
#32908=DIRECTION('ref_axis',(1.,0.,0.));
#32909=DIRECTION('center_axis',(-0.623254323343969,0.782019212317096,0.));
#32910=DIRECTION('ref_axis',(0.782019212317096,0.623254323343969,0.));
#32911=DIRECTION('',(0.,0.,1.));
#32912=DIRECTION('',(0.782019212317096,0.623254323343969,0.));
#32913=DIRECTION('',(0.,0.,-1.));
#32914=DIRECTION('',(0.782019212317096,0.623254323343969,0.));
#32915=DIRECTION('center_axis',(0.,0.,1.));
#32916=DIRECTION('ref_axis',(1.,0.,0.));
#32917=DIRECTION('center_axis',(0.,0.,1.));
#32918=DIRECTION('ref_axis',(1.,0.,0.));
#32919=DIRECTION('',(0.198441315278714,-0.980112771261784,0.));
#32920=DIRECTION('center_axis',(0.980112771261784,0.198441315278714,0.));
#32921=DIRECTION('ref_axis',(0.198441315278714,-0.980112771261784,0.));
#32922=DIRECTION('',(0.,0.,-1.));
#32923=DIRECTION('',(0.198441315278714,-0.980112771261784,0.));
#32924=DIRECTION('center_axis',(0.,0.,-1.));
#32925=DIRECTION('ref_axis',(-1.,0.,0.));
#32926=DIRECTION('center_axis',(0.,0.,-1.));
#32927=DIRECTION('ref_axis',(1.,0.,0.));
#32928=DIRECTION('center_axis',(-0.853133811599361,0.521692150128738,0.));
#32929=DIRECTION('ref_axis',(0.521692150128738,0.853133811599361,0.));
#32930=DIRECTION('',(0.,0.,1.));
#32931=DIRECTION('',(0.521692150128738,0.853133811599361,0.));
#32932=DIRECTION('',(0.,0.,-1.));
#32933=DIRECTION('',(0.521692150128738,0.853133811599361,0.));
#32934=DIRECTION('center_axis',(0.,0.,1.));
#32935=DIRECTION('ref_axis',(1.,0.,0.));
#32936=DIRECTION('center_axis',(0.,0.,1.));
#32937=DIRECTION('ref_axis',(1.,0.,0.));
#32938=DIRECTION('',(0.521692150128738,-0.853133811599361,0.));
#32939=DIRECTION('center_axis',(0.853133811599361,0.521692150128738,0.));
#32940=DIRECTION('ref_axis',(0.521692150128738,-0.853133811599361,0.));
#32941=DIRECTION('',(0.,0.,-1.));
#32942=DIRECTION('',(0.521692150128738,-0.853133811599361,0.));
#32943=DIRECTION('center_axis',(0.,0.,-1.));
#32944=DIRECTION('ref_axis',(-1.,0.,0.));
#32945=DIRECTION('center_axis',(0.,0.,-1.));
#32946=DIRECTION('ref_axis',(1.,0.,0.));
#32947=DIRECTION('center_axis',(-0.980112771261782,0.198441315278721,0.));
#32948=DIRECTION('ref_axis',(0.198441315278721,0.980112771261782,0.));
#32949=DIRECTION('',(0.,0.,1.));
#32950=DIRECTION('',(0.198441315278721,0.980112771261782,0.));
#32951=DIRECTION('',(0.,0.,-1.));
#32952=DIRECTION('',(0.198441315278721,0.980112771261782,0.));
#32953=DIRECTION('center_axis',(0.,0.,1.));
#32954=DIRECTION('ref_axis',(1.,0.,0.));
#32955=DIRECTION('center_axis',(0.,0.,1.));
#32956=DIRECTION('ref_axis',(1.,0.,0.));
#32957=DIRECTION('',(0.782019212317093,-0.623254323343973,0.));
#32958=DIRECTION('center_axis',(0.623254323343973,0.782019212317093,0.));
#32959=DIRECTION('ref_axis',(0.782019212317093,-0.623254323343973,0.));
#32960=DIRECTION('',(0.,0.,-1.));
#32961=DIRECTION('',(0.782019212317093,-0.623254323343973,0.));
#32962=DIRECTION('center_axis',(0.,0.,-1.));
#32963=DIRECTION('ref_axis',(-1.,0.,0.));
#32964=DIRECTION('center_axis',(0.,0.,-1.));
#32965=DIRECTION('ref_axis',(1.,0.,0.));
#32966=DIRECTION('center_axis',(-0.988875665786087,-0.148744470875808,0.));
#32967=DIRECTION('ref_axis',(-0.148744470875808,0.988875665786087,0.));
#32968=DIRECTION('',(0.,0.,1.));
#32969=DIRECTION('',(-0.148744470875808,0.988875665786087,0.));
#32970=DIRECTION('',(0.,0.,-1.));
#32971=DIRECTION('',(-0.148744470875808,0.988875665786087,0.));
#32972=DIRECTION('center_axis',(0.,0.,1.));
#32973=DIRECTION('ref_axis',(1.,0.,0.));
#32974=DIRECTION('center_axis',(0.,0.,1.));
#32975=DIRECTION('ref_axis',(1.,0.,0.));
#32976=DIRECTION('',(0.948023216125631,-0.318201165439121,0.));
#32977=DIRECTION('center_axis',(0.318201165439121,0.948023216125631,0.));
#32978=DIRECTION('ref_axis',(0.948023216125631,-0.318201165439121,0.));
#32979=DIRECTION('',(0.,0.,-1.));
#32980=DIRECTION('',(0.948023216125631,-0.318201165439121,0.));
#32981=DIRECTION('center_axis',(0.,0.,-1.));
#32982=DIRECTION('ref_axis',(-1.,0.,0.));
#32983=DIRECTION('center_axis',(0.,0.,-1.));
#32984=DIRECTION('ref_axis',(1.,0.,0.));
#32985=DIRECTION('center_axis',(-0.87836556076609,-0.477989478608131,0.));
#32986=DIRECTION('ref_axis',(-0.477989478608131,0.87836556076609,0.));
#32987=DIRECTION('',(0.,0.,1.));
#32988=DIRECTION('',(-0.477989478608131,0.87836556076609,0.));
#32989=DIRECTION('',(0.,0.,-1.));
#32990=DIRECTION('',(-0.477989478608131,0.87836556076609,0.));
#32991=DIRECTION('center_axis',(0.,0.,1.));
#32992=DIRECTION('ref_axis',(1.,0.,0.));
#32993=DIRECTION('center_axis',(0.,0.,1.));
#32994=DIRECTION('ref_axis',(1.,0.,0.));
#32995=DIRECTION('',(0.999681628736863,0.0252317491667324,0.));
#32996=DIRECTION('center_axis',(-0.0252317491667324,0.999681628736863,0.));
#32997=DIRECTION('ref_axis',(0.999681628736863,0.0252317491667324,0.));
#32998=DIRECTION('',(0.,0.,-1.));
#32999=DIRECTION('',(0.999681628736863,0.0252317491667324,0.));
#33000=DIRECTION('center_axis',(0.,0.,-1.));
#33001=DIRECTION('ref_axis',(-1.,0.,0.));
#33002=DIRECTION('center_axis',(0.,0.,-1.));
#33003=DIRECTION('ref_axis',(1.,0.,0.));
#33004=DIRECTION('center_axis',(-0.661911605822662,-0.749581900846909,0.));
#33005=DIRECTION('ref_axis',(-0.749581900846909,0.661911605822662,0.));
#33006=DIRECTION('',(0.,0.,1.));
#33007=DIRECTION('',(-0.749581900846909,0.661911605822662,0.));
#33008=DIRECTION('',(0.,0.,-1.));
#33009=DIRECTION('',(-0.749581900846909,0.661911605822662,0.));
#33010=DIRECTION('center_axis',(0.,0.,1.));
#33011=DIRECTION('ref_axis',(1.,0.,0.));
#33012=DIRECTION('center_axis',(0.,0.,1.));
#33013=DIRECTION('ref_axis',(1.,0.,0.));
#33014=DIRECTION('',(0.930763683192905,0.365621342442119,0.));
#33015=DIRECTION('center_axis',(-0.365621342442119,0.930763683192905,0.));
#33016=DIRECTION('ref_axis',(0.930763683192905,0.365621342442119,0.));
#33017=DIRECTION('',(0.,0.,-1.));
#33018=DIRECTION('',(0.930763683192905,0.365621342442119,0.));
#33019=DIRECTION('center_axis',(0.,0.,-1.));
#33020=DIRECTION('ref_axis',(-1.,0.,0.));
#33021=DIRECTION('center_axis',(0.,0.,-1.));
#33022=DIRECTION('ref_axis',(1.,0.,0.));
#33023=DIRECTION('center_axis',(0.,0.,-1.));
#33024=DIRECTION('ref_axis',(-1.,0.,0.));
#33025=DIRECTION('center_axis',(0.,0.,1.));
#33026=DIRECTION('ref_axis',(1.,0.,0.));
#33027=DIRECTION('center_axis',(0.,0.,1.));
#33028=DIRECTION('ref_axis',(1.,0.,0.));
#33029=DIRECTION('',(0.707106781186548,8.65956056235493E-17,-0.707106781186547));
#33030=DIRECTION('center_axis',(0.,0.,1.));
#33031=DIRECTION('ref_axis',(1.,0.,0.));
#33032=DIRECTION('center_axis',(0.,0.,1.));
#33033=DIRECTION('ref_axis',(1.,0.,0.));
#33034=DIRECTION('',(0.707106781186548,8.65956056235494E-17,-0.707106781186547));
#33035=DIRECTION('center_axis',(0.,0.,1.));
#33036=DIRECTION('ref_axis',(1.,0.,0.));
#33037=DIRECTION('center_axis',(0.,0.,1.));
#33038=DIRECTION('ref_axis',(1.,0.,0.));
#33039=DIRECTION('center_axis',(0.,0.,1.));
#33040=DIRECTION('ref_axis',(1.,0.,0.));
#33041=DIRECTION('center_axis',(0.,0.,1.));
#33042=DIRECTION('ref_axis',(1.,0.,0.));
#33043=DIRECTION('center_axis',(0.,0.,1.));
#33044=DIRECTION('ref_axis',(1.,0.,0.));
#33045=DIRECTION('center_axis',(0.,0.,1.));
#33046=DIRECTION('ref_axis',(1.,0.,0.));
#33047=DIRECTION('center_axis',(0.,0.,1.));
#33048=DIRECTION('ref_axis',(1.,0.,0.));
#33049=DIRECTION('center_axis',(0.,0.,1.));
#33050=DIRECTION('ref_axis',(1.,0.,0.));
#33051=DIRECTION('center_axis',(0.,0.,1.));
#33052=DIRECTION('ref_axis',(1.,0.,0.));
#33053=DIRECTION('center_axis',(0.,0.,1.));
#33054=DIRECTION('ref_axis',(1.,0.,0.));
#33055=DIRECTION('center_axis',(0.,0.,1.));
#33056=DIRECTION('ref_axis',(1.,0.,0.));
#33057=DIRECTION('center_axis',(0.,0.,1.));
#33058=DIRECTION('ref_axis',(1.,0.,0.));
#33059=DIRECTION('center_axis',(0.,0.,1.));
#33060=DIRECTION('ref_axis',(1.,0.,0.));
#33061=DIRECTION('center_axis',(0.,0.,1.));
#33062=DIRECTION('ref_axis',(1.,0.,0.));
#33063=DIRECTION('center_axis',(0.,0.,1.));
#33064=DIRECTION('ref_axis',(1.,0.,0.));
#33065=DIRECTION('center_axis',(0.,0.,1.));
#33066=DIRECTION('ref_axis',(1.,0.,0.));
#33067=DIRECTION('center_axis',(0.,0.,1.));
#33068=DIRECTION('ref_axis',(1.,0.,0.));
#33069=DIRECTION('',(0.,0.,-1.));
#33070=DIRECTION('center_axis',(0.,0.,1.));
#33071=DIRECTION('ref_axis',(1.,0.,0.));
#33072=DIRECTION('center_axis',(0.,0.,1.));
#33073=DIRECTION('ref_axis',(1.,0.,0.));
#33074=DIRECTION('center_axis',(0.,0.,1.));
#33075=DIRECTION('ref_axis',(1.,0.,0.));
#33076=DIRECTION('center_axis',(0.,0.,1.));
#33077=DIRECTION('ref_axis',(1.,0.,0.));
#33078=DIRECTION('center_axis',(0.,0.,1.));
#33079=DIRECTION('ref_axis',(1.,0.,0.));
#33080=DIRECTION('center_axis',(0.,0.,1.));
#33081=DIRECTION('ref_axis',(1.,0.,0.));
#33082=DIRECTION('center_axis',(0.,0.,1.));
#33083=DIRECTION('ref_axis',(1.,0.,0.));
#33084=DIRECTION('center_axis',(0.,0.,1.));
#33085=DIRECTION('ref_axis',(1.,0.,0.));
#33086=DIRECTION('center_axis',(0.,0.,1.));
#33087=DIRECTION('ref_axis',(1.,0.,0.));
#33088=DIRECTION('center_axis',(0.,0.,1.));
#33089=DIRECTION('ref_axis',(1.,0.,0.));
#33090=DIRECTION('center_axis',(0.,0.,1.));
#33091=DIRECTION('ref_axis',(1.,0.,0.));
#33092=DIRECTION('center_axis',(0.,0.,1.));
#33093=DIRECTION('ref_axis',(1.,0.,0.));
#33094=DIRECTION('center_axis',(0.,0.,1.));
#33095=DIRECTION('ref_axis',(1.,0.,0.));
#33096=DIRECTION('center_axis',(0.,0.,1.));
#33097=DIRECTION('ref_axis',(1.,0.,0.));
#33098=DIRECTION('center_axis',(0.,0.,1.));
#33099=DIRECTION('ref_axis',(1.,0.,0.));
#33100=DIRECTION('center_axis',(0.,0.,1.));
#33101=DIRECTION('ref_axis',(1.,0.,0.));
#33102=DIRECTION('center_axis',(0.,0.,1.));
#33103=DIRECTION('ref_axis',(1.,0.,0.));
#33104=DIRECTION('center_axis',(0.,0.,1.));
#33105=DIRECTION('ref_axis',(1.,0.,0.));
#33106=DIRECTION('center_axis',(0.,0.,1.));
#33107=DIRECTION('ref_axis',(1.,0.,0.));
#33108=DIRECTION('center_axis',(0.,0.,1.));
#33109=DIRECTION('ref_axis',(1.,0.,0.));
#33110=DIRECTION('center_axis',(0.,0.,-1.));
#33111=DIRECTION('ref_axis',(1.,0.,0.));
#33112=DIRECTION('center_axis',(0.,0.,1.));
#33113=DIRECTION('ref_axis',(1.,0.,0.));
#33114=DIRECTION('',(-0.707106781186548,-8.65956056235493E-17,-0.707106781186547));
#33115=DIRECTION('center_axis',(0.,0.,1.));
#33116=DIRECTION('ref_axis',(1.,0.,0.));
#33117=DIRECTION('axis',(0.,0.,1.));
#33118=DIRECTION('refdir',(1.,0.,0.));
#33119=DIRECTION('center_axis',(0.,0.70710678118654,-0.707106781186555));
#33120=DIRECTION('ref_axis',(-1.,0.,0.));
#33121=DIRECTION('',(0.,0.707106781186555,0.70710678118654));
#33122=DIRECTION('',(1.,0.,0.));
#33123=DIRECTION('',(0.,-0.707106781186555,-0.70710678118654));
#33124=DIRECTION('',(-1.,0.,0.));
#33125=DIRECTION('center_axis',(0.,0.,1.));
#33126=DIRECTION('ref_axis',(0.,1.,0.));
#33127=DIRECTION('',(0.,-0.707106781186555,0.70710678118654));
#33128=DIRECTION('center_axis',(0.,0.,-1.));
#33129=DIRECTION('ref_axis',(0.,1.,0.));
#33130=DIRECTION('center_axis',(0.,0.,1.));
#33131=DIRECTION('ref_axis',(0.,1.,0.));
#33132=DIRECTION('center_axis',(0.,-0.70710678118654,-0.707106781186555));
#33133=DIRECTION('ref_axis',(-1.,0.,0.));
#33134=DIRECTION('',(0.,-0.707106781186555,0.70710678118654));
#33135=DIRECTION('',(-1.,0.,0.));
#33136=DIRECTION('',(1.,0.,0.));
#33137=DIRECTION('center_axis',(0.,0.,1.));
#33138=DIRECTION('ref_axis',(0.,-1.,0.));
#33139=DIRECTION('center_axis',(0.,0.,-1.));
#33140=DIRECTION('ref_axis',(0.,-1.,0.));
#33141=DIRECTION('center_axis',(0.,0.,1.));
#33142=DIRECTION('ref_axis',(0.,-1.,0.));
#33143=DIRECTION('center_axis',(0.,0.,1.));
#33144=DIRECTION('ref_axis',(0.,-1.,0.));
#33145=DIRECTION('',(0.,0.,1.));
#33146=DIRECTION('center_axis',(0.,0.,1.));
#33147=DIRECTION('ref_axis',(0.,-1.,0.));
#33148=DIRECTION('',(0.,0.,1.));
#33149=DIRECTION('center_axis',(0.,1.,0.));
#33150=DIRECTION('ref_axis',(-1.,0.,0.));
#33151=DIRECTION('',(0.,0.,1.));
#33152=DIRECTION('',(-1.,0.,0.));
#33153=DIRECTION('center_axis',(0.,0.,1.));
#33154=DIRECTION('ref_axis',(1.,0.,0.));
#33155=DIRECTION('center_axis',(0.,0.707106781186528,0.707106781186568));
#33156=DIRECTION('ref_axis',(1.,0.,0.));
#33157=DIRECTION('',(0.,-0.707106781186568,0.707106781186528));
#33158=DIRECTION('',(1.,0.,0.));
#33159=DIRECTION('',(0.,0.707106781186568,-0.707106781186528));
#33160=DIRECTION('center_axis',(0.,0.,-1.));
#33161=DIRECTION('ref_axis',(0.,1.,0.));
#33162=DIRECTION('',(0.,0.707106781186566,0.707106781186529));
#33163=DIRECTION('center_axis',(0.,0.,-1.));
#33164=DIRECTION('ref_axis',(0.,1.,0.));
#33165=DIRECTION('center_axis',(0.,0.,1.));
#33166=DIRECTION('ref_axis',(0.,1.,0.));
#33167=DIRECTION('center_axis',(0.,-0.707106781186528,0.707106781186568));
#33168=DIRECTION('ref_axis',(1.,0.,0.));
#33169=DIRECTION('',(0.,0.707106781186568,0.707106781186528));
#33170=DIRECTION('',(-1.,0.,0.));
#33171=DIRECTION('',(1.,0.,0.));
#33172=DIRECTION('center_axis',(0.,0.,-1.));
#33173=DIRECTION('ref_axis',(0.,-1.,0.));
#33174=DIRECTION('center_axis',(0.,0.,-1.));
#33175=DIRECTION('ref_axis',(0.,-1.,0.));
#33176=DIRECTION('center_axis',(0.,0.,1.));
#33177=DIRECTION('ref_axis',(0.,1.,0.));
#33178=DIRECTION('',(0.,0.,1.));
#33179=DIRECTION('center_axis',(0.,0.,1.));
#33180=DIRECTION('ref_axis',(1.,0.,0.));
#33181=DIRECTION('center_axis',(0.,-1.,0.));
#33182=DIRECTION('ref_axis',(1.,0.,0.));
#33183=DIRECTION('axis',(0.,0.,1.));
#33184=DIRECTION('refdir',(1.,0.,0.));
#33185=DIRECTION('center_axis',(0.,0.,1.));
#33186=DIRECTION('ref_axis',(1.,0.,0.));
#33187=DIRECTION('',(0.,0.,-1.));
#33188=DIRECTION('center_axis',(0.,0.,1.));
#33189=DIRECTION('ref_axis',(1.,0.,0.));
#33190=DIRECTION('center_axis',(0.,0.,1.));
#33191=DIRECTION('ref_axis',(1.,0.,0.));
#33192=DIRECTION('',(0.,0.,-1.));
#33193=DIRECTION('center_axis',(0.,0.,1.));
#33194=DIRECTION('ref_axis',(1.,0.,0.));
#33195=DIRECTION('',(0.,0.,-1.));
#33196=DIRECTION('center_axis',(0.,0.,1.));
#33197=DIRECTION('ref_axis',(1.,0.,0.));
#33198=DIRECTION('',(0.,0.,-1.));
#33199=DIRECTION('center_axis',(0.,0.,1.));
#33200=DIRECTION('ref_axis',(1.,0.,0.));
#33201=DIRECTION('',(0.,0.,-1.));
#33202=DIRECTION('center_axis',(0.,0.,1.));
#33203=DIRECTION('ref_axis',(1.,0.,0.));
#33204=DIRECTION('',(0.,0.,-1.));
#33205=DIRECTION('center_axis',(0.,0.,1.));
#33206=DIRECTION('ref_axis',(1.,0.,0.));
#33207=DIRECTION('',(0.,0.,-1.));
#33208=DIRECTION('center_axis',(0.,0.,1.));
#33209=DIRECTION('ref_axis',(1.,0.,0.));
#33210=DIRECTION('',(0.,0.,-1.));
#33211=DIRECTION('center_axis',(0.,0.,1.));
#33212=DIRECTION('ref_axis',(1.,0.,0.));
#33213=DIRECTION('',(0.,0.,-1.));
#33214=DIRECTION('center_axis',(0.,0.,1.));
#33215=DIRECTION('ref_axis',(1.,0.,0.));
#33216=DIRECTION('',(0.,0.,-1.));
#33217=DIRECTION('center_axis',(0.,0.,1.));
#33218=DIRECTION('ref_axis',(0.852304747849821,-0.523045520765308,0.));
#33219=DIRECTION('',(0.,0.,1.));
#33220=DIRECTION('center_axis',(0.,0.,1.));
#33221=DIRECTION('ref_axis',(1.,4.73084717204786E-14,0.));
#33222=DIRECTION('center_axis',(0.,0.,1.));
#33223=DIRECTION('ref_axis',(1.,4.73084717204786E-14,0.));
#33224=DIRECTION('',(0.,0.,1.));
#33225=DIRECTION('center_axis',(0.,0.,1.));
#33226=DIRECTION('ref_axis',(1.,4.73084717204786E-14,0.));
#33227=DIRECTION('',(0.,0.,1.));
#33228=DIRECTION('center_axis',(0.,0.,1.));
#33229=DIRECTION('ref_axis',(1.,4.73084717204786E-14,0.));
#33230=DIRECTION('',(0.,0.,1.));
#33231=DIRECTION('center_axis',(0.,0.,1.));
#33232=DIRECTION('ref_axis',(1.,4.73084717204786E-14,0.));
#33233=DIRECTION('',(0.,0.,1.));
#33234=DIRECTION('center_axis',(0.,0.,1.));
#33235=DIRECTION('ref_axis',(1.,4.73084717204786E-14,0.));
#33236=DIRECTION('',(0.,0.,1.));
#33237=DIRECTION('center_axis',(0.,0.,1.));
#33238=DIRECTION('ref_axis',(1.,4.73084717204786E-14,0.));
#33239=DIRECTION('',(0.,0.,1.));
#33240=DIRECTION('center_axis',(0.,0.,1.));
#33241=DIRECTION('ref_axis',(1.,4.73084717204786E-14,0.));
#33242=DIRECTION('',(0.,0.,1.));
#33243=DIRECTION('center_axis',(0.,0.,1.));
#33244=DIRECTION('ref_axis',(1.,4.73084717204786E-14,0.));
#33245=DIRECTION('',(0.,0.,1.));
#33246=DIRECTION('center_axis',(0.,-2.11251572852923E-15,-1.));
#33247=DIRECTION('ref_axis',(-4.14386955393131E-16,1.,-2.11251572852923E-15));
#33248=DIRECTION('center_axis',(0.,0.,1.));
#33249=DIRECTION('ref_axis',(1.,6.12323399573678E-17,0.));
#33250=DIRECTION('center_axis',(0.,0.,-1.));
#33251=DIRECTION('ref_axis',(1.,0.,0.));
#33252=DIRECTION('center_axis',(0.,0.,-1.));
#33253=DIRECTION('ref_axis',(1.83758917935762E-15,1.,0.));
#33254=DIRECTION('center_axis',(0.,0.,1.));
#33255=DIRECTION('ref_axis',(1.,0.,0.));
#33256=DIRECTION('center_axis',(0.,0.,1.));
#33257=DIRECTION('ref_axis',(1.,0.,0.));
#33258=DIRECTION('center_axis',(0.,0.,1.));
#33259=DIRECTION('ref_axis',(1.,0.,0.));
#33260=DIRECTION('center_axis',(0.,0.,1.));
#33261=DIRECTION('ref_axis',(1.,0.,0.));
#33262=DIRECTION('center_axis',(0.,0.,1.));
#33263=DIRECTION('ref_axis',(1.,0.,0.));
#33264=DIRECTION('center_axis',(0.,0.,-1.));
#33265=DIRECTION('ref_axis',(1.,4.73084717204786E-14,0.));
#33266=DIRECTION('center_axis',(0.,0.,1.));
#33267=DIRECTION('ref_axis',(0.889076734145909,0.457758190314979,0.));
#33268=DIRECTION('center_axis',(0.,0.99026806874157,-0.139173100960066));
#33269=DIRECTION('ref_axis',(0.,0.139173100960066,0.99026806874157));
#33270=DIRECTION('',(2.75812094787263E-18,-0.986882465954279,0.161440386496073));
#33271=DIRECTION('center_axis',(0.,0.99026806874157,-0.139173100960066));
#33272=DIRECTION('ref_axis',(1.,0.,0.));
#33273=DIRECTION('center_axis',(0.,0.99026806874157,-0.139173100960066));
#33274=DIRECTION('ref_axis',(1.,0.,0.));
#33275=DIRECTION('center_axis',(0.,0.99026806874157,-0.139173100960066));
#33276=DIRECTION('ref_axis',(1.,0.,0.));
#33277=DIRECTION('center_axis',(0.,0.,-1.));
#33278=DIRECTION('ref_axis',(0.,1.,0.));
#33279=DIRECTION('center_axis',(0.,0.99026806874157,-0.139173100960066));
#33280=DIRECTION('ref_axis',(1.,0.,0.));
#33281=DIRECTION('center_axis',(0.,0.,-1.));
#33282=DIRECTION('ref_axis',(0.,1.,0.));
#33283=DIRECTION('center_axis',(1.,0.,0.));
#33284=DIRECTION('ref_axis',(0.,-1.,0.));
#33285=DIRECTION('center_axis',(0.,0.,1.));
#33286=DIRECTION('ref_axis',(0.,1.,0.));
#33287=DIRECTION('center_axis',(0.,0.,1.));
#33288=DIRECTION('ref_axis',(0.,1.,0.));
#33289=DIRECTION('center_axis',(0.,0.99026806874157,-0.139173100960066));
#33290=DIRECTION('ref_axis',(0.,0.139173100960066,0.99026806874157));
#33291=DIRECTION('',(1.,0.,0.));
#33292=DIRECTION('center_axis',(0.,0.,1.));
#33293=DIRECTION('ref_axis',(1.,0.,0.));
#33294=DIRECTION('center_axis',(0.,0.,-1.));
#33295=DIRECTION('ref_axis',(-1.,0.,0.));
#33296=DIRECTION('center_axis',(0.,0.,1.));
#33297=DIRECTION('ref_axis',(1.,0.,0.));
#33298=DIRECTION('center_axis',(0.,0.,1.));
#33299=DIRECTION('ref_axis',(1.,0.,0.));
#33300=DIRECTION('',(0.707106781186573,8.65956056235524E-17,-0.707106781186522));
#33301=DIRECTION('center_axis',(0.,0.,1.));
#33302=DIRECTION('ref_axis',(-0.592677092377571,-0.805440167964616,0.));
#33303=DIRECTION('center_axis',(0.,0.,1.));
#33304=DIRECTION('ref_axis',(1.,0.,0.));
#33305=DIRECTION('center_axis',(0.,0.,-1.));
#33306=DIRECTION('ref_axis',(-1.,0.,0.));
#33307=DIRECTION('center_axis',(0.,0.,1.));
#33308=DIRECTION('ref_axis',(1.,0.,0.));
#33309=DIRECTION('center_axis',(0.,0.,1.));
#33310=DIRECTION('ref_axis',(1.,0.,0.));
#33311=DIRECTION('',(0.,0.,-1.));
#33312=DIRECTION('axis',(0.,0.,1.));
#33313=DIRECTION('refdir',(1.,0.,0.));
#33314=DIRECTION('center_axis',(1.,0.,0.));
#33315=DIRECTION('ref_axis',(0.,1.,0.));
#33316=DIRECTION('center_axis',(0.,0.,1.));
#33317=DIRECTION('ref_axis',(1.,0.,0.));
#33318=DIRECTION('center_axis',(0.,0.,1.));
#33319=DIRECTION('ref_axis',(1.,0.,0.));
#33320=DIRECTION('',(0.,0.,-1.));
#33321=DIRECTION('center_axis',(0.,0.,-1.));
#33322=DIRECTION('ref_axis',(1.,0.,0.));
#33323=DIRECTION('center_axis',(0.,0.,1.));
#33324=DIRECTION('ref_axis',(1.,0.,0.));
#33325=DIRECTION('',(-0.707106781186522,-8.65956056235463E-17,-0.707106781186573));
#33326=DIRECTION('center_axis',(0.,0.,1.));
#33327=DIRECTION('ref_axis',(1.,0.,0.));
#33328=DIRECTION('axis',(0.,0.,1.));
#33329=DIRECTION('refdir',(1.,0.,0.));
#33330=DIRECTION('center_axis',(0.,0.,1.));
#33331=DIRECTION('ref_axis',(1.,0.,0.));
#33332=DIRECTION('',(0.,0.,-1.));
#33333=DIRECTION('center_axis',(0.,0.,1.));
#33334=DIRECTION('ref_axis',(1.,0.,0.));
#33335=DIRECTION('center_axis',(0.,0.,1.));
#33336=DIRECTION('ref_axis',(1.,0.,0.));
#33337=DIRECTION('',(0.,0.,-1.));
#33338=DIRECTION('center_axis',(0.,0.,1.));
#33339=DIRECTION('ref_axis',(1.,0.,0.));
#33340=DIRECTION('',(0.,0.,-1.));
#33341=DIRECTION('center_axis',(0.,0.,1.));
#33342=DIRECTION('ref_axis',(1.,0.,0.));
#33343=DIRECTION('',(0.,0.,-1.));
#33344=DIRECTION('center_axis',(0.,0.,1.));
#33345=DIRECTION('ref_axis',(1.,0.,0.));
#33346=DIRECTION('',(0.,0.,-1.));
#33347=DIRECTION('center_axis',(0.,0.,1.));
#33348=DIRECTION('ref_axis',(1.,0.,0.));
#33349=DIRECTION('',(0.,0.,-1.));
#33350=DIRECTION('center_axis',(0.,0.,1.));
#33351=DIRECTION('ref_axis',(1.,0.,0.));
#33352=DIRECTION('',(0.,0.,-1.));
#33353=DIRECTION('center_axis',(0.,0.,1.));
#33354=DIRECTION('ref_axis',(1.,0.,0.));
#33355=DIRECTION('',(0.,0.,-1.));
#33356=DIRECTION('center_axis',(0.,0.,1.));
#33357=DIRECTION('ref_axis',(1.,0.,0.));
#33358=DIRECTION('',(0.,0.,-1.));
#33359=DIRECTION('center_axis',(0.,0.,1.));
#33360=DIRECTION('ref_axis',(1.,0.,0.));
#33361=DIRECTION('',(0.,0.,-1.));
#33362=DIRECTION('center_axis',(0.,0.,1.));
#33363=DIRECTION('ref_axis',(1.,0.,0.));
#33364=DIRECTION('',(0.,0.,-1.));
#33365=DIRECTION('center_axis',(0.,0.,1.));
#33366=DIRECTION('ref_axis',(1.,0.,0.));
#33367=DIRECTION('',(0.,0.,-1.));
#33368=DIRECTION('center_axis',(0.,0.,1.));
#33369=DIRECTION('ref_axis',(1.,0.,0.));
#33370=DIRECTION('',(0.,0.,-1.));
#33371=DIRECTION('center_axis',(0.,0.,1.));
#33372=DIRECTION('ref_axis',(1.,0.,0.));
#33373=DIRECTION('',(0.,0.,-1.));
#33374=DIRECTION('center_axis',(0.,0.,1.));
#33375=DIRECTION('ref_axis',(-0.530268055707691,-0.847830047294849,0.));
#33376=DIRECTION('',(0.,0.,1.));
#33377=DIRECTION('center_axis',(0.,0.,1.));
#33378=DIRECTION('ref_axis',(1.,9.13482547654578E-14,0.));
#33379=DIRECTION('center_axis',(0.,0.,1.));
#33380=DIRECTION('ref_axis',(1.,9.13482547654578E-14,0.));
#33381=DIRECTION('',(0.,0.,1.));
#33382=DIRECTION('center_axis',(0.,0.,1.));
#33383=DIRECTION('ref_axis',(1.,9.13482547654578E-14,0.));
#33384=DIRECTION('',(0.,0.,1.));
#33385=DIRECTION('center_axis',(0.,0.,1.));
#33386=DIRECTION('ref_axis',(1.,9.13482547654578E-14,0.));
#33387=DIRECTION('',(0.,0.,1.));
#33388=DIRECTION('center_axis',(0.,0.,1.));
#33389=DIRECTION('ref_axis',(1.,9.13482547654578E-14,0.));
#33390=DIRECTION('',(0.,0.,1.));
#33391=DIRECTION('center_axis',(0.,0.,1.));
#33392=DIRECTION('ref_axis',(1.,9.13482547654578E-14,0.));
#33393=DIRECTION('',(0.,0.,1.));
#33394=DIRECTION('center_axis',(0.,0.,1.));
#33395=DIRECTION('ref_axis',(1.,9.13482547654578E-14,0.));
#33396=DIRECTION('',(0.,0.,1.));
#33397=DIRECTION('center_axis',(0.,0.,1.));
#33398=DIRECTION('ref_axis',(1.,9.13482547654578E-14,0.));
#33399=DIRECTION('',(0.,0.,1.));
#33400=DIRECTION('center_axis',(0.,0.,1.));
#33401=DIRECTION('ref_axis',(1.,9.13482547654578E-14,0.));
#33402=DIRECTION('',(0.,0.,1.));
#33403=DIRECTION('center_axis',(0.,0.,1.));
#33404=DIRECTION('ref_axis',(1.,9.13482547654578E-14,0.));
#33405=DIRECTION('',(0.,0.,1.));
#33406=DIRECTION('center_axis',(0.,0.,1.));
#33407=DIRECTION('ref_axis',(1.,9.13482547654578E-14,0.));
#33408=DIRECTION('',(0.,0.,1.));
#33409=DIRECTION('center_axis',(0.,0.,1.));
#33410=DIRECTION('ref_axis',(1.,9.13482547654578E-14,0.));
#33411=DIRECTION('',(0.,0.,1.));
#33412=DIRECTION('center_axis',(0.,0.,1.));
#33413=DIRECTION('ref_axis',(1.,9.13482547654578E-14,0.));
#33414=DIRECTION('',(0.,0.,1.));
#33415=DIRECTION('center_axis',(0.,0.,1.));
#33416=DIRECTION('ref_axis',(1.,9.13482547654578E-14,0.));
#33417=DIRECTION('',(0.,0.,1.));
#33418=DIRECTION('center_axis',(0.,0.,1.));
#33419=DIRECTION('ref_axis',(1.,0.,0.));
#33420=DIRECTION('center_axis',(0.,0.,1.));
#33421=DIRECTION('ref_axis',(1.,0.,0.));
#33422=DIRECTION('center_axis',(0.,0.,1.));
#33423=DIRECTION('ref_axis',(1.,0.,0.));
#33424=DIRECTION('center_axis',(0.,0.,-1.));
#33425=DIRECTION('ref_axis',(1.,9.13482547654578E-14,0.));
#33426=DIRECTION('center_axis',(0.,0.,1.));
#33427=DIRECTION('ref_axis',(1.,9.13482547654578E-14,0.));
#33428=DIRECTION('center_axis',(0.,0.,1.));
#33429=DIRECTION('ref_axis',(1.,0.,0.));
#33430=DIRECTION('center_axis',(0.,0.,-1.));
#33431=DIRECTION('ref_axis',(1.,0.,0.));
#33432=DIRECTION('center_axis',(0.,0.,1.));
#33433=DIRECTION('ref_axis',(1.,0.,0.));
#33434=DIRECTION('center_axis',(-2.40370335797945E-16,-1.,0.));
#33435=DIRECTION('ref_axis',(1.,-2.40370335797945E-16,0.));
#33436=DIRECTION('',(1.,-2.40370335797945E-16,0.));
#33437=DIRECTION('',(0.,0.,1.));
#33438=DIRECTION('',(1.,-2.40370335797945E-16,0.));
#33439=DIRECTION('',(0.,0.,1.));
#33440=DIRECTION('center_axis',(-0.866025403784439,-0.5,0.));
#33441=DIRECTION('ref_axis',(0.5,-0.866025403784439,0.));
#33442=DIRECTION('',(0.5,-0.866025403784439,0.));
#33443=DIRECTION('',(0.,0.,1.));
#33444=DIRECTION('',(0.5,-0.866025403784439,0.));
#33445=DIRECTION('center_axis',(-0.866025403784439,0.5,0.));
#33446=DIRECTION('ref_axis',(-0.5,-0.866025403784439,0.));
#33447=DIRECTION('',(-0.5,-0.866025403784439,0.));
#33448=DIRECTION('',(0.,0.,1.));
#33449=DIRECTION('',(-0.5,-0.866025403784439,0.));
#33450=DIRECTION('center_axis',(1.20185167898973E-16,1.,0.));
#33451=DIRECTION('ref_axis',(-1.,1.20185167898973E-16,0.));
#33452=DIRECTION('',(-1.,1.20185167898973E-16,0.));
#33453=DIRECTION('',(0.,0.,1.));
#33454=DIRECTION('',(-1.,1.20185167898973E-16,0.));
#33455=DIRECTION('center_axis',(0.866025403784439,0.5,0.));
#33456=DIRECTION('ref_axis',(-0.5,0.866025403784439,0.));
#33457=DIRECTION('',(-0.5,0.866025403784439,0.));
#33458=DIRECTION('',(0.,0.,1.));
#33459=DIRECTION('',(-0.5,0.866025403784439,0.));
#33460=DIRECTION('center_axis',(0.866025403784439,-0.5,0.));
#33461=DIRECTION('ref_axis',(0.5,0.866025403784439,0.));
#33462=DIRECTION('',(0.5,0.866025403784439,0.));
#33463=DIRECTION('',(0.5,0.866025403784439,0.));
#33464=DIRECTION('center_axis',(0.,0.,1.));
#33465=DIRECTION('ref_axis',(1.,0.,0.));
#33466=DIRECTION('center_axis',(0.,0.,-1.));
#33467=DIRECTION('ref_axis',(-1.,0.,0.));
#33468=DIRECTION('center_axis',(0.,0.,1.));
#33469=DIRECTION('ref_axis',(1.,0.,0.));
#33470=DIRECTION('center_axis',(0.,0.,1.));
#33471=DIRECTION('ref_axis',(1.,0.,0.));
#33472=DIRECTION('',(0.707106781186548,8.65956056235494E-17,-0.707106781186547));
#33473=DIRECTION('center_axis',(0.,0.,1.));
#33474=DIRECTION('ref_axis',(1.,0.,0.));
#33475=DIRECTION('center_axis',(0.,0.,1.));
#33476=DIRECTION('ref_axis',(1.,0.,0.));
#33477=DIRECTION('center_axis',(0.,0.,1.));
#33478=DIRECTION('ref_axis',(1.,0.,0.));
#33479=DIRECTION('',(0.,0.,-1.));
#33480=DIRECTION('center_axis',(0.,0.,-1.));
#33481=DIRECTION('ref_axis',(1.,0.,0.));
#33482=DIRECTION('center_axis',(0.,0.,1.));
#33483=DIRECTION('ref_axis',(1.,0.,0.));
#33484=DIRECTION('',(-0.707106781186547,-8.65956056235493E-17,-0.707106781186548));
#33485=DIRECTION('center_axis',(0.,0.,1.));
#33486=DIRECTION('ref_axis',(1.,0.,0.));
#33487=DIRECTION('axis',(0.,0.,1.));
#33488=DIRECTION('refdir',(1.,0.,0.));
#33489=DIRECTION('center_axis',(-0.707106781186574,0.707106781186521,0.));
#33490=DIRECTION('ref_axis',(0.,0.,1.));
#33491=DIRECTION('',(0.577350269189601,0.577350269189643,-0.577350269189633));
#33492=DIRECTION('',(0.,0.,-1.));
#33493=DIRECTION('',(-0.577350269189601,-0.577350269189643,-0.577350269189633));
#33494=DIRECTION('',(-0.577350269189615,-0.577350269189658,0.577350269189605));
#33495=DIRECTION('',(0.,0.,1.));
#33496=DIRECTION('',(0.577350269189615,0.577350269189658,0.577350269189605));
#33497=DIRECTION('center_axis',(0.,1.,0.));
#33498=DIRECTION('ref_axis',(-1.,0.,0.));
#33499=DIRECTION('',(-1.,0.,0.));
#33500=DIRECTION('',(0.,0.,1.));
#33501=DIRECTION('',(1.,0.,0.));
#33502=DIRECTION('center_axis',(0.,0.707106781186541,0.707106781186554));
#33503=DIRECTION('ref_axis',(1.,0.,0.));
#33504=DIRECTION('',(-0.577350269189629,0.577350269189629,-0.577350269189619));
#33505=DIRECTION('',(1.,0.,0.));
#33506=DIRECTION('',(0.577350269189629,0.577350269189629,-0.577350269189619));
#33507=DIRECTION('',(0.577350269189601,-0.577350269189643,0.577350269189633));
#33508=DIRECTION('center_axis',(-0.707106781186541,0.,0.707106781186554));
#33509=DIRECTION('ref_axis',(0.707106781186554,0.,0.707106781186541));
#33510=DIRECTION('',(0.,-1.,0.));
#33511=DIRECTION('',(-0.577350269189615,0.577350269189658,-0.577350269189605));
#33512=DIRECTION('',(-0.577350269189629,-0.577350269189629,-0.577350269189619));
#33513=DIRECTION('',(0.,1.,0.));
#33514=DIRECTION('center_axis',(0.707106781186574,0.707106781186521,0.));
#33515=DIRECTION('ref_axis',(0.,0.,-1.));
#33516=DIRECTION('',(0.577350269189615,-0.577350269189658,-0.577350269189605));
#33517=DIRECTION('',(0.,0.,-1.));
#33518=DIRECTION('',(-0.577350269189615,0.577350269189658,-0.577350269189605));
#33519=DIRECTION('',(-0.577350269189601,0.577350269189643,0.577350269189633));
#33520=DIRECTION('center_axis',(0.707106781186541,0.,-0.707106781186554));
#33521=DIRECTION('ref_axis',(-0.707106781186554,0.,-0.707106781186541));
#33522=DIRECTION('',(0.,-1.,0.));
#33523=DIRECTION('',(0.577350269189615,0.577350269189658,0.577350269189605));
#33524=DIRECTION('',(0.577350269189629,-0.577350269189629,0.577350269189619));
#33525=DIRECTION('',(0.,1.,0.));
#33526=DIRECTION('',(0.577350269189629,0.577350269189629,0.577350269189619));
#33527=DIRECTION('center_axis',(1.,0.,0.));
#33528=DIRECTION('ref_axis',(0.,1.,0.));
#33529=DIRECTION('',(0.,1.,0.));
#33530=DIRECTION('',(0.,0.,1.));
#33531=DIRECTION('center_axis',(0.707106781186541,0.,0.707106781186554));
#33532=DIRECTION('ref_axis',(0.707106781186554,0.,-0.707106781186541));
#33533=DIRECTION('',(0.,-1.,0.));
#33534=DIRECTION('',(0.577350269189629,-0.577350269189629,-0.577350269189619));
#33535=DIRECTION('',(-0.577350269189615,-0.577350269189658,0.577350269189605));
#33536=DIRECTION('center_axis',(-0.707106781186574,-0.707106781186521,0.));
#33537=DIRECTION('ref_axis',(0.,0.,1.));
#33538=DIRECTION('',(0.,0.,-1.));
#33539=DIRECTION('',(0.577350269189615,-0.577350269189658,-0.577350269189605));
#33540=DIRECTION('',(0.577350269189601,-0.577350269189643,0.577350269189633));
#33541=DIRECTION('',(0.,0.,1.));
#33542=DIRECTION('',(-0.577350269189601,0.577350269189643,0.577350269189633));
#33543=DIRECTION('center_axis',(0.,-1.,0.));
#33544=DIRECTION('ref_axis',(1.,0.,0.));
#33545=DIRECTION('',(-1.,0.,0.));
#33546=DIRECTION('',(0.,0.,-1.));
#33547=DIRECTION('',(1.,0.,0.));
#33548=DIRECTION('center_axis',(0.,-0.707106781186541,-0.707106781186554));
#33549=DIRECTION('ref_axis',(-1.,0.,0.));
#33550=DIRECTION('',(-0.577350269189629,-0.577350269189629,0.577350269189619));
#33551=DIRECTION('',(1.,0.,0.));
#33552=DIRECTION('',(0.577350269189601,0.577350269189643,-0.577350269189633));
#33553=DIRECTION('center_axis',(-0.707106781186541,0.,-0.707106781186554));
#33554=DIRECTION('ref_axis',(-0.707106781186554,0.,0.707106781186541));
#33555=DIRECTION('',(0.577350269189629,-0.577350269189629,-0.577350269189619));
#33556=DIRECTION('',(0.,-1.,0.));
#33557=DIRECTION('',(0.,1.,0.));
#33558=DIRECTION('center_axis',(0.707106781186574,-0.707106781186521,0.));
#33559=DIRECTION('ref_axis',(0.,0.,-1.));
#33560=DIRECTION('',(-0.577350269189601,-0.577350269189643,-0.577350269189633));
#33561=DIRECTION('center_axis',(0.,0.707106781186541,-0.707106781186554));
#33562=DIRECTION('ref_axis',(-1.,0.,0.));
#33563=DIRECTION('',(-1.,0.,0.));
#33564=DIRECTION('center_axis',(0.,0.,1.));
#33565=DIRECTION('ref_axis',(1.,0.,0.));
#33566=DIRECTION('center_axis',(0.,-0.707106781186541,0.707106781186554));
#33567=DIRECTION('ref_axis',(1.,0.,0.));
#33568=DIRECTION('',(-1.,0.,0.));
#33569=DIRECTION('center_axis',(0.,0.,1.));
#33570=DIRECTION('ref_axis',(1.,0.,0.));
#33571=DIRECTION('center_axis',(-1.,0.,0.));
#33572=DIRECTION('ref_axis',(0.,-1.,0.));
#33573=DIRECTION('axis',(0.,0.,1.));
#33574=DIRECTION('refdir',(1.,0.,0.));
#33575=DIRECTION('center_axis',(0.,0.,1.));
#33576=DIRECTION('ref_axis',(1.,0.,0.));
#33577=DIRECTION('',(0.,0.,-1.));
#33578=DIRECTION('center_axis',(0.,0.,1.));
#33579=DIRECTION('ref_axis',(1.,0.,0.));
#33580=DIRECTION('center_axis',(0.,0.,1.));
#33581=DIRECTION('ref_axis',(1.,0.,0.));
#33582=DIRECTION('',(0.,0.,-1.));
#33583=DIRECTION('center_axis',(0.,0.,1.));
#33584=DIRECTION('ref_axis',(1.,0.,0.));
#33585=DIRECTION('',(0.,0.,-1.));
#33586=DIRECTION('center_axis',(0.,0.,1.));
#33587=DIRECTION('ref_axis',(1.,0.,0.));
#33588=DIRECTION('',(0.,0.,-1.));
#33589=DIRECTION('center_axis',(0.,0.,1.));
#33590=DIRECTION('ref_axis',(1.,0.,0.));
#33591=DIRECTION('',(0.,0.,-1.));
#33592=DIRECTION('center_axis',(0.,0.,1.));
#33593=DIRECTION('ref_axis',(1.,0.,0.));
#33594=DIRECTION('',(0.,0.,-1.));
#33595=DIRECTION('center_axis',(0.,0.,1.));
#33596=DIRECTION('ref_axis',(1.,0.,0.));
#33597=DIRECTION('',(0.,0.,-1.));
#33598=DIRECTION('center_axis',(0.,0.,1.));
#33599=DIRECTION('ref_axis',(1.,0.,0.));
#33600=DIRECTION('',(0.,0.,-1.));
#33601=DIRECTION('center_axis',(0.,0.,1.));
#33602=DIRECTION('ref_axis',(1.,0.,0.));
#33603=DIRECTION('',(0.,0.,-1.));
#33604=DIRECTION('center_axis',(0.,0.,1.));
#33605=DIRECTION('ref_axis',(1.,0.,0.));
#33606=DIRECTION('',(0.,0.,-1.));
#33607=DIRECTION('center_axis',(0.,0.,1.));
#33608=DIRECTION('ref_axis',(1.,0.,0.));
#33609=DIRECTION('',(0.,0.,-1.));
#33610=DIRECTION('center_axis',(0.,0.,1.));
#33611=DIRECTION('ref_axis',(1.,0.,0.));
#33612=DIRECTION('',(0.,0.,-1.));
#33613=DIRECTION('center_axis',(0.,0.,1.));
#33614=DIRECTION('ref_axis',(1.,0.,0.));
#33615=DIRECTION('',(0.,0.,-1.));
#33616=DIRECTION('center_axis',(0.,0.,1.));
#33617=DIRECTION('ref_axis',(1.,0.,0.));
#33618=DIRECTION('',(0.,0.,-1.));
#33619=DIRECTION('center_axis',(0.,0.,1.));
#33620=DIRECTION('ref_axis',(1.,0.,0.));
#33621=DIRECTION('',(0.,0.,-1.));
#33622=DIRECTION('center_axis',(0.,0.,1.));
#33623=DIRECTION('ref_axis',(1.,0.,0.));
#33624=DIRECTION('',(0.,0.,-1.));
#33625=DIRECTION('center_axis',(0.,0.,1.));
#33626=DIRECTION('ref_axis',(1.,0.,0.));
#33627=DIRECTION('',(0.,0.,-1.));
#33628=DIRECTION('center_axis',(0.,0.,1.));
#33629=DIRECTION('ref_axis',(1.,0.,0.));
#33630=DIRECTION('',(0.,0.,-1.));
#33631=DIRECTION('center_axis',(0.,0.,1.));
#33632=DIRECTION('ref_axis',(1.,0.,0.));
#33633=DIRECTION('',(0.,0.,-1.));
#33634=DIRECTION('center_axis',(0.,0.,1.));
#33635=DIRECTION('ref_axis',(1.,0.,0.));
#33636=DIRECTION('',(0.,0.,-1.));
#33637=DIRECTION('center_axis',(0.,0.,1.));
#33638=DIRECTION('ref_axis',(1.,1.08272661726521E-13,0.));
#33639=DIRECTION('',(0.,0.,1.));
#33640=DIRECTION('center_axis',(0.,0.,1.));
#33641=DIRECTION('ref_axis',(1.,1.08272661726521E-13,0.));
#33642=DIRECTION('center_axis',(0.,0.,1.));
#33643=DIRECTION('ref_axis',(1.,1.08272661726521E-13,0.));
#33644=DIRECTION('',(0.,0.,1.));
#33645=DIRECTION('center_axis',(0.,0.,1.));
#33646=DIRECTION('ref_axis',(1.,1.08272661726521E-13,0.));
#33647=DIRECTION('center_axis',(0.,0.,1.));
#33648=DIRECTION('ref_axis',(1.,1.08272661726521E-13,0.));
#33649=DIRECTION('',(0.,0.,1.));
#33650=DIRECTION('center_axis',(0.,0.,1.));
#33651=DIRECTION('ref_axis',(1.,1.08272661726521E-13,0.));
#33652=DIRECTION('',(0.,0.,1.));
#33653=DIRECTION('center_axis',(0.,0.,1.));
#33654=DIRECTION('ref_axis',(1.,1.08272661726521E-13,0.));
#33655=DIRECTION('',(0.,0.,1.));
#33656=DIRECTION('center_axis',(0.,0.,1.));
#33657=DIRECTION('ref_axis',(1.,1.08272661726521E-13,0.));
#33658=DIRECTION('',(0.,0.,1.));
#33659=DIRECTION('center_axis',(0.,0.,1.));
#33660=DIRECTION('ref_axis',(1.,1.08272661726521E-13,0.));
#33661=DIRECTION('',(0.,0.,1.));
#33662=DIRECTION('center_axis',(0.,0.,1.));
#33663=DIRECTION('ref_axis',(1.,1.08272661726521E-13,0.));
#33664=DIRECTION('',(0.,0.,1.));
#33665=DIRECTION('center_axis',(0.,0.,1.));
#33666=DIRECTION('ref_axis',(1.,1.08272661726521E-13,0.));
#33667=DIRECTION('',(0.,0.,1.));
#33668=DIRECTION('center_axis',(0.,0.,1.));
#33669=DIRECTION('ref_axis',(1.,1.08272661726521E-13,0.));
#33670=DIRECTION('',(0.,0.,1.));
#33671=DIRECTION('center_axis',(0.,0.,1.));
#33672=DIRECTION('ref_axis',(1.,1.08272661726521E-13,0.));
#33673=DIRECTION('',(0.,0.,1.));
#33674=DIRECTION('center_axis',(0.,0.,1.));
#33675=DIRECTION('ref_axis',(1.,1.08272661726521E-13,0.));
#33676=DIRECTION('',(0.,0.,1.));
#33677=DIRECTION('center_axis',(0.,0.,1.));
#33678=DIRECTION('ref_axis',(1.,1.08272661726521E-13,0.));
#33679=DIRECTION('',(0.,0.,1.));
#33680=DIRECTION('center_axis',(0.,0.,1.));
#33681=DIRECTION('ref_axis',(1.,1.08272661726521E-13,0.));
#33682=DIRECTION('',(0.,0.,1.));
#33683=DIRECTION('center_axis',(0.,0.,1.));
#33684=DIRECTION('ref_axis',(1.,1.08272661726521E-13,0.));
#33685=DIRECTION('',(0.,0.,1.));
#33686=DIRECTION('center_axis',(0.,0.,1.));
#33687=DIRECTION('ref_axis',(1.,1.08272661726521E-13,0.));
#33688=DIRECTION('',(0.,0.,1.));
#33689=DIRECTION('center_axis',(0.,0.,1.));
#33690=DIRECTION('ref_axis',(1.,1.08272661726521E-13,0.));
#33691=DIRECTION('',(0.,0.,1.));
#33692=DIRECTION('center_axis',(0.,0.,1.));
#33693=DIRECTION('ref_axis',(1.,1.08272661726521E-13,0.));
#33694=DIRECTION('',(0.,0.,1.));
#33695=DIRECTION('center_axis',(0.,0.,1.));
#33696=DIRECTION('ref_axis',(1.,1.08272661726521E-13,0.));
#33697=DIRECTION('',(0.,0.,1.));
#33698=DIRECTION('center_axis',(0.,0.,1.));
#33699=DIRECTION('ref_axis',(1.,1.08272661726521E-13,0.));
#33700=DIRECTION('',(0.,0.,1.));
#33701=DIRECTION('center_axis',(0.,0.,1.));
#33702=DIRECTION('ref_axis',(1.,0.,0.));
#33703=DIRECTION('center_axis',(0.,0.,1.));
#33704=DIRECTION('ref_axis',(1.,0.,0.));
#33705=DIRECTION('center_axis',(0.,0.,1.));
#33706=DIRECTION('ref_axis',(1.,0.,0.));
#33707=DIRECTION('center_axis',(0.,0.,-1.));
#33708=DIRECTION('ref_axis',(1.,1.08272661726521E-13,0.));
#33709=DIRECTION('center_axis',(0.,0.,1.));
#33710=DIRECTION('ref_axis',(0.888988591948248,0.457929343224335,0.));
#33711=DIRECTION('center_axis',(0.,0.,-1.));
#33712=DIRECTION('ref_axis',(1.,0.,0.));
#33713=DIRECTION('',(0.866025403784438,1.06057523872491E-16,0.5));
#33714=DIRECTION('center_axis',(0.,0.,1.));
#33715=DIRECTION('ref_axis',(1.,0.,0.));
#33716=DIRECTION('center_axis',(-0.5,0.866025403784439,0.));
#33717=DIRECTION('ref_axis',(-0.866025403784439,-0.5,0.));
#33718=DIRECTION('',(0.,0.,1.));
#33719=DIRECTION('',(-0.866025403784439,-0.5,0.));
#33720=DIRECTION('',(0.,0.,1.));
#33721=DIRECTION('center_axis',(0.5,0.866025403784439,0.));
#33722=DIRECTION('ref_axis',(-0.866025403784439,0.5,0.));
#33723=DIRECTION('',(0.,0.,1.));
#33724=DIRECTION('',(-0.866025403784439,0.5,0.));
#33725=DIRECTION('center_axis',(1.,-3.20493781063927E-16,0.));
#33726=DIRECTION('ref_axis',(3.20493781063927E-16,1.,0.));
#33727=DIRECTION('',(0.,0.,1.));
#33728=DIRECTION('',(3.20493781063927E-16,1.,0.));
#33729=DIRECTION('center_axis',(0.,0.,1.));
#33730=DIRECTION('ref_axis',(1.,0.,0.));
#33731=DIRECTION('',(0.866025403784439,0.5,0.));
#33732=DIRECTION('',(0.866025403784439,-0.5,0.));
#33733=DIRECTION('',(1.60246890531964E-16,-1.,0.));
#33734=DIRECTION('center_axis',(0.,0.,1.));
#33735=DIRECTION('ref_axis',(1.,0.,0.));
#33736=DIRECTION('center_axis',(0.5,-0.866025403784439,0.));
#33737=DIRECTION('ref_axis',(0.866025403784439,0.5,0.));
#33738=DIRECTION('',(0.,0.,1.));
#33739=DIRECTION('center_axis',(-0.5,-0.866025403784439,0.));
#33740=DIRECTION('ref_axis',(0.866025403784439,-0.5,0.));
#33741=DIRECTION('',(0.,0.,1.));
#33742=DIRECTION('center_axis',(-1.,-1.60246890531964E-16,0.));
#33743=DIRECTION('ref_axis',(1.60246890531964E-16,-1.,0.));
#33744=DIRECTION('center_axis',(0.,0.,1.));
#33745=DIRECTION('ref_axis',(1.,0.,0.));
#33746=DIRECTION('center_axis',(0.,0.,-1.));
#33747=DIRECTION('ref_axis',(-1.,0.,0.));
#33748=DIRECTION('center_axis',(0.,0.,1.));
#33749=DIRECTION('ref_axis',(1.,0.,0.));
#33750=DIRECTION('center_axis',(0.,0.,1.));
#33751=DIRECTION('ref_axis',(1.,0.,0.));
#33752=DIRECTION('',(0.707106781186548,8.65956056235493E-17,-0.707106781186548));
#33753=DIRECTION('center_axis',(0.,0.,1.));
#33754=DIRECTION('ref_axis',(1.,0.,0.));
#33755=DIRECTION('center_axis',(0.,0.,1.));
#33756=DIRECTION('ref_axis',(1.,0.,0.));
#33757=DIRECTION('center_axis',(0.,0.,-1.));
#33758=DIRECTION('ref_axis',(-1.,0.,0.));
#33759=DIRECTION('center_axis',(0.,0.,1.));
#33760=DIRECTION('ref_axis',(1.,0.,0.));
#33761=DIRECTION('center_axis',(0.,0.,1.));
#33762=DIRECTION('ref_axis',(1.,0.,0.));
#33763=DIRECTION('',(0.,0.,-1.));
#33764=DIRECTION('axis',(0.,0.,1.));
#33765=DIRECTION('refdir',(1.,0.,0.));
#33766=DIRECTION('center_axis',(0.,1.50614812182896E-15,1.));
#33767=DIRECTION('ref_axis',(1.,2.918397135658E-17,0.));
#33768=DIRECTION('center_axis',(0.,0.,-1.));
#33769=DIRECTION('ref_axis',(1.,6.12323399573679E-17,0.));
#33770=DIRECTION('',(-0.923879532511297,6.62558070326733E-16,0.382683432365065));
#33771=DIRECTION('center_axis',(0.,0.,1.));
#33772=DIRECTION('ref_axis',(1.,0.,0.));
#33773=DIRECTION('center_axis',(0.,0.,1.));
#33774=DIRECTION('ref_axis',(1.,0.,0.));
#33775=DIRECTION('',(0.707106781186552,8.65956056235499E-17,-0.707106781186543));
#33776=DIRECTION('center_axis',(1.617924002207E-32,-2.64227041353223E-16,
1.));
#33777=DIRECTION('ref_axis',(1.,6.12323399573677E-17,0.));
#33778=DIRECTION('center_axis',(0.,0.,1.));
#33779=DIRECTION('ref_axis',(1.,0.,0.));
#33780=DIRECTION('',(0.,1.,0.));
#33781=DIRECTION('center_axis',(0.,0.,-1.));
#33782=DIRECTION('ref_axis',(-1.,-6.6613381477509E-15,0.));
#33783=DIRECTION('',(-1.,0.,0.));
#33784=DIRECTION('center_axis',(0.,0.,-1.));
#33785=DIRECTION('ref_axis',(0.,-1.,0.));
#33786=DIRECTION('',(0.,-1.,0.));
#33787=DIRECTION('center_axis',(0.,0.,-1.));
#33788=DIRECTION('ref_axis',(1.,-2.22044604925032E-15,0.));
#33789=DIRECTION('',(1.,0.,0.));
#33790=DIRECTION('center_axis',(0.,0.,-1.));
#33791=DIRECTION('ref_axis',(-4.4408920985006E-15,1.,0.));
#33792=DIRECTION('center_axis',(0.,-6.02855361754257E-16,1.));
#33793=DIRECTION('ref_axis',(1.,3.12740491884801E-17,0.));
#33794=DIRECTION('',(0.382683432365095,6.1579899433011E-16,-0.923879532511285));
#33795=DIRECTION('center_axis',(0.,0.,-1.));
#33796=DIRECTION('ref_axis',(1.,0.,0.));
#33797=DIRECTION('center_axis',(0.,0.,1.));
#33798=DIRECTION('ref_axis',(1.,0.,0.));
#33799=DIRECTION('center_axis',(0.,0.,1.));
#33800=DIRECTION('ref_axis',(1.,0.,0.));
#33801=DIRECTION('',(0.,0.,1.));
#33802=DIRECTION('center_axis',(0.,6.02855361754257E-16,-1.));
#33803=DIRECTION('ref_axis',(1.,-3.12740491884801E-17,0.));
#33804=DIRECTION('center_axis',(2.4268860033105E-32,3.96340562029835E-16,
-1.));
#33805=DIRECTION('ref_axis',(1.,-6.12323399573677E-17,0.));
#33806=DIRECTION('',(0.382683432365094,-6.1579899433011E-16,0.923879532511285));
#33807=DIRECTION('center_axis',(0.,0.,-1.));
#33808=DIRECTION('ref_axis',(1.,0.,0.));
#33809=DIRECTION('center_axis',(3.90858224776604E-33,6.38319922199173E-17,
1.));
#33810=DIRECTION('ref_axis',(1.,-6.12323399573679E-17,0.));
#33811=DIRECTION('',(0.707106781186553,-8.659560562355E-17,0.707106781186542));
#33812=DIRECTION('center_axis',(0.,-1.50614812182896E-15,-1.));
#33813=DIRECTION('ref_axis',(1.,-2.918397135658E-17,0.));
#33814=DIRECTION('',(-0.923879532511297,-6.62558070326733E-16,-0.382683432365064));
#33815=DIRECTION('center_axis',(0.,0.,-1.));
#33816=DIRECTION('ref_axis',(1.,0.,0.));
#33817=DIRECTION('center_axis',(0.,0.,1.));
#33818=DIRECTION('ref_axis',(1.,0.,0.));
#33819=DIRECTION('',(0.,-1.,0.));
#33820=DIRECTION('center_axis',(0.,0.,1.));
#33821=DIRECTION('ref_axis',(-4.4408920985006E-15,1.,0.));
#33822=DIRECTION('',(-1.,0.,0.));
#33823=DIRECTION('center_axis',(0.,0.,1.));
#33824=DIRECTION('ref_axis',(1.,-2.22044604925032E-15,0.));
#33825=DIRECTION('',(0.,1.,0.));
#33826=DIRECTION('center_axis',(0.,0.,1.));
#33827=DIRECTION('ref_axis',(0.,-1.,0.));
#33828=DIRECTION('',(1.,0.,0.));
#33829=DIRECTION('center_axis',(0.,0.,1.));
#33830=DIRECTION('ref_axis',(-1.,-6.6613381477509E-15,0.));
#33831=DIRECTION('center_axis',(0.,0.,-1.));
#33832=DIRECTION('ref_axis',(1.,-2.27062013982434E-15,0.));
#33833=DIRECTION('',(0.,-0.382683432365106,0.92387953251128));
#33834=DIRECTION('center_axis',(4.72225197640989E-30,2.03272489022952E-15,
-1.));
#33835=DIRECTION('ref_axis',(1.,-2.32311416026233E-15,0.));
#33836=DIRECTION('',(0.382683432365098,-9.61357393951414E-15,-0.923879532511283));
#33837=DIRECTION('center_axis',(0.,0.,1.));
#33838=DIRECTION('ref_axis',(1.,-2.22044604925032E-15,0.));
#33839=DIRECTION('center_axis',(0.,0.923879532511288,0.382683432365087));
#33840=DIRECTION('ref_axis',(0.,-0.382683432365087,0.923879532511288));
#33841=DIRECTION('',(0.,-0.382683432365087,0.923879532511288));
#33842=DIRECTION('',(1.,0.,0.));
#33843=DIRECTION('',(-1.,0.,0.));
#33844=DIRECTION('center_axis',(0.,0.,-1.));
#33845=DIRECTION('ref_axis',(-4.54124027964863E-15,1.,0.));
#33846=DIRECTION('',(0.382683432365071,0.,0.923879532511295));
#33847=DIRECTION('center_axis',(-5.80778540065573E-16,-2.69842970080559E-30,
-1.));
#33848=DIRECTION('ref_axis',(-4.64622832052459E-15,1.,0.));
#33849=DIRECTION('center_axis',(0.,0.,1.));
#33850=DIRECTION('ref_axis',(-4.4408920985006E-15,1.,0.));
#33851=DIRECTION('center_axis',(-0.923879532511282,0.,0.382683432365102));
#33852=DIRECTION('ref_axis',(0.382683432365102,0.,0.923879532511282));
#33853=DIRECTION('',(0.382683432365101,0.,0.923879532511282));
#33854=DIRECTION('',(0.,1.,0.));
#33855=DIRECTION('',(0.,-1.,0.));
#33856=DIRECTION('center_axis',(0.,0.,-1.));
#33857=DIRECTION('ref_axis',(-1.,-6.81186041947294E-15,0.));
#33858=DIRECTION('',(0.,0.382683432365072,0.923879532511294));
#33859=DIRECTION('center_axis',(-4.04764455120838E-30,5.80778540065573E-16,
-1.));
#33860=DIRECTION('ref_axis',(-1.,-6.96934248078688E-15,0.));
#33861=DIRECTION('center_axis',(0.,0.,1.));
#33862=DIRECTION('ref_axis',(-1.,-6.6613381477509E-15,0.));
#33863=DIRECTION('center_axis',(0.,-0.923879532511288,0.382683432365087));
#33864=DIRECTION('ref_axis',(0.,-0.382683432365087,-0.923879532511288));
#33865=DIRECTION('',(0.,0.382683432365087,0.923879532511288));
#33866=DIRECTION('',(-1.,0.,0.));
#33867=DIRECTION('',(1.,0.,0.));
#33868=DIRECTION('center_axis',(0.,0.,-1.));
#33869=DIRECTION('ref_axis',(0.,-1.,0.));
#33870=DIRECTION('',(-0.382683432365058,0.,0.9238795325113));
#33871=DIRECTION('center_axis',(-2.61350343029512E-15,0.,-1.));
#33872=DIRECTION('ref_axis',(0.,-1.,0.));
#33873=DIRECTION('center_axis',(0.,0.,1.));
#33874=DIRECTION('ref_axis',(0.,-1.,0.));
#33875=DIRECTION('center_axis',(0.923879532511282,0.,0.382683432365101));
#33876=DIRECTION('ref_axis',(0.382683432365101,0.,-0.923879532511282));
#33877=DIRECTION('',(0.,-1.,0.));
#33878=DIRECTION('',(0.,1.,0.));
#33879=DIRECTION('center_axis',(-1.,0.,0.));
#33880=DIRECTION('ref_axis',(0.,-1.,0.));
#33881=DIRECTION('',(0.,0.,1.));
#33882=DIRECTION('',(0.,1.,0.));
#33883=DIRECTION('',(0.,0.,1.));
#33884=DIRECTION('center_axis',(0.,0.,1.));
#33885=DIRECTION('ref_axis',(-4.4408920985006E-15,1.,0.));
#33886=DIRECTION('',(0.,0.,1.));
#33887=DIRECTION('center_axis',(0.,0.,-1.));
#33888=DIRECTION('ref_axis',(-4.4408920985006E-15,1.,0.));
#33889=DIRECTION('center_axis',(0.,1.,0.));
#33890=DIRECTION('ref_axis',(-1.,0.,0.));
#33891=DIRECTION('',(0.,0.,1.));
#33892=DIRECTION('',(1.,0.,0.));
#33893=DIRECTION('center_axis',(0.,0.,1.));
#33894=DIRECTION('ref_axis',(1.,-2.22044604925032E-15,0.));
#33895=DIRECTION('',(0.,0.,1.));
#33896=DIRECTION('center_axis',(0.,0.,-1.));
#33897=DIRECTION('ref_axis',(1.,-2.22044604925032E-15,0.));
#33898=DIRECTION('center_axis',(0.,-0.707106781186549,0.707106781186546));
#33899=DIRECTION('ref_axis',(1.,0.,0.));
#33900=DIRECTION('',(0.,0.707106781186546,0.707106781186549));
#33901=DIRECTION('',(0.,0.707106781186546,0.707106781186549));
#33902=DIRECTION('center_axis',(0.,0.,-1.));
#33903=DIRECTION('ref_axis',(0.,-1.,0.));
#33904=DIRECTION('',(-0.707106781186552,0.,0.707106781186543));
#33905=DIRECTION('center_axis',(0.707106781186543,0.,0.707106781186552));
#33906=DIRECTION('ref_axis',(0.707106781186552,0.,-0.707106781186543));
#33907=DIRECTION('',(-0.707106781186552,6.28036983473505E-15,0.707106781186543));
#33908=DIRECTION('center_axis',(0.,0.,-1.));
#33909=DIRECTION('ref_axis',(1.,-2.22044604925032E-15,0.));
#33910=DIRECTION('',(0.,-0.707106781186562,0.707106781186533));
#33911=DIRECTION('center_axis',(-0.382683432365119,0.,-0.923879532511275));
#33912=DIRECTION('ref_axis',(-0.923879532511275,0.,0.382683432365119));
#33913=DIRECTION('',(-0.923879532511278,9.61357393951443E-15,0.382683432365112));
#33914=DIRECTION('',(0.,1.,0.));
#33915=DIRECTION('',(0.923879532511278,0.,-0.382683432365112));
#33916=DIRECTION('center_axis',(0.,0.,1.));
#33917=DIRECTION('ref_axis',(-1.,-6.97217532708781E-15,0.));
#33918=DIRECTION('',(0.,-0.923879532511291,0.38268343236508));
#33919=DIRECTION('center_axis',(-5.47062821941541E-31,7.54888803857301E-17,
-1.));
#33920=DIRECTION('ref_axis',(-1.,-7.24693251703008E-15,0.));
#33921=DIRECTION('center_axis',(0.,-0.382683432365091,-0.923879532511286));
#33922=DIRECTION('ref_axis',(-1.,0.,0.));
#33923=DIRECTION('',(0.,-0.923879532511286,0.382683432365091));
#33924=DIRECTION('',(-1.,0.,0.));
#33925=DIRECTION('center_axis',(0.,0.,1.));
#33926=DIRECTION('ref_axis',(0.,-1.,0.));
#33927=DIRECTION('',(0.923879532511292,0.,0.382683432365078));
#33928=DIRECTION('center_axis',(1.4342887273289E-15,0.,-1.));
#33929=DIRECTION('ref_axis',(0.,-1.,0.));
#33930=DIRECTION('center_axis',(0.382683432365081,0.,-0.92387953251129));
#33931=DIRECTION('ref_axis',(-0.92387953251129,0.,-0.382683432365081));
#33932=DIRECTION('',(0.92387953251129,-9.61357393951456E-15,0.382683432365082));
#33933=DIRECTION('',(0.,-1.,0.));
#33934=DIRECTION('center_axis',(0.,0.,1.));
#33935=DIRECTION('ref_axis',(1.,-2.32405844236264E-15,0.));
#33936=DIRECTION('',(0.,0.923879532511303,0.382683432365051));
#33937=DIRECTION('center_axis',(-3.28237693164936E-30,-1.35879984694316E-15,
-1.));
#33938=DIRECTION('ref_axis',(1.,-2.41564417234341E-15,0.));
#33939=DIRECTION('center_axis',(0.,0.382683432365091,-0.923879532511286));
#33940=DIRECTION('ref_axis',(-1.,0.,0.));
#33941=DIRECTION('',(0.,0.923879532511286,0.382683432365091));
#33942=DIRECTION('',(1.,0.,0.));
#33943=DIRECTION('center_axis',(0.,0.,1.));
#33944=DIRECTION('ref_axis',(-4.64811688472521E-15,1.,0.));
#33945=DIRECTION('center_axis',(-6.79399923471573E-16,-3.28237693164927E-30,
-1.));
#33946=DIRECTION('ref_axis',(-4.83128834468673E-15,1.,0.));
#33947=DIRECTION('center_axis',(0.,0.,1.));
#33948=DIRECTION('ref_axis',(1.,-2.22044604925032E-15,0.));
#33949=DIRECTION('',(0.,0.707106781186562,0.707106781186533));
#33950=DIRECTION('center_axis',(-4.55360012010954E-30,-1.96012757272133E-15,
1.));
#33951=DIRECTION('ref_axis',(1.,-2.32311416026233E-15,0.));
#33952=DIRECTION('',(0.707106781186578,-6.28036983473483E-15,0.707106781186517));
#33953=DIRECTION('center_axis',(0.,0.707106781186549,-0.707106781186546));
#33954=DIRECTION('ref_axis',(-1.,0.,0.));
#33955=DIRECTION('',(0.,0.707106781186546,0.707106781186549));
#33956=DIRECTION('',(-1.,0.,0.));
#33957=DIRECTION('center_axis',(0.,0.,1.));
#33958=DIRECTION('ref_axis',(-4.4408920985006E-15,1.,0.));
#33959=DIRECTION('',(0.707106781186552,0.,-0.707106781186543));
#33960=DIRECTION('center_axis',(-1.81493293770492E-15,-8.43259281501748E-30,
1.));
#33961=DIRECTION('ref_axis',(-4.64622832052459E-15,1.,0.));
#33962=DIRECTION('center_axis',(-0.707106781186543,0.,-0.707106781186552));
#33963=DIRECTION('ref_axis',(-0.707106781186552,0.,0.707106781186543));
#33964=DIRECTION('',(-0.707106781186552,6.28036983473505E-15,0.707106781186543));
#33965=DIRECTION('',(0.,-1.,0.));
#33966=DIRECTION('center_axis',(-0.923879532511297,0.,-0.382683432365065));
#33967=DIRECTION('ref_axis',(-0.382683432365065,0.,0.923879532511297));
#33968=DIRECTION('',(0.382683432365068,0.,-0.923879532511296));
#33969=DIRECTION('',(-0.382683432365068,0.,0.923879532511296));
#33970=DIRECTION('center_axis',(0.,0.,1.));
#33971=DIRECTION('ref_axis',(-4.54124027964863E-15,1.,0.));
#33972=DIRECTION('',(0.,-0.382683432365081,-0.923879532511291));
#33973=DIRECTION('center_axis',(0.,0.923879532511287,-0.382683432365088));
#33974=DIRECTION('ref_axis',(0.,0.382683432365088,0.923879532511287));
#33975=DIRECTION('',(0.,-0.3826834323651,-0.923879532511283));
#33976=DIRECTION('center_axis',(0.,0.,1.));
#33977=DIRECTION('ref_axis',(1.,-2.27062013982434E-15,0.));
#33978=DIRECTION('',(-0.382683432365108,9.6135739395144E-15,-0.923879532511279));
#33979=DIRECTION('center_axis',(0.92387953251128,0.,-0.382683432365108));
#33980=DIRECTION('ref_axis',(-0.382683432365108,0.,-0.92387953251128));
#33981=DIRECTION('',(-0.382683432365102,0.,-0.923879532511282));
#33982=DIRECTION('',(0.,1.,0.));
#33983=DIRECTION('',(0.,-1.,0.));
#33984=DIRECTION('center_axis',(0.,0.,1.));
#33985=DIRECTION('ref_axis',(0.,-1.,0.));
#33986=DIRECTION('',(0.,0.382683432365081,-0.923879532511291));
#33987=DIRECTION('center_axis',(2.68610074780331E-15,0.,1.));
#33988=DIRECTION('ref_axis',(0.,-1.,0.));
#33989=DIRECTION('center_axis',(0.,0.,-1.));
#33990=DIRECTION('ref_axis',(0.,-1.,0.));
#33991=DIRECTION('center_axis',(0.,-0.923879532511287,-0.382683432365088));
#33992=DIRECTION('ref_axis',(0.,0.382683432365088,-0.923879532511287));
#33993=DIRECTION('',(0.,0.38268343236509,-0.923879532511287));
#33994=DIRECTION('',(1.,0.,0.));
#33995=DIRECTION('',(-1.,0.,0.));
#33996=DIRECTION('center_axis',(0.,0.,1.));
#33997=DIRECTION('ref_axis',(-1.,-6.81186041947294E-15,0.));
#33998=DIRECTION('center_axis',(3.54168898230734E-30,-5.08181222557377E-16,
1.));
#33999=DIRECTION('ref_axis',(-1.,-6.96934248078688E-15,0.));
#34000=DIRECTION('center_axis',(0.,0.,-1.));
#34001=DIRECTION('ref_axis',(-1.,-6.6613381477509E-15,0.));
#34002=DIRECTION('center_axis',(0.,0.,1.));
#34003=DIRECTION('ref_axis',(0.,-1.,0.));
#34004=DIRECTION('',(0.707106781186552,0.,0.707106781186543));
#34005=DIRECTION('',(0.,-0.707106781186546,0.707106781186549));
#34006=DIRECTION('center_axis',(0.,-0.707106781186549,-0.707106781186546));
#34007=DIRECTION('ref_axis',(-1.,0.,0.));
#34008=DIRECTION('',(0.,-0.707106781186546,0.707106781186549));
#34009=DIRECTION('center_axis',(0.,0.,1.));
#34010=DIRECTION('ref_axis',(-1.,-6.66133814775091E-15,0.));
#34011=DIRECTION('center_axis',(0.707106781186517,0.,-0.707106781186578));
#34012=DIRECTION('ref_axis',(-0.707106781186578,0.,-0.707106781186517));
#34013=DIRECTION('center_axis',(-0.707106781186543,0.,0.707106781186552));
#34014=DIRECTION('ref_axis',(0.707106781186552,0.,0.707106781186543));
#34015=DIRECTION('',(0.707106781186552,-6.28036983473505E-15,0.707106781186543));
#34016=DIRECTION('',(-0.707106781186552,0.,-0.707106781186543));
#34017=DIRECTION('center_axis',(0.,0.,-1.));
#34018=DIRECTION('ref_axis',(-1.,-6.66133814775091E-15,0.));
#34019=DIRECTION('center_axis',(0.,0.707106781186549,0.707106781186546));
#34020=DIRECTION('ref_axis',(1.,0.,0.));
#34021=DIRECTION('',(0.,-0.707106781186546,0.707106781186549));
#34022=DIRECTION('center_axis',(0.,0.,-1.));
#34023=DIRECTION('ref_axis',(-4.4408920985006E-15,1.,0.));
#34024=DIRECTION('center_axis',(0.,0.,1.));
#34025=DIRECTION('ref_axis',(0.,-1.,0.));
#34026=DIRECTION('',(0.,0.,1.));
#34027=DIRECTION('',(0.,0.,1.));
#34028=DIRECTION('center_axis',(0.,-1.,0.));
#34029=DIRECTION('ref_axis',(1.,0.,0.));
#34030=DIRECTION('',(0.,0.,1.));
#34031=DIRECTION('center_axis',(0.,0.,1.));
#34032=DIRECTION('ref_axis',(-1.,-6.6613381477509E-15,0.));
#34033=DIRECTION('center_axis',(1.,0.,0.));
#34034=DIRECTION('ref_axis',(0.,1.,0.));
#34035=DIRECTION('axis',(0.,0.,1.));
#34036=DIRECTION('refdir',(1.,0.,0.));
#34037=DIRECTION('center_axis',(1.,0.,0.));
#34038=DIRECTION('ref_axis',(0.,1.,0.));
#34039=DIRECTION('center_axis',(1.,0.,0.));
#34040=DIRECTION('ref_axis',(0.,0.,-1.));
#34041=DIRECTION('',(0.707106781186541,-0.707106781186554,-8.65956056235502E-17));
#34042=DIRECTION('center_axis',(1.,0.,0.));
#34043=DIRECTION('ref_axis',(0.,1.,0.));
#34044=DIRECTION('center_axis',(-1.,0.,0.));
#34045=DIRECTION('ref_axis',(0.,1.,0.));
#34046=DIRECTION('center_axis',(-1.,0.,0.));
#34047=DIRECTION('ref_axis',(0.,1.,0.));
#34048=DIRECTION('',(0.707106781186548,0.707106781186547,8.65956056235492E-17));
#34049=DIRECTION('center_axis',(1.,0.,0.));
#34050=DIRECTION('ref_axis',(0.,1.,0.));
#34051=DIRECTION('',(-1.,0.,0.));
#34052=DIRECTION('center_axis',(1.,0.,0.));
#34053=DIRECTION('ref_axis',(0.,0.,-1.));
#34054=DIRECTION('center_axis',(1.,0.,0.));
#34055=DIRECTION('ref_axis',(0.,1.,0.));
#34056=DIRECTION('center_axis',(1.,0.,0.));
#34057=DIRECTION('ref_axis',(0.,0.,-1.));
#34058=DIRECTION('',(-1.,0.,0.));
#34059=DIRECTION('center_axis',(1.,0.,0.));
#34060=DIRECTION('ref_axis',(0.,0.,-1.));
#34061=DIRECTION('center_axis',(-1.,0.,0.));
#34062=DIRECTION('ref_axis',(0.,0.,1.));
#34063=DIRECTION('center_axis',(1.,0.,0.));
#34064=DIRECTION('ref_axis',(0.,0.,-1.));
#34065=DIRECTION('center_axis',(1.,0.,0.));
#34066=DIRECTION('ref_axis',(0.,1.,0.));
#34067=DIRECTION('center_axis',(1.,0.,0.));
#34068=DIRECTION('ref_axis',(0.,0.,-1.));
#34069=DIRECTION('',(-0.707106781186546,0.707106781186549,8.65956056235495E-17));
#34070=DIRECTION('center_axis',(1.,0.,0.));
#34071=DIRECTION('ref_axis',(0.,1.,0.));
#34072=DIRECTION('center_axis',(1.,0.,0.));
#34073=DIRECTION('ref_axis',(0.,0.,-1.));
#34074=DIRECTION('',(-1.,0.,0.));
#34075=DIRECTION('center_axis',(1.,0.,0.));
#34076=DIRECTION('ref_axis',(0.,0.,-1.));
#34077=DIRECTION('center_axis',(1.,0.,0.));
#34078=DIRECTION('ref_axis',(0.,1.,0.));
#34079=DIRECTION('center_axis',(1.,0.,0.));
#34080=DIRECTION('ref_axis',(0.,0.,-1.));
#34081=DIRECTION('',(-1.,0.,0.));
#34082=DIRECTION('center_axis',(-1.,0.,0.));
#34083=DIRECTION('ref_axis',(0.,0.,1.));
#34084=DIRECTION('center_axis',(1.,0.,0.));
#34085=DIRECTION('ref_axis',(0.,0.,-1.));
#34086=DIRECTION('center_axis',(1.,0.,0.));
#34087=DIRECTION('ref_axis',(0.,1.,0.));
#34088=DIRECTION('center_axis',(1.,0.,0.));
#34089=DIRECTION('ref_axis',(0.,0.,-1.));
#34090=DIRECTION('',(-1.,0.,0.));
#34091=DIRECTION('center_axis',(-1.,0.,0.));
#34092=DIRECTION('ref_axis',(0.,1.,0.));
#34093=DIRECTION('center_axis',(1.,0.,0.));
#34094=DIRECTION('ref_axis',(0.,0.,-1.));
#34095=DIRECTION('',(-0.707106781186552,-0.707106781186543,-8.65956056235488E-17));
#34096=DIRECTION('center_axis',(1.,0.,0.));
#34097=DIRECTION('ref_axis',(0.,0.,-1.));
#34098=DIRECTION('center_axis',(1.,0.,0.));
#34099=DIRECTION('ref_axis',(0.,0.,-1.));
#34100=DIRECTION('center_axis',(1.,0.,0.));
#34101=DIRECTION('ref_axis',(0.,1.,0.));
#34102=DIRECTION('',(-1.,0.,0.));
#34103=DIRECTION('center_axis',(1.,0.,0.));
#34104=DIRECTION('ref_axis',(0.,0.,-1.));
#34105=DIRECTION('center_axis',(-1.,0.,0.));
#34106=DIRECTION('ref_axis',(0.,0.,1.));
#34107=DIRECTION('center_axis',(1.,0.,0.));
#34108=DIRECTION('ref_axis',(0.,0.,-1.));
#34109=DIRECTION('center_axis',(1.,0.,0.));
#34110=DIRECTION('ref_axis',(0.,1.,0.));
#34111=DIRECTION('',(-1.,0.,0.));
#34112=DIRECTION('center_axis',(1.,0.,0.));
#34113=DIRECTION('ref_axis',(0.,0.,-1.));
#34114=DIRECTION('center_axis',(1.,0.,0.));
#34115=DIRECTION('ref_axis',(0.,0.,-1.));
#34116=DIRECTION('axis',(0.,0.,1.));
#34117=DIRECTION('refdir',(1.,0.,0.));
#34118=DIRECTION('center_axis',(0.,0.,1.));
#34119=DIRECTION('ref_axis',(1.,0.,0.));
#34120=DIRECTION('',(0.,0.,-1.));
#34121=DIRECTION('center_axis',(0.,0.,1.));
#34122=DIRECTION('ref_axis',(1.,0.,0.));
#34123=DIRECTION('center_axis',(0.,0.,1.));
#34124=DIRECTION('ref_axis',(1.,0.,0.));
#34125=DIRECTION('',(0.,0.,-1.));
#34126=DIRECTION('center_axis',(0.,0.,1.));
#34127=DIRECTION('ref_axis',(1.,0.,0.));
#34128=DIRECTION('',(0.,0.,-1.));
#34129=DIRECTION('center_axis',(0.,0.,1.));
#34130=DIRECTION('ref_axis',(1.,0.,0.));
#34131=DIRECTION('',(0.,0.,-1.));
#34132=DIRECTION('center_axis',(0.,0.,1.));
#34133=DIRECTION('ref_axis',(1.,0.,0.));
#34134=DIRECTION('',(0.,0.,-1.));
#34135=DIRECTION('center_axis',(0.,0.,1.));
#34136=DIRECTION('ref_axis',(1.,0.,0.));
#34137=DIRECTION('',(0.,0.,-1.));
#34138=DIRECTION('center_axis',(0.,0.,1.));
#34139=DIRECTION('ref_axis',(1.,0.,0.));
#34140=DIRECTION('',(0.,0.,-1.));
#34141=DIRECTION('center_axis',(0.,0.,1.));
#34142=DIRECTION('ref_axis',(1.,0.,0.));
#34143=DIRECTION('',(0.,0.,-1.));
#34144=DIRECTION('center_axis',(0.,0.,1.));
#34145=DIRECTION('ref_axis',(1.,0.,0.));
#34146=DIRECTION('',(0.,0.,-1.));
#34147=DIRECTION('center_axis',(0.,0.,1.));
#34148=DIRECTION('ref_axis',(1.,0.,0.));
#34149=DIRECTION('',(0.,0.,-1.));
#34150=DIRECTION('center_axis',(0.,0.,1.));
#34151=DIRECTION('ref_axis',(1.,0.,0.));
#34152=DIRECTION('',(0.,0.,-1.));
#34153=DIRECTION('center_axis',(0.,0.,1.));
#34154=DIRECTION('ref_axis',(1.,0.,0.));
#34155=DIRECTION('',(0.,0.,-1.));
#34156=DIRECTION('center_axis',(0.,0.,1.));
#34157=DIRECTION('ref_axis',(1.,0.,0.));
#34158=DIRECTION('',(0.,0.,-1.));
#34159=DIRECTION('center_axis',(0.,0.,1.));
#34160=DIRECTION('ref_axis',(1.,0.,0.));
#34161=DIRECTION('',(0.,0.,-1.));
#34162=DIRECTION('center_axis',(0.,0.,1.));
#34163=DIRECTION('ref_axis',(1.,0.,0.));
#34164=DIRECTION('',(0.,0.,-1.));
#34165=DIRECTION('center_axis',(0.,0.,1.));
#34166=DIRECTION('ref_axis',(1.,0.,0.));
#34167=DIRECTION('',(0.,0.,-1.));
#34168=DIRECTION('center_axis',(0.,0.,1.));
#34169=DIRECTION('ref_axis',(1.,0.,0.));
#34170=DIRECTION('',(0.,0.,-1.));
#34171=DIRECTION('center_axis',(0.,0.,1.));
#34172=DIRECTION('ref_axis',(1.,0.,0.));
#34173=DIRECTION('',(0.,0.,-1.));
#34174=DIRECTION('center_axis',(0.,0.,1.));
#34175=DIRECTION('ref_axis',(1.,0.,0.));
#34176=DIRECTION('',(0.,0.,-1.));
#34177=DIRECTION('center_axis',(0.,0.,1.));
#34178=DIRECTION('ref_axis',(1.,0.,0.));
#34179=DIRECTION('',(0.,0.,-1.));
#34180=DIRECTION('center_axis',(0.,0.,1.));
#34181=DIRECTION('ref_axis',(1.,0.,0.));
#34182=DIRECTION('',(0.,0.,-1.));
#34183=DIRECTION('center_axis',(0.,0.,1.));
#34184=DIRECTION('ref_axis',(1.,0.,0.));
#34185=DIRECTION('',(0.,0.,-1.));
#34186=DIRECTION('center_axis',(0.,0.,1.));
#34187=DIRECTION('ref_axis',(1.,0.,0.));
#34188=DIRECTION('',(0.,0.,-1.));
#34189=DIRECTION('center_axis',(0.,0.,1.));
#34190=DIRECTION('ref_axis',(0.960739260171429,-0.277452831964742,0.));
#34191=DIRECTION('',(0.,0.,1.));
#34192=DIRECTION('center_axis',(0.,0.,1.));
#34193=DIRECTION('ref_axis',(1.,2.16645715620364E-14,0.));
#34194=DIRECTION('center_axis',(0.,0.,1.));
#34195=DIRECTION('ref_axis',(1.,2.16645715620364E-14,0.));
#34196=DIRECTION('',(0.,0.,1.));
#34197=DIRECTION('center_axis',(0.,0.,1.));
#34198=DIRECTION('ref_axis',(1.,2.16645715620364E-14,0.));
#34199=DIRECTION('',(0.,0.,1.));
#34200=DIRECTION('center_axis',(0.,0.,1.));
#34201=DIRECTION('ref_axis',(1.,2.16645715620364E-14,0.));
#34202=DIRECTION('',(0.,0.,1.));
#34203=DIRECTION('center_axis',(0.,0.,1.));
#34204=DIRECTION('ref_axis',(1.,2.16645715620364E-14,0.));
#34205=DIRECTION('',(0.,0.,1.));
#34206=DIRECTION('center_axis',(0.,0.,1.));
#34207=DIRECTION('ref_axis',(1.,2.16645715620364E-14,0.));
#34208=DIRECTION('',(0.,0.,1.));
#34209=DIRECTION('center_axis',(0.,0.,1.));
#34210=DIRECTION('ref_axis',(1.,2.16645715620364E-14,0.));
#34211=DIRECTION('',(0.,0.,1.));
#34212=DIRECTION('center_axis',(0.,0.,1.));
#34213=DIRECTION('ref_axis',(1.,2.16645715620364E-14,0.));
#34214=DIRECTION('',(0.,0.,1.));
#34215=DIRECTION('center_axis',(0.,0.,1.));
#34216=DIRECTION('ref_axis',(1.,2.16645715620364E-14,0.));
#34217=DIRECTION('',(0.,0.,1.));
#34218=DIRECTION('center_axis',(0.,0.,1.));
#34219=DIRECTION('ref_axis',(1.,2.16645715620364E-14,0.));
#34220=DIRECTION('',(0.,0.,1.));
#34221=DIRECTION('center_axis',(0.,0.,1.));
#34222=DIRECTION('ref_axis',(1.,2.16645715620364E-14,0.));
#34223=DIRECTION('',(0.,0.,1.));
#34224=DIRECTION('center_axis',(0.,0.,1.));
#34225=DIRECTION('ref_axis',(1.,2.16645715620364E-14,0.));
#34226=DIRECTION('',(0.,0.,1.));
#34227=DIRECTION('center_axis',(0.,0.,1.));
#34228=DIRECTION('ref_axis',(1.,2.16645715620364E-14,0.));
#34229=DIRECTION('',(0.,0.,1.));
#34230=DIRECTION('center_axis',(0.,0.,1.));
#34231=DIRECTION('ref_axis',(1.,2.16645715620364E-14,0.));
#34232=DIRECTION('',(0.,0.,1.));
#34233=DIRECTION('center_axis',(0.,0.,1.));
#34234=DIRECTION('ref_axis',(1.,2.16645715620364E-14,0.));
#34235=DIRECTION('',(0.,0.,1.));
#34236=DIRECTION('center_axis',(0.,0.,1.));
#34237=DIRECTION('ref_axis',(1.,2.16645715620364E-14,0.));
#34238=DIRECTION('',(0.,0.,1.));
#34239=DIRECTION('center_axis',(0.,0.,1.));
#34240=DIRECTION('ref_axis',(1.,2.16645715620364E-14,0.));
#34241=DIRECTION('',(0.,0.,1.));
#34242=DIRECTION('center_axis',(0.,0.,1.));
#34243=DIRECTION('ref_axis',(1.,2.16645715620364E-14,0.));
#34244=DIRECTION('',(0.,0.,1.));
#34245=DIRECTION('center_axis',(0.,0.,1.));
#34246=DIRECTION('ref_axis',(1.,2.16645715620364E-14,0.));
#34247=DIRECTION('',(0.,0.,1.));
#34248=DIRECTION('center_axis',(0.,0.,1.));
#34249=DIRECTION('ref_axis',(1.,2.16645715620364E-14,0.));
#34250=DIRECTION('',(0.,0.,1.));
#34251=DIRECTION('center_axis',(0.,0.,1.));
#34252=DIRECTION('ref_axis',(1.,2.16645715620364E-14,0.));
#34253=DIRECTION('',(0.,0.,1.));
#34254=DIRECTION('center_axis',(0.,0.,1.));
#34255=DIRECTION('ref_axis',(1.,2.16645715620364E-14,0.));
#34256=DIRECTION('',(0.,0.,1.));
#34257=DIRECTION('center_axis',(0.,0.,1.));
#34258=DIRECTION('ref_axis',(1.,0.,0.));
#34259=DIRECTION('center_axis',(0.,0.,1.));
#34260=DIRECTION('ref_axis',(1.,0.,0.));
#34261=DIRECTION('center_axis',(0.,0.,1.));
#34262=DIRECTION('ref_axis',(1.,0.,0.));
#34263=DIRECTION('center_axis',(0.,0.,-1.));
#34264=DIRECTION('ref_axis',(1.,2.16645715620364E-14,0.));
#34265=DIRECTION('center_axis',(0.,0.,1.));
#34266=DIRECTION('ref_axis',(0.889074692313968,0.457762156022997,0.));
#34267=DIRECTION('center_axis',(0.,0.,-1.));
#34268=DIRECTION('ref_axis',(1.,0.,0.));
#34269=DIRECTION('',(0.866025403784439,1.06057523872491E-16,0.5));
#34270=DIRECTION('center_axis',(0.,0.,1.));
#34271=DIRECTION('ref_axis',(1.,0.,0.));
#34272=DIRECTION('center_axis',(-0.5,0.866025403784439,0.));
#34273=DIRECTION('ref_axis',(-0.866025403784439,-0.5,0.));
#34274=DIRECTION('',(0.,0.,1.));
#34275=DIRECTION('',(-0.866025403784439,-0.5,0.));
#34276=DIRECTION('',(0.,0.,1.));
#34277=DIRECTION('center_axis',(0.5,0.866025403784439,0.));
#34278=DIRECTION('ref_axis',(-0.866025403784439,0.5,0.));
#34279=DIRECTION('',(0.,0.,1.));
#34280=DIRECTION('',(-0.866025403784439,0.5,0.));
#34281=DIRECTION('center_axis',(1.,-2.13662520709285E-16,0.));
#34282=DIRECTION('ref_axis',(2.13662520709285E-16,1.,0.));
#34283=DIRECTION('',(0.,0.,1.));
#34284=DIRECTION('',(2.13662520709285E-16,1.,0.));
#34285=DIRECTION('center_axis',(0.,0.,1.));
#34286=DIRECTION('ref_axis',(1.,0.,0.));
#34287=DIRECTION('',(0.866025403784439,0.5,0.));
#34288=DIRECTION('',(0.866025403784439,-0.5,0.));
#34289=DIRECTION('',(0.,-1.,0.));
#34290=DIRECTION('center_axis',(0.,0.,1.));
#34291=DIRECTION('ref_axis',(1.,0.,0.));
#34292=DIRECTION('center_axis',(0.5,-0.866025403784439,0.));
#34293=DIRECTION('ref_axis',(0.866025403784439,0.5,0.));
#34294=DIRECTION('',(0.,0.,1.));
#34295=DIRECTION('center_axis',(-0.5,-0.866025403784439,0.));
#34296=DIRECTION('ref_axis',(0.866025403784439,-0.5,0.));
#34297=DIRECTION('',(0.,0.,1.));
#34298=DIRECTION('center_axis',(-1.,0.,0.));
#34299=DIRECTION('ref_axis',(0.,-1.,0.));
#34300=DIRECTION('center_axis',(0.,0.,1.));
#34301=DIRECTION('ref_axis',(1.,0.,0.));
#34302=DIRECTION('center_axis',(0.,0.,-1.));
#34303=DIRECTION('ref_axis',(-1.,0.,0.));
#34304=DIRECTION('center_axis',(0.,0.,1.));
#34305=DIRECTION('ref_axis',(1.,0.,0.));
#34306=DIRECTION('center_axis',(0.,0.,1.));
#34307=DIRECTION('ref_axis',(1.,0.,0.));
#34308=DIRECTION('',(0.707106781186547,8.65956056235493E-17,-0.707106781186548));
#34309=DIRECTION('center_axis',(0.,0.,1.));
#34310=DIRECTION('ref_axis',(-0.357033271046359,-0.934091667539079,0.));
#34311=DIRECTION('center_axis',(0.,0.,1.));
#34312=DIRECTION('ref_axis',(1.,0.,0.));
#34313=DIRECTION('center_axis',(0.,0.,-1.));
#34314=DIRECTION('ref_axis',(-1.,0.,0.));
#34315=DIRECTION('center_axis',(0.,0.,1.));
#34316=DIRECTION('ref_axis',(1.,0.,0.));
#34317=DIRECTION('center_axis',(0.,0.,1.));
#34318=DIRECTION('ref_axis',(1.,0.,0.));
#34319=DIRECTION('',(0.,0.,-1.));
#34320=DIRECTION('axis',(0.,0.,1.));
#34321=DIRECTION('refdir',(1.,0.,0.));
#34322=DIRECTION('center_axis',(0.,0.,1.));
#34323=DIRECTION('ref_axis',(1.,0.,0.));
#34324=DIRECTION('',(0.,0.,-1.));
#34325=DIRECTION('center_axis',(0.,0.,1.));
#34326=DIRECTION('ref_axis',(1.,0.,0.));
#34327=DIRECTION('center_axis',(0.,0.,1.));
#34328=DIRECTION('ref_axis',(1.,0.,0.));
#34329=DIRECTION('',(0.,0.,-1.));
#34330=DIRECTION('center_axis',(0.,0.,1.));
#34331=DIRECTION('ref_axis',(1.,0.,0.));
#34332=DIRECTION('',(0.,0.,-1.));
#34333=DIRECTION('center_axis',(0.,0.,1.));
#34334=DIRECTION('ref_axis',(1.,0.,0.));
#34335=DIRECTION('',(0.,0.,-1.));
#34336=DIRECTION('center_axis',(0.,0.,1.));
#34337=DIRECTION('ref_axis',(1.,0.,0.));
#34338=DIRECTION('',(0.,0.,-1.));
#34339=DIRECTION('center_axis',(0.,0.,1.));
#34340=DIRECTION('ref_axis',(1.,0.,0.));
#34341=DIRECTION('',(0.,0.,-1.));
#34342=DIRECTION('center_axis',(0.,0.,1.));
#34343=DIRECTION('ref_axis',(1.,0.,0.));
#34344=DIRECTION('',(0.,0.,-1.));
#34345=DIRECTION('center_axis',(0.,0.,1.));
#34346=DIRECTION('ref_axis',(1.,0.,0.));
#34347=DIRECTION('',(0.,0.,-1.));
#34348=DIRECTION('center_axis',(0.,0.,1.));
#34349=DIRECTION('ref_axis',(1.,0.,0.));
#34350=DIRECTION('',(0.,0.,-1.));
#34351=DIRECTION('center_axis',(0.,0.,1.));
#34352=DIRECTION('ref_axis',(1.,0.,0.));
#34353=DIRECTION('',(0.,0.,-1.));
#34354=DIRECTION('center_axis',(0.,0.,1.));
#34355=DIRECTION('ref_axis',(1.,0.,0.));
#34356=DIRECTION('',(0.,0.,-1.));
#34357=DIRECTION('center_axis',(0.,0.,1.));
#34358=DIRECTION('ref_axis',(1.,0.,0.));
#34359=DIRECTION('',(0.,0.,-1.));
#34360=DIRECTION('center_axis',(0.,0.,1.));
#34361=DIRECTION('ref_axis',(1.,0.,0.));
#34362=DIRECTION('',(0.,0.,-1.));
#34363=DIRECTION('center_axis',(0.,0.,1.));
#34364=DIRECTION('ref_axis',(1.,0.,0.));
#34365=DIRECTION('',(0.,0.,-1.));
#34366=DIRECTION('center_axis',(0.,0.,1.));
#34367=DIRECTION('ref_axis',(1.,0.,0.));
#34368=DIRECTION('',(0.,0.,-1.));
#34369=DIRECTION('center_axis',(0.,0.,1.));
#34370=DIRECTION('ref_axis',(1.,0.,0.));
#34371=DIRECTION('',(0.,0.,-1.));
#34372=DIRECTION('center_axis',(0.,0.,1.));
#34373=DIRECTION('ref_axis',(1.,0.,0.));
#34374=DIRECTION('',(0.,0.,-1.));
#34375=DIRECTION('center_axis',(0.,0.,1.));
#34376=DIRECTION('ref_axis',(1.,0.,0.));
#34377=DIRECTION('',(0.,0.,-1.));
#34378=DIRECTION('center_axis',(0.,0.,1.));
#34379=DIRECTION('ref_axis',(1.,0.,0.));
#34380=DIRECTION('',(0.,0.,-1.));
#34381=DIRECTION('center_axis',(0.,0.,1.));
#34382=DIRECTION('ref_axis',(1.,0.,0.));
#34383=DIRECTION('',(0.,0.,-1.));
#34384=DIRECTION('center_axis',(0.,0.,1.));
#34385=DIRECTION('ref_axis',(1.,0.,0.));
#34386=DIRECTION('',(0.,0.,-1.));
#34387=DIRECTION('center_axis',(0.,0.,1.));
#34388=DIRECTION('ref_axis',(1.,0.,0.));
#34389=DIRECTION('',(0.,0.,-1.));
#34390=DIRECTION('center_axis',(0.,0.,1.));
#34391=DIRECTION('ref_axis',(1.,0.,0.));
#34392=DIRECTION('',(0.,0.,-1.));
#34393=DIRECTION('center_axis',(0.,0.,1.));
#34394=DIRECTION('ref_axis',(-0.745989836172204,-0.665957329209438,0.));
#34395=DIRECTION('',(0.,0.,1.));
#34396=DIRECTION('center_axis',(0.,0.,1.));
#34397=DIRECTION('ref_axis',(1.,2.60874502654993E-14,0.));
#34398=DIRECTION('center_axis',(0.,0.,1.));
#34399=DIRECTION('ref_axis',(1.,2.60874502654993E-14,0.));
#34400=DIRECTION('',(0.,0.,1.));
#34401=DIRECTION('center_axis',(0.,0.,1.));
#34402=DIRECTION('ref_axis',(1.,2.60874502654993E-14,0.));
#34403=DIRECTION('',(0.,0.,1.));
#34404=DIRECTION('center_axis',(0.,0.,1.));
#34405=DIRECTION('ref_axis',(1.,2.60874502654993E-14,0.));
#34406=DIRECTION('',(0.,0.,1.));
#34407=DIRECTION('center_axis',(0.,0.,1.));
#34408=DIRECTION('ref_axis',(1.,2.60874502654993E-14,0.));
#34409=DIRECTION('',(0.,0.,1.));
#34410=DIRECTION('center_axis',(0.,0.,1.));
#34411=DIRECTION('ref_axis',(1.,2.60874502654993E-14,0.));
#34412=DIRECTION('',(0.,0.,1.));
#34413=DIRECTION('center_axis',(0.,0.,1.));
#34414=DIRECTION('ref_axis',(1.,2.60874502654993E-14,0.));
#34415=DIRECTION('',(0.,0.,1.));
#34416=DIRECTION('center_axis',(0.,0.,1.));
#34417=DIRECTION('ref_axis',(1.,2.60874502654993E-14,0.));
#34418=DIRECTION('',(0.,0.,1.));
#34419=DIRECTION('center_axis',(0.,0.,1.));
#34420=DIRECTION('ref_axis',(1.,2.60874502654993E-14,0.));
#34421=DIRECTION('',(0.,0.,1.));
#34422=DIRECTION('center_axis',(0.,0.,1.));
#34423=DIRECTION('ref_axis',(1.,2.60874502654993E-14,0.));
#34424=DIRECTION('',(0.,0.,1.));
#34425=DIRECTION('center_axis',(0.,0.,1.));
#34426=DIRECTION('ref_axis',(1.,2.60874502654993E-14,0.));
#34427=DIRECTION('',(0.,0.,1.));
#34428=DIRECTION('center_axis',(0.,0.,1.));
#34429=DIRECTION('ref_axis',(1.,2.60874502654993E-14,0.));
#34430=DIRECTION('',(0.,0.,1.));
#34431=DIRECTION('center_axis',(0.,0.,1.));
#34432=DIRECTION('ref_axis',(1.,2.60874502654993E-14,0.));
#34433=DIRECTION('',(0.,0.,1.));
#34434=DIRECTION('center_axis',(0.,0.,1.));
#34435=DIRECTION('ref_axis',(1.,2.60874502654993E-14,0.));
#34436=DIRECTION('',(0.,0.,1.));
#34437=DIRECTION('center_axis',(0.,0.,1.));
#34438=DIRECTION('ref_axis',(1.,2.60874502654993E-14,0.));
#34439=DIRECTION('',(0.,0.,1.));
#34440=DIRECTION('center_axis',(0.,0.,1.));
#34441=DIRECTION('ref_axis',(1.,2.60874502654993E-14,0.));
#34442=DIRECTION('',(0.,0.,1.));
#34443=DIRECTION('center_axis',(0.,0.,1.));
#34444=DIRECTION('ref_axis',(1.,2.60874502654993E-14,0.));
#34445=DIRECTION('',(0.,0.,1.));
#34446=DIRECTION('center_axis',(0.,0.,1.));
#34447=DIRECTION('ref_axis',(1.,2.60874502654993E-14,0.));
#34448=DIRECTION('',(0.,0.,1.));
#34449=DIRECTION('center_axis',(0.,0.,1.));
#34450=DIRECTION('ref_axis',(1.,2.60874502654993E-14,0.));
#34451=DIRECTION('',(0.,0.,1.));
#34452=DIRECTION('center_axis',(0.,0.,1.));
#34453=DIRECTION('ref_axis',(1.,2.60874502654993E-14,0.));
#34454=DIRECTION('',(0.,0.,1.));
#34455=DIRECTION('center_axis',(0.,0.,1.));
#34456=DIRECTION('ref_axis',(1.,2.60874502654993E-14,0.));
#34457=DIRECTION('',(0.,0.,1.));
#34458=DIRECTION('center_axis',(0.,0.,1.));
#34459=DIRECTION('ref_axis',(1.,2.60874502654993E-14,0.));
#34460=DIRECTION('',(0.,0.,1.));
#34461=DIRECTION('center_axis',(0.,0.,1.));
#34462=DIRECTION('ref_axis',(1.,2.60874502654993E-14,0.));
#34463=DIRECTION('',(0.,0.,1.));
#34464=DIRECTION('center_axis',(0.,0.,1.));
#34465=DIRECTION('ref_axis',(1.,0.,0.));
#34466=DIRECTION('center_axis',(0.,0.,1.));
#34467=DIRECTION('ref_axis',(1.,0.,0.));
#34468=DIRECTION('center_axis',(0.,0.,1.));
#34469=DIRECTION('ref_axis',(1.,0.,0.));
#34470=DIRECTION('center_axis',(0.,0.,1.));
#34471=DIRECTION('ref_axis',(1.,0.,0.));
#34472=DIRECTION('center_axis',(0.,0.,1.));
#34473=DIRECTION('ref_axis',(1.,0.,0.));
#34474=DIRECTION('center_axis',(0.,0.,1.));
#34475=DIRECTION('ref_axis',(1.,0.,0.));
#34476=DIRECTION('center_axis',(0.,0.,-1.));
#34477=DIRECTION('ref_axis',(1.,2.60874502654993E-14,0.));
#34478=DIRECTION('center_axis',(0.,0.,1.));
#34479=DIRECTION('ref_axis',(1.,2.60874502654993E-14,0.));
#34480=DIRECTION('center_axis',(0.,0.,1.));
#34481=DIRECTION('ref_axis',(1.,0.,0.));
#34482=DIRECTION('center_axis',(1.22464679914735E-16,-1.,0.));
#34483=DIRECTION('ref_axis',(-1.,-1.22464679914735E-16,0.));
#34484=DIRECTION('center_axis',(0.,0.,-1.));
#34485=DIRECTION('ref_axis',(1.,0.,0.));
#34486=DIRECTION('center_axis',(0.,0.,1.));
#34487=DIRECTION('ref_axis',(1.,0.,0.));
#34488=DIRECTION('center_axis',(0.,0.,1.));
#34489=DIRECTION('ref_axis',(0.602919366379948,-0.797802129380463,0.));
#34490=DIRECTION('center_axis',(0.,0.,-1.));
#34491=DIRECTION('ref_axis',(-1.,0.,0.));
#34492=DIRECTION('center_axis',(0.,0.,1.));
#34493=DIRECTION('ref_axis',(1.,0.,0.));
#34494=DIRECTION('center_axis',(0.,0.,1.));
#34495=DIRECTION('ref_axis',(1.,0.,0.));
#34496=DIRECTION('',(0.5,-0.866025403784439,0.));
#34497=DIRECTION('center_axis',(0.,0.,1.));
#34498=DIRECTION('ref_axis',(1.,0.,0.));
#34499=DIRECTION('center_axis',(0.,0.,1.));
#34500=DIRECTION('ref_axis',(1.,0.,0.));
#34501=DIRECTION('',(-0.5,-0.866025403784439,0.));
#34502=DIRECTION('center_axis',(0.,0.,1.));
#34503=DIRECTION('ref_axis',(1.,0.,0.));
#34504=DIRECTION('center_axis',(0.,0.,1.));
#34505=DIRECTION('ref_axis',(1.,0.,0.));
#34506=DIRECTION('',(-1.,2.40370335797945E-16,0.));
#34507=DIRECTION('center_axis',(0.,0.,1.));
#34508=DIRECTION('ref_axis',(1.,0.,0.));
#34509=DIRECTION('center_axis',(0.,0.,1.));
#34510=DIRECTION('ref_axis',(1.,0.,0.));
#34511=DIRECTION('',(-0.5,0.866025403784439,0.));
#34512=DIRECTION('center_axis',(0.,0.,1.));
#34513=DIRECTION('ref_axis',(1.,0.,0.));
#34514=DIRECTION('center_axis',(0.,0.,1.));
#34515=DIRECTION('ref_axis',(1.,0.,0.));
#34516=DIRECTION('',(0.5,0.866025403784439,0.));
#34517=DIRECTION('center_axis',(0.,0.,1.));
#34518=DIRECTION('ref_axis',(1.,0.,0.));
#34519=DIRECTION('center_axis',(0.,0.,1.));
#34520=DIRECTION('ref_axis',(1.,0.,0.));
#34521=DIRECTION('',(1.,-1.20185167898973E-16,0.));
#34522=DIRECTION('center_axis',(0.,0.,1.));
#34523=DIRECTION('ref_axis',(1.,0.,0.));
#34524=DIRECTION('center_axis',(0.,0.,1.));
#34525=DIRECTION('ref_axis',(1.,0.,0.));
#34526=DIRECTION('',(-0.857492925712544,-1.05012596676537E-16,0.514495755427527));
#34527=DIRECTION('center_axis',(0.866025403784439,0.5,0.));
#34528=DIRECTION('ref_axis',(0.5,-0.866025403784439,0.));
#34529=DIRECTION('',(0.5,-0.866025403784439,0.));
#34530=DIRECTION('',(0.,0.,-1.));
#34531=DIRECTION('',(0.,0.,-1.));
#34532=DIRECTION('center_axis',(1.20185167898973E-16,1.,0.));
#34533=DIRECTION('ref_axis',(1.,-1.20185167898973E-16,0.));
#34534=DIRECTION('',(1.,-1.20185167898973E-16,0.));
#34535=DIRECTION('',(0.,0.,-1.));
#34536=DIRECTION('center_axis',(-0.866025403784439,0.5,0.));
#34537=DIRECTION('ref_axis',(0.5,0.866025403784439,0.));
#34538=DIRECTION('',(0.5,0.866025403784439,0.));
#34539=DIRECTION('',(0.,0.,-1.));
#34540=DIRECTION('center_axis',(-0.866025403784439,-0.5,0.));
#34541=DIRECTION('ref_axis',(-0.5,0.866025403784439,0.));
#34542=DIRECTION('',(-0.5,0.866025403784439,0.));
#34543=DIRECTION('',(0.,0.,-1.));
#34544=DIRECTION('center_axis',(-2.40370335797945E-16,-1.,0.));
#34545=DIRECTION('ref_axis',(-1.,2.40370335797945E-16,0.));
#34546=DIRECTION('',(-1.,2.40370335797945E-16,0.));
#34547=DIRECTION('',(0.,0.,-1.));
#34548=DIRECTION('center_axis',(0.866025403784439,-0.5,0.));
#34549=DIRECTION('ref_axis',(-0.5,-0.866025403784439,0.));
#34550=DIRECTION('',(-0.5,-0.866025403784439,0.));
#34551=DIRECTION('center_axis',(-0.836392077301054,-0.548131638411821,0.));
#34552=DIRECTION('ref_axis',(-0.548131638411821,0.836392077301054,0.));
#34553=DIRECTION('',(0.,0.,1.));
#34554=DIRECTION('',(-0.548131638411821,0.836392077301054,0.));
#34555=DIRECTION('',(0.,0.,-1.));
#34556=DIRECTION('',(-0.548131638411821,0.836392077301054,0.));
#34557=DIRECTION('center_axis',(0.,0.,1.));
#34558=DIRECTION('ref_axis',(1.,0.,0.));
#34559=DIRECTION('center_axis',(0.,0.,1.));
#34560=DIRECTION('ref_axis',(1.,0.,0.));
#34561=DIRECTION('',(0.957515659832182,0.288381277436904,0.));
#34562=DIRECTION('center_axis',(-0.288381277436904,0.957515659832182,0.));
#34563=DIRECTION('ref_axis',(0.957515659832182,0.288381277436904,0.));
#34564=DIRECTION('',(0.,0.,-1.));
#34565=DIRECTION('',(0.957515659832182,0.288381277436904,0.));
#34566=DIRECTION('center_axis',(0.,0.,-1.));
#34567=DIRECTION('ref_axis',(-1.,0.,0.));
#34568=DIRECTION('center_axis',(0.,0.,-1.));
#34569=DIRECTION('ref_axis',(1.,0.,0.));
#34570=DIRECTION('center_axis',(-0.973423524654541,-0.229012317679924,0.));
#34571=DIRECTION('ref_axis',(-0.229012317679924,0.973423524654541,0.));
#34572=DIRECTION('',(0.,0.,1.));
#34573=DIRECTION('',(-0.229012317679924,0.973423524654541,0.));
#34574=DIRECTION('',(0.,0.,-1.));
#34575=DIRECTION('',(-0.229012317679924,0.973423524654541,0.));
#34576=DIRECTION('center_axis',(0.,0.,1.));
#34577=DIRECTION('ref_axis',(1.,0.,0.));
#34578=DIRECTION('center_axis',(0.,0.,1.));
#34579=DIRECTION('ref_axis',(1.,0.,0.));
#34580=DIRECTION('',(0.998402605672661,-0.0564998848320951,0.));
#34581=DIRECTION('center_axis',(0.0564998848320951,0.998402605672661,0.));
#34582=DIRECTION('ref_axis',(0.998402605672661,-0.0564998848320951,0.));
#34583=DIRECTION('',(0.,0.,-1.));
#34584=DIRECTION('',(0.998402605672661,-0.0564998848320951,0.));
#34585=DIRECTION('center_axis',(0.,0.,-1.));
#34586=DIRECTION('ref_axis',(-1.,0.,0.));
#34587=DIRECTION('center_axis',(0.,0.,-1.));
#34588=DIRECTION('ref_axis',(1.,0.,0.));
#34589=DIRECTION('center_axis',(-0.993045728733512,0.117729268426028,0.));
#34590=DIRECTION('ref_axis',(0.117729268426028,0.993045728733512,0.));
#34591=DIRECTION('',(0.,0.,1.));
#34592=DIRECTION('',(0.117729268426028,0.993045728733512,0.));
#34593=DIRECTION('',(0.,0.,-1.));
#34594=DIRECTION('',(0.117729268426028,0.993045728733512,0.));
#34595=DIRECTION('center_axis',(0.,0.,1.));
#34596=DIRECTION('ref_axis',(1.,0.,0.));
#34597=DIRECTION('center_axis',(0.,0.,1.));
#34598=DIRECTION('ref_axis',(1.,0.,0.));
#34599=DIRECTION('',(0.918867462415862,-0.394566327140867,0.));
#34600=DIRECTION('center_axis',(0.394566327140867,0.918867462415862,0.));
#34601=DIRECTION('ref_axis',(0.918867462415862,-0.394566327140867,0.));
#34602=DIRECTION('',(0.,0.,-1.));
#34603=DIRECTION('',(0.918867462415862,-0.394566327140867,0.));
#34604=DIRECTION('center_axis',(0.,0.,-1.));
#34605=DIRECTION('ref_axis',(-1.,0.,0.));
#34606=DIRECTION('center_axis',(0.,0.,-1.));
#34607=DIRECTION('ref_axis',(1.,0.,0.));
#34608=DIRECTION('center_axis',(-0.892891962133153,0.450270967260834,0.));
#34609=DIRECTION('ref_axis',(0.450270967260834,0.892891962133153,0.));
#34610=DIRECTION('',(0.,0.,1.));
#34611=DIRECTION('',(0.450270967260834,0.892891962133153,0.));
#34612=DIRECTION('',(0.,0.,-1.));
#34613=DIRECTION('',(0.450270967260834,0.892891962133153,0.));
#34614=DIRECTION('center_axis',(0.,0.,1.));
#34615=DIRECTION('ref_axis',(1.,0.,0.));
#34616=DIRECTION('center_axis',(0.,0.,1.));
#34617=DIRECTION('ref_axis',(1.,0.,0.));
#34618=DIRECTION('',(0.728503342152264,-0.685042247217631,0.));
#34619=DIRECTION('center_axis',(0.685042247217631,0.728503342152264,0.));
#34620=DIRECTION('ref_axis',(0.728503342152264,-0.685042247217631,0.));
#34621=DIRECTION('',(0.,0.,-1.));
#34622=DIRECTION('',(0.728503342152264,-0.685042247217631,0.));
#34623=DIRECTION('center_axis',(0.,0.,-1.));
#34624=DIRECTION('ref_axis',(-1.,0.,0.));
#34625=DIRECTION('center_axis',(0.,0.,-1.));
#34626=DIRECTION('ref_axis',(1.,0.,0.));
#34627=DIRECTION('center_axis',(-0.685042247217632,0.728503342152263,0.));
#34628=DIRECTION('ref_axis',(0.728503342152263,0.685042247217632,0.));
#34629=DIRECTION('',(0.,0.,1.));
#34630=DIRECTION('',(0.728503342152263,0.685042247217632,0.));
#34631=DIRECTION('',(0.,0.,-1.));
#34632=DIRECTION('',(0.728503342152263,0.685042247217632,0.));
#34633=DIRECTION('center_axis',(0.,0.,1.));
#34634=DIRECTION('ref_axis',(1.,0.,0.));
#34635=DIRECTION('center_axis',(0.,0.,1.));
#34636=DIRECTION('ref_axis',(1.,0.,0.));
#34637=DIRECTION('',(0.450270967260841,-0.89289196213315,0.));
#34638=DIRECTION('center_axis',(0.89289196213315,0.450270967260841,0.));
#34639=DIRECTION('ref_axis',(0.450270967260841,-0.89289196213315,0.));
#34640=DIRECTION('',(0.,0.,-1.));
#34641=DIRECTION('',(0.450270967260841,-0.89289196213315,0.));
#34642=DIRECTION('center_axis',(0.,0.,-1.));
#34643=DIRECTION('ref_axis',(-1.,0.,0.));
#34644=DIRECTION('center_axis',(0.,0.,-1.));
#34645=DIRECTION('ref_axis',(1.,0.,0.));
#34646=DIRECTION('center_axis',(-0.394566327140866,0.918867462415863,0.));
#34647=DIRECTION('ref_axis',(0.918867462415863,0.394566327140866,0.));
#34648=DIRECTION('',(0.,0.,1.));
#34649=DIRECTION('',(0.918867462415863,0.394566327140866,0.));
#34650=DIRECTION('',(0.,0.,-1.));
#34651=DIRECTION('',(0.918867462415863,0.394566327140866,0.));
#34652=DIRECTION('center_axis',(0.,0.,1.));
#34653=DIRECTION('ref_axis',(1.,0.,0.));
#34654=DIRECTION('center_axis',(0.,0.,1.));
#34655=DIRECTION('ref_axis',(1.,0.,0.));
#34656=DIRECTION('',(0.117729268426029,-0.993045728733512,0.));
#34657=DIRECTION('center_axis',(0.993045728733512,0.117729268426029,0.));
#34658=DIRECTION('ref_axis',(0.117729268426029,-0.993045728733512,0.));
#34659=DIRECTION('',(0.,0.,-1.));
#34660=DIRECTION('',(0.117729268426029,-0.993045728733512,0.));
#34661=DIRECTION('center_axis',(0.,0.,-1.));
#34662=DIRECTION('ref_axis',(-1.,0.,0.));
#34663=DIRECTION('center_axis',(0.,0.,-1.));
#34664=DIRECTION('ref_axis',(1.,0.,0.));
#34665=DIRECTION('center_axis',(-0.0564998848320997,0.998402605672661,0.));
#34666=DIRECTION('ref_axis',(0.998402605672661,0.0564998848320997,0.));
#34667=DIRECTION('',(0.,0.,1.));
#34668=DIRECTION('',(0.998402605672661,0.0564998848320997,0.));
#34669=DIRECTION('',(0.,0.,-1.));
#34670=DIRECTION('',(0.998402605672661,0.0564998848320997,0.));
#34671=DIRECTION('center_axis',(0.,0.,1.));
#34672=DIRECTION('ref_axis',(1.,0.,0.));
#34673=DIRECTION('center_axis',(0.,0.,1.));
#34674=DIRECTION('ref_axis',(1.,0.,0.));
#34675=DIRECTION('',(-0.229012317679922,-0.973423524654541,0.));
#34676=DIRECTION('center_axis',(0.973423524654541,-0.229012317679922,0.));
#34677=DIRECTION('ref_axis',(-0.229012317679922,-0.973423524654541,0.));
#34678=DIRECTION('',(0.,0.,-1.));
#34679=DIRECTION('',(-0.229012317679922,-0.973423524654541,0.));
#34680=DIRECTION('center_axis',(0.,0.,-1.));
#34681=DIRECTION('ref_axis',(-1.,0.,0.));
#34682=DIRECTION('center_axis',(0.,0.,-1.));
#34683=DIRECTION('ref_axis',(1.,0.,0.));
#34684=DIRECTION('center_axis',(0.288381277436907,0.957515659832181,0.));
#34685=DIRECTION('ref_axis',(0.957515659832181,-0.288381277436907,0.));
#34686=DIRECTION('',(0.,0.,1.));
#34687=DIRECTION('',(0.957515659832181,-0.288381277436907,0.));
#34688=DIRECTION('',(0.,0.,-1.));
#34689=DIRECTION('',(0.957515659832181,-0.288381277436907,0.));
#34690=DIRECTION('center_axis',(0.,0.,1.));
#34691=DIRECTION('ref_axis',(1.,0.,0.));
#34692=DIRECTION('center_axis',(0.,0.,1.));
#34693=DIRECTION('ref_axis',(1.,0.,0.));
#34694=DIRECTION('',(-0.548131638411824,-0.836392077301052,0.));
#34695=DIRECTION('center_axis',(0.836392077301052,-0.548131638411824,0.));
#34696=DIRECTION('ref_axis',(-0.548131638411824,-0.836392077301052,0.));
#34697=DIRECTION('',(0.,0.,-1.));
#34698=DIRECTION('',(-0.548131638411824,-0.836392077301052,0.));
#34699=DIRECTION('center_axis',(0.,0.,-1.));
#34700=DIRECTION('ref_axis',(-1.,0.,0.));
#34701=DIRECTION('center_axis',(0.,0.,-1.));
#34702=DIRECTION('ref_axis',(1.,0.,0.));
#34703=DIRECTION('center_axis',(0.598479401592652,0.801138193989839,0.));
#34704=DIRECTION('ref_axis',(0.801138193989839,-0.598479401592652,0.));
#34705=DIRECTION('',(0.,0.,1.));
#34706=DIRECTION('',(0.801138193989839,-0.598479401592652,0.));
#34707=DIRECTION('',(0.,0.,-1.));
#34708=DIRECTION('',(0.801138193989839,-0.598479401592652,0.));
#34709=DIRECTION('center_axis',(0.,0.,1.));
#34710=DIRECTION('ref_axis',(1.,0.,0.));
#34711=DIRECTION('center_axis',(0.,0.,1.));
#34712=DIRECTION('ref_axis',(1.,0.,0.));
#34713=DIRECTION('',(-0.801138193989839,-0.598479401592652,0.));
#34714=DIRECTION('center_axis',(0.,0.,1.));
#34715=DIRECTION('ref_axis',(1.,0.,0.));
#34716=DIRECTION('center_axis',(0.598479401592652,-0.801138193989839,0.));
#34717=DIRECTION('ref_axis',(-0.801138193989839,-0.598479401592652,0.));
#34718=DIRECTION('',(0.,0.,-1.));
#34719=DIRECTION('',(-0.801138193989839,-0.598479401592652,0.));
#34720=DIRECTION('center_axis',(0.,0.,-1.));
#34721=DIRECTION('ref_axis',(-1.,0.,0.));
#34722=DIRECTION('center_axis',(0.,0.,-1.));
#34723=DIRECTION('ref_axis',(1.,0.,0.));
#34724=DIRECTION('center_axis',(0.,0.,-1.));
#34725=DIRECTION('ref_axis',(1.,0.,0.));
#34726=DIRECTION('center_axis',(0.728503342152263,0.685042247217632,0.));
#34727=DIRECTION('ref_axis',(0.685042247217632,-0.728503342152263,0.));
#34728=DIRECTION('',(0.,0.,1.));
#34729=DIRECTION('',(0.685042247217632,-0.728503342152263,0.));
#34730=DIRECTION('',(0.,0.,-1.));
#34731=DIRECTION('',(0.685042247217632,-0.728503342152263,0.));
#34732=DIRECTION('center_axis',(0.,0.,1.));
#34733=DIRECTION('ref_axis',(1.,0.,0.));
#34734=DIRECTION('center_axis',(0.,0.,1.));
#34735=DIRECTION('ref_axis',(1.,0.,0.));
#34736=DIRECTION('',(-0.892891962133152,-0.450270967260837,0.));
#34737=DIRECTION('center_axis',(0.450270967260837,-0.892891962133152,0.));
#34738=DIRECTION('ref_axis',(-0.892891962133152,-0.450270967260837,0.));
#34739=DIRECTION('',(0.,0.,-1.));
#34740=DIRECTION('',(-0.892891962133152,-0.450270967260837,0.));
#34741=DIRECTION('center_axis',(0.,0.,-1.));
#34742=DIRECTION('ref_axis',(-1.,0.,0.));
#34743=DIRECTION('center_axis',(0.,0.,-1.));
#34744=DIRECTION('ref_axis',(1.,0.,0.));
#34745=DIRECTION('center_axis',(0.918867462415866,0.394566327140858,0.));
#34746=DIRECTION('ref_axis',(0.394566327140858,-0.918867462415866,0.));
#34747=DIRECTION('',(0.,0.,1.));
#34748=DIRECTION('',(0.394566327140858,-0.918867462415866,0.));
#34749=DIRECTION('',(0.,0.,-1.));
#34750=DIRECTION('',(0.394566327140858,-0.918867462415866,0.));
#34751=DIRECTION('center_axis',(0.,0.,1.));
#34752=DIRECTION('ref_axis',(1.,0.,0.));
#34753=DIRECTION('center_axis',(0.,0.,1.));
#34754=DIRECTION('ref_axis',(1.,0.,0.));
#34755=DIRECTION('',(-0.993045728733513,-0.117729268426025,0.));
#34756=DIRECTION('center_axis',(0.117729268426025,-0.993045728733513,0.));
#34757=DIRECTION('ref_axis',(-0.993045728733513,-0.117729268426025,0.));
#34758=DIRECTION('',(0.,0.,-1.));
#34759=DIRECTION('',(-0.993045728733513,-0.117729268426025,0.));
#34760=DIRECTION('center_axis',(0.,0.,-1.));
#34761=DIRECTION('ref_axis',(-1.,0.,0.));
#34762=DIRECTION('center_axis',(0.,0.,-1.));
#34763=DIRECTION('ref_axis',(1.,0.,0.));
#34764=DIRECTION('center_axis',(0.998402605672661,0.0564998848320982,0.));
#34765=DIRECTION('ref_axis',(0.0564998848320982,-0.998402605672661,0.));
#34766=DIRECTION('',(0.,0.,1.));
#34767=DIRECTION('',(0.0564998848320982,-0.998402605672661,0.));
#34768=DIRECTION('',(0.,0.,-1.));
#34769=DIRECTION('',(0.0564998848320982,-0.998402605672661,0.));
#34770=DIRECTION('center_axis',(0.,0.,1.));
#34771=DIRECTION('ref_axis',(1.,0.,0.));
#34772=DIRECTION('center_axis',(0.,0.,1.));
#34773=DIRECTION('ref_axis',(1.,0.,0.));
#34774=DIRECTION('',(-0.973423524654541,0.229012317679922,0.));
#34775=DIRECTION('center_axis',(-0.229012317679922,-0.973423524654541,0.));
#34776=DIRECTION('ref_axis',(-0.973423524654541,0.229012317679922,0.));
#34777=DIRECTION('',(0.,0.,-1.));
#34778=DIRECTION('',(-0.973423524654541,0.229012317679922,0.));
#34779=DIRECTION('center_axis',(0.,0.,-1.));
#34780=DIRECTION('ref_axis',(-1.,0.,0.));
#34781=DIRECTION('center_axis',(0.,0.,-1.));
#34782=DIRECTION('ref_axis',(1.,0.,0.));
#34783=DIRECTION('center_axis',(0.957515659832181,-0.288381277436909,0.));
#34784=DIRECTION('ref_axis',(-0.288381277436909,-0.957515659832181,0.));
#34785=DIRECTION('',(0.,0.,1.));
#34786=DIRECTION('',(-0.288381277436909,-0.957515659832181,0.));
#34787=DIRECTION('',(0.,0.,-1.));
#34788=DIRECTION('',(-0.288381277436909,-0.957515659832181,0.));
#34789=DIRECTION('center_axis',(0.,0.,1.));
#34790=DIRECTION('ref_axis',(1.,0.,0.));
#34791=DIRECTION('center_axis',(0.,0.,1.));
#34792=DIRECTION('ref_axis',(1.,0.,0.));
#34793=DIRECTION('',(-0.836392077301054,0.548131638411822,0.));
#34794=DIRECTION('center_axis',(-0.548131638411822,-0.836392077301054,0.));
#34795=DIRECTION('ref_axis',(-0.836392077301054,0.548131638411822,0.));
#34796=DIRECTION('',(0.,0.,-1.));
#34797=DIRECTION('',(-0.836392077301054,0.548131638411822,0.));
#34798=DIRECTION('center_axis',(0.,0.,-1.));
#34799=DIRECTION('ref_axis',(-1.,0.,0.));
#34800=DIRECTION('center_axis',(0.,0.,-1.));
#34801=DIRECTION('ref_axis',(1.,0.,0.));
#34802=DIRECTION('center_axis',(0.801138193989838,-0.598479401592653,0.));
#34803=DIRECTION('ref_axis',(-0.598479401592653,-0.801138193989838,0.));
#34804=DIRECTION('',(0.,0.,1.));
#34805=DIRECTION('',(-0.598479401592653,-0.801138193989838,0.));
#34806=DIRECTION('',(0.,0.,-1.));
#34807=DIRECTION('',(-0.598479401592653,-0.801138193989838,0.));
#34808=DIRECTION('center_axis',(0.,0.,1.));
#34809=DIRECTION('ref_axis',(1.,0.,0.));
#34810=DIRECTION('center_axis',(0.,0.,1.));
#34811=DIRECTION('ref_axis',(1.,0.,0.));
#34812=DIRECTION('',(-0.598479401592653,0.801138193989838,0.));
#34813=DIRECTION('center_axis',(-0.801138193989838,-0.598479401592653,0.));
#34814=DIRECTION('ref_axis',(-0.598479401592653,0.801138193989838,0.));
#34815=DIRECTION('',(0.,0.,-1.));
#34816=DIRECTION('',(-0.598479401592653,0.801138193989838,0.));
#34817=DIRECTION('center_axis',(0.,0.,-1.));
#34818=DIRECTION('ref_axis',(-1.,0.,0.));
#34819=DIRECTION('center_axis',(0.,0.,-1.));
#34820=DIRECTION('ref_axis',(1.,0.,0.));
#34821=DIRECTION('center_axis',(0.548131638411824,-0.836392077301052,0.));
#34822=DIRECTION('ref_axis',(-0.836392077301052,-0.548131638411824,0.));
#34823=DIRECTION('',(0.,0.,1.));
#34824=DIRECTION('',(-0.836392077301052,-0.548131638411824,0.));
#34825=DIRECTION('',(0.,0.,-1.));
#34826=DIRECTION('',(-0.836392077301052,-0.548131638411824,0.));
#34827=DIRECTION('center_axis',(0.,0.,1.));
#34828=DIRECTION('ref_axis',(1.,0.,0.));
#34829=DIRECTION('center_axis',(0.,0.,1.));
#34830=DIRECTION('ref_axis',(1.,0.,0.));
#34831=DIRECTION('',(-0.288381277436909,0.957515659832181,0.));
#34832=DIRECTION('center_axis',(-0.957515659832181,-0.288381277436909,0.));
#34833=DIRECTION('ref_axis',(-0.288381277436909,0.957515659832181,0.));
#34834=DIRECTION('',(0.,0.,-1.));
#34835=DIRECTION('',(-0.288381277436909,0.957515659832181,0.));
#34836=DIRECTION('center_axis',(0.,0.,-1.));
#34837=DIRECTION('ref_axis',(-1.,0.,0.));
#34838=DIRECTION('center_axis',(0.,0.,-1.));
#34839=DIRECTION('ref_axis',(1.,0.,0.));
#34840=DIRECTION('center_axis',(0.229012317679921,-0.973423524654542,0.));
#34841=DIRECTION('ref_axis',(-0.973423524654542,-0.229012317679921,0.));
#34842=DIRECTION('',(0.,0.,1.));
#34843=DIRECTION('',(-0.973423524654542,-0.229012317679921,0.));
#34844=DIRECTION('',(0.,0.,-1.));
#34845=DIRECTION('',(-0.973423524654542,-0.229012317679921,0.));
#34846=DIRECTION('center_axis',(0.,0.,1.));
#34847=DIRECTION('ref_axis',(1.,0.,0.));
#34848=DIRECTION('center_axis',(0.,0.,1.));
#34849=DIRECTION('ref_axis',(1.,0.,0.));
#34850=DIRECTION('',(0.0564998848320982,0.998402605672661,0.));
#34851=DIRECTION('center_axis',(-0.998402605672661,0.0564998848320982,0.));
#34852=DIRECTION('ref_axis',(0.0564998848320982,0.998402605672661,0.));
#34853=DIRECTION('',(0.,0.,-1.));
#34854=DIRECTION('',(0.0564998848320982,0.998402605672661,0.));
#34855=DIRECTION('center_axis',(0.,0.,-1.));
#34856=DIRECTION('ref_axis',(-1.,0.,0.));
#34857=DIRECTION('center_axis',(0.,0.,-1.));
#34858=DIRECTION('ref_axis',(1.,0.,0.));
#34859=DIRECTION('center_axis',(-0.117729268426025,-0.993045728733512,0.));
#34860=DIRECTION('ref_axis',(-0.993045728733512,0.117729268426025,0.));
#34861=DIRECTION('',(0.,0.,1.));
#34862=DIRECTION('',(-0.993045728733512,0.117729268426025,0.));
#34863=DIRECTION('',(0.,0.,-1.));
#34864=DIRECTION('',(-0.993045728733512,0.117729268426025,0.));
#34865=DIRECTION('center_axis',(0.,0.,1.));
#34866=DIRECTION('ref_axis',(1.,0.,0.));
#34867=DIRECTION('center_axis',(0.,0.,1.));
#34868=DIRECTION('ref_axis',(1.,0.,0.));
#34869=DIRECTION('',(0.394566327140861,0.918867462415865,0.));
#34870=DIRECTION('center_axis',(-0.918867462415865,0.394566327140861,0.));
#34871=DIRECTION('ref_axis',(0.394566327140861,0.918867462415865,0.));
#34872=DIRECTION('',(0.,0.,-1.));
#34873=DIRECTION('',(0.394566327140861,0.918867462415865,0.));
#34874=DIRECTION('center_axis',(0.,0.,-1.));
#34875=DIRECTION('ref_axis',(-1.,0.,0.));
#34876=DIRECTION('center_axis',(0.,0.,-1.));
#34877=DIRECTION('ref_axis',(1.,0.,0.));
#34878=DIRECTION('center_axis',(-0.450270967260838,-0.892891962133151,0.));
#34879=DIRECTION('ref_axis',(-0.892891962133151,0.450270967260838,0.));
#34880=DIRECTION('',(0.,0.,1.));
#34881=DIRECTION('',(-0.892891962133151,0.450270967260838,0.));
#34882=DIRECTION('',(0.,0.,-1.));
#34883=DIRECTION('',(-0.892891962133151,0.450270967260838,0.));
#34884=DIRECTION('center_axis',(0.,0.,1.));
#34885=DIRECTION('ref_axis',(1.,0.,0.));
#34886=DIRECTION('center_axis',(0.,0.,1.));
#34887=DIRECTION('ref_axis',(1.,0.,0.));
#34888=DIRECTION('',(0.685042247217633,0.728503342152262,0.));
#34889=DIRECTION('center_axis',(-0.728503342152262,0.685042247217633,0.));
#34890=DIRECTION('ref_axis',(0.685042247217633,0.728503342152262,0.));
#34891=DIRECTION('',(0.,0.,-1.));
#34892=DIRECTION('',(0.685042247217633,0.728503342152262,0.));
#34893=DIRECTION('center_axis',(0.,0.,-1.));
#34894=DIRECTION('ref_axis',(-1.,0.,0.));
#34895=DIRECTION('center_axis',(0.,0.,-1.));
#34896=DIRECTION('ref_axis',(1.,0.,0.));
#34897=DIRECTION('center_axis',(-0.288381277436908,-0.957515659832181,0.));
#34898=DIRECTION('ref_axis',(-0.957515659832181,0.288381277436908,0.));
#34899=DIRECTION('',(0.,0.,1.));
#34900=DIRECTION('',(-0.957515659832181,0.288381277436908,0.));
#34901=DIRECTION('',(0.,0.,-1.));
#34902=DIRECTION('',(-0.957515659832181,0.288381277436908,0.));
#34903=DIRECTION('center_axis',(0.,0.,1.));
#34904=DIRECTION('ref_axis',(1.,0.,0.));
#34905=DIRECTION('center_axis',(0.,0.,1.));
#34906=DIRECTION('ref_axis',(1.,0.,0.));
#34907=DIRECTION('',(0.548131638411823,0.836392077301053,0.));
#34908=DIRECTION('center_axis',(-0.836392077301053,0.548131638411823,0.));
#34909=DIRECTION('ref_axis',(0.548131638411823,0.836392077301053,0.));
#34910=DIRECTION('',(0.,0.,-1.));
#34911=DIRECTION('',(0.548131638411823,0.836392077301053,0.));
#34912=DIRECTION('center_axis',(0.,0.,-1.));
#34913=DIRECTION('ref_axis',(-1.,0.,0.));
#34914=DIRECTION('center_axis',(0.,0.,-1.));
#34915=DIRECTION('ref_axis',(1.,0.,0.));
#34916=DIRECTION('center_axis',(0.0564998848320982,-0.998402605672661,0.));
#34917=DIRECTION('ref_axis',(-0.998402605672661,-0.0564998848320982,0.));
#34918=DIRECTION('',(0.,0.,1.));
#34919=DIRECTION('',(-0.998402605672661,-0.0564998848320982,0.));
#34920=DIRECTION('',(0.,0.,-1.));
#34921=DIRECTION('',(-0.998402605672661,-0.0564998848320982,0.));
#34922=DIRECTION('center_axis',(0.,0.,1.));
#34923=DIRECTION('ref_axis',(1.,0.,0.));
#34924=DIRECTION('center_axis',(0.,0.,1.));
#34925=DIRECTION('ref_axis',(1.,0.,0.));
#34926=DIRECTION('',(0.22901231767992,0.973423524654542,0.));
#34927=DIRECTION('center_axis',(-0.973423524654542,0.22901231767992,0.));
#34928=DIRECTION('ref_axis',(0.22901231767992,0.973423524654542,0.));
#34929=DIRECTION('',(0.,0.,-1.));
#34930=DIRECTION('',(0.22901231767992,0.973423524654542,0.));
#34931=DIRECTION('center_axis',(0.,0.,-1.));
#34932=DIRECTION('ref_axis',(-1.,0.,0.));
#34933=DIRECTION('center_axis',(0.,0.,-1.));
#34934=DIRECTION('ref_axis',(1.,0.,0.));
#34935=DIRECTION('center_axis',(0.394566327140863,-0.918867462415864,0.));
#34936=DIRECTION('ref_axis',(-0.918867462415864,-0.394566327140863,0.));
#34937=DIRECTION('',(0.,0.,1.));
#34938=DIRECTION('',(-0.918867462415864,-0.394566327140863,0.));
#34939=DIRECTION('',(0.,0.,-1.));
#34940=DIRECTION('',(-0.918867462415864,-0.394566327140863,0.));
#34941=DIRECTION('center_axis',(0.,0.,1.));
#34942=DIRECTION('ref_axis',(1.,0.,0.));
#34943=DIRECTION('center_axis',(0.,0.,1.));
#34944=DIRECTION('ref_axis',(1.,0.,0.));
#34945=DIRECTION('',(-0.117729268426026,0.993045728733512,0.));
#34946=DIRECTION('center_axis',(-0.993045728733512,-0.117729268426026,0.));
#34947=DIRECTION('ref_axis',(-0.117729268426026,0.993045728733512,0.));
#34948=DIRECTION('',(0.,0.,-1.));
#34949=DIRECTION('',(-0.117729268426026,0.993045728733512,0.));
#34950=DIRECTION('center_axis',(0.,0.,-1.));
#34951=DIRECTION('ref_axis',(-1.,0.,0.));
#34952=DIRECTION('center_axis',(0.,0.,-1.));
#34953=DIRECTION('ref_axis',(1.,0.,0.));
#34954=DIRECTION('center_axis',(0.685042247217634,-0.728503342152261,0.));
#34955=DIRECTION('ref_axis',(-0.728503342152261,-0.685042247217634,0.));
#34956=DIRECTION('',(0.,0.,1.));
#34957=DIRECTION('',(-0.728503342152261,-0.685042247217634,0.));
#34958=DIRECTION('',(0.,0.,-1.));
#34959=DIRECTION('',(-0.728503342152261,-0.685042247217634,0.));
#34960=DIRECTION('center_axis',(0.,0.,1.));
#34961=DIRECTION('ref_axis',(1.,0.,0.));
#34962=DIRECTION('center_axis',(0.,0.,1.));
#34963=DIRECTION('ref_axis',(1.,0.,0.));
#34964=DIRECTION('',(-0.450270967260839,0.892891962133151,0.));
#34965=DIRECTION('center_axis',(-0.892891962133151,-0.450270967260839,0.));
#34966=DIRECTION('ref_axis',(-0.450270967260839,0.892891962133151,0.));
#34967=DIRECTION('',(0.,0.,-1.));
#34968=DIRECTION('',(-0.450270967260839,0.892891962133151,0.));
#34969=DIRECTION('center_axis',(0.,0.,-1.));
#34970=DIRECTION('ref_axis',(-1.,0.,0.));
#34971=DIRECTION('center_axis',(0.,0.,-1.));
#34972=DIRECTION('ref_axis',(1.,0.,0.));
#34973=DIRECTION('center_axis',(0.892891962133151,-0.450270967260839,0.));
#34974=DIRECTION('ref_axis',(-0.450270967260839,-0.892891962133151,0.));
#34975=DIRECTION('',(0.,0.,1.));
#34976=DIRECTION('',(-0.450270967260839,-0.892891962133151,0.));
#34977=DIRECTION('',(0.,0.,-1.));
#34978=DIRECTION('',(-0.450270967260839,-0.892891962133151,0.));
#34979=DIRECTION('center_axis',(0.,0.,1.));
#34980=DIRECTION('ref_axis',(1.,0.,0.));
#34981=DIRECTION('center_axis',(0.,0.,1.));
#34982=DIRECTION('ref_axis',(1.,0.,0.));
#34983=DIRECTION('',(-0.728503342152262,0.685042247217633,0.));
#34984=DIRECTION('center_axis',(-0.685042247217633,-0.728503342152262,0.));
#34985=DIRECTION('ref_axis',(-0.728503342152262,0.685042247217633,0.));
#34986=DIRECTION('',(0.,0.,-1.));
#34987=DIRECTION('',(-0.728503342152262,0.685042247217633,0.));
#34988=DIRECTION('center_axis',(0.,0.,-1.));
#34989=DIRECTION('ref_axis',(-1.,0.,0.));
#34990=DIRECTION('center_axis',(0.,0.,-1.));
#34991=DIRECTION('ref_axis',(1.,0.,0.));
#34992=DIRECTION('center_axis',(0.993045728733513,-0.117729268426024,0.));
#34993=DIRECTION('ref_axis',(-0.117729268426024,-0.993045728733513,0.));
#34994=DIRECTION('',(0.,0.,1.));
#34995=DIRECTION('',(-0.117729268426024,-0.993045728733513,0.));
#34996=DIRECTION('',(0.,0.,-1.));
#34997=DIRECTION('',(-0.117729268426024,-0.993045728733513,0.));
#34998=DIRECTION('center_axis',(0.,0.,1.));
#34999=DIRECTION('ref_axis',(1.,0.,0.));
#35000=DIRECTION('center_axis',(0.,0.,1.));
#35001=DIRECTION('ref_axis',(1.,0.,0.));
#35002=DIRECTION('',(-0.918867462415865,0.39456632714086,0.));
#35003=DIRECTION('center_axis',(-0.39456632714086,-0.918867462415865,0.));
#35004=DIRECTION('ref_axis',(-0.918867462415865,0.39456632714086,0.));
#35005=DIRECTION('',(0.,0.,-1.));
#35006=DIRECTION('',(-0.918867462415865,0.39456632714086,0.));
#35007=DIRECTION('center_axis',(0.,0.,-1.));
#35008=DIRECTION('ref_axis',(-1.,0.,0.));
#35009=DIRECTION('center_axis',(0.,0.,-1.));
#35010=DIRECTION('ref_axis',(1.,0.,0.));
#35011=DIRECTION('center_axis',(0.973423524654542,0.229012317679921,0.));
#35012=DIRECTION('ref_axis',(0.229012317679921,-0.973423524654542,0.));
#35013=DIRECTION('',(0.,0.,1.));
#35014=DIRECTION('',(0.229012317679921,-0.973423524654542,0.));
#35015=DIRECTION('',(0.,0.,-1.));
#35016=DIRECTION('',(0.229012317679921,-0.973423524654542,0.));
#35017=DIRECTION('center_axis',(0.,0.,1.));
#35018=DIRECTION('ref_axis',(1.,0.,0.));
#35019=DIRECTION('center_axis',(0.,0.,1.));
#35020=DIRECTION('ref_axis',(1.,0.,0.));
#35021=DIRECTION('',(-0.998402605672661,0.0564998848320951,0.));
#35022=DIRECTION('center_axis',(-0.0564998848320951,-0.998402605672661,
0.));
#35023=DIRECTION('ref_axis',(-0.998402605672661,0.0564998848320951,0.));
#35024=DIRECTION('',(0.,0.,-1.));
#35025=DIRECTION('',(-0.998402605672661,0.0564998848320951,0.));
#35026=DIRECTION('center_axis',(0.,0.,-1.));
#35027=DIRECTION('ref_axis',(-1.,0.,0.));
#35028=DIRECTION('center_axis',(0.,0.,-1.));
#35029=DIRECTION('ref_axis',(1.,0.,0.));
#35030=DIRECTION('center_axis',(0.836392077301052,0.548131638411824,0.));
#35031=DIRECTION('ref_axis',(0.548131638411824,-0.836392077301052,0.));
#35032=DIRECTION('',(0.,0.,1.));
#35033=DIRECTION('',(0.548131638411824,-0.836392077301052,0.));
#35034=DIRECTION('',(0.,0.,-1.));
#35035=DIRECTION('',(0.548131638411824,-0.836392077301052,0.));
#35036=DIRECTION('center_axis',(0.,0.,1.));
#35037=DIRECTION('ref_axis',(1.,0.,0.));
#35038=DIRECTION('center_axis',(0.,0.,1.));
#35039=DIRECTION('ref_axis',(1.,0.,0.));
#35040=DIRECTION('',(-0.95751565983218,-0.288381277436911,0.));
#35041=DIRECTION('center_axis',(0.288381277436911,-0.95751565983218,0.));
#35042=DIRECTION('ref_axis',(-0.95751565983218,-0.288381277436911,0.));
#35043=DIRECTION('',(0.,0.,-1.));
#35044=DIRECTION('',(-0.95751565983218,-0.288381277436911,0.));
#35045=DIRECTION('center_axis',(0.,0.,-1.));
#35046=DIRECTION('ref_axis',(-1.,0.,0.));
#35047=DIRECTION('center_axis',(0.,0.,-1.));
#35048=DIRECTION('ref_axis',(1.,0.,0.));
#35049=DIRECTION('center_axis',(0.,0.,1.));
#35050=DIRECTION('ref_axis',(1.,0.,0.));
#35051=DIRECTION('center_axis',(0.,0.,1.));
#35052=DIRECTION('ref_axis',(1.,0.,0.));
#35053=DIRECTION('',(-0.801138193989839,0.598479401592653,0.));
#35054=DIRECTION('',(0.801138193989839,0.598479401592653,0.));
#35055=DIRECTION('center_axis',(-0.598479401592653,-0.801138193989839,0.));
#35056=DIRECTION('ref_axis',(-0.801138193989839,0.598479401592653,0.));
#35057=DIRECTION('',(0.,0.,1.));
#35058=DIRECTION('',(-0.801138193989839,0.598479401592653,0.));
#35059=DIRECTION('',(0.,0.,-1.));
#35060=DIRECTION('center_axis',(-0.598479401592653,0.801138193989839,0.));
#35061=DIRECTION('ref_axis',(0.801138193989839,0.598479401592653,0.));
#35062=DIRECTION('',(0.,0.,-1.));
#35063=DIRECTION('',(0.801138193989839,0.598479401592653,0.));
#35064=DIRECTION('center_axis',(0.,0.,-1.));
#35065=DIRECTION('ref_axis',(-1.,0.,0.));
#35066=DIRECTION('center_axis',(0.,0.,-1.));
#35067=DIRECTION('ref_axis',(1.,0.,0.));
#35068=DIRECTION('center_axis',(0.450270967260841,0.89289196213315,0.));
#35069=DIRECTION('ref_axis',(0.89289196213315,-0.450270967260841,0.));
#35070=DIRECTION('',(0.,0.,1.));
#35071=DIRECTION('',(0.89289196213315,-0.450270967260841,0.));
#35072=DIRECTION('',(0.,0.,-1.));
#35073=DIRECTION('',(0.89289196213315,-0.450270967260841,0.));
#35074=DIRECTION('center_axis',(0.,0.,1.));
#35075=DIRECTION('ref_axis',(1.,0.,0.));
#35076=DIRECTION('center_axis',(0.,0.,1.));
#35077=DIRECTION('ref_axis',(1.,0.,0.));
#35078=DIRECTION('',(-0.685042247217634,-0.728503342152261,0.));
#35079=DIRECTION('center_axis',(0.728503342152261,-0.685042247217634,0.));
#35080=DIRECTION('ref_axis',(-0.685042247217634,-0.728503342152261,0.));
#35081=DIRECTION('',(0.,0.,-1.));
#35082=DIRECTION('',(-0.685042247217634,-0.728503342152261,0.));
#35083=DIRECTION('center_axis',(0.,0.,-1.));
#35084=DIRECTION('ref_axis',(-1.,0.,0.));
#35085=DIRECTION('center_axis',(0.,0.,-1.));
#35086=DIRECTION('ref_axis',(1.,0.,0.));
#35087=DIRECTION('center_axis',(0.117729268426028,0.993045728733512,0.));
#35088=DIRECTION('ref_axis',(0.993045728733512,-0.117729268426028,0.));
#35089=DIRECTION('',(0.,0.,1.));
#35090=DIRECTION('',(0.993045728733512,-0.117729268426028,0.));
#35091=DIRECTION('',(0.,0.,-1.));
#35092=DIRECTION('',(0.993045728733512,-0.117729268426028,0.));
#35093=DIRECTION('center_axis',(0.,0.,1.));
#35094=DIRECTION('ref_axis',(1.,0.,0.));
#35095=DIRECTION('center_axis',(0.,0.,1.));
#35096=DIRECTION('ref_axis',(1.,0.,0.));
#35097=DIRECTION('',(-0.394566327140863,-0.918867462415864,0.));
#35098=DIRECTION('center_axis',(0.918867462415864,-0.394566327140863,0.));
#35099=DIRECTION('ref_axis',(-0.394566327140863,-0.918867462415864,0.));
#35100=DIRECTION('',(0.,0.,-1.));
#35101=DIRECTION('',(-0.394566327140863,-0.918867462415864,0.));
#35102=DIRECTION('center_axis',(0.,0.,-1.));
#35103=DIRECTION('ref_axis',(-1.,0.,0.));
#35104=DIRECTION('center_axis',(0.,0.,-1.));
#35105=DIRECTION('ref_axis',(1.,0.,0.));
#35106=DIRECTION('center_axis',(-0.22901231767992,0.973423524654542,0.));
#35107=DIRECTION('ref_axis',(0.973423524654542,0.22901231767992,0.));
#35108=DIRECTION('',(0.,0.,1.));
#35109=DIRECTION('',(0.973423524654542,0.22901231767992,0.));
#35110=DIRECTION('',(0.,0.,-1.));
#35111=DIRECTION('',(0.973423524654542,0.22901231767992,0.));
#35112=DIRECTION('center_axis',(0.,0.,1.));
#35113=DIRECTION('ref_axis',(1.,0.,0.));
#35114=DIRECTION('center_axis',(0.,0.,1.));
#35115=DIRECTION('ref_axis',(1.,0.,0.));
#35116=DIRECTION('',(-0.0564998848320967,-0.998402605672661,0.));
#35117=DIRECTION('center_axis',(0.998402605672661,-0.0564998848320967,0.));
#35118=DIRECTION('ref_axis',(-0.0564998848320967,-0.998402605672661,0.));
#35119=DIRECTION('',(0.,0.,-1.));
#35120=DIRECTION('',(-0.0564998848320967,-0.998402605672661,0.));
#35121=DIRECTION('center_axis',(0.,0.,-1.));
#35122=DIRECTION('ref_axis',(-1.,0.,0.));
#35123=DIRECTION('center_axis',(0.,0.,-1.));
#35124=DIRECTION('ref_axis',(1.,0.,0.));
#35125=DIRECTION('center_axis',(-0.548131638411821,0.836392077301054,0.));
#35126=DIRECTION('ref_axis',(0.836392077301054,0.548131638411821,0.));
#35127=DIRECTION('',(0.,0.,1.));
#35128=DIRECTION('',(0.836392077301054,0.548131638411821,0.));
#35129=DIRECTION('',(0.,0.,-1.));
#35130=DIRECTION('',(0.836392077301054,0.548131638411821,0.));
#35131=DIRECTION('center_axis',(0.,0.,1.));
#35132=DIRECTION('ref_axis',(1.,0.,0.));
#35133=DIRECTION('center_axis',(0.,0.,1.));
#35134=DIRECTION('ref_axis',(1.,0.,0.));
#35135=DIRECTION('',(0.288381277436903,-0.957515659832182,0.));
#35136=DIRECTION('center_axis',(0.957515659832182,0.288381277436903,0.));
#35137=DIRECTION('ref_axis',(0.288381277436903,-0.957515659832182,0.));
#35138=DIRECTION('',(0.,0.,-1.));
#35139=DIRECTION('',(0.288381277436903,-0.957515659832182,0.));
#35140=DIRECTION('center_axis',(0.,0.,-1.));
#35141=DIRECTION('ref_axis',(-1.,0.,0.));
#35142=DIRECTION('center_axis',(0.,0.,-1.));
#35143=DIRECTION('ref_axis',(1.,0.,0.));
#35144=DIRECTION('center_axis',(-0.801138193989837,0.598479401592655,0.));
#35145=DIRECTION('ref_axis',(0.598479401592655,0.801138193989837,0.));
#35146=DIRECTION('',(0.,0.,1.));
#35147=DIRECTION('',(0.598479401592655,0.801138193989837,0.));
#35148=DIRECTION('',(0.,0.,-1.));
#35149=DIRECTION('',(0.598479401592655,0.801138193989837,0.));
#35150=DIRECTION('center_axis',(0.,0.,1.));
#35151=DIRECTION('ref_axis',(1.,0.,0.));
#35152=DIRECTION('center_axis',(0.,0.,1.));
#35153=DIRECTION('ref_axis',(1.,0.,0.));
#35154=DIRECTION('',(0.598479401592655,-0.801138193989837,0.));
#35155=DIRECTION('center_axis',(0.801138193989837,0.598479401592655,0.));
#35156=DIRECTION('ref_axis',(0.598479401592655,-0.801138193989837,0.));
#35157=DIRECTION('',(0.,0.,-1.));
#35158=DIRECTION('',(0.598479401592655,-0.801138193989837,0.));
#35159=DIRECTION('center_axis',(0.,0.,-1.));
#35160=DIRECTION('ref_axis',(-1.,0.,0.));
#35161=DIRECTION('center_axis',(0.,0.,-1.));
#35162=DIRECTION('ref_axis',(1.,0.,0.));
#35163=DIRECTION('center_axis',(-0.95751565983218,0.288381277436912,0.));
#35164=DIRECTION('ref_axis',(0.288381277436912,0.95751565983218,0.));
#35165=DIRECTION('',(0.,0.,1.));
#35166=DIRECTION('',(0.288381277436912,0.95751565983218,0.));
#35167=DIRECTION('',(0.,0.,-1.));
#35168=DIRECTION('',(0.288381277436912,0.95751565983218,0.));
#35169=DIRECTION('center_axis',(0.,0.,1.));
#35170=DIRECTION('ref_axis',(1.,0.,0.));
#35171=DIRECTION('center_axis',(0.,0.,1.));
#35172=DIRECTION('ref_axis',(1.,0.,0.));
#35173=DIRECTION('',(0.836392077301051,-0.548131638411826,0.));
#35174=DIRECTION('center_axis',(0.548131638411826,0.836392077301051,0.));
#35175=DIRECTION('ref_axis',(0.836392077301051,-0.548131638411826,0.));
#35176=DIRECTION('',(0.,0.,-1.));
#35177=DIRECTION('',(0.836392077301051,-0.548131638411826,0.));
#35178=DIRECTION('center_axis',(0.,0.,-1.));
#35179=DIRECTION('ref_axis',(-1.,0.,0.));
#35180=DIRECTION('center_axis',(0.,0.,-1.));
#35181=DIRECTION('ref_axis',(1.,0.,0.));
#35182=DIRECTION('center_axis',(-0.998402605672661,-0.0564998848320951,
0.));
#35183=DIRECTION('ref_axis',(-0.0564998848320951,0.998402605672661,0.));
#35184=DIRECTION('',(0.,0.,1.));
#35185=DIRECTION('',(-0.0564998848320951,0.998402605672661,0.));
#35186=DIRECTION('',(0.,0.,-1.));
#35187=DIRECTION('',(-0.0564998848320951,0.998402605672661,0.));
#35188=DIRECTION('center_axis',(0.,0.,1.));
#35189=DIRECTION('ref_axis',(1.,0.,0.));
#35190=DIRECTION('center_axis',(0.,0.,1.));
#35191=DIRECTION('ref_axis',(1.,0.,0.));
#35192=DIRECTION('',(0.973423524654543,-0.229012317679917,0.));
#35193=DIRECTION('center_axis',(0.229012317679917,0.973423524654543,0.));
#35194=DIRECTION('ref_axis',(0.973423524654543,-0.229012317679917,0.));
#35195=DIRECTION('',(0.,0.,-1.));
#35196=DIRECTION('',(0.973423524654543,-0.229012317679917,0.));
#35197=DIRECTION('center_axis',(0.,0.,-1.));
#35198=DIRECTION('ref_axis',(-1.,0.,0.));
#35199=DIRECTION('center_axis',(0.,0.,-1.));
#35200=DIRECTION('ref_axis',(1.,0.,0.));
#35201=DIRECTION('center_axis',(-0.918867462415863,-0.394566327140866,0.));
#35202=DIRECTION('ref_axis',(-0.394566327140866,0.918867462415863,0.));
#35203=DIRECTION('',(0.,0.,1.));
#35204=DIRECTION('',(-0.394566327140866,0.918867462415863,0.));
#35205=DIRECTION('',(0.,0.,-1.));
#35206=DIRECTION('',(-0.394566327140866,0.918867462415863,0.));
#35207=DIRECTION('center_axis',(0.,0.,1.));
#35208=DIRECTION('ref_axis',(1.,0.,0.));
#35209=DIRECTION('center_axis',(0.,0.,1.));
#35210=DIRECTION('ref_axis',(1.,0.,0.));
#35211=DIRECTION('',(0.993045728733512,0.117729268426028,0.));
#35212=DIRECTION('center_axis',(-0.117729268426028,0.993045728733512,0.));
#35213=DIRECTION('ref_axis',(0.993045728733512,0.117729268426028,0.));
#35214=DIRECTION('',(0.,0.,-1.));
#35215=DIRECTION('',(0.993045728733512,0.117729268426028,0.));
#35216=DIRECTION('center_axis',(0.,0.,-1.));
#35217=DIRECTION('ref_axis',(-1.,0.,0.));
#35218=DIRECTION('center_axis',(0.,0.,-1.));
#35219=DIRECTION('ref_axis',(1.,0.,0.));
#35220=DIRECTION('center_axis',(-0.728503342152263,-0.685042247217632,0.));
#35221=DIRECTION('ref_axis',(-0.685042247217632,0.728503342152263,0.));
#35222=DIRECTION('',(0.,0.,1.));
#35223=DIRECTION('',(-0.685042247217632,0.728503342152263,0.));
#35224=DIRECTION('',(0.,0.,-1.));
#35225=DIRECTION('',(-0.685042247217632,0.728503342152263,0.));
#35226=DIRECTION('center_axis',(0.,0.,1.));
#35227=DIRECTION('ref_axis',(1.,0.,0.));
#35228=DIRECTION('center_axis',(0.,0.,1.));
#35229=DIRECTION('ref_axis',(1.,0.,0.));
#35230=DIRECTION('',(0.89289196213315,0.450270967260841,0.));
#35231=DIRECTION('center_axis',(-0.450270967260841,0.89289196213315,0.));
#35232=DIRECTION('ref_axis',(0.89289196213315,0.450270967260841,0.));
#35233=DIRECTION('',(0.,0.,-1.));
#35234=DIRECTION('',(0.89289196213315,0.450270967260841,0.));
#35235=DIRECTION('center_axis',(0.,0.,-1.));
#35236=DIRECTION('ref_axis',(-1.,0.,0.));
#35237=DIRECTION('center_axis',(0.,0.,-1.));
#35238=DIRECTION('ref_axis',(1.,0.,0.));
#35239=DIRECTION('center_axis',(0.,0.,-1.));
#35240=DIRECTION('ref_axis',(-1.,0.,0.));
#35241=DIRECTION('center_axis',(0.,0.,1.));
#35242=DIRECTION('ref_axis',(1.,0.,0.));
#35243=DIRECTION('center_axis',(0.,0.,1.));
#35244=DIRECTION('ref_axis',(1.,0.,0.));
#35245=DIRECTION('',(0.707106781186549,8.65956056235495E-17,-0.707106781186546));
#35246=DIRECTION('center_axis',(0.,0.,1.));
#35247=DIRECTION('ref_axis',(1.,0.,0.));
#35248=DIRECTION('center_axis',(0.,0.,1.));
#35249=DIRECTION('ref_axis',(1.,0.,0.));
#35250=DIRECTION('',(0.707106781186548,8.65956056235494E-17,-0.707106781186547));
#35251=DIRECTION('center_axis',(0.,0.,1.));
#35252=DIRECTION('ref_axis',(1.,0.,0.));
#35253=DIRECTION('center_axis',(0.,0.,1.));
#35254=DIRECTION('ref_axis',(1.,0.,0.));
#35255=DIRECTION('center_axis',(0.,0.,1.));
#35256=DIRECTION('ref_axis',(1.,0.,0.));
#35257=DIRECTION('center_axis',(0.,0.,1.));
#35258=DIRECTION('ref_axis',(1.,0.,0.));
#35259=DIRECTION('center_axis',(0.,0.,1.));
#35260=DIRECTION('ref_axis',(1.,0.,0.));
#35261=DIRECTION('center_axis',(0.,0.,1.));
#35262=DIRECTION('ref_axis',(1.,0.,0.));
#35263=DIRECTION('center_axis',(0.,0.,1.));
#35264=DIRECTION('ref_axis',(1.,0.,0.));
#35265=DIRECTION('center_axis',(0.,0.,1.));
#35266=DIRECTION('ref_axis',(1.,0.,0.));
#35267=DIRECTION('center_axis',(0.,0.,1.));
#35268=DIRECTION('ref_axis',(1.,0.,0.));
#35269=DIRECTION('center_axis',(0.,0.,1.));
#35270=DIRECTION('ref_axis',(1.,0.,0.));
#35271=DIRECTION('center_axis',(0.,0.,1.));
#35272=DIRECTION('ref_axis',(1.,0.,0.));
#35273=DIRECTION('center_axis',(0.,0.,1.));
#35274=DIRECTION('ref_axis',(1.,0.,0.));
#35275=DIRECTION('center_axis',(0.,0.,1.));
#35276=DIRECTION('ref_axis',(1.,0.,0.));
#35277=DIRECTION('center_axis',(0.,0.,1.));
#35278=DIRECTION('ref_axis',(1.,0.,0.));
#35279=DIRECTION('center_axis',(0.,0.,1.));
#35280=DIRECTION('ref_axis',(1.,0.,0.));
#35281=DIRECTION('center_axis',(0.,0.,1.));
#35282=DIRECTION('ref_axis',(1.,0.,0.));
#35283=DIRECTION('center_axis',(0.,0.,1.));
#35284=DIRECTION('ref_axis',(1.,0.,0.));
#35285=DIRECTION('',(0.,0.,-1.));
#35286=DIRECTION('center_axis',(0.,0.,1.));
#35287=DIRECTION('ref_axis',(1.,0.,0.));
#35288=DIRECTION('center_axis',(0.,0.,1.));
#35289=DIRECTION('ref_axis',(1.,0.,0.));
#35290=DIRECTION('center_axis',(0.,0.,1.));
#35291=DIRECTION('ref_axis',(1.,0.,0.));
#35292=DIRECTION('center_axis',(0.,0.,1.));
#35293=DIRECTION('ref_axis',(1.,0.,0.));
#35294=DIRECTION('center_axis',(0.,0.,1.));
#35295=DIRECTION('ref_axis',(1.,0.,0.));
#35296=DIRECTION('center_axis',(0.,0.,1.));
#35297=DIRECTION('ref_axis',(1.,0.,0.));
#35298=DIRECTION('center_axis',(0.,0.,1.));
#35299=DIRECTION('ref_axis',(1.,0.,0.));
#35300=DIRECTION('center_axis',(0.,0.,1.));
#35301=DIRECTION('ref_axis',(1.,0.,0.));
#35302=DIRECTION('center_axis',(0.,0.,1.));
#35303=DIRECTION('ref_axis',(1.,0.,0.));
#35304=DIRECTION('center_axis',(0.,0.,1.));
#35305=DIRECTION('ref_axis',(1.,0.,0.));
#35306=DIRECTION('center_axis',(0.,0.,1.));
#35307=DIRECTION('ref_axis',(1.,0.,0.));
#35308=DIRECTION('center_axis',(0.,0.,1.));
#35309=DIRECTION('ref_axis',(1.,0.,0.));
#35310=DIRECTION('center_axis',(0.,0.,1.));
#35311=DIRECTION('ref_axis',(1.,0.,0.));
#35312=DIRECTION('center_axis',(0.,0.,1.));
#35313=DIRECTION('ref_axis',(1.,0.,0.));
#35314=DIRECTION('center_axis',(0.,0.,1.));
#35315=DIRECTION('ref_axis',(1.,0.,0.));
#35316=DIRECTION('center_axis',(0.,0.,1.));
#35317=DIRECTION('ref_axis',(1.,0.,0.));
#35318=DIRECTION('center_axis',(0.,0.,1.));
#35319=DIRECTION('ref_axis',(1.,0.,0.));
#35320=DIRECTION('center_axis',(0.,0.,1.));
#35321=DIRECTION('ref_axis',(1.,0.,0.));
#35322=DIRECTION('center_axis',(0.,0.,1.));
#35323=DIRECTION('ref_axis',(1.,0.,0.));
#35324=DIRECTION('center_axis',(0.,0.,1.));
#35325=DIRECTION('ref_axis',(1.,0.,0.));
#35326=DIRECTION('center_axis',(0.,0.,-1.));
#35327=DIRECTION('ref_axis',(1.,0.,0.));
#35328=DIRECTION('center_axis',(0.,0.,1.));
#35329=DIRECTION('ref_axis',(1.,0.,0.));
#35330=DIRECTION('',(-0.707106781186548,-8.65956056235493E-17,-0.707106781186547));
#35331=DIRECTION('center_axis',(0.,0.,1.));
#35332=DIRECTION('ref_axis',(1.,0.,0.));
#35333=DIRECTION('axis',(0.,0.,1.));
#35334=DIRECTION('refdir',(1.,0.,0.));
#35335=DIRECTION('center_axis',(0.,0.,1.));
#35336=DIRECTION('ref_axis',(1.,0.,0.));
#35337=DIRECTION('',(0.,0.,-1.));
#35338=DIRECTION('center_axis',(0.,0.,1.));
#35339=DIRECTION('ref_axis',(1.,0.,0.));
#35340=DIRECTION('center_axis',(0.,0.,1.));
#35341=DIRECTION('ref_axis',(1.,0.,0.));
#35342=DIRECTION('',(0.,0.,-1.));
#35343=DIRECTION('center_axis',(0.,0.,1.));
#35344=DIRECTION('ref_axis',(1.,0.,0.));
#35345=DIRECTION('',(0.,0.,-1.));
#35346=DIRECTION('center_axis',(0.,0.,1.));
#35347=DIRECTION('ref_axis',(1.,0.,0.));
#35348=DIRECTION('',(0.,0.,-1.));
#35349=DIRECTION('center_axis',(0.,0.,1.));
#35350=DIRECTION('ref_axis',(1.,0.,0.));
#35351=DIRECTION('',(0.,0.,-1.));
#35352=DIRECTION('center_axis',(0.,0.,1.));
#35353=DIRECTION('ref_axis',(1.,0.,0.));
#35354=DIRECTION('',(0.,0.,-1.));
#35355=DIRECTION('center_axis',(0.,0.,1.));
#35356=DIRECTION('ref_axis',(1.,0.,0.));
#35357=DIRECTION('',(0.,0.,-1.));
#35358=DIRECTION('center_axis',(0.,0.,1.));
#35359=DIRECTION('ref_axis',(1.,0.,0.));
#35360=DIRECTION('',(0.,0.,-1.));
#35361=DIRECTION('center_axis',(0.,0.,1.));
#35362=DIRECTION('ref_axis',(1.,0.,0.));
#35363=DIRECTION('',(0.,0.,-1.));
#35364=DIRECTION('center_axis',(0.,0.,1.));
#35365=DIRECTION('ref_axis',(1.,0.,0.));
#35366=DIRECTION('',(0.,0.,-1.));
#35367=DIRECTION('center_axis',(0.,0.,1.));
#35368=DIRECTION('ref_axis',(1.,0.,0.));
#35369=DIRECTION('',(0.,0.,-1.));
#35370=DIRECTION('center_axis',(0.,0.,1.));
#35371=DIRECTION('ref_axis',(1.,0.,0.));
#35372=DIRECTION('',(0.,0.,-1.));
#35373=DIRECTION('center_axis',(0.,0.,1.));
#35374=DIRECTION('ref_axis',(1.,0.,0.));
#35375=DIRECTION('',(0.,0.,-1.));
#35376=DIRECTION('center_axis',(0.,0.,1.));
#35377=DIRECTION('ref_axis',(1.,0.,0.));
#35378=DIRECTION('',(0.,0.,-1.));
#35379=DIRECTION('center_axis',(0.,0.,1.));
#35380=DIRECTION('ref_axis',(1.,0.,0.));
#35381=DIRECTION('',(0.,0.,-1.));
#35382=DIRECTION('center_axis',(0.,0.,1.));
#35383=DIRECTION('ref_axis',(1.,0.,0.));
#35384=DIRECTION('',(0.,0.,-1.));
#35385=DIRECTION('center_axis',(0.,0.,1.));
#35386=DIRECTION('ref_axis',(1.,0.,0.));
#35387=DIRECTION('',(0.,0.,-1.));
#35388=DIRECTION('center_axis',(0.,0.,1.));
#35389=DIRECTION('ref_axis',(1.,0.,0.));
#35390=DIRECTION('',(0.,0.,-1.));
#35391=DIRECTION('center_axis',(0.,0.,1.));
#35392=DIRECTION('ref_axis',(1.,0.,0.));
#35393=DIRECTION('',(0.,0.,-1.));
#35394=DIRECTION('center_axis',(0.,0.,1.));
#35395=DIRECTION('ref_axis',(1.,0.,0.));
#35396=DIRECTION('',(0.,0.,-1.));
#35397=DIRECTION('center_axis',(0.,0.,1.));
#35398=DIRECTION('ref_axis',(1.,0.,0.));
#35399=DIRECTION('center_axis',(0.,0.,1.));
#35400=DIRECTION('ref_axis',(0.472251364843622,-0.881463923483733,0.));
#35401=DIRECTION('',(0.,0.,1.));
#35402=DIRECTION('center_axis',(0.,0.,1.));
#35403=DIRECTION('ref_axis',(1.,9.72557910080329E-14,0.));
#35404=DIRECTION('center_axis',(0.,0.,1.));
#35405=DIRECTION('ref_axis',(1.,9.72557910080329E-14,0.));
#35406=DIRECTION('',(0.,0.,1.));
#35407=DIRECTION('center_axis',(0.,0.,1.));
#35408=DIRECTION('ref_axis',(1.,9.72557910080329E-14,0.));
#35409=DIRECTION('',(0.,0.,1.));
#35410=DIRECTION('center_axis',(0.,0.,1.));
#35411=DIRECTION('ref_axis',(1.,9.72557910080329E-14,0.));
#35412=DIRECTION('',(0.,0.,1.));
#35413=DIRECTION('center_axis',(0.,0.,1.));
#35414=DIRECTION('ref_axis',(1.,9.72557910080329E-14,0.));
#35415=DIRECTION('',(0.,0.,1.));
#35416=DIRECTION('center_axis',(0.,0.,1.));
#35417=DIRECTION('ref_axis',(1.,9.72557910080329E-14,0.));
#35418=DIRECTION('',(0.,0.,1.));
#35419=DIRECTION('center_axis',(0.,0.,1.));
#35420=DIRECTION('ref_axis',(1.,9.72557910080329E-14,0.));
#35421=DIRECTION('',(0.,0.,1.));
#35422=DIRECTION('center_axis',(0.,0.,1.));
#35423=DIRECTION('ref_axis',(1.,9.72557910080329E-14,0.));
#35424=DIRECTION('',(0.,0.,1.));
#35425=DIRECTION('center_axis',(0.,0.,1.));
#35426=DIRECTION('ref_axis',(1.,9.72557910080329E-14,0.));
#35427=DIRECTION('',(0.,0.,1.));
#35428=DIRECTION('center_axis',(0.,0.,1.));
#35429=DIRECTION('ref_axis',(1.,9.72557910080329E-14,0.));
#35430=DIRECTION('',(0.,0.,1.));
#35431=DIRECTION('center_axis',(0.,0.,1.));
#35432=DIRECTION('ref_axis',(1.,9.72557910080329E-14,0.));
#35433=DIRECTION('',(0.,0.,1.));
#35434=DIRECTION('center_axis',(0.,0.,1.));
#35435=DIRECTION('ref_axis',(1.,9.72557910080329E-14,0.));
#35436=DIRECTION('',(0.,0.,1.));
#35437=DIRECTION('center_axis',(0.,0.,1.));
#35438=DIRECTION('ref_axis',(1.,9.72557910080329E-14,0.));
#35439=DIRECTION('',(0.,0.,1.));
#35440=DIRECTION('center_axis',(0.,0.,1.));
#35441=DIRECTION('ref_axis',(1.,9.72557910080329E-14,0.));
#35442=DIRECTION('',(0.,0.,1.));
#35443=DIRECTION('center_axis',(0.,0.,1.));
#35444=DIRECTION('ref_axis',(1.,9.72557910080329E-14,0.));
#35445=DIRECTION('',(0.,0.,1.));
#35446=DIRECTION('center_axis',(0.,0.,1.));
#35447=DIRECTION('ref_axis',(1.,9.72557910080329E-14,0.));
#35448=DIRECTION('',(0.,0.,1.));
#35449=DIRECTION('center_axis',(0.,0.,1.));
#35450=DIRECTION('ref_axis',(1.,9.72557910080329E-14,0.));
#35451=DIRECTION('',(0.,0.,1.));
#35452=DIRECTION('center_axis',(0.,0.,1.));
#35453=DIRECTION('ref_axis',(1.,9.72557910080329E-14,0.));
#35454=DIRECTION('',(0.,0.,1.));
#35455=DIRECTION('center_axis',(0.,0.,1.));
#35456=DIRECTION('ref_axis',(1.,9.72557910080329E-14,0.));
#35457=DIRECTION('',(0.,0.,1.));
#35458=DIRECTION('center_axis',(0.,0.,1.));
#35459=DIRECTION('ref_axis',(1.,0.,0.));
#35460=DIRECTION('center_axis',(0.,0.,1.));
#35461=DIRECTION('ref_axis',(1.,0.,0.));
#35462=DIRECTION('center_axis',(0.,0.,1.));
#35463=DIRECTION('ref_axis',(1.,0.,0.));
#35464=DIRECTION('center_axis',(0.,0.,1.));
#35465=DIRECTION('ref_axis',(1.,0.,0.));
#35466=DIRECTION('center_axis',(0.,0.,1.));
#35467=DIRECTION('ref_axis',(1.,0.,0.));
#35468=DIRECTION('center_axis',(0.,0.,-1.));
#35469=DIRECTION('ref_axis',(1.,9.72557910080329E-14,0.));
#35470=DIRECTION('center_axis',(0.,0.,1.));
#35471=DIRECTION('ref_axis',(1.,9.72557910080329E-14,0.));
#35472=DIRECTION('center_axis',(0.,0.,1.));
#35473=DIRECTION('ref_axis',(1.,0.,0.));
#35474=DIRECTION('center_axis',(1.22464679914735E-16,-1.,0.));
#35475=DIRECTION('ref_axis',(-1.,-1.22464679914735E-16,0.));
#35476=DIRECTION('center_axis',(0.,0.,-1.));
#35477=DIRECTION('ref_axis',(1.,0.,0.));
#35478=DIRECTION('center_axis',(0.,0.,1.));
#35479=DIRECTION('ref_axis',(1.,0.,0.));
#35480=DIRECTION('center_axis',(0.,0.,1.));
#35481=DIRECTION('ref_axis',(-0.917573945891785,-0.397565156698344,0.));
#35482=DIRECTION('center_axis',(0.,0.,-1.));
#35483=DIRECTION('ref_axis',(-1.,0.,0.));
#35484=DIRECTION('center_axis',(0.,0.,1.));
#35485=DIRECTION('ref_axis',(1.,0.,0.));
#35486=DIRECTION('center_axis',(0.,0.,1.));
#35487=DIRECTION('ref_axis',(1.,0.,0.));
#35488=DIRECTION('',(0.5,-0.866025403784439,0.));
#35489=DIRECTION('center_axis',(0.,0.,1.));
#35490=DIRECTION('ref_axis',(1.,0.,0.));
#35491=DIRECTION('center_axis',(0.,0.,1.));
#35492=DIRECTION('ref_axis',(1.,0.,0.));
#35493=DIRECTION('',(-0.5,-0.866025403784439,0.));
#35494=DIRECTION('center_axis',(0.,0.,1.));
#35495=DIRECTION('ref_axis',(1.,0.,0.));
#35496=DIRECTION('center_axis',(0.,0.,1.));
#35497=DIRECTION('ref_axis',(1.,0.,0.));
#35498=DIRECTION('',(-1.,1.92296268638356E-16,0.));
#35499=DIRECTION('center_axis',(0.,0.,1.));
#35500=DIRECTION('ref_axis',(1.,0.,0.));
#35501=DIRECTION('center_axis',(0.,0.,1.));
#35502=DIRECTION('ref_axis',(1.,0.,0.));
#35503=DIRECTION('',(-0.5,0.866025403784439,0.));
#35504=DIRECTION('center_axis',(0.,0.,1.));
#35505=DIRECTION('ref_axis',(1.,0.,0.));
#35506=DIRECTION('center_axis',(0.,0.,1.));
#35507=DIRECTION('ref_axis',(1.,0.,0.));
#35508=DIRECTION('',(0.5,0.866025403784438,0.));
#35509=DIRECTION('center_axis',(0.,0.,1.));
#35510=DIRECTION('ref_axis',(1.,0.,0.));
#35511=DIRECTION('center_axis',(0.,0.,1.));
#35512=DIRECTION('ref_axis',(1.,0.,0.));
#35513=DIRECTION('',(1.,-1.92296268638356E-16,0.));
#35514=DIRECTION('center_axis',(0.,0.,1.));
#35515=DIRECTION('ref_axis',(1.,0.,0.));
#35516=DIRECTION('center_axis',(0.,0.,1.));
#35517=DIRECTION('ref_axis',(1.,0.,0.));
#35518=DIRECTION('',(-0.857492925712544,-1.05012596676537E-16,0.514495755427527));
#35519=DIRECTION('center_axis',(0.866025403784439,0.5,0.));
#35520=DIRECTION('ref_axis',(0.5,-0.866025403784439,0.));
#35521=DIRECTION('',(0.5,-0.866025403784439,0.));
#35522=DIRECTION('',(0.,0.,-1.));
#35523=DIRECTION('',(0.,0.,-1.));
#35524=DIRECTION('center_axis',(1.92296268638356E-16,1.,0.));
#35525=DIRECTION('ref_axis',(1.,-1.92296268638356E-16,0.));
#35526=DIRECTION('',(1.,-1.92296268638356E-16,0.));
#35527=DIRECTION('',(0.,0.,-1.));
#35528=DIRECTION('center_axis',(-0.866025403784438,0.5,0.));
#35529=DIRECTION('ref_axis',(0.5,0.866025403784438,0.));
#35530=DIRECTION('',(0.5,0.866025403784438,0.));
#35531=DIRECTION('',(0.,0.,-1.));
#35532=DIRECTION('center_axis',(-0.866025403784439,-0.5,0.));
#35533=DIRECTION('ref_axis',(-0.5,0.866025403784439,0.));
#35534=DIRECTION('',(-0.5,0.866025403784439,0.));
#35535=DIRECTION('',(0.,0.,-1.));
#35536=DIRECTION('center_axis',(-1.92296268638356E-16,-1.,0.));
#35537=DIRECTION('ref_axis',(-1.,1.92296268638356E-16,0.));
#35538=DIRECTION('',(-1.,1.92296268638356E-16,0.));
#35539=DIRECTION('',(0.,0.,-1.));
#35540=DIRECTION('center_axis',(0.866025403784439,-0.5,0.));
#35541=DIRECTION('ref_axis',(-0.5,-0.866025403784439,0.));
#35542=DIRECTION('',(-0.5,-0.866025403784439,0.));
#35543=DIRECTION('center_axis',(-0.713210659190727,-0.700949752561999,0.));
#35544=DIRECTION('ref_axis',(-0.700949752561999,0.713210659190727,0.));
#35545=DIRECTION('',(0.,0.,1.));
#35546=DIRECTION('',(-0.700949752561999,0.713210659190727,0.));
#35547=DIRECTION('',(0.,0.,-1.));
#35548=DIRECTION('',(-0.700949752561999,0.713210659190727,0.));
#35549=DIRECTION('center_axis',(0.,0.,1.));
#35550=DIRECTION('ref_axis',(1.,0.,0.));
#35551=DIRECTION('center_axis',(0.,0.,1.));
#35552=DIRECTION('ref_axis',(1.,0.,0.));
#35553=DIRECTION('',(0.995401637679912,0.0957892462865752,0.));
#35554=DIRECTION('center_axis',(-0.0957892462865752,0.995401637679912,0.));
#35555=DIRECTION('ref_axis',(0.995401637679912,0.0957892462865752,0.));
#35556=DIRECTION('',(0.,0.,-1.));
#35557=DIRECTION('',(0.995401637679912,0.0957892462865752,0.));
#35558=DIRECTION('center_axis',(0.,0.,-1.));
#35559=DIRECTION('ref_axis',(-1.,0.,0.));
#35560=DIRECTION('center_axis',(0.,0.,-1.));
#35561=DIRECTION('ref_axis',(1.,0.,0.));
#35562=DIRECTION('center_axis',(-0.909937728342724,-0.414744898146418,0.));
#35563=DIRECTION('ref_axis',(-0.414744898146418,0.909937728342724,0.));
#35564=DIRECTION('',(0.,0.,1.));
#35565=DIRECTION('',(-0.414744898146418,0.909937728342724,0.));
#35566=DIRECTION('',(0.,0.,-1.));
#35567=DIRECTION('',(-0.414744898146418,0.909937728342724,0.));
#35568=DIRECTION('center_axis',(0.,0.,1.));
#35569=DIRECTION('ref_axis',(1.,0.,0.));
#35570=DIRECTION('center_axis',(0.,0.,1.));
#35571=DIRECTION('ref_axis',(1.,0.,0.));
#35572=DIRECTION('',(0.968133425390015,-0.250434962899744,0.));
#35573=DIRECTION('center_axis',(0.250434962899744,0.968133425390015,0.));
#35574=DIRECTION('ref_axis',(0.968133425390015,-0.250434962899744,0.));
#35575=DIRECTION('',(0.,0.,-1.));
#35576=DIRECTION('',(0.968133425390015,-0.250434962899744,0.));
#35577=DIRECTION('center_axis',(0.,0.,-1.));
#35578=DIRECTION('ref_axis',(-1.,0.,0.));
#35579=DIRECTION('center_axis',(0.,0.,-1.));
#35580=DIRECTION('ref_axis',(1.,0.,0.));
#35581=DIRECTION('center_axis',(-0.996912878205979,-0.0785156880315736,
0.));
#35582=DIRECTION('ref_axis',(-0.0785156880315736,0.996912878205979,0.));
#35583=DIRECTION('',(0.,0.,1.));
#35584=DIRECTION('',(-0.0785156880315736,0.996912878205979,0.));
#35585=DIRECTION('',(0.,0.,-1.));
#35586=DIRECTION('',(-0.0785156880315736,0.996912878205979,0.));
#35587=DIRECTION('center_axis',(0.,0.,1.));
#35588=DIRECTION('ref_axis',(1.,0.,0.));
#35589=DIRECTION('center_axis',(0.,0.,1.));
#35590=DIRECTION('ref_axis',(1.,0.,0.));
#35591=DIRECTION('',(0.824094033870449,-0.566453019533952,0.));
#35592=DIRECTION('center_axis',(0.566453019533952,0.824094033870449,0.));
#35593=DIRECTION('ref_axis',(0.824094033870449,-0.566453019533952,0.));
#35594=DIRECTION('',(0.,0.,-1.));
#35595=DIRECTION('',(0.824094033870449,-0.566453019533952,0.));
#35596=DIRECTION('center_axis',(0.,0.,-1.));
#35597=DIRECTION('ref_axis',(-1.,0.,0.));
#35598=DIRECTION('center_axis',(0.,0.,-1.));
#35599=DIRECTION('ref_axis',(1.,0.,0.));
#35600=DIRECTION('center_axis',(-0.963645622090473,0.26718367282801,0.));
#35601=DIRECTION('ref_axis',(0.26718367282801,0.963645622090473,0.));
#35602=DIRECTION('',(0.,0.,1.));
#35603=DIRECTION('',(0.26718367282801,0.963645622090473,0.));
#35604=DIRECTION('',(0.,0.,-1.));
#35605=DIRECTION('',(0.26718367282801,0.963645622090473,0.));
#35606=DIRECTION('center_axis',(0.,0.,1.));
#35607=DIRECTION('ref_axis',(1.,0.,0.));
#35608=DIRECTION('center_axis',(0.,0.,1.));
#35609=DIRECTION('ref_axis',(1.,0.,0.));
#35610=DIRECTION('',(0.580656739533499,-0.814148482056146,0.));
#35611=DIRECTION('center_axis',(0.814148482056146,0.580656739533499,0.));
#35612=DIRECTION('ref_axis',(0.580656739533499,-0.814148482056146,0.));
#35613=DIRECTION('',(0.,0.,-1.));
#35614=DIRECTION('',(0.580656739533499,-0.814148482056146,0.));
#35615=DIRECTION('center_axis',(0.,0.,-1.));
#35616=DIRECTION('ref_axis',(-1.,0.,0.));
#35617=DIRECTION('center_axis',(0.,0.,-1.));
#35618=DIRECTION('ref_axis',(1.,0.,0.));
#35619=DIRECTION('center_axis',(-0.814148482056146,0.580656739533499,0.));
#35620=DIRECTION('ref_axis',(0.580656739533499,0.814148482056146,0.));
#35621=DIRECTION('',(0.,0.,1.));
#35622=DIRECTION('',(0.580656739533499,0.814148482056146,0.));
#35623=DIRECTION('',(0.,0.,-1.));
#35624=DIRECTION('',(0.580656739533499,0.814148482056146,0.));
#35625=DIRECTION('center_axis',(0.,0.,1.));
#35626=DIRECTION('ref_axis',(1.,0.,0.));
#35627=DIRECTION('center_axis',(0.,0.,1.));
#35628=DIRECTION('ref_axis',(1.,0.,0.));
#35629=DIRECTION('',(0.267183672828016,-0.963645622090472,0.));
#35630=DIRECTION('center_axis',(0.963645622090472,0.267183672828016,0.));
#35631=DIRECTION('ref_axis',(0.267183672828016,-0.963645622090472,0.));
#35632=DIRECTION('',(0.,0.,-1.));
#35633=DIRECTION('',(0.267183672828016,-0.963645622090472,0.));
#35634=DIRECTION('center_axis',(0.,0.,-1.));
#35635=DIRECTION('ref_axis',(-1.,0.,0.));
#35636=DIRECTION('center_axis',(0.,0.,-1.));
#35637=DIRECTION('ref_axis',(1.,0.,0.));
#35638=DIRECTION('center_axis',(-0.56645301953395,0.82409403387045,0.));
#35639=DIRECTION('ref_axis',(0.82409403387045,0.56645301953395,0.));
#35640=DIRECTION('',(0.,0.,1.));
#35641=DIRECTION('',(0.82409403387045,0.56645301953395,0.));
#35642=DIRECTION('',(0.,0.,-1.));
#35643=DIRECTION('',(0.82409403387045,0.56645301953395,0.));
#35644=DIRECTION('center_axis',(0.,0.,1.));
#35645=DIRECTION('ref_axis',(1.,0.,0.));
#35646=DIRECTION('center_axis',(0.,0.,1.));
#35647=DIRECTION('ref_axis',(1.,0.,0.));
#35648=DIRECTION('',(-0.0785156880315734,-0.996912878205979,0.));
#35649=DIRECTION('center_axis',(0.996912878205979,-0.0785156880315734,0.));
#35650=DIRECTION('ref_axis',(-0.0785156880315734,-0.996912878205979,0.));
#35651=DIRECTION('',(0.,0.,-1.));
#35652=DIRECTION('',(-0.0785156880315734,-0.996912878205979,0.));
#35653=DIRECTION('center_axis',(0.,0.,-1.));
#35654=DIRECTION('ref_axis',(-1.,0.,0.));
#35655=DIRECTION('center_axis',(0.,0.,-1.));
#35656=DIRECTION('ref_axis',(1.,0.,0.));
#35657=DIRECTION('center_axis',(-0.250434962899748,0.968133425390014,0.));
#35658=DIRECTION('ref_axis',(0.968133425390014,0.250434962899748,0.));
#35659=DIRECTION('',(0.,0.,1.));
#35660=DIRECTION('',(0.968133425390014,0.250434962899748,0.));
#35661=DIRECTION('',(0.,0.,-1.));
#35662=DIRECTION('',(0.968133425390014,0.250434962899748,0.));
#35663=DIRECTION('center_axis',(0.,0.,1.));
#35664=DIRECTION('ref_axis',(1.,0.,0.));
#35665=DIRECTION('center_axis',(0.,0.,1.));
#35666=DIRECTION('ref_axis',(1.,0.,0.));
#35667=DIRECTION('',(-0.414744898146415,-0.909937728342726,0.));
#35668=DIRECTION('center_axis',(0.909937728342726,-0.414744898146415,0.));
#35669=DIRECTION('ref_axis',(-0.414744898146415,-0.909937728342726,0.));
#35670=DIRECTION('',(0.,0.,-1.));
#35671=DIRECTION('',(-0.414744898146415,-0.909937728342726,0.));
#35672=DIRECTION('center_axis',(0.,0.,-1.));
#35673=DIRECTION('ref_axis',(-1.,0.,0.));
#35674=DIRECTION('center_axis',(0.,0.,-1.));
#35675=DIRECTION('ref_axis',(1.,0.,0.));
#35676=DIRECTION('center_axis',(0.0957892462865784,0.995401637679911,0.));
#35677=DIRECTION('ref_axis',(0.995401637679911,-0.0957892462865784,0.));
#35678=DIRECTION('',(0.,0.,1.));
#35679=DIRECTION('',(0.995401637679911,-0.0957892462865784,0.));
#35680=DIRECTION('',(0.,0.,-1.));
#35681=DIRECTION('',(0.995401637679911,-0.0957892462865784,0.));
#35682=DIRECTION('center_axis',(0.,0.,1.));
#35683=DIRECTION('ref_axis',(1.,0.,0.));
#35684=DIRECTION('center_axis',(0.,0.,1.));
#35685=DIRECTION('ref_axis',(1.,0.,0.));
#35686=DIRECTION('',(-0.700949752562001,-0.713210659190726,0.));
#35687=DIRECTION('center_axis',(0.713210659190726,-0.700949752562001,0.));
#35688=DIRECTION('ref_axis',(-0.700949752562001,-0.713210659190726,0.));
#35689=DIRECTION('',(0.,0.,-1.));
#35690=DIRECTION('',(-0.700949752562001,-0.713210659190726,0.));
#35691=DIRECTION('center_axis',(0.,0.,-1.));
#35692=DIRECTION('ref_axis',(-1.,0.,0.));
#35693=DIRECTION('center_axis',(0.,0.,-1.));
#35694=DIRECTION('ref_axis',(1.,0.,0.));
#35695=DIRECTION('center_axis',(0.43045985867203,0.902609721902028,0.));
#35696=DIRECTION('ref_axis',(0.902609721902028,-0.43045985867203,0.));
#35697=DIRECTION('',(0.,0.,1.));
#35698=DIRECTION('',(0.902609721902028,-0.43045985867203,0.));
#35699=DIRECTION('',(0.,0.,-1.));
#35700=DIRECTION('',(0.902609721902028,-0.43045985867203,0.));
#35701=DIRECTION('center_axis',(0.,0.,1.));
#35702=DIRECTION('ref_axis',(1.,0.,0.));
#35703=DIRECTION('center_axis',(0.,0.,1.));
#35704=DIRECTION('ref_axis',(1.,0.,0.));
#35705=DIRECTION('',(-0.902609721902028,-0.43045985867203,0.));
#35706=DIRECTION('center_axis',(0.,0.,1.));
#35707=DIRECTION('ref_axis',(1.,0.,0.));
#35708=DIRECTION('center_axis',(0.43045985867203,-0.902609721902028,0.));
#35709=DIRECTION('ref_axis',(-0.902609721902028,-0.43045985867203,0.));
#35710=DIRECTION('',(0.,0.,-1.));
#35711=DIRECTION('',(-0.902609721902028,-0.43045985867203,0.));
#35712=DIRECTION('center_axis',(0.,0.,-1.));
#35713=DIRECTION('ref_axis',(-1.,0.,0.));
#35714=DIRECTION('center_axis',(0.,0.,-1.));
#35715=DIRECTION('ref_axis',(1.,0.,0.));
#35716=DIRECTION('center_axis',(0.,0.,-1.));
#35717=DIRECTION('ref_axis',(1.,0.,0.));
#35718=DIRECTION('center_axis',(0.580656739533499,0.814148482056146,0.));
#35719=DIRECTION('ref_axis',(0.814148482056146,-0.580656739533499,0.));
#35720=DIRECTION('',(0.,0.,1.));
#35721=DIRECTION('',(0.814148482056146,-0.580656739533499,0.));
#35722=DIRECTION('',(0.,0.,-1.));
#35723=DIRECTION('',(0.814148482056146,-0.580656739533499,0.));
#35724=DIRECTION('center_axis',(0.,0.,1.));
#35725=DIRECTION('ref_axis',(1.,0.,0.));
#35726=DIRECTION('center_axis',(0.,0.,1.));
#35727=DIRECTION('ref_axis',(1.,0.,0.));
#35728=DIRECTION('',(-0.963645622090472,-0.267183672828013,0.));
#35729=DIRECTION('center_axis',(0.267183672828013,-0.963645622090472,0.));
#35730=DIRECTION('ref_axis',(-0.963645622090472,-0.267183672828013,0.));
#35731=DIRECTION('',(0.,0.,-1.));
#35732=DIRECTION('',(-0.963645622090472,-0.267183672828013,0.));
#35733=DIRECTION('center_axis',(0.,0.,-1.));
#35734=DIRECTION('ref_axis',(-1.,0.,0.));
#35735=DIRECTION('center_axis',(0.,0.,-1.));
#35736=DIRECTION('ref_axis',(1.,0.,0.));
#35737=DIRECTION('center_axis',(0.824094033870453,0.566453019533945,0.));
#35738=DIRECTION('ref_axis',(0.566453019533945,-0.824094033870453,0.));
#35739=DIRECTION('',(0.,0.,1.));
#35740=DIRECTION('',(0.566453019533945,-0.824094033870453,0.));
#35741=DIRECTION('',(0.,0.,-1.));
#35742=DIRECTION('',(0.566453019533945,-0.824094033870453,0.));
#35743=DIRECTION('center_axis',(0.,0.,1.));
#35744=DIRECTION('ref_axis',(1.,0.,0.));
#35745=DIRECTION('center_axis',(0.,0.,1.));
#35746=DIRECTION('ref_axis',(1.,0.,0.));
#35747=DIRECTION('',(-0.996912878205979,0.078515688031577,0.));
#35748=DIRECTION('center_axis',(-0.078515688031577,-0.996912878205979,0.));
#35749=DIRECTION('ref_axis',(-0.996912878205979,0.078515688031577,0.));
#35750=DIRECTION('',(0.,0.,-1.));
#35751=DIRECTION('',(-0.996912878205979,0.078515688031577,0.));
#35752=DIRECTION('center_axis',(0.,0.,-1.));
#35753=DIRECTION('ref_axis',(-1.,0.,0.));
#35754=DIRECTION('center_axis',(0.,0.,-1.));
#35755=DIRECTION('ref_axis',(1.,0.,0.));
#35756=DIRECTION('center_axis',(0.968133425390014,0.250434962899747,0.));
#35757=DIRECTION('ref_axis',(0.250434962899747,-0.968133425390014,0.));
#35758=DIRECTION('',(0.,0.,1.));
#35759=DIRECTION('',(0.250434962899747,-0.968133425390014,0.));
#35760=DIRECTION('',(0.,0.,-1.));
#35761=DIRECTION('',(0.250434962899747,-0.968133425390014,0.));
#35762=DIRECTION('center_axis',(0.,0.,1.));
#35763=DIRECTION('ref_axis',(1.,0.,0.));
#35764=DIRECTION('center_axis',(0.,0.,1.));
#35765=DIRECTION('ref_axis',(1.,0.,0.));
#35766=DIRECTION('',(-0.909937728342725,0.414744898146415,0.));
#35767=DIRECTION('center_axis',(-0.414744898146415,-0.909937728342725,0.));
#35768=DIRECTION('ref_axis',(-0.909937728342725,0.414744898146415,0.));
#35769=DIRECTION('',(0.,0.,-1.));
#35770=DIRECTION('',(-0.909937728342725,0.414744898146415,0.));
#35771=DIRECTION('center_axis',(0.,0.,-1.));
#35772=DIRECTION('ref_axis',(-1.,0.,0.));
#35773=DIRECTION('center_axis',(0.,0.,-1.));
#35774=DIRECTION('ref_axis',(1.,0.,0.));
#35775=DIRECTION('center_axis',(0.995401637679911,-0.0957892462865797,0.));
#35776=DIRECTION('ref_axis',(-0.0957892462865797,-0.995401637679911,0.));
#35777=DIRECTION('',(0.,0.,1.));
#35778=DIRECTION('',(-0.0957892462865797,-0.995401637679911,0.));
#35779=DIRECTION('',(0.,0.,-1.));
#35780=DIRECTION('',(-0.0957892462865797,-0.995401637679911,0.));
#35781=DIRECTION('center_axis',(0.,0.,1.));
#35782=DIRECTION('ref_axis',(1.,0.,0.));
#35783=DIRECTION('center_axis',(0.,0.,1.));
#35784=DIRECTION('ref_axis',(1.,0.,0.));
#35785=DIRECTION('',(-0.713210659190727,0.700949752562,0.));
#35786=DIRECTION('center_axis',(-0.700949752562,-0.713210659190727,0.));
#35787=DIRECTION('ref_axis',(-0.713210659190727,0.700949752562,0.));
#35788=DIRECTION('',(0.,0.,-1.));
#35789=DIRECTION('',(-0.713210659190727,0.700949752562,0.));
#35790=DIRECTION('center_axis',(0.,0.,-1.));
#35791=DIRECTION('ref_axis',(-1.,0.,0.));
#35792=DIRECTION('center_axis',(0.,0.,-1.));
#35793=DIRECTION('ref_axis',(1.,0.,0.));
#35794=DIRECTION('center_axis',(0.902609721902027,-0.430459858672031,0.));
#35795=DIRECTION('ref_axis',(-0.430459858672031,-0.902609721902027,0.));
#35796=DIRECTION('',(0.,0.,1.));
#35797=DIRECTION('',(-0.430459858672031,-0.902609721902027,0.));
#35798=DIRECTION('',(0.,0.,-1.));
#35799=DIRECTION('',(-0.430459858672031,-0.902609721902027,0.));
#35800=DIRECTION('center_axis',(0.,0.,1.));
#35801=DIRECTION('ref_axis',(1.,0.,0.));
#35802=DIRECTION('center_axis',(0.,0.,1.));
#35803=DIRECTION('ref_axis',(1.,0.,0.));
#35804=DIRECTION('',(-0.430459858672031,0.902609721902027,0.));
#35805=DIRECTION('center_axis',(-0.902609721902027,-0.430459858672031,0.));
#35806=DIRECTION('ref_axis',(-0.430459858672031,0.902609721902027,0.));
#35807=DIRECTION('',(0.,0.,-1.));
#35808=DIRECTION('',(-0.430459858672031,0.902609721902027,0.));
#35809=DIRECTION('center_axis',(0.,0.,-1.));
#35810=DIRECTION('ref_axis',(-1.,0.,0.));
#35811=DIRECTION('center_axis',(0.,0.,-1.));
#35812=DIRECTION('ref_axis',(1.,0.,0.));
#35813=DIRECTION('center_axis',(0.700949752562001,-0.713210659190726,0.));
#35814=DIRECTION('ref_axis',(-0.713210659190726,-0.700949752562001,0.));
#35815=DIRECTION('',(0.,0.,1.));
#35816=DIRECTION('',(-0.713210659190726,-0.700949752562001,0.));
#35817=DIRECTION('',(0.,0.,-1.));
#35818=DIRECTION('',(-0.713210659190726,-0.700949752562001,0.));
#35819=DIRECTION('center_axis',(0.,0.,1.));
#35820=DIRECTION('ref_axis',(1.,0.,0.));
#35821=DIRECTION('center_axis',(0.,0.,1.));
#35822=DIRECTION('ref_axis',(1.,0.,0.));
#35823=DIRECTION('',(-0.0957892462865797,0.995401637679911,0.));
#35824=DIRECTION('center_axis',(-0.995401637679911,-0.0957892462865797,
0.));
#35825=DIRECTION('ref_axis',(-0.0957892462865797,0.995401637679911,0.));
#35826=DIRECTION('',(0.,0.,-1.));
#35827=DIRECTION('',(-0.0957892462865797,0.995401637679911,0.));
#35828=DIRECTION('center_axis',(0.,0.,-1.));
#35829=DIRECTION('ref_axis',(-1.,0.,0.));
#35830=DIRECTION('center_axis',(0.,0.,-1.));
#35831=DIRECTION('ref_axis',(1.,0.,0.));
#35832=DIRECTION('center_axis',(0.414744898146414,-0.909937728342726,0.));
#35833=DIRECTION('ref_axis',(-0.909937728342726,-0.414744898146414,0.));
#35834=DIRECTION('',(0.,0.,1.));
#35835=DIRECTION('',(-0.909937728342726,-0.414744898146414,0.));
#35836=DIRECTION('',(0.,0.,-1.));
#35837=DIRECTION('',(-0.909937728342726,-0.414744898146414,0.));
#35838=DIRECTION('center_axis',(0.,0.,1.));
#35839=DIRECTION('ref_axis',(1.,0.,0.));
#35840=DIRECTION('center_axis',(0.,0.,1.));
#35841=DIRECTION('ref_axis',(1.,0.,0.));
#35842=DIRECTION('',(0.250434962899747,0.968133425390014,0.));
#35843=DIRECTION('center_axis',(-0.968133425390014,0.250434962899747,0.));
#35844=DIRECTION('ref_axis',(0.250434962899747,0.968133425390014,0.));
#35845=DIRECTION('',(0.,0.,-1.));
#35846=DIRECTION('',(0.250434962899747,0.968133425390014,0.));
#35847=DIRECTION('center_axis',(0.,0.,-1.));
#35848=DIRECTION('ref_axis',(-1.,0.,0.));
#35849=DIRECTION('center_axis',(0.,0.,-1.));
#35850=DIRECTION('ref_axis',(1.,0.,0.));
#35851=DIRECTION('center_axis',(0.078515688031576,-0.996912878205979,0.));
#35852=DIRECTION('ref_axis',(-0.996912878205979,-0.078515688031576,0.));
#35853=DIRECTION('',(0.,0.,1.));
#35854=DIRECTION('',(-0.996912878205979,-0.078515688031576,0.));
#35855=DIRECTION('',(0.,0.,-1.));
#35856=DIRECTION('',(-0.996912878205979,-0.078515688031576,0.));
#35857=DIRECTION('center_axis',(0.,0.,1.));
#35858=DIRECTION('ref_axis',(1.,0.,0.));
#35859=DIRECTION('center_axis',(0.,0.,1.));
#35860=DIRECTION('ref_axis',(1.,0.,0.));
#35861=DIRECTION('',(0.566453019533946,0.824094033870453,0.));
#35862=DIRECTION('center_axis',(-0.824094033870453,0.566453019533946,0.));
#35863=DIRECTION('ref_axis',(0.566453019533946,0.824094033870453,0.));
#35864=DIRECTION('',(0.,0.,-1.));
#35865=DIRECTION('',(0.566453019533946,0.824094033870453,0.));
#35866=DIRECTION('center_axis',(0.,0.,-1.));
#35867=DIRECTION('ref_axis',(-1.,0.,0.));
#35868=DIRECTION('center_axis',(0.,0.,-1.));
#35869=DIRECTION('ref_axis',(1.,0.,0.));
#35870=DIRECTION('center_axis',(-0.267183672828014,-0.963645622090472,0.));
#35871=DIRECTION('ref_axis',(-0.963645622090472,0.267183672828014,0.));
#35872=DIRECTION('',(0.,0.,1.));
#35873=DIRECTION('',(-0.963645622090472,0.267183672828014,0.));
#35874=DIRECTION('',(0.,0.,-1.));
#35875=DIRECTION('',(-0.963645622090472,0.267183672828014,0.));
#35876=DIRECTION('center_axis',(0.,0.,1.));
#35877=DIRECTION('ref_axis',(1.,0.,0.));
#35878=DIRECTION('center_axis',(0.,0.,1.));
#35879=DIRECTION('ref_axis',(1.,0.,0.));
#35880=DIRECTION('',(0.814148482056147,0.580656739533497,0.));
#35881=DIRECTION('center_axis',(-0.580656739533497,0.814148482056147,0.));
#35882=DIRECTION('ref_axis',(0.814148482056147,0.580656739533497,0.));
#35883=DIRECTION('',(0.,0.,-1.));
#35884=DIRECTION('',(0.814148482056147,0.580656739533497,0.));
#35885=DIRECTION('center_axis',(0.,0.,-1.));
#35886=DIRECTION('ref_axis',(-1.,0.,0.));
#35887=DIRECTION('center_axis',(0.,0.,-1.));
#35888=DIRECTION('ref_axis',(1.,0.,0.));
#35889=DIRECTION('center_axis',(-0.0957892462865788,-0.995401637679911,
0.));
#35890=DIRECTION('ref_axis',(-0.995401637679911,0.0957892462865788,0.));
#35891=DIRECTION('',(0.,0.,1.));
#35892=DIRECTION('',(-0.995401637679911,0.0957892462865788,0.));
#35893=DIRECTION('',(0.,0.,-1.));
#35894=DIRECTION('',(-0.995401637679911,0.0957892462865788,0.));
#35895=DIRECTION('center_axis',(0.,0.,1.));
#35896=DIRECTION('ref_axis',(1.,0.,0.));
#35897=DIRECTION('center_axis',(0.,0.,1.));
#35898=DIRECTION('ref_axis',(1.,0.,0.));
#35899=DIRECTION('',(0.700949752562,0.713210659190726,0.));
#35900=DIRECTION('center_axis',(-0.713210659190726,0.700949752562,0.));
#35901=DIRECTION('ref_axis',(0.700949752562,0.713210659190726,0.));
#35902=DIRECTION('',(0.,0.,-1.));
#35903=DIRECTION('',(0.700949752562,0.713210659190726,0.));
#35904=DIRECTION('center_axis',(0.,0.,-1.));
#35905=DIRECTION('ref_axis',(-1.,0.,0.));
#35906=DIRECTION('center_axis',(0.,0.,-1.));
#35907=DIRECTION('ref_axis',(1.,0.,0.));
#35908=DIRECTION('center_axis',(0.250434962899746,-0.968133425390014,0.));
#35909=DIRECTION('ref_axis',(-0.968133425390014,-0.250434962899746,0.));
#35910=DIRECTION('',(0.,0.,1.));
#35911=DIRECTION('',(-0.968133425390014,-0.250434962899746,0.));
#35912=DIRECTION('',(0.,0.,-1.));
#35913=DIRECTION('',(-0.968133425390014,-0.250434962899746,0.));
#35914=DIRECTION('center_axis',(0.,0.,1.));
#35915=DIRECTION('ref_axis',(1.,0.,0.));
#35916=DIRECTION('center_axis',(0.,0.,1.));
#35917=DIRECTION('ref_axis',(1.,0.,0.));
#35918=DIRECTION('',(0.414744898146414,0.909937728342726,0.));
#35919=DIRECTION('center_axis',(-0.909937728342726,0.414744898146414,0.));
#35920=DIRECTION('ref_axis',(0.414744898146414,0.909937728342726,0.));
#35921=DIRECTION('',(0.,0.,-1.));
#35922=DIRECTION('',(0.414744898146414,0.909937728342726,0.));
#35923=DIRECTION('center_axis',(0.,0.,-1.));
#35924=DIRECTION('ref_axis',(-1.,0.,0.));
#35925=DIRECTION('center_axis',(0.,0.,-1.));
#35926=DIRECTION('ref_axis',(1.,0.,0.));
#35927=DIRECTION('center_axis',(0.566453019533948,-0.824094033870452,0.));
#35928=DIRECTION('ref_axis',(-0.824094033870452,-0.566453019533948,0.));
#35929=DIRECTION('',(0.,0.,1.));
#35930=DIRECTION('',(-0.824094033870452,-0.566453019533948,0.));
#35931=DIRECTION('',(0.,0.,-1.));
#35932=DIRECTION('',(-0.824094033870452,-0.566453019533948,0.));
#35933=DIRECTION('center_axis',(0.,0.,1.));
#35934=DIRECTION('ref_axis',(1.,0.,0.));
#35935=DIRECTION('center_axis',(0.,0.,1.));
#35936=DIRECTION('ref_axis',(1.,0.,0.));
#35937=DIRECTION('',(0.0785156880315752,0.996912878205979,0.));
#35938=DIRECTION('center_axis',(-0.996912878205979,0.0785156880315752,0.));
#35939=DIRECTION('ref_axis',(0.0785156880315752,0.996912878205979,0.));
#35940=DIRECTION('',(0.,0.,-1.));
#35941=DIRECTION('',(0.0785156880315752,0.996912878205979,0.));
#35942=DIRECTION('center_axis',(0.,0.,-1.));
#35943=DIRECTION('ref_axis',(-1.,0.,0.));
#35944=DIRECTION('center_axis',(0.,0.,-1.));
#35945=DIRECTION('ref_axis',(1.,0.,0.));
#35946=DIRECTION('center_axis',(0.814148482056148,-0.580656739533496,0.));
#35947=DIRECTION('ref_axis',(-0.580656739533496,-0.814148482056148,0.));
#35948=DIRECTION('',(0.,0.,1.));
#35949=DIRECTION('',(-0.580656739533496,-0.814148482056148,0.));
#35950=DIRECTION('',(0.,0.,-1.));
#35951=DIRECTION('',(-0.580656739533496,-0.814148482056148,0.));
#35952=DIRECTION('center_axis',(0.,0.,1.));
#35953=DIRECTION('ref_axis',(1.,0.,0.));
#35954=DIRECTION('center_axis',(0.,0.,1.));
#35955=DIRECTION('ref_axis',(1.,0.,0.));
#35956=DIRECTION('',(-0.267183672828014,0.963645622090472,0.));
#35957=DIRECTION('center_axis',(-0.963645622090472,-0.267183672828014,0.));
#35958=DIRECTION('ref_axis',(-0.267183672828014,0.963645622090472,0.));
#35959=DIRECTION('',(0.,0.,-1.));
#35960=DIRECTION('',(-0.267183672828014,0.963645622090472,0.));
#35961=DIRECTION('center_axis',(0.,0.,-1.));
#35962=DIRECTION('ref_axis',(-1.,0.,0.));
#35963=DIRECTION('center_axis',(0.,0.,-1.));
#35964=DIRECTION('ref_axis',(1.,0.,0.));
#35965=DIRECTION('center_axis',(0.963645622090472,-0.267183672828014,0.));
#35966=DIRECTION('ref_axis',(-0.267183672828014,-0.963645622090472,0.));
#35967=DIRECTION('',(0.,0.,1.));
#35968=DIRECTION('',(-0.267183672828014,-0.963645622090472,0.));
#35969=DIRECTION('',(0.,0.,-1.));
#35970=DIRECTION('',(-0.267183672828014,-0.963645622090472,0.));
#35971=DIRECTION('center_axis',(0.,0.,1.));
#35972=DIRECTION('ref_axis',(1.,0.,0.));
#35973=DIRECTION('center_axis',(0.,0.,1.));
#35974=DIRECTION('ref_axis',(1.,0.,0.));
#35975=DIRECTION('',(-0.580656739533497,0.814148482056147,0.));
#35976=DIRECTION('center_axis',(-0.814148482056147,-0.580656739533497,0.));
#35977=DIRECTION('ref_axis',(-0.580656739533497,0.814148482056147,0.));
#35978=DIRECTION('',(0.,0.,-1.));
#35979=DIRECTION('',(-0.580656739533497,0.814148482056147,0.));
#35980=DIRECTION('center_axis',(0.,0.,-1.));
#35981=DIRECTION('ref_axis',(-1.,0.,0.));
#35982=DIRECTION('center_axis',(0.,0.,-1.));
#35983=DIRECTION('ref_axis',(1.,0.,0.));
#35984=DIRECTION('center_axis',(0.996912878205979,0.078515688031576,0.));
#35985=DIRECTION('ref_axis',(0.078515688031576,-0.996912878205979,0.));
#35986=DIRECTION('',(0.,0.,1.));
#35987=DIRECTION('',(0.078515688031576,-0.996912878205979,0.));
#35988=DIRECTION('',(0.,0.,-1.));
#35989=DIRECTION('',(0.078515688031576,-0.996912878205979,0.));
#35990=DIRECTION('center_axis',(0.,0.,1.));
#35991=DIRECTION('ref_axis',(1.,0.,0.));
#35992=DIRECTION('center_axis',(0.,0.,1.));
#35993=DIRECTION('ref_axis',(1.,0.,0.));
#35994=DIRECTION('',(-0.824094033870453,0.566453019533946,0.));
#35995=DIRECTION('center_axis',(-0.566453019533946,-0.824094033870453,0.));
#35996=DIRECTION('ref_axis',(-0.824094033870453,0.566453019533946,0.));
#35997=DIRECTION('',(0.,0.,-1.));
#35998=DIRECTION('',(-0.824094033870453,0.566453019533946,0.));
#35999=DIRECTION('center_axis',(0.,0.,-1.));
#36000=DIRECTION('ref_axis',(-1.,0.,0.));
#36001=DIRECTION('center_axis',(0.,0.,-1.));
#36002=DIRECTION('ref_axis',(1.,0.,0.));
#36003=DIRECTION('center_axis',(0.909937728342726,0.414744898146415,0.));
#36004=DIRECTION('ref_axis',(0.414744898146415,-0.909937728342726,0.));
#36005=DIRECTION('',(0.,0.,1.));
#36006=DIRECTION('',(0.414744898146415,-0.909937728342726,0.));
#36007=DIRECTION('',(0.,0.,-1.));
#36008=DIRECTION('',(0.414744898146415,-0.909937728342726,0.));
#36009=DIRECTION('center_axis',(0.,0.,1.));
#36010=DIRECTION('ref_axis',(1.,0.,0.));
#36011=DIRECTION('center_axis',(0.,0.,1.));
#36012=DIRECTION('ref_axis',(1.,0.,0.));
#36013=DIRECTION('',(-0.968133425390015,0.250434962899744,0.));
#36014=DIRECTION('center_axis',(-0.250434962899744,-0.968133425390015,0.));
#36015=DIRECTION('ref_axis',(-0.968133425390015,0.250434962899744,0.));
#36016=DIRECTION('',(0.,0.,-1.));
#36017=DIRECTION('',(-0.968133425390015,0.250434962899744,0.));
#36018=DIRECTION('center_axis',(0.,0.,-1.));
#36019=DIRECTION('ref_axis',(-1.,0.,0.));
#36020=DIRECTION('center_axis',(0.,0.,-1.));
#36021=DIRECTION('ref_axis',(1.,0.,0.));
#36022=DIRECTION('center_axis',(0.713210659190726,0.700949752562001,0.));
#36023=DIRECTION('ref_axis',(0.700949752562001,-0.713210659190726,0.));
#36024=DIRECTION('',(0.,0.,1.));
#36025=DIRECTION('',(0.700949752562001,-0.713210659190726,0.));
#36026=DIRECTION('',(0.,0.,-1.));
#36027=DIRECTION('',(0.700949752562001,-0.713210659190726,0.));
#36028=DIRECTION('center_axis',(0.,0.,1.));
#36029=DIRECTION('ref_axis',(1.,0.,0.));
#36030=DIRECTION('center_axis',(0.,0.,1.));
#36031=DIRECTION('ref_axis',(1.,0.,0.));
#36032=DIRECTION('',(-0.995401637679911,-0.0957892462865814,0.));
#36033=DIRECTION('center_axis',(0.0957892462865814,-0.995401637679911,0.));
#36034=DIRECTION('ref_axis',(-0.995401637679911,-0.0957892462865814,0.));
#36035=DIRECTION('',(0.,0.,-1.));
#36036=DIRECTION('',(-0.995401637679911,-0.0957892462865814,0.));
#36037=DIRECTION('center_axis',(0.,0.,-1.));
#36038=DIRECTION('ref_axis',(-1.,0.,0.));
#36039=DIRECTION('center_axis',(0.,0.,-1.));
#36040=DIRECTION('ref_axis',(1.,0.,0.));
#36041=DIRECTION('center_axis',(0.,0.,1.));
#36042=DIRECTION('ref_axis',(1.,0.,0.));
#36043=DIRECTION('center_axis',(0.,0.,1.));
#36044=DIRECTION('ref_axis',(1.,0.,0.));
#36045=DIRECTION('',(-0.902609721902027,0.430459858672031,0.));
#36046=DIRECTION('',(0.902609721902027,0.430459858672031,0.));
#36047=DIRECTION('center_axis',(-0.430459858672031,-0.902609721902027,0.));
#36048=DIRECTION('ref_axis',(-0.902609721902027,0.430459858672031,0.));
#36049=DIRECTION('',(0.,0.,1.));
#36050=DIRECTION('',(-0.902609721902027,0.430459858672031,0.));
#36051=DIRECTION('',(0.,0.,-1.));
#36052=DIRECTION('center_axis',(-0.430459858672031,0.902609721902027,0.));
#36053=DIRECTION('ref_axis',(0.902609721902027,0.430459858672031,0.));
#36054=DIRECTION('',(0.,0.,-1.));
#36055=DIRECTION('',(0.902609721902027,0.430459858672031,0.));
#36056=DIRECTION('center_axis',(0.,0.,-1.));
#36057=DIRECTION('ref_axis',(-1.,0.,0.));
#36058=DIRECTION('center_axis',(0.,0.,-1.));
#36059=DIRECTION('ref_axis',(1.,0.,0.));
#36060=DIRECTION('center_axis',(0.267183672828015,0.963645622090472,0.));
#36061=DIRECTION('ref_axis',(0.963645622090472,-0.267183672828015,0.));
#36062=DIRECTION('',(0.,0.,1.));
#36063=DIRECTION('',(0.963645622090472,-0.267183672828015,0.));
#36064=DIRECTION('',(0.,0.,-1.));
#36065=DIRECTION('',(0.963645622090472,-0.267183672828015,0.));
#36066=DIRECTION('center_axis',(0.,0.,1.));
#36067=DIRECTION('ref_axis',(1.,0.,0.));
#36068=DIRECTION('center_axis',(0.,0.,1.));
#36069=DIRECTION('ref_axis',(1.,0.,0.));
#36070=DIRECTION('',(-0.814148482056148,-0.580656739533496,0.));
#36071=DIRECTION('center_axis',(0.580656739533496,-0.814148482056148,0.));
#36072=DIRECTION('ref_axis',(-0.814148482056148,-0.580656739533496,0.));
#36073=DIRECTION('',(0.,0.,-1.));
#36074=DIRECTION('',(-0.814148482056148,-0.580656739533496,0.));
#36075=DIRECTION('center_axis',(0.,0.,-1.));
#36076=DIRECTION('ref_axis',(-1.,0.,0.));
#36077=DIRECTION('center_axis',(0.,0.,-1.));
#36078=DIRECTION('ref_axis',(1.,0.,0.));
#36079=DIRECTION('center_axis',(-0.0785156880315738,0.996912878205979,0.));
#36080=DIRECTION('ref_axis',(0.996912878205979,0.0785156880315738,0.));
#36081=DIRECTION('',(0.,0.,1.));
#36082=DIRECTION('',(0.996912878205979,0.0785156880315738,0.));
#36083=DIRECTION('',(0.,0.,-1.));
#36084=DIRECTION('',(0.996912878205979,0.0785156880315738,0.));
#36085=DIRECTION('center_axis',(0.,0.,1.));
#36086=DIRECTION('ref_axis',(1.,0.,0.));
#36087=DIRECTION('center_axis',(0.,0.,1.));
#36088=DIRECTION('ref_axis',(1.,0.,0.));
#36089=DIRECTION('',(-0.566453019533948,-0.824094033870452,0.));
#36090=DIRECTION('center_axis',(0.824094033870452,-0.566453019533948,0.));
#36091=DIRECTION('ref_axis',(-0.566453019533948,-0.824094033870452,0.));
#36092=DIRECTION('',(0.,0.,-1.));
#36093=DIRECTION('',(-0.566453019533948,-0.824094033870452,0.));
#36094=DIRECTION('center_axis',(0.,0.,-1.));
#36095=DIRECTION('ref_axis',(-1.,0.,0.));
#36096=DIRECTION('center_axis',(0.,0.,-1.));
#36097=DIRECTION('ref_axis',(1.,0.,0.));
#36098=DIRECTION('center_axis',(-0.414744898146415,0.909937728342726,0.));
#36099=DIRECTION('ref_axis',(0.909937728342726,0.414744898146415,0.));
#36100=DIRECTION('',(0.,0.,1.));
#36101=DIRECTION('',(0.909937728342726,0.414744898146415,0.));
#36102=DIRECTION('',(0.,0.,-1.));
#36103=DIRECTION('',(0.909937728342726,0.414744898146415,0.));
#36104=DIRECTION('center_axis',(0.,0.,1.));
#36105=DIRECTION('ref_axis',(1.,0.,0.));
#36106=DIRECTION('center_axis',(0.,0.,1.));
#36107=DIRECTION('ref_axis',(1.,0.,0.));
#36108=DIRECTION('',(-0.250434962899745,-0.968133425390015,0.));
#36109=DIRECTION('center_axis',(0.968133425390015,-0.250434962899745,0.));
#36110=DIRECTION('ref_axis',(-0.250434962899745,-0.968133425390015,0.));
#36111=DIRECTION('',(0.,0.,-1.));
#36112=DIRECTION('',(-0.250434962899745,-0.968133425390015,0.));
#36113=DIRECTION('center_axis',(0.,0.,-1.));
#36114=DIRECTION('ref_axis',(-1.,0.,0.));
#36115=DIRECTION('center_axis',(0.,0.,-1.));
#36116=DIRECTION('ref_axis',(1.,0.,0.));
#36117=DIRECTION('center_axis',(-0.700949752561999,0.713210659190727,0.));
#36118=DIRECTION('ref_axis',(0.713210659190727,0.700949752561999,0.));
#36119=DIRECTION('',(0.,0.,1.));
#36120=DIRECTION('',(0.713210659190727,0.700949752561999,0.));
#36121=DIRECTION('',(0.,0.,-1.));
#36122=DIRECTION('',(0.713210659190727,0.700949752561999,0.));
#36123=DIRECTION('center_axis',(0.,0.,1.));
#36124=DIRECTION('ref_axis',(1.,0.,0.));
#36125=DIRECTION('center_axis',(0.,0.,1.));
#36126=DIRECTION('ref_axis',(1.,0.,0.));
#36127=DIRECTION('',(0.0957892462865748,-0.995401637679912,0.));
#36128=DIRECTION('center_axis',(0.995401637679912,0.0957892462865748,0.));
#36129=DIRECTION('ref_axis',(0.0957892462865748,-0.995401637679912,0.));
#36130=DIRECTION('',(0.,0.,-1.));
#36131=DIRECTION('',(0.0957892462865748,-0.995401637679912,0.));
#36132=DIRECTION('center_axis',(0.,0.,-1.));
#36133=DIRECTION('ref_axis',(-1.,0.,0.));
#36134=DIRECTION('center_axis',(0.,0.,-1.));
#36135=DIRECTION('ref_axis',(1.,0.,0.));
#36136=DIRECTION('center_axis',(-0.902609721902026,0.430459858672033,0.));
#36137=DIRECTION('ref_axis',(0.430459858672033,0.902609721902026,0.));
#36138=DIRECTION('',(0.,0.,1.));
#36139=DIRECTION('',(0.430459858672033,0.902609721902026,0.));
#36140=DIRECTION('',(0.,0.,-1.));
#36141=DIRECTION('',(0.430459858672033,0.902609721902026,0.));
#36142=DIRECTION('center_axis',(0.,0.,1.));
#36143=DIRECTION('ref_axis',(1.,0.,0.));
#36144=DIRECTION('center_axis',(0.,0.,1.));
#36145=DIRECTION('ref_axis',(1.,0.,0.));
#36146=DIRECTION('',(0.430459858672033,-0.902609721902027,0.));
#36147=DIRECTION('center_axis',(0.902609721902027,0.430459858672033,0.));
#36148=DIRECTION('ref_axis',(0.430459858672033,-0.902609721902027,0.));
#36149=DIRECTION('',(0.,0.,-1.));
#36150=DIRECTION('',(0.430459858672033,-0.902609721902027,0.));
#36151=DIRECTION('center_axis',(0.,0.,-1.));
#36152=DIRECTION('ref_axis',(-1.,0.,0.));
#36153=DIRECTION('center_axis',(0.,0.,-1.));
#36154=DIRECTION('ref_axis',(1.,0.,0.));
#36155=DIRECTION('center_axis',(-0.995401637679911,0.0957892462865809,0.));
#36156=DIRECTION('ref_axis',(0.0957892462865809,0.995401637679911,0.));
#36157=DIRECTION('',(0.,0.,1.));
#36158=DIRECTION('',(0.0957892462865809,0.995401637679911,0.));
#36159=DIRECTION('',(0.,0.,-1.));
#36160=DIRECTION('',(0.0957892462865809,0.995401637679911,0.));
#36161=DIRECTION('center_axis',(0.,0.,1.));
#36162=DIRECTION('ref_axis',(1.,0.,0.));
#36163=DIRECTION('center_axis',(0.,0.,1.));
#36164=DIRECTION('ref_axis',(1.,0.,0.));
#36165=DIRECTION('',(0.713210659190723,-0.700949752562004,0.));
#36166=DIRECTION('center_axis',(0.700949752562004,0.713210659190723,0.));
#36167=DIRECTION('ref_axis',(0.713210659190723,-0.700949752562004,0.));
#36168=DIRECTION('',(0.,0.,-1.));
#36169=DIRECTION('',(0.713210659190723,-0.700949752562004,0.));
#36170=DIRECTION('center_axis',(0.,0.,-1.));
#36171=DIRECTION('ref_axis',(-1.,0.,0.));
#36172=DIRECTION('center_axis',(0.,0.,-1.));
#36173=DIRECTION('ref_axis',(1.,0.,0.));
#36174=DIRECTION('center_axis',(-0.968133425390015,-0.250434962899744,0.));
#36175=DIRECTION('ref_axis',(-0.250434962899744,0.968133425390015,0.));
#36176=DIRECTION('',(0.,0.,1.));
#36177=DIRECTION('',(-0.250434962899744,0.968133425390015,0.));
#36178=DIRECTION('',(0.,0.,-1.));
#36179=DIRECTION('',(-0.250434962899744,0.968133425390015,0.));
#36180=DIRECTION('center_axis',(0.,0.,1.));
#36181=DIRECTION('ref_axis',(1.,0.,0.));
#36182=DIRECTION('center_axis',(0.,0.,1.));
#36183=DIRECTION('ref_axis',(1.,0.,0.));
#36184=DIRECTION('',(0.909937728342727,-0.414744898146412,0.));
#36185=DIRECTION('center_axis',(0.414744898146412,0.909937728342727,0.));
#36186=DIRECTION('ref_axis',(0.909937728342727,-0.414744898146412,0.));
#36187=DIRECTION('',(0.,0.,-1.));
#36188=DIRECTION('',(0.909937728342727,-0.414744898146412,0.));
#36189=DIRECTION('center_axis',(0.,0.,-1.));
#36190=DIRECTION('ref_axis',(-1.,0.,0.));
#36191=DIRECTION('center_axis',(0.,0.,-1.));
#36192=DIRECTION('ref_axis',(1.,0.,0.));
#36193=DIRECTION('center_axis',(-0.82409403387045,-0.56645301953395,0.));
#36194=DIRECTION('ref_axis',(-0.56645301953395,0.82409403387045,0.));
#36195=DIRECTION('',(0.,0.,1.));
#36196=DIRECTION('',(-0.56645301953395,0.82409403387045,0.));
#36197=DIRECTION('',(0.,0.,-1.));
#36198=DIRECTION('',(-0.56645301953395,0.82409403387045,0.));
#36199=DIRECTION('center_axis',(0.,0.,1.));
#36200=DIRECTION('ref_axis',(1.,0.,0.));
#36201=DIRECTION('center_axis',(0.,0.,1.));
#36202=DIRECTION('ref_axis',(1.,0.,0.));
#36203=DIRECTION('',(0.996912878205979,-0.0785156880315738,0.));
#36204=DIRECTION('center_axis',(0.0785156880315738,0.996912878205979,0.));
#36205=DIRECTION('ref_axis',(0.996912878205979,-0.0785156880315738,0.));
#36206=DIRECTION('',(0.,0.,-1.));
#36207=DIRECTION('',(0.996912878205979,-0.0785156880315738,0.));
#36208=DIRECTION('center_axis',(0.,0.,-1.));
#36209=DIRECTION('ref_axis',(-1.,0.,0.));
#36210=DIRECTION('center_axis',(0.,0.,-1.));
#36211=DIRECTION('ref_axis',(1.,0.,0.));
#36212=DIRECTION('center_axis',(-0.580656739533499,-0.814148482056146,0.));
#36213=DIRECTION('ref_axis',(-0.814148482056146,0.580656739533499,0.));
#36214=DIRECTION('',(0.,0.,1.));
#36215=DIRECTION('',(-0.814148482056146,0.580656739533499,0.));
#36216=DIRECTION('',(0.,0.,-1.));
#36217=DIRECTION('',(-0.814148482056146,0.580656739533499,0.));
#36218=DIRECTION('center_axis',(0.,0.,1.));
#36219=DIRECTION('ref_axis',(1.,0.,0.));
#36220=DIRECTION('center_axis',(0.,0.,1.));
#36221=DIRECTION('ref_axis',(1.,0.,0.));
#36222=DIRECTION('',(0.963645622090472,0.267183672828016,0.));
#36223=DIRECTION('center_axis',(-0.267183672828016,0.963645622090472,0.));
#36224=DIRECTION('ref_axis',(0.963645622090472,0.267183672828016,0.));
#36225=DIRECTION('',(0.,0.,-1.));
#36226=DIRECTION('',(0.963645622090472,0.267183672828016,0.));
#36227=DIRECTION('center_axis',(0.,0.,-1.));
#36228=DIRECTION('ref_axis',(-1.,0.,0.));
#36229=DIRECTION('center_axis',(0.,0.,-1.));
#36230=DIRECTION('ref_axis',(1.,0.,0.));
#36231=DIRECTION('center_axis',(0.,0.,-1.));
#36232=DIRECTION('ref_axis',(-1.,0.,0.));
#36233=DIRECTION('center_axis',(0.,0.,1.));
#36234=DIRECTION('ref_axis',(1.,0.,0.));
#36235=DIRECTION('center_axis',(0.,0.,1.));
#36236=DIRECTION('ref_axis',(1.,0.,0.));
#36237=DIRECTION('',(0.707106781186547,8.65956056235493E-17,-0.707106781186548));
#36238=DIRECTION('center_axis',(0.,0.,1.));
#36239=DIRECTION('ref_axis',(1.,0.,0.));
#36240=DIRECTION('center_axis',(0.,0.,1.));
#36241=DIRECTION('ref_axis',(1.,0.,0.));
#36242=DIRECTION('',(0.707106781186547,8.65956056235493E-17,-0.707106781186548));
#36243=DIRECTION('center_axis',(0.,0.,1.));
#36244=DIRECTION('ref_axis',(1.,0.,0.));
#36245=DIRECTION('center_axis',(0.,0.,1.));
#36246=DIRECTION('ref_axis',(1.,0.,0.));
#36247=DIRECTION('center_axis',(0.,0.,1.));
#36248=DIRECTION('ref_axis',(1.,0.,0.));
#36249=DIRECTION('center_axis',(0.,0.,1.));
#36250=DIRECTION('ref_axis',(1.,0.,0.));
#36251=DIRECTION('center_axis',(0.,0.,1.));
#36252=DIRECTION('ref_axis',(1.,0.,0.));
#36253=DIRECTION('center_axis',(0.,0.,1.));
#36254=DIRECTION('ref_axis',(1.,0.,0.));
#36255=DIRECTION('center_axis',(0.,0.,1.));
#36256=DIRECTION('ref_axis',(1.,0.,0.));
#36257=DIRECTION('center_axis',(0.,0.,1.));
#36258=DIRECTION('ref_axis',(1.,0.,0.));
#36259=DIRECTION('center_axis',(0.,0.,1.));
#36260=DIRECTION('ref_axis',(1.,0.,0.));
#36261=DIRECTION('center_axis',(0.,0.,1.));
#36262=DIRECTION('ref_axis',(1.,0.,0.));
#36263=DIRECTION('center_axis',(0.,0.,1.));
#36264=DIRECTION('ref_axis',(1.,0.,0.));
#36265=DIRECTION('center_axis',(0.,0.,1.));
#36266=DIRECTION('ref_axis',(1.,0.,0.));
#36267=DIRECTION('center_axis',(0.,0.,1.));
#36268=DIRECTION('ref_axis',(1.,0.,0.));
#36269=DIRECTION('center_axis',(0.,0.,1.));
#36270=DIRECTION('ref_axis',(1.,0.,0.));
#36271=DIRECTION('center_axis',(0.,0.,1.));
#36272=DIRECTION('ref_axis',(1.,0.,0.));
#36273=DIRECTION('center_axis',(0.,0.,1.));
#36274=DIRECTION('ref_axis',(1.,0.,0.));
#36275=DIRECTION('center_axis',(0.,0.,1.));
#36276=DIRECTION('ref_axis',(1.,0.,0.));
#36277=DIRECTION('',(0.,0.,-1.));
#36278=DIRECTION('center_axis',(0.,0.,1.));
#36279=DIRECTION('ref_axis',(1.,0.,0.));
#36280=DIRECTION('center_axis',(0.,0.,1.));
#36281=DIRECTION('ref_axis',(1.,0.,0.));
#36282=DIRECTION('center_axis',(0.,0.,1.));
#36283=DIRECTION('ref_axis',(1.,0.,0.));
#36284=DIRECTION('center_axis',(0.,0.,1.));
#36285=DIRECTION('ref_axis',(1.,0.,0.));
#36286=DIRECTION('center_axis',(0.,0.,1.));
#36287=DIRECTION('ref_axis',(1.,0.,0.));
#36288=DIRECTION('center_axis',(0.,0.,1.));
#36289=DIRECTION('ref_axis',(1.,0.,0.));
#36290=DIRECTION('center_axis',(0.,0.,1.));
#36291=DIRECTION('ref_axis',(1.,0.,0.));
#36292=DIRECTION('center_axis',(0.,0.,1.));
#36293=DIRECTION('ref_axis',(1.,0.,0.));
#36294=DIRECTION('center_axis',(0.,0.,1.));
#36295=DIRECTION('ref_axis',(1.,0.,0.));
#36296=DIRECTION('center_axis',(0.,0.,1.));
#36297=DIRECTION('ref_axis',(1.,0.,0.));
#36298=DIRECTION('center_axis',(0.,0.,1.));
#36299=DIRECTION('ref_axis',(1.,0.,0.));
#36300=DIRECTION('center_axis',(0.,0.,1.));
#36301=DIRECTION('ref_axis',(1.,0.,0.));
#36302=DIRECTION('center_axis',(0.,0.,1.));
#36303=DIRECTION('ref_axis',(1.,0.,0.));
#36304=DIRECTION('center_axis',(0.,0.,1.));
#36305=DIRECTION('ref_axis',(1.,0.,0.));
#36306=DIRECTION('center_axis',(0.,0.,1.));
#36307=DIRECTION('ref_axis',(1.,0.,0.));
#36308=DIRECTION('center_axis',(0.,0.,1.));
#36309=DIRECTION('ref_axis',(1.,0.,0.));
#36310=DIRECTION('center_axis',(0.,0.,1.));
#36311=DIRECTION('ref_axis',(1.,0.,0.));
#36312=DIRECTION('center_axis',(0.,0.,1.));
#36313=DIRECTION('ref_axis',(1.,0.,0.));
#36314=DIRECTION('center_axis',(0.,0.,1.));
#36315=DIRECTION('ref_axis',(1.,0.,0.));
#36316=DIRECTION('center_axis',(0.,0.,1.));
#36317=DIRECTION('ref_axis',(1.,0.,0.));
#36318=DIRECTION('center_axis',(0.,0.,-1.));
#36319=DIRECTION('ref_axis',(1.,0.,0.));
#36320=DIRECTION('center_axis',(0.,0.,1.));
#36321=DIRECTION('ref_axis',(1.,0.,0.));
#36322=DIRECTION('',(-0.707106781186548,-8.65956056235494E-17,-0.707106781186547));
#36323=DIRECTION('center_axis',(0.,0.,1.));
#36324=DIRECTION('ref_axis',(1.,0.,0.));
#36325=DIRECTION('',(0.,0.,1.));
#36326=DIRECTION('',(1.,0.,0.));
#36327=DIRECTION('',(0.,0.,1.));
#36328=DIRECTION('',(1.,0.,0.));
#36329=DIRECTION('',(0.,0.,1.));
#36330=DIRECTION('',(1.,0.,0.));
#36331=DIRECTION('',(0.,0.,1.));
#36332=DIRECTION('',(1.,0.,0.));
#36333=DIRECTION('',(0.,0.,1.));
#36334=DIRECTION('',(1.,0.,0.));
#36335=DIRECTION('',(0.,0.,1.));
#36336=DIRECTION('',(1.,0.,0.));
#36337=DIRECTION('',(0.,0.,1.));
#36338=DIRECTION('',(1.,0.,0.));
#36339=DIRECTION('',(0.,0.,1.));
#36340=DIRECTION('',(1.,0.,0.));
#36341=DIRECTION('',(0.,0.,1.));
#36342=DIRECTION('',(1.,0.,0.));
#36343=DIRECTION('',(-1.,0.,-2.22044604925031E-16));
#36344=DIRECTION('',(-2.22044604925031E-16,0.,1.));
#36345=DIRECTION('',(0.,0.,1.));
#36346=DIRECTION('',(1.,0.,0.));
#36347=DIRECTION('',(0.,0.,1.));
#36348=DIRECTION('',(-0.5,0.866025403784439,0.));
#36349=DIRECTION('',(0.,0.,1.));
#36350=DIRECTION('',(1.,0.,0.));
#36351=DIRECTION('',(0.,0.,1.));
#36352=DIRECTION('',(1.,0.,0.));
#36353=DIRECTION('',(0.,1.,-2.22044604925031E-16));
#36354=DIRECTION('',(1.,0.,0.));
#36355=DIRECTION('',(0.,0.,1.));
#36356=DIRECTION('',(1.,0.,0.));
#36357=DIRECTION('',(0.,0.,1.));
#36358=DIRECTION('',(1.,0.,0.));
#36359=DIRECTION('',(0.,0.,1.));
#36360=DIRECTION('',(1.,0.,0.));
#36361=DIRECTION('',(0.,0.,1.));
#36362=DIRECTION('',(1.,0.,0.));
#36363=DIRECTION('',(-1.,0.,-2.22044604925031E-16));
#36364=DIRECTION('',(-2.22044604925031E-16,0.,1.));
#36365=DIRECTION('',(0.,0.,1.));
#36366=DIRECTION('',(-1.,1.22464679914735E-16,0.));
#36367=DIRECTION('',(0.,-1.,-2.22044604925031E-16));
#36368=DIRECTION('',(1.,0.,0.));
#36369=DIRECTION('',(0.,0.,1.));
#36370=DIRECTION('',(1.,0.,0.));
#36371=DIRECTION('',(0.,0.,1.));
#36372=DIRECTION('',(1.,0.,0.));
#36373=DIRECTION('',(0.,0.,1.));
#36374=DIRECTION('',(1.,0.,0.));
#36375=DIRECTION('',(-1.,0.,-2.22044604925031E-16));
#36376=DIRECTION('',(-2.22044604925031E-16,0.,1.));
#36377=DIRECTION('',(-1.,0.,-2.22044604925031E-16));
#36378=DIRECTION('',(-2.22044604925031E-16,0.,1.));
#36379=DIRECTION('',(-1.,0.,-2.22044604925031E-16));
#36380=DIRECTION('',(-2.22044604925031E-16,0.,1.));
#36381=CARTESIAN_POINT('',(0.,0.,0.));
#36382=CARTESIAN_POINT('',(0.,0.,0.));
#36383=CARTESIAN_POINT('Origin',(34.6,13.,5.98232233047034));
#36384=CARTESIAN_POINT('',(34.6,14.2,6.));
#36385=CARTESIAN_POINT('',(34.6,14.1146446609407,5.96464466094067));
#36386=CARTESIAN_POINT('',(34.6,14.2,6.));
#36387=CARTESIAN_POINT('',(35.7146446609407,13.,5.96464466094067));
#36388=CARTESIAN_POINT('Origin',(34.6,13.,5.96464466094067));
#36389=CARTESIAN_POINT('',(35.8,13.,6.));
#36390=CARTESIAN_POINT('',(35.7146446609407,13.,5.96464466094067));
#36391=CARTESIAN_POINT('Origin',(34.6,13.,6.));
#36392=CARTESIAN_POINT('Origin',(18.85,14.1573223304703,5.98232233047034));
#36393=CARTESIAN_POINT('',(9.4,14.2,6.));
#36394=CARTESIAN_POINT('',(9.4,14.1146446609407,5.96464466094067));
#36395=CARTESIAN_POINT('',(9.4,14.2,6.));
#36396=CARTESIAN_POINT('',(18.85,14.1146446609407,5.96464466094067));
#36397=CARTESIAN_POINT('',(18.85,14.2,6.));
#36398=CARTESIAN_POINT('Origin',(9.4,13.,5.98232233047034));
#36399=CARTESIAN_POINT('',(8.2,13.,6.));
#36400=CARTESIAN_POINT('',(8.28535533905933,13.,5.96464466094067));
#36401=CARTESIAN_POINT('',(8.2,13.,6.));
#36402=CARTESIAN_POINT('Origin',(9.4,13.,5.96464466094067));
#36403=CARTESIAN_POINT('Origin',(9.4,13.,6.));
#36404=CARTESIAN_POINT('Origin',(8.24267766952966,-3.25,5.98232233047034));
#36405=CARTESIAN_POINT('',(8.2,-13.,6.));
#36406=CARTESIAN_POINT('',(8.28535533905933,-13.,5.96464466094067));
#36407=CARTESIAN_POINT('',(8.2,-13.,6.));
#36408=CARTESIAN_POINT('',(8.28535533905933,-3.25,5.96464466094067));
#36409=CARTESIAN_POINT('',(8.2,-3.25,6.));
#36410=CARTESIAN_POINT('Origin',(9.4,-13.,5.98232233047034));
#36411=CARTESIAN_POINT('',(9.4,-14.2,6.));
#36412=CARTESIAN_POINT('',(9.4,-14.1146446609407,5.96464466094067));
#36413=CARTESIAN_POINT('',(9.4,-14.2,6.));
#36414=CARTESIAN_POINT('Origin',(9.4,-13.,5.96464466094067));
#36415=CARTESIAN_POINT('Origin',(9.4,-13.,6.));
#36416=CARTESIAN_POINT('Origin',(25.15,-14.1573223304703,5.98232233047034));
#36417=CARTESIAN_POINT('',(34.6,-14.2,6.));
#36418=CARTESIAN_POINT('',(34.6,-14.1146446609407,5.96464466094067));
#36419=CARTESIAN_POINT('',(34.6,-14.2,6.));
#36420=CARTESIAN_POINT('',(25.15,-14.1146446609407,5.96464466094067));
#36421=CARTESIAN_POINT('',(25.15,-14.2,6.));
#36422=CARTESIAN_POINT('Origin',(34.6,-13.,5.98232233047034));
#36423=CARTESIAN_POINT('',(35.8,-13.,6.));
#36424=CARTESIAN_POINT('',(35.7146446609407,-13.,5.96464466094067));
#36425=CARTESIAN_POINT('',(35.8,-13.,6.));
#36426=CARTESIAN_POINT('Origin',(34.6,-13.,5.96464466094067));
#36427=CARTESIAN_POINT('Origin',(34.6,-13.,6.));
#36428=CARTESIAN_POINT('Origin',(35.7573223304703,3.25,5.98232233047034));
#36429=CARTESIAN_POINT('',(35.7146446609407,3.25,5.96464466094067));
#36430=CARTESIAN_POINT('',(35.8,3.25,6.));
#36431=CARTESIAN_POINT('Origin',(28.3,-14.075,5.925));
#36432=CARTESIAN_POINT('',(34.6,-14.0353553390593,5.88535533905933));
#36433=CARTESIAN_POINT('',(34.6,-14.15,6.));
#36434=CARTESIAN_POINT('',(9.4,-14.0353553390593,5.88535533905933));
#36435=CARTESIAN_POINT('',(31.45,-14.0353553390593,5.88535533905933));
#36436=CARTESIAN_POINT('',(9.4,-14.,5.85));
#36437=CARTESIAN_POINT('Origin',(34.6,-13.,5.925));
#36438=CARTESIAN_POINT('',(35.6353553390593,-13.,5.88535533905933));
#36439=CARTESIAN_POINT('',(35.6,-13.,5.85));
#36440=CARTESIAN_POINT('Origin',(34.6,-13.,5.88535533905933));
#36441=CARTESIAN_POINT('Origin',(35.675,6.5,5.925));
#36442=CARTESIAN_POINT('',(35.6353553390593,13.,5.88535533905933));
#36443=CARTESIAN_POINT('',(35.6,13.,5.85));
#36444=CARTESIAN_POINT('',(35.6353553390593,9.75,5.88535533905933));
#36445=CARTESIAN_POINT('Origin',(34.6,13.,5.925));
#36446=CARTESIAN_POINT('',(34.6,14.0353553390593,5.88535533905933));
#36447=CARTESIAN_POINT('',(34.6,14.,5.85));
#36448=CARTESIAN_POINT('Origin',(34.6,13.,5.88535533905933));
#36449=CARTESIAN_POINT('Origin',(22.,0.,6.));
#36450=CARTESIAN_POINT('',(35.,15.,6.));
#36451=CARTESIAN_POINT('',(36.8,13.2,6.));
#36452=CARTESIAN_POINT('Origin',(35.,13.2,6.));
#36453=CARTESIAN_POINT('',(9.,15.,6.));
#36454=CARTESIAN_POINT('',(25.25,15.,6.));
#36455=CARTESIAN_POINT('',(7.2,13.2,6.));
#36456=CARTESIAN_POINT('Origin',(9.,13.2,6.));
#36457=CARTESIAN_POINT('',(7.2,-13.2,6.));
#36458=CARTESIAN_POINT('',(7.2,3.3,6.));
#36459=CARTESIAN_POINT('',(9.,-15.,6.));
#36460=CARTESIAN_POINT('Origin',(9.,-13.2,6.));
#36461=CARTESIAN_POINT('',(35.,-15.,6.));
#36462=CARTESIAN_POINT('',(18.75,-15.,6.));
#36463=CARTESIAN_POINT('',(36.8,-13.2,6.));
#36464=CARTESIAN_POINT('Origin',(35.,-13.2,6.));
#36465=CARTESIAN_POINT('',(36.8,-3.3,6.));
#36466=CARTESIAN_POINT('Origin',(29.,-9.2,4.175));
#36467=CARTESIAN_POINT('',(28.445,-9.2,4.2));
#36468=CARTESIAN_POINT('Origin',(29.,-9.2,4.2));
#36469=CARTESIAN_POINT('',(28.495,-9.2,4.15));
#36470=CARTESIAN_POINT('',(28.47,-9.2,4.175));
#36471=CARTESIAN_POINT('Origin',(29.,-9.2,4.15));
#36472=CARTESIAN_POINT('Origin',(22.,3.5527136788005E-15,4.2));
#36473=CARTESIAN_POINT('',(8.7,13.,4.2));
#36474=CARTESIAN_POINT('',(9.4,13.7,4.2));
#36475=CARTESIAN_POINT('Origin',(9.4,13.,4.2));
#36476=CARTESIAN_POINT('',(8.7,-13.,4.2));
#36477=CARTESIAN_POINT('',(8.7,-6.5,4.2));
#36478=CARTESIAN_POINT('',(9.4,-13.7,4.2));
#36479=CARTESIAN_POINT('Origin',(9.4,-13.,4.2));
#36480=CARTESIAN_POINT('',(34.6,-13.7,4.2));
#36481=CARTESIAN_POINT('',(28.3,-13.7,4.2));
#36482=CARTESIAN_POINT('',(35.3,-13.,4.2));
#36483=CARTESIAN_POINT('Origin',(34.6,-13.,4.2));
#36484=CARTESIAN_POINT('',(35.3,13.,4.2));
#36485=CARTESIAN_POINT('',(35.3,6.5,4.2));
#36486=CARTESIAN_POINT('',(34.6,13.7,4.2));
#36487=CARTESIAN_POINT('Origin',(34.6,13.,4.2));
#36488=CARTESIAN_POINT('',(15.7,13.7,4.2));
#36489=CARTESIAN_POINT('',(28.445,9.2,4.2));
#36490=CARTESIAN_POINT('Origin',(29.,9.2,4.2));
#36491=CARTESIAN_POINT('',(10.445,9.2,4.2));
#36492=CARTESIAN_POINT('Origin',(11.,9.2,4.2));
#36493=CARTESIAN_POINT('',(32.725,1.07156594925393E-16,4.2));
#36494=CARTESIAN_POINT('Origin',(33.6,0.,4.2));
#36495=CARTESIAN_POINT('',(18.95,-12.55,4.2));
#36496=CARTESIAN_POINT('',(21.05,-12.55,4.2));
#36497=CARTESIAN_POINT('',(21.5,-12.55,4.2));
#36498=CARTESIAN_POINT('',(18.95,12.55,4.2));
#36499=CARTESIAN_POINT('',(18.95,-6.25,4.2));
#36500=CARTESIAN_POINT('',(21.05,12.55,4.2));
#36501=CARTESIAN_POINT('',(20.5,12.55,4.2));
#36502=CARTESIAN_POINT('',(21.05,6.25,4.2));
#36503=CARTESIAN_POINT('',(10.445,-9.2,4.2));
#36504=CARTESIAN_POINT('Origin',(11.,-9.2,4.2));
#36505=CARTESIAN_POINT('Origin',(29.,-9.2,3.215));
#36506=CARTESIAN_POINT('',(28.495,-9.2,2.2));
#36507=CARTESIAN_POINT('Origin',(29.,-9.2,2.2));
#36508=CARTESIAN_POINT('',(28.495,-9.2,3.215));
#36509=CARTESIAN_POINT('Origin',(29.,9.2,4.175));
#36510=CARTESIAN_POINT('',(28.495,9.2,4.15));
#36511=CARTESIAN_POINT('',(28.47,9.2,4.175));
#36512=CARTESIAN_POINT('Origin',(29.,9.2,4.15));
#36513=CARTESIAN_POINT('Origin',(29.,9.2,3.215));
#36514=CARTESIAN_POINT('',(28.495,9.2,2.2));
#36515=CARTESIAN_POINT('Origin',(29.,9.2,2.2));
#36516=CARTESIAN_POINT('',(28.495,9.2,3.215));
#36517=CARTESIAN_POINT('Origin',(11.,-9.2,4.175));
#36518=CARTESIAN_POINT('',(10.495,-9.2,4.15));
#36519=CARTESIAN_POINT('',(10.47,-9.2,4.175));
#36520=CARTESIAN_POINT('Origin',(11.,-9.2,4.15));
#36521=CARTESIAN_POINT('Origin',(11.,-9.2,3.215));
#36522=CARTESIAN_POINT('',(10.495,-9.2,2.2));
#36523=CARTESIAN_POINT('Origin',(11.,-9.2,2.2));
#36524=CARTESIAN_POINT('',(10.495,-9.2,3.215));
#36525=CARTESIAN_POINT('Origin',(11.,9.2,4.175));
#36526=CARTESIAN_POINT('',(10.495,9.2,4.15));
#36527=CARTESIAN_POINT('',(10.47,9.2,4.175));
#36528=CARTESIAN_POINT('Origin',(11.,9.2,4.15));
#36529=CARTESIAN_POINT('Origin',(11.,9.2,3.215));
#36530=CARTESIAN_POINT('',(10.495,9.2,2.2));
#36531=CARTESIAN_POINT('Origin',(11.,9.2,2.2));
#36532=CARTESIAN_POINT('',(10.495,9.2,3.215));
#36533=CARTESIAN_POINT('Origin',(20.5,12.525,4.175));
#36534=CARTESIAN_POINT('',(19.,12.5,4.15));
#36535=CARTESIAN_POINT('',(18.95,12.55,4.2));
#36536=CARTESIAN_POINT('',(21.,12.5,4.15));
#36537=CARTESIAN_POINT('',(20.5,12.5,4.15));
#36538=CARTESIAN_POINT('',(21.05,12.55,4.2));
#36539=CARTESIAN_POINT('Origin',(21.5,-12.525,4.175));
#36540=CARTESIAN_POINT('',(21.,-12.5,4.15));
#36541=CARTESIAN_POINT('',(21.05,-12.55,4.2));
#36542=CARTESIAN_POINT('',(19.,-12.5,4.15));
#36543=CARTESIAN_POINT('',(21.5,-12.5,4.15));
#36544=CARTESIAN_POINT('',(19.,-12.5,4.15));
#36545=CARTESIAN_POINT('Origin',(21.025,6.25,4.175));
#36546=CARTESIAN_POINT('',(21.,6.25,4.15));
#36547=CARTESIAN_POINT('Origin',(18.975,-6.25,4.175));
#36548=CARTESIAN_POINT('',(19.,-6.25,4.15));
#36549=CARTESIAN_POINT('Origin',(19.,-12.5,4.2));
#36550=CARTESIAN_POINT('',(19.,-12.5,3.6));
#36551=CARTESIAN_POINT('',(19.,-12.5,4.2));
#36552=CARTESIAN_POINT('',(19.,12.5,3.6));
#36553=CARTESIAN_POINT('',(19.,12.5,3.6));
#36554=CARTESIAN_POINT('',(19.,12.5,4.2));
#36555=CARTESIAN_POINT('Origin',(21.,-12.5,4.2));
#36556=CARTESIAN_POINT('',(21.,-12.5,3.6));
#36557=CARTESIAN_POINT('',(21.,-12.5,4.2));
#36558=CARTESIAN_POINT('',(19.,-12.5,3.6));
#36559=CARTESIAN_POINT('Origin',(31.45,-14.0176776695297,5.84267766952966));
#36560=CARTESIAN_POINT('',(20.0776208734813,-14.,5.8));
#36561=CARTESIAN_POINT('',(19.9223791265187,-14.,5.8));
#36562=CARTESIAN_POINT('Origin',(20.,-13.7514718625762,5.2));
#36563=CARTESIAN_POINT('',(9.4,-14.,5.8));
#36564=CARTESIAN_POINT('',(31.45,-14.,5.8));
#36565=CARTESIAN_POINT('',(9.4,-14.,5.8));
#36566=CARTESIAN_POINT('',(34.6,-14.,5.8));
#36567=CARTESIAN_POINT('',(34.6,-14.0353553390593,5.88535533905933));
#36568=CARTESIAN_POINT('',(31.45,-14.,5.8));
#36569=CARTESIAN_POINT('Origin',(9.4,-13.,5.84267766952966));
#36570=CARTESIAN_POINT('',(8.4,-13.,5.8));
#36571=CARTESIAN_POINT('',(8.36464466094067,-13.,5.88535533905933));
#36572=CARTESIAN_POINT('',(8.4,-13.,5.8));
#36573=CARTESIAN_POINT('Origin',(9.4,-13.,5.88535533905933));
#36574=CARTESIAN_POINT('Origin',(9.4,-13.,5.8));
#36575=CARTESIAN_POINT('Origin',(8.38232233047034,-9.75,5.84267766952966));
#36576=CARTESIAN_POINT('',(8.4,13.,5.8));
#36577=CARTESIAN_POINT('',(8.36464466094067,13.,5.88535533905933));
#36578=CARTESIAN_POINT('',(8.4,13.,5.8));
#36579=CARTESIAN_POINT('',(8.36464466094067,-9.75,5.88535533905933));
#36580=CARTESIAN_POINT('',(8.4,-9.75,5.8));
#36581=CARTESIAN_POINT('Origin',(9.4,13.,5.84267766952966));
#36582=CARTESIAN_POINT('',(9.4,14.,5.8));
#36583=CARTESIAN_POINT('',(9.4,14.0353553390593,5.88535533905933));
#36584=CARTESIAN_POINT('',(9.4,14.,5.8));
#36585=CARTESIAN_POINT('Origin',(9.4,13.,5.88535533905933));
#36586=CARTESIAN_POINT('Origin',(9.4,13.,5.8));
#36587=CARTESIAN_POINT('Origin',(12.55,14.0176776695297,5.84267766952966));
#36588=CARTESIAN_POINT('',(19.9223791265187,14.,5.8));
#36589=CARTESIAN_POINT('',(20.0776208734813,14.,5.8));
#36590=CARTESIAN_POINT('Origin',(20.,13.7514718625762,5.2));
#36591=CARTESIAN_POINT('',(34.6,14.,5.8));
#36592=CARTESIAN_POINT('',(12.55,14.,5.8));
#36593=CARTESIAN_POINT('',(34.6,14.,5.8));
#36594=CARTESIAN_POINT('',(12.55,14.0353553390593,5.88535533905933));
#36595=CARTESIAN_POINT('',(12.55,14.,5.8));
#36596=CARTESIAN_POINT('Origin',(34.6,13.,5.84267766952966));
#36597=CARTESIAN_POINT('',(35.6,13.,5.8));
#36598=CARTESIAN_POINT('',(35.6,13.,5.8));
#36599=CARTESIAN_POINT('Origin',(34.6,13.,5.8));
#36600=CARTESIAN_POINT('Origin',(35.6176776695297,9.75,5.84267766952967));
#36601=CARTESIAN_POINT('',(35.6,-13.,5.8));
#36602=CARTESIAN_POINT('',(35.6,-13.,5.8));
#36603=CARTESIAN_POINT('',(35.6,9.75,5.8));
#36604=CARTESIAN_POINT('Origin',(34.6,-13.,5.84267766952966));
#36605=CARTESIAN_POINT('Origin',(34.6,-13.,5.8));
#36606=CARTESIAN_POINT('Origin',(34.6,-14.,6.));
#36607=CARTESIAN_POINT('',(34.6,-14.,4.5));
#36608=CARTESIAN_POINT('',(34.6,-14.,6.));
#36609=CARTESIAN_POINT('',(9.4,-14.,4.5));
#36610=CARTESIAN_POINT('',(28.3,-14.,4.5));
#36611=CARTESIAN_POINT('',(9.4,-14.,6.));
#36612=CARTESIAN_POINT('',(20.,-14.,4.595));
#36613=CARTESIAN_POINT('Origin',(20.,-14.,5.2));
#36614=CARTESIAN_POINT('Origin',(20.,-14.,5.2));
#36615=CARTESIAN_POINT('Origin',(34.6,-13.,6.));
#36616=CARTESIAN_POINT('',(35.6,-13.,4.5));
#36617=CARTESIAN_POINT('',(35.6,-13.,6.));
#36618=CARTESIAN_POINT('Origin',(34.6,-13.,4.5));
#36619=CARTESIAN_POINT('Origin',(35.6,13.,6.));
#36620=CARTESIAN_POINT('',(35.6,13.,4.5));
#36621=CARTESIAN_POINT('',(35.6,13.,6.));
#36622=CARTESIAN_POINT('',(35.6,6.5,4.5));
#36623=CARTESIAN_POINT('Origin',(34.6,13.,6.));
#36624=CARTESIAN_POINT('',(34.6,14.,4.5));
#36625=CARTESIAN_POINT('',(34.6,14.,6.));
#36626=CARTESIAN_POINT('Origin',(34.6,13.,4.5));
#36627=CARTESIAN_POINT('Origin',(9.4,14.,6.));
#36628=CARTESIAN_POINT('',(20.,14.,4.595));
#36629=CARTESIAN_POINT('Origin',(20.,14.,5.2));
#36630=CARTESIAN_POINT('Origin',(20.,14.,5.2));
#36631=CARTESIAN_POINT('',(9.4,14.,4.5));
#36632=CARTESIAN_POINT('',(9.4,14.,6.));
#36633=CARTESIAN_POINT('',(15.7,14.,4.5));
#36634=CARTESIAN_POINT('Origin',(20.,14.59,5.2));
#36635=CARTESIAN_POINT('',(20.,15.2,4.595));
#36636=CARTESIAN_POINT('',(20.,14.59,4.595));
#36637=CARTESIAN_POINT('',(19.9223791265187,15.2,5.8));
#36638=CARTESIAN_POINT('Origin',(20.,15.2,5.2));
#36639=CARTESIAN_POINT('',(20.0776208734813,15.2,5.8));
#36640=CARTESIAN_POINT('Origin',(20.,15.4485281374238,5.2));
#36641=CARTESIAN_POINT('Origin',(20.,15.2,5.2));
#36642=CARTESIAN_POINT('Origin',(36.975,-7.025,0.));
#36643=CARTESIAN_POINT('',(37.,-7.05,2.05));
#36644=CARTESIAN_POINT('',(37.,-7.05,0.149999999999996));
#36645=CARTESIAN_POINT('',(37.,-7.05,0.));
#36646=CARTESIAN_POINT('',(36.975,-7.025,0.0896446609406665));
#36647=CARTESIAN_POINT('',(37.1479963503908,-7.19799635039082,0.507294796295184));
#36648=CARTESIAN_POINT('',(36.95,-7.,0.149999999999999));
#36649=CARTESIAN_POINT('',(35.3058538083499,-5.35585380834979,4.11932003440591));
#36650=CARTESIAN_POINT('',(36.95,-7.,2.));
#36651=CARTESIAN_POINT('',(36.95,-7.,0.));
#36652=CARTESIAN_POINT('',(36.95,-7.,2.));
#36653=CARTESIAN_POINT('Origin',(36.975,-6.6,2.025));
#36654=CARTESIAN_POINT('',(36.95,7.,2.));
#36655=CARTESIAN_POINT('',(36.95,-6.6,2.));
#36656=CARTESIAN_POINT('',(37.,7.05,2.05));
#36657=CARTESIAN_POINT('',(34.3666666666667,4.41666666666652,-0.583333333333435));
#36658=CARTESIAN_POINT('',(37.,-6.6,2.05));
#36659=CARTESIAN_POINT('Origin',(36.9823223304703,-9.9,0.107322330470332));
#36660=CARTESIAN_POINT('',(37.,-13.2,0.149999999999996));
#36661=CARTESIAN_POINT('',(37.,-9.9,0.149999999999996));
#36662=CARTESIAN_POINT('',(36.9646446609407,-13.2,0.0646446609406699));
#36663=CARTESIAN_POINT('',(37.,-13.2,0.149999999999996));
#36664=CARTESIAN_POINT('',(36.9646446609407,-7.03535533905933,0.0646446609406699));
#36665=CARTESIAN_POINT('',(36.9646446609407,-9.9,0.0646446609406684));
#36666=CARTESIAN_POINT('',(35.1179858427056,-8.88201415729434,-4.39358410311806));
#36667=CARTESIAN_POINT('Origin',(37.,-13.2,0.));
#36668=CARTESIAN_POINT('',(37.,7.05,0.150000000000001));
#36669=CARTESIAN_POINT('',(37.,7.05,0.));
#36670=CARTESIAN_POINT('',(37.,13.2,0.15));
#36671=CARTESIAN_POINT('',(37.,-9.9,0.149999999999996));
#36672=CARTESIAN_POINT('',(37.,13.2,5.80000000000001));
#36673=CARTESIAN_POINT('',(37.,13.2,0.));
#36674=CARTESIAN_POINT('',(37.,-13.2,5.8));
#36675=CARTESIAN_POINT('',(37.,-9.9,5.80000000000001));
#36676=CARTESIAN_POINT('',(37.,-13.2,0.));
#36677=CARTESIAN_POINT('Origin',(10.675,-7.01767766952966,0.107322330470336));
#36678=CARTESIAN_POINT('',(7.03535533905933,-7.03535533905933,0.0646446609406731));
#36679=CARTESIAN_POINT('',(10.675,-7.03535533905933,0.064644660940672));
#36680=CARTESIAN_POINT('',(7.025,-7.025,0.0896446609406749));
#36681=CARTESIAN_POINT('',(6.1707415527494,-6.17074155274938,2.15200699006485));
#36682=CARTESIAN_POINT('',(7.05,-7.,0.149999999999999));
#36683=CARTESIAN_POINT('',(7.24749543798848,-6.80250456201151,0.626796164898609));
#36684=CARTESIAN_POINT('',(10.675,-7.,0.149999999999999));
#36685=CARTESIAN_POINT('Origin',(7.025,-7.025,0.));
#36686=CARTESIAN_POINT('',(7.,-7.05,0.15));
#36687=CARTESIAN_POINT('',(8.11662550049235,-5.93337449950761,-2.54577242738026));
#36688=CARTESIAN_POINT('',(7.,-7.05,2.05));
#36689=CARTESIAN_POINT('',(7.,-7.05,0.));
#36690=CARTESIAN_POINT('',(7.05,-7.,2.));
#36691=CARTESIAN_POINT('',(7.,-7.05,2.05));
#36692=CARTESIAN_POINT('',(7.05,-7.,0.));
#36693=CARTESIAN_POINT('Origin',(7.01767766952966,9.9,0.107322330470337));
#36694=CARTESIAN_POINT('',(7.03535533905933,-13.2,0.0646446609406725));
#36695=CARTESIAN_POINT('',(7.03535533905933,9.9,0.0646446609406732));
#36696=CARTESIAN_POINT('',(7.,-13.2,0.15));
#36697=CARTESIAN_POINT('',(7.,-13.2,0.15));
#36698=CARTESIAN_POINT('',(7.,9.9,0.15));
#36699=CARTESIAN_POINT('Origin',(14.45,-7.05,0.05));
#36700=CARTESIAN_POINT('',(36.9353553390593,-7.06464466094067,0.0353553390593268));
#36701=CARTESIAN_POINT('',(36.9,-7.1,0.));
#36702=CARTESIAN_POINT('',(7.06464466094067,-7.06464466094067,0.0353553390593268));
#36703=CARTESIAN_POINT('',(18.225,-7.06464466094067,0.035355339059327));
#36704=CARTESIAN_POINT('',(7.,-7.,0.1));
#36705=CARTESIAN_POINT('Origin',(18.225,-7.10732233047034,0.0176776695296635));
#36706=CARTESIAN_POINT('',(7.1,-7.15,0.));
#36707=CARTESIAN_POINT('',(5.67626910198315,-3.71280955683808,1.42373089801684));
#36708=CARTESIAN_POINT('',(36.9,-7.15,0.));
#36709=CARTESIAN_POINT('',(35.8061358310127,-9.79082171216312,-1.09386416898729));
#36710=CARTESIAN_POINT('',(18.225,-7.15,0.));
#36711=CARTESIAN_POINT('Origin',(7.05,6.6,0.05));
#36712=CARTESIAN_POINT('',(7.1,-13.2,0.));
#36713=CARTESIAN_POINT('',(7.1,6.6,0.));
#36714=CARTESIAN_POINT('',(7.1,-13.2,0.));
#36715=CARTESIAN_POINT('Origin',(35.,13.2,5.98232233047034));
#36716=CARTESIAN_POINT('',(36.8853553390593,13.2,5.96464466094067));
#36717=CARTESIAN_POINT('',(36.8,13.2,6.));
#36718=CARTESIAN_POINT('',(35.,15.0853553390593,5.96464466094067));
#36719=CARTESIAN_POINT('Origin',(35.,13.2,5.96464466094067));
#36720=CARTESIAN_POINT('',(35.,15.0853553390593,5.96464466094067));
#36721=CARTESIAN_POINT('Origin',(36.8426776695297,-3.3,5.98232233047034));
#36722=CARTESIAN_POINT('',(36.8853553390593,-13.2,5.96464466094068));
#36723=CARTESIAN_POINT('',(36.8,-13.2,6.));
#36724=CARTESIAN_POINT('',(36.8853553390593,-3.3,5.96464466094067));
#36725=CARTESIAN_POINT('Origin',(35.,-13.2,5.98232233047034));
#36726=CARTESIAN_POINT('',(35.,-15.0853553390593,5.96464466094067));
#36727=CARTESIAN_POINT('',(35.,-15.,6.));
#36728=CARTESIAN_POINT('Origin',(35.,-13.2,5.96464466094067));
#36729=CARTESIAN_POINT('Origin',(18.75,-15.0426776695297,5.98232233047034));
#36730=CARTESIAN_POINT('',(9.,-15.0853553390593,5.96464466094067));
#36731=CARTESIAN_POINT('',(9.,-15.,6.));
#36732=CARTESIAN_POINT('',(18.75,-15.0853553390593,5.96464466094067));
#36733=CARTESIAN_POINT('Origin',(9.,-13.2,5.98232233047034));
#36734=CARTESIAN_POINT('',(7.11464466094067,-13.2,5.96464466094067));
#36735=CARTESIAN_POINT('',(7.2,-13.2,6.));
#36736=CARTESIAN_POINT('Origin',(9.,-13.2,5.96464466094067));
#36737=CARTESIAN_POINT('Origin',(7.15732233047034,3.3,5.98232233047034));
#36738=CARTESIAN_POINT('',(7.11464466094067,13.2,5.96464466094067));
#36739=CARTESIAN_POINT('',(7.2,13.2,6.));
#36740=CARTESIAN_POINT('',(7.11464466094067,3.3,5.96464466094067));
#36741=CARTESIAN_POINT('Origin',(9.,13.2,5.98232233047034));
#36742=CARTESIAN_POINT('',(9.,15.0853553390593,5.96464466094067));
#36743=CARTESIAN_POINT('',(9.,15.,6.));
#36744=CARTESIAN_POINT('Origin',(9.,13.2,5.96464466094067));
#36745=CARTESIAN_POINT('Origin',(25.25,15.0426776695297,5.98232233047034));
#36746=CARTESIAN_POINT('',(25.25,15.0853553390593,5.96464466094067));
#36747=CARTESIAN_POINT('Origin',(7.075,6.6,5.925));
#36748=CARTESIAN_POINT('',(7.03535533905933,13.2,5.88535533905933));
#36749=CARTESIAN_POINT('',(7.15,13.2,6.));
#36750=CARTESIAN_POINT('',(7.03535533905933,-13.2,5.88535533905933));
#36751=CARTESIAN_POINT('',(7.03535533905933,9.9,5.88535533905933));
#36752=CARTESIAN_POINT('',(7.,-13.2,5.85));
#36753=CARTESIAN_POINT('Origin',(9.,13.2,5.925));
#36754=CARTESIAN_POINT('',(9.,15.1646446609407,5.88535533905933));
#36755=CARTESIAN_POINT('',(9.,15.2,5.85));
#36756=CARTESIAN_POINT('Origin',(9.,13.2,5.88535533905933));
#36757=CARTESIAN_POINT('Origin',(28.5,15.125,5.925));
#36758=CARTESIAN_POINT('',(35.,15.1646446609407,5.88535533905933));
#36759=CARTESIAN_POINT('',(35.,15.2,5.85));
#36760=CARTESIAN_POINT('',(31.75,15.1646446609407,5.88535533905933));
#36761=CARTESIAN_POINT('Origin',(35.,13.2,5.925));
#36762=CARTESIAN_POINT('',(36.9646446609407,13.2,5.88535533905933));
#36763=CARTESIAN_POINT('',(37.,13.2,5.85));
#36764=CARTESIAN_POINT('Origin',(35.,13.2,5.88535533905933));
#36765=CARTESIAN_POINT('Origin',(7.01767766952966,9.9,5.84267766952966));
#36766=CARTESIAN_POINT('',(7.,-13.2,5.8));
#36767=CARTESIAN_POINT('',(7.,-13.2,5.8));
#36768=CARTESIAN_POINT('',(7.,13.2,5.8));
#36769=CARTESIAN_POINT('',(7.03535533905933,13.2,5.88535533905933));
#36770=CARTESIAN_POINT('',(7.,9.9,5.8));
#36771=CARTESIAN_POINT('Origin',(9.,-13.2,5.84267766952966));
#36772=CARTESIAN_POINT('',(9.,-15.2,5.8));
#36773=CARTESIAN_POINT('',(9.,-15.1646446609407,5.88535533905933));
#36774=CARTESIAN_POINT('',(9.,-15.2,5.8));
#36775=CARTESIAN_POINT('Origin',(9.,-13.2,5.88535533905933));
#36776=CARTESIAN_POINT('Origin',(9.,-13.2,5.8));
#36777=CARTESIAN_POINT('Origin',(12.25,-15.1823223304703,5.84267766952966));
#36778=CARTESIAN_POINT('',(19.9223791265187,-15.2,5.8));
#36779=CARTESIAN_POINT('',(20.0776208734813,-15.2,5.8));
#36780=CARTESIAN_POINT('Origin',(20.,-15.4485281374238,5.2));
#36781=CARTESIAN_POINT('',(35.,-15.2,5.8));
#36782=CARTESIAN_POINT('',(12.25,-15.2,5.8));
#36783=CARTESIAN_POINT('',(35.,-15.1646446609407,5.88535533905933));
#36784=CARTESIAN_POINT('',(35.,-15.2,5.8));
#36785=CARTESIAN_POINT('',(12.25,-15.1646446609407,5.88535533905933));
#36786=CARTESIAN_POINT('',(12.25,-15.2,5.8));
#36787=CARTESIAN_POINT('Origin',(35.,-13.2,5.84267766952966));
#36788=CARTESIAN_POINT('',(36.9646446609407,-13.2,5.88535533905933));
#36789=CARTESIAN_POINT('',(37.,-13.2,5.8));
#36790=CARTESIAN_POINT('Origin',(35.,-13.2,5.88535533905933));
#36791=CARTESIAN_POINT('Origin',(35.,-13.2,5.8));
#36792=CARTESIAN_POINT('Origin',(36.9823223304703,-9.9,5.84267766952967));
#36793=CARTESIAN_POINT('',(37.,13.2,5.80000000000001));
#36794=CARTESIAN_POINT('',(36.9646446609407,-9.9,5.88535533905933));
#36795=CARTESIAN_POINT('Origin',(35.,13.2,5.84267766952967));
#36796=CARTESIAN_POINT('',(35.,15.2,5.8));
#36797=CARTESIAN_POINT('',(35.,15.2,5.8));
#36798=CARTESIAN_POINT('Origin',(35.,13.2,5.8));
#36799=CARTESIAN_POINT('Origin',(31.75,15.1823223304703,5.84267766952966));
#36800=CARTESIAN_POINT('',(9.,15.2,5.8));
#36801=CARTESIAN_POINT('',(31.75,15.2,5.8));
#36802=CARTESIAN_POINT('',(9.,15.2,5.8));
#36803=CARTESIAN_POINT('',(31.75,15.2,5.8));
#36804=CARTESIAN_POINT('Origin',(9.,13.2,5.84267766952966));
#36805=CARTESIAN_POINT('Origin',(9.,13.2,5.8));
#36806=CARTESIAN_POINT('Origin',(9.,-15.2,0.));
#36807=CARTESIAN_POINT('',(9.,-15.2,0.150000000000001));
#36808=CARTESIAN_POINT('',(9.,-15.2,0.));
#36809=CARTESIAN_POINT('',(35.,-15.2,0.15));
#36810=CARTESIAN_POINT('',(12.25,-15.2,0.150000000000001));
#36811=CARTESIAN_POINT('',(35.,-15.2,0.));
#36812=CARTESIAN_POINT('',(20.,-15.2,4.595));
#36813=CARTESIAN_POINT('Origin',(20.,-15.2,5.2));
#36814=CARTESIAN_POINT('Origin',(20.,-15.2,5.2));
#36815=CARTESIAN_POINT('Origin',(9.,-13.2,0.));
#36816=CARTESIAN_POINT('',(7.,-13.2,0.));
#36817=CARTESIAN_POINT('Origin',(9.,-13.2,0.15));
#36818=CARTESIAN_POINT('Origin',(7.,13.2,0.));
#36819=CARTESIAN_POINT('',(7.,13.2,0.15));
#36820=CARTESIAN_POINT('',(7.,13.2,0.));
#36821=CARTESIAN_POINT('',(7.,7.05,0.15));
#36822=CARTESIAN_POINT('',(7.,9.9,0.15));
#36823=CARTESIAN_POINT('',(7.,7.05,2.05));
#36824=CARTESIAN_POINT('',(7.,7.05,0.));
#36825=CARTESIAN_POINT('',(7.,6.6,2.05));
#36826=CARTESIAN_POINT('Origin',(9.,13.2,0.));
#36827=CARTESIAN_POINT('',(9.,15.2,0.15));
#36828=CARTESIAN_POINT('',(9.,15.2,0.));
#36829=CARTESIAN_POINT('Origin',(9.,13.2,0.15));
#36830=CARTESIAN_POINT('Origin',(35.,15.2,0.));
#36831=CARTESIAN_POINT('',(35.,15.2,0.150000000000001));
#36832=CARTESIAN_POINT('',(35.,15.2,0.));
#36833=CARTESIAN_POINT('',(31.75,15.2,0.150000000000001));
#36834=CARTESIAN_POINT('Origin',(35.,-13.2,0.107322330470338));
#36835=CARTESIAN_POINT('',(35.,-15.1646446609407,0.0646446609406744));
#36836=CARTESIAN_POINT('',(35.,-15.2,0.15));
#36837=CARTESIAN_POINT('Origin',(35.,-13.2,0.0646446609406753));
#36838=CARTESIAN_POINT('Origin',(35.,-13.2,0.15));
#36839=CARTESIAN_POINT('Origin',(12.25,-15.1823223304703,0.107322330470337));
#36840=CARTESIAN_POINT('',(9.,-15.1646446609407,0.0646446609406738));
#36841=CARTESIAN_POINT('',(9.,-15.2,0.150000000000001));
#36842=CARTESIAN_POINT('',(12.25,-15.1646446609407,0.0646446609406733));
#36843=CARTESIAN_POINT('Origin',(9.,-13.2,0.107322330470337));
#36844=CARTESIAN_POINT('Origin',(9.,-13.2,0.0646446609406728));
#36845=CARTESIAN_POINT('Origin',(36.95,-6.6,0.05));
#36846=CARTESIAN_POINT('',(36.9,-13.2,0.));
#36847=CARTESIAN_POINT('',(36.9,-13.2,0.));
#36848=CARTESIAN_POINT('',(36.9,-6.6,0.));
#36849=CARTESIAN_POINT('Origin',(35.,-13.2,0.05));
#36850=CARTESIAN_POINT('',(35.,-15.1,0.));
#36851=CARTESIAN_POINT('',(35.,-15.1,0.));
#36852=CARTESIAN_POINT('Origin',(35.,-13.2,0.));
#36853=CARTESIAN_POINT('Origin',(15.5,-15.15,0.05));
#36854=CARTESIAN_POINT('',(9.,-15.1,0.));
#36855=CARTESIAN_POINT('',(9.,-15.1,0.));
#36856=CARTESIAN_POINT('',(15.5,-15.1,0.));
#36857=CARTESIAN_POINT('Origin',(9.,-13.2,0.05));
#36858=CARTESIAN_POINT('Origin',(9.,-13.2,0.));
#36859=CARTESIAN_POINT('Origin',(36.9353553390593,7.12588190451026,0.0353553390593253));
#36860=CARTESIAN_POINT('',(36.85,7.15,0.));
#36861=CARTESIAN_POINT('',(36.8741180954897,7.06464466094067,0.035355339059327));
#36862=CARTESIAN_POINT('',(36.85,7.15,0.));
#36863=CARTESIAN_POINT('',(36.9353553390593,7.12588190451026,0.0353553390593251));
#36864=CARTESIAN_POINT('',(36.9353553390593,7.12588190451026,0.0353553390593253));
#36865=CARTESIAN_POINT('',(36.8741180954897,7.06464466094067,0.0353553390593253));
#36866=CARTESIAN_POINT('Origin',(7.15,7.15,0.));
#36867=CARTESIAN_POINT('',(7.06464466094067,7.12588190451025,0.0353553390593283));
#36868=CARTESIAN_POINT('',(7.12588190451025,7.06464466094067,0.0353553390593273));
#36869=CARTESIAN_POINT('',(7.06464466094067,7.12588190451025,0.0353553390593291));
#36870=CARTESIAN_POINT('',(7.15,7.15,0.));
#36871=CARTESIAN_POINT('',(7.15,7.15,0.));
#36872=CARTESIAN_POINT('',(7.12588190451025,7.06464466094067,0.035355339059327));
#36873=CARTESIAN_POINT('Origin',(36.8926776695297,-3.3,0.0176776695296627));
#36874=CARTESIAN_POINT('',(36.85,13.2,0.));
#36875=CARTESIAN_POINT('',(36.9353553390593,13.2,0.035355339059327));
#36876=CARTESIAN_POINT('',(36.85,13.2,0.));
#36877=CARTESIAN_POINT('',(36.9353553390593,-3.3,0.0353553390593253));
#36878=CARTESIAN_POINT('',(36.85,-3.3,0.));
#36879=CARTESIAN_POINT('Origin',(35.,13.2,0.0176776695296633));
#36880=CARTESIAN_POINT('',(35.,15.05,0.));
#36881=CARTESIAN_POINT('',(35.,15.1353553390593,0.0353553390593202));
#36882=CARTESIAN_POINT('',(35.,15.05,0.));
#36883=CARTESIAN_POINT('Origin',(35.,13.2,0.0353553390593266));
#36884=CARTESIAN_POINT('Origin',(35.,13.2,0.));
#36885=CARTESIAN_POINT('Origin',(25.25,15.0926776695297,0.0176776695296636));
#36886=CARTESIAN_POINT('',(9.,15.05,0.));
#36887=CARTESIAN_POINT('',(9.,15.1353553390593,0.0353553390593265));
#36888=CARTESIAN_POINT('',(9.,15.05,0.));
#36889=CARTESIAN_POINT('',(25.25,15.1353553390593,0.0353553390593273));
#36890=CARTESIAN_POINT('',(25.25,15.05,0.));
#36891=CARTESIAN_POINT('Origin',(9.,13.2,0.017677669529664));
#36892=CARTESIAN_POINT('',(7.15,13.2,0.));
#36893=CARTESIAN_POINT('',(7.06464466094067,13.2,0.0353553390593274));
#36894=CARTESIAN_POINT('',(7.15,13.2,0.));
#36895=CARTESIAN_POINT('Origin',(9.,13.2,0.0353553390593279));
#36896=CARTESIAN_POINT('Origin',(9.,13.2,0.));
#36897=CARTESIAN_POINT('Origin',(7.10732233047034,3.3,0.0176776695296642));
#36898=CARTESIAN_POINT('',(7.15,3.3,0.));
#36899=CARTESIAN_POINT('',(7.06464466094067,3.3,0.0353553390593283));
#36900=CARTESIAN_POINT('Origin',(25.775,7.10732233047034,0.0176776695296635));
#36901=CARTESIAN_POINT('',(25.775,7.06464466094067,0.035355339059327));
#36902=CARTESIAN_POINT('',(25.775,7.15,0.));
#36903=CARTESIAN_POINT('Origin',(36.9545130195779,7.04548698042206,0.107322330470334));
#36904=CARTESIAN_POINT('',(36.9646446609407,7.09659258262892,0.0646446609406684));
#36905=CARTESIAN_POINT('',(36.9034074173711,7.03535533905933,0.064644660940667));
#36906=CARTESIAN_POINT('',(36.9646446609407,7.09659258262892,0.0646446609406675));
#36907=CARTESIAN_POINT('',(37.,7.05,0.149999999999996));
#36908=CARTESIAN_POINT('',(36.95,7.,0.149999999999999));
#36909=CARTESIAN_POINT('',(36.95,7.,0.149999999999999));
#36910=CARTESIAN_POINT('',(36.9034074173711,7.03535533905933,0.064644660940672));
#36911=CARTESIAN_POINT('Origin',(7.04548698042206,7.04548698042206,0.107322330470336));
#36912=CARTESIAN_POINT('',(7.05,7.,0.149999999999999));
#36913=CARTESIAN_POINT('',(7.0965925826289,7.03535533905933,0.064644660940672));
#36914=CARTESIAN_POINT('',(7.05,7.,0.149999999999999));
#36915=CARTESIAN_POINT('',(7.,7.05,0.15));
#36916=CARTESIAN_POINT('',(7.03535533905933,7.09659258262891,0.0646446609406737));
#36917=CARTESIAN_POINT('',(7.03535533905933,7.09659258262891,0.0646446609406732));
#36918=CARTESIAN_POINT('',(7.09659258262891,7.03535533905933,0.0646446609406715));
#36919=CARTESIAN_POINT('Origin',(7.025,7.025,0.));
#36920=CARTESIAN_POINT('',(7.05,7.,2.));
#36921=CARTESIAN_POINT('',(7.05,7.,0.));
#36922=CARTESIAN_POINT('',(7.05,7.,2.));
#36923=CARTESIAN_POINT('Origin',(7.025,6.6,2.025));
#36924=CARTESIAN_POINT('',(7.05,6.6,2.));
#36925=CARTESIAN_POINT('Origin',(7.01767766952966,9.9,0.107322330470337));
#36926=CARTESIAN_POINT('',(7.03535533905933,13.2,0.0646446609406729));
#36927=CARTESIAN_POINT('',(7.,13.2,0.15));
#36928=CARTESIAN_POINT('',(7.03535533905933,9.9,0.0646446609406732));
#36929=CARTESIAN_POINT('Origin',(9.,13.2,0.107322330470336));
#36930=CARTESIAN_POINT('',(9.,15.1646446609407,0.0646446609406726));
#36931=CARTESIAN_POINT('',(9.,15.2,0.15));
#36932=CARTESIAN_POINT('Origin',(9.,13.2,0.0646446609406726));
#36933=CARTESIAN_POINT('Origin',(31.75,15.1823223304703,0.107322330470337));
#36934=CARTESIAN_POINT('',(35.,15.1646446609407,0.0646446609406739));
#36935=CARTESIAN_POINT('',(35.,15.2,0.150000000000001));
#36936=CARTESIAN_POINT('',(31.75,15.1646446609407,0.0646446609406733));
#36937=CARTESIAN_POINT('Origin',(35.,13.2,0.107322330470338));
#36938=CARTESIAN_POINT('',(36.9646446609407,13.2,0.0646446609406714));
#36939=CARTESIAN_POINT('',(37.,13.2,0.15));
#36940=CARTESIAN_POINT('Origin',(35.,13.2,0.0646446609406769));
#36941=CARTESIAN_POINT('Origin',(35.,13.2,0.15));
#36942=CARTESIAN_POINT('Origin',(36.9823223304703,-9.9,0.107322330470332));
#36943=CARTESIAN_POINT('',(36.9646446609407,-9.9,0.0646446609406684));
#36944=CARTESIAN_POINT('Origin',(10.7352062072616,10.7352062072616,-3.60458758547682));
#36945=CARTESIAN_POINT('',(10.7658248290464,10.7045875854768,-3.60458758547682));
#36946=CARTESIAN_POINT('',(10.7045875854768,10.7658248290464,-3.60458758547682));
#36947=CARTESIAN_POINT('Origin',(33.325,7.01767766952966,0.107322330470336));
#36948=CARTESIAN_POINT('',(33.325,7.03535533905933,0.064644660940672));
#36949=CARTESIAN_POINT('',(33.325,7.,0.149999999999999));
#36950=CARTESIAN_POINT('Origin',(36.975,7.025,0.));
#36951=CARTESIAN_POINT('',(36.95,7.,0.));
#36952=CARTESIAN_POINT('Origin',(37.9814604594051,6.01853954059497,1.11207908118983));
#36953=CARTESIAN_POINT('',(38.0120790811898,6.04915816237976,1.11207908118983));
#36954=CARTESIAN_POINT('',(37.9508418376203,5.98792091881018,1.11207908118983));
#36955=CARTESIAN_POINT('Origin',(35.,13.2,0.05));
#36956=CARTESIAN_POINT('',(35.,15.1,0.));
#36957=CARTESIAN_POINT('',(36.9,13.2,0.));
#36958=CARTESIAN_POINT('Origin',(7.05,6.6,0.05));
#36959=CARTESIAN_POINT('',(7.1,13.2,0.));
#36960=CARTESIAN_POINT('Origin',(28.5,15.15,0.05));
#36961=CARTESIAN_POINT('',(9.,15.1,0.));
#36962=CARTESIAN_POINT('Origin',(9.,13.2,0.05));
#36963=CARTESIAN_POINT('Origin',(6.9,-7.,0.));
#36964=CARTESIAN_POINT('',(6.9,-7.,2.));
#36965=CARTESIAN_POINT('Origin',(22.,0.,2.));
#36966=CARTESIAN_POINT('',(37.1,7.,2.));
#36967=CARTESIAN_POINT('',(32.725,-1.07156594925393E-16,2.));
#36968=CARTESIAN_POINT('Origin',(33.6,0.,2.));
#36969=CARTESIAN_POINT('Origin',(37.1,7.,0.));
#36970=CARTESIAN_POINT('Origin',(22.,0.,0.));
#36971=CARTESIAN_POINT('Origin',(29.55,7.05,0.05));
#36972=CARTESIAN_POINT('Origin',(36.95,-6.6,0.05));
#36973=CARTESIAN_POINT('Origin',(22.,0.,0.));
#36974=CARTESIAN_POINT('Origin',(9.4,13.,4.5));
#36975=CARTESIAN_POINT('',(8.4,13.,4.5));
#36976=CARTESIAN_POINT('Origin',(8.7,13.,4.5));
#36977=CARTESIAN_POINT('Origin',(9.4,13.7,4.5));
#36978=CARTESIAN_POINT('Origin',(9.4,13.,4.5));
#36979=CARTESIAN_POINT('Origin',(15.7,13.7,4.5));
#36980=CARTESIAN_POINT('Origin',(34.6,13.7,4.5));
#36981=CARTESIAN_POINT('Origin',(34.6,13.,4.5));
#36982=CARTESIAN_POINT('Origin',(35.3,13.,4.5));
#36983=CARTESIAN_POINT('Origin',(35.3,6.5,4.5));
#36984=CARTESIAN_POINT('Origin',(35.3,-13.,4.5));
#36985=CARTESIAN_POINT('Origin',(34.6,-13.,4.5));
#36986=CARTESIAN_POINT('Origin',(34.6,-13.7,4.5));
#36987=CARTESIAN_POINT('Origin',(28.3,-13.7,4.5));
#36988=CARTESIAN_POINT('Origin',(9.4,-13.7,4.5));
#36989=CARTESIAN_POINT('Origin',(9.4,-13.,4.5));
#36990=CARTESIAN_POINT('',(8.4,-13.,4.5));
#36991=CARTESIAN_POINT('Origin',(8.7,-13.,4.5));
#36992=CARTESIAN_POINT('Origin',(9.4,-13.,4.5));
#36993=CARTESIAN_POINT('Origin',(8.7,-6.5,4.5));
#36994=CARTESIAN_POINT('',(8.4,-6.5,4.5));
#36995=CARTESIAN_POINT('Origin',(9.4,-13.,6.));
#36996=CARTESIAN_POINT('',(8.4,-13.,6.));
#36997=CARTESIAN_POINT('Origin',(8.4,-13.,6.));
#36998=CARTESIAN_POINT('',(8.4,13.,6.));
#36999=CARTESIAN_POINT('Origin',(9.4,13.,6.));
#37000=CARTESIAN_POINT('Origin',(9.4,-13.,5.925));
#37001=CARTESIAN_POINT('',(8.4,-13.,5.85));
#37002=CARTESIAN_POINT('Origin',(8.325,-6.5,5.925));
#37003=CARTESIAN_POINT('',(8.4,13.,5.85));
#37004=CARTESIAN_POINT('Origin',(9.4,13.,5.925));
#37005=CARTESIAN_POINT('',(9.4,14.,5.85));
#37006=CARTESIAN_POINT('Origin',(15.7,14.075,5.925));
#37007=CARTESIAN_POINT('Origin',(9.,-13.2,5.925));
#37008=CARTESIAN_POINT('',(9.,-15.2,5.85));
#37009=CARTESIAN_POINT('Origin',(15.5,-15.125,5.925));
#37010=CARTESIAN_POINT('',(35.,-15.2,5.85));
#37011=CARTESIAN_POINT('Origin',(35.,-13.2,5.925));
#37012=CARTESIAN_POINT('',(37.,-13.2,5.85));
#37013=CARTESIAN_POINT('Origin',(36.925,-6.6,5.925));
#37014=CARTESIAN_POINT('Origin',(35.,-13.2,0.));
#37015=CARTESIAN_POINT('Origin',(20.,-14.59,5.2));
#37016=CARTESIAN_POINT('',(20.,-14.59,4.595));
#37017=CARTESIAN_POINT('Origin',(33.6,0.,3.09));
#37018=CARTESIAN_POINT('',(32.725,-1.07156594925393E-16,3.09));
#37019=CARTESIAN_POINT('Origin',(29.,-9.2,2.04828269369554));
#37020=CARTESIAN_POINT('',(29.,-9.2,1.89656538739108));
#37021=CARTESIAN_POINT('',(28.7475,-9.2,2.04828269369554));
#37022=CARTESIAN_POINT('Origin',(29.,9.2,2.04828269369554));
#37023=CARTESIAN_POINT('',(29.,9.2,1.89656538739108));
#37024=CARTESIAN_POINT('',(28.7475,9.2,2.04828269369554));
#37025=CARTESIAN_POINT('Origin',(11.,-9.2,2.04828269369554));
#37026=CARTESIAN_POINT('',(11.,-9.2,1.89656538739108));
#37027=CARTESIAN_POINT('',(10.7475,-9.2,2.04828269369554));
#37028=CARTESIAN_POINT('Origin',(11.,9.2,2.04828269369554));
#37029=CARTESIAN_POINT('',(11.,9.2,1.89656538739108));
#37030=CARTESIAN_POINT('',(10.7475,9.2,2.04828269369554));
#37031=CARTESIAN_POINT('Origin',(21.,12.5,4.2));
#37032=CARTESIAN_POINT('',(21.,12.5,3.6));
#37033=CARTESIAN_POINT('',(21.,12.5,4.2));
#37034=CARTESIAN_POINT('',(21.,-12.5,3.6));
#37035=CARTESIAN_POINT('Origin',(19.,12.5,4.2));
#37036=CARTESIAN_POINT('',(21.,12.5,3.6));
#37037=CARTESIAN_POINT('Origin',(20.,0.,3.6));
#37038=CARTESIAN_POINT('Origin',(35.,13.2,0.));
#37039=CARTESIAN_POINT('',(0.,0.,0.));
#37040=CARTESIAN_POINT('Origin',(33.5,-5.31299340340571E-17,33.4823223304703));
#37041=CARTESIAN_POINT('',(35.15,-2.02066721859314E-16,33.5));
#37042=CARTESIAN_POINT('Origin',(33.5,0.,33.5));
#37043=CARTESIAN_POINT('',(35.2353553390593,2.12519736136229E-16,33.4646446609407));
#37044=CARTESIAN_POINT('',(35.1926776695297,2.07293228997771E-16,33.4823223304703));
#37045=CARTESIAN_POINT('',(31.7646446609407,-2.12519736136228E-16,33.4646446609407));
#37046=CARTESIAN_POINT('Origin',(33.5,-1.06259868068114E-16,33.4646446609407));
#37047=CARTESIAN_POINT('Origin',(33.5,-1.06259868068114E-16,33.4646446609407));
#37048=CARTESIAN_POINT('Origin',(33.5,0.,33.45));
#37049=CARTESIAN_POINT('',(31.7353553390593,-2.16106643565346E-16,33.4353553390593));
#37050=CARTESIAN_POINT('',(31.75,-2.14313189850787E-16,33.45));
#37051=CARTESIAN_POINT('',(35.2646446609407,-2.16106643565346E-16,33.4353553390593));
#37052=CARTESIAN_POINT('Origin',(33.5,-1.08053321782673E-16,33.4353553390593));
#37053=CARTESIAN_POINT('Origin',(33.5,-1.08053321782673E-16,33.4353553390593));
#37054=CARTESIAN_POINT('Origin',(33.5,0.,33.5));
#37055=CARTESIAN_POINT('',(32.895,-7.40911313484154E-17,33.5));
#37056=CARTESIAN_POINT('Origin',(33.5,0.,33.5));
#37057=CARTESIAN_POINT('Origin',(33.5,-5.40266608913365E-17,33.3926776695297));
#37058=CARTESIAN_POINT('',(35.3,2.20436423846523E-16,33.35));
#37059=CARTESIAN_POINT('',(35.2823223304703,2.18271533705935E-16,33.3926776695297));
#37060=CARTESIAN_POINT('',(31.7,-2.20436423846523E-16,33.35));
#37061=CARTESIAN_POINT('Origin',(33.5,0.,33.35));
#37062=CARTESIAN_POINT('Origin',(33.5,0.,33.35));
#37063=CARTESIAN_POINT('Origin',(33.5,0.,29.95));
#37064=CARTESIAN_POINT('',(31.7,-2.9062945342485E-16,32.));
#37065=CARTESIAN_POINT('',(31.7,-2.20436423846523E-16,29.95));
#37066=CARTESIAN_POINT('',(33.5,-1.8,31.6971145840745));
#37067=CARTESIAN_POINT('Ctrl Pts',(33.5,-1.8,31.6971145840745));
#37068=CARTESIAN_POINT('Ctrl Pts',(33.3860566581303,-1.8,31.6971145840745));
#37069=CARTESIAN_POINT('Ctrl Pts',(33.2685178334622,-1.78900665408164,31.700965713284));
#37070=CARTESIAN_POINT('Ctrl Pts',(33.0352764413812,-1.74303207564077,31.716553300941));
#37071=CARTESIAN_POINT('Ctrl Pts',(32.9195702475634,-1.70806396550477,31.7282741932561));
#37072=CARTESIAN_POINT('Ctrl Pts',(32.6981116334826,-1.61596921995123,31.7574686694119));
#37073=CARTESIAN_POINT('Ctrl Pts',(32.5921667861828,-1.55876952413463,31.7749340986735));
#37074=CARTESIAN_POINT('Ctrl Pts',(32.3964416611508,-1.42691365092969,31.8121191258143));
#37075=CARTESIAN_POINT('Ctrl Pts',(32.3066617865707,-1.3522461988423,31.8318008558006));
#37076=CARTESIAN_POINT('Ctrl Pts',(32.1477879055675,-1.19337231783909,31.8695928089871));
#37077=CARTESIAN_POINT('Ctrl Pts',(32.0731245394823,-1.10360856854857,31.8890590514301));
#37078=CARTESIAN_POINT('Ctrl Pts',(31.9412537861583,-0.907874271943785,
31.9254652923589));
#37079=CARTESIAN_POINT('Ctrl Pts',(31.8840366362977,-0.801904114450162,
31.9423720162283));
#37080=CARTESIAN_POINT('Ctrl Pts',(31.7919223266258,-0.580395123714868,
31.9704300444786));
#37081=CARTESIAN_POINT('Ctrl Pts',(31.7569520118305,-0.464664625832372,
31.9815821366528));
#37082=CARTESIAN_POINT('Ctrl Pts',(31.7109845655851,-0.231415814089425,
31.9963717720298));
#37083=CARTESIAN_POINT('Ctrl Pts',(31.7,-0.113894433434802,32.));
#37084=CARTESIAN_POINT('Ctrl Pts',(31.7,-1.66533453693773E-16,32.));
#37085=CARTESIAN_POINT('Ctrl Pts',(31.7,-2.22044604925031E-16,32.));
#37086=CARTESIAN_POINT('Ctrl Pts',(31.7,0.113894433434802,32.));
#37087=CARTESIAN_POINT('Ctrl Pts',(31.7109845655851,0.231415814089425,31.9963717720298));
#37088=CARTESIAN_POINT('Ctrl Pts',(31.7569520118305,0.464664625832373,31.9815821366528));
#37089=CARTESIAN_POINT('Ctrl Pts',(31.7919223266258,0.58039512371487,31.9704300444786));
#37090=CARTESIAN_POINT('Ctrl Pts',(31.8840366362977,0.801904114450163,31.9423720162283));
#37091=CARTESIAN_POINT('Ctrl Pts',(31.9412537861583,0.907874271943785,31.9254652923589));
#37092=CARTESIAN_POINT('Ctrl Pts',(32.0731245394823,1.10360856854856,31.8890590514301));
#37093=CARTESIAN_POINT('Ctrl Pts',(32.1477879055675,1.19337231783909,31.8695928089871));
#37094=CARTESIAN_POINT('Ctrl Pts',(32.3066617865707,1.3522461988423,31.8318008558006));
#37095=CARTESIAN_POINT('Ctrl Pts',(32.3964416611508,1.4269136509297,31.8121191258143));
#37096=CARTESIAN_POINT('Ctrl Pts',(32.5921667861828,1.55876952413463,31.7749340986735));
#37097=CARTESIAN_POINT('Ctrl Pts',(32.6981116334826,1.61596921995123,31.7574686694119));
#37098=CARTESIAN_POINT('Ctrl Pts',(32.9195702475634,1.70806396550477,31.7282741932561));
#37099=CARTESIAN_POINT('Ctrl Pts',(33.0352764413812,1.74303207564077,31.716553300941));
#37100=CARTESIAN_POINT('Ctrl Pts',(33.2685178334622,1.78900665408164,31.700965713284));
#37101=CARTESIAN_POINT('Ctrl Pts',(33.3860566581303,1.8,31.6971145840745));
#37102=CARTESIAN_POINT('Ctrl Pts',(33.6139433418697,1.8,31.6971145840745));
#37103=CARTESIAN_POINT('Ctrl Pts',(33.7314821665378,1.78900665408164,31.700965713284));
#37104=CARTESIAN_POINT('Ctrl Pts',(33.9647235586188,1.74303207564077,31.716553300941));
#37105=CARTESIAN_POINT('Ctrl Pts',(34.0804297524366,1.70806396550477,31.7282741932561));
#37106=CARTESIAN_POINT('Ctrl Pts',(34.3018883665174,1.61596921995123,31.7574686694119));
#37107=CARTESIAN_POINT('Ctrl Pts',(34.4078332138172,1.55876952413463,31.7749340986735));
#37108=CARTESIAN_POINT('Ctrl Pts',(34.6035583388492,1.4269136509297,31.8121191258143));
#37109=CARTESIAN_POINT('Ctrl Pts',(34.6933382134293,1.3522461988423,31.8318008558006));
#37110=CARTESIAN_POINT('Ctrl Pts',(34.8522120944325,1.19337231783909,31.8695928089871));
#37111=CARTESIAN_POINT('Ctrl Pts',(34.9268754605177,1.10360856854856,31.8890590514301));
#37112=CARTESIAN_POINT('Ctrl Pts',(35.0587462138417,0.907874271943785,31.9254652923589));
#37113=CARTESIAN_POINT('Ctrl Pts',(35.1159633637023,0.801904114450164,31.9423720162283));
#37114=CARTESIAN_POINT('Ctrl Pts',(35.2080776733742,0.58039512371487,31.9704300444786));
#37115=CARTESIAN_POINT('Ctrl Pts',(35.2430479881695,0.464664625832375,31.9815821366528));
#37116=CARTESIAN_POINT('Ctrl Pts',(35.2890154344149,0.231415814089427,31.9963717720298));
#37117=CARTESIAN_POINT('Ctrl Pts',(35.3,0.113894433434802,32.));
#37118=CARTESIAN_POINT('Ctrl Pts',(35.3,-0.113894433434802,32.));
#37119=CARTESIAN_POINT('Ctrl Pts',(35.2890154344149,-0.231415814089426,
31.9963717720298));
#37120=CARTESIAN_POINT('Ctrl Pts',(35.2430479881695,-0.464664625832374,
31.9815821366528));
#37121=CARTESIAN_POINT('Ctrl Pts',(35.2080776733742,-0.58039512371487,31.9704300444786));
#37122=CARTESIAN_POINT('Ctrl Pts',(35.1159633637023,-0.801904114450163,
31.9423720162283));
#37123=CARTESIAN_POINT('Ctrl Pts',(35.0587462138417,-0.907874271943786,
31.9254652923589));
#37124=CARTESIAN_POINT('Ctrl Pts',(34.9268754605177,-1.10360856854856,31.8890590514301));
#37125=CARTESIAN_POINT('Ctrl Pts',(34.8522120944325,-1.19337231783909,31.8695928089871));
#37126=CARTESIAN_POINT('Ctrl Pts',(34.6933382134293,-1.3522461988423,31.8318008558006));
#37127=CARTESIAN_POINT('Ctrl Pts',(34.6035583388492,-1.4269136509297,31.8121191258143));
#37128=CARTESIAN_POINT('Ctrl Pts',(34.4078332138172,-1.55876952413463,31.7749340986735));
#37129=CARTESIAN_POINT('Ctrl Pts',(34.3018883665174,-1.61596921995123,31.7574686694119));
#37130=CARTESIAN_POINT('Ctrl Pts',(34.0804297524366,-1.70806396550477,31.7282741932561));
#37131=CARTESIAN_POINT('Ctrl Pts',(33.9647235586188,-1.74303207564076,31.716553300941));
#37132=CARTESIAN_POINT('Ctrl Pts',(33.7314821665378,-1.78900665408164,31.700965713284));
#37133=CARTESIAN_POINT('Ctrl Pts',(33.6139433418697,-1.8,31.6971145840745));
#37134=CARTESIAN_POINT('Ctrl Pts',(33.5,-1.8,31.6971145840745));
#37135=CARTESIAN_POINT('Origin',(8.025,3.53553390593274,30.0355339059327));
#37136=CARTESIAN_POINT('',(8.,3.60696374383365,30.3832734323853));
#37137=CARTESIAN_POINT('',(8.,3.8832734323853,30.1069637438337));
#37138=CARTESIAN_POINT('Ctrl Pts',(8.,3.60696374383365,30.3832734323853));
#37139=CARTESIAN_POINT('Ctrl Pts',(8.01789140164846,3.66596515189423,30.3528888836206));
#37140=CARTESIAN_POINT('Ctrl Pts',(8.0275,3.72132986391805,30.3128928896246));
#37141=CARTESIAN_POINT('Ctrl Pts',(8.0275,3.81289288962462,30.2213298639181));
#37142=CARTESIAN_POINT('Ctrl Pts',(8.01789140164846,3.85288888362064,30.1659651518942));
#37143=CARTESIAN_POINT('Ctrl Pts',(8.,3.8832734323853,30.1069637438336));
#37144=CARTESIAN_POINT('',(8.,3.53553390593274,30.3905339059327));
#37145=CARTESIAN_POINT('Origin',(8.,3.53553390593274,30.0355339059327));
#37146=CARTESIAN_POINT('',(8.05,3.53553390593274,30.3405339059327));
#37147=CARTESIAN_POINT('',(8.025,3.53553390593274,30.3655339059327));
#37148=CARTESIAN_POINT('',(8.05,3.53553390593274,29.7305339059327));
#37149=CARTESIAN_POINT('Origin',(8.05,3.53553390593274,30.0355339059327));
#37150=CARTESIAN_POINT('Origin',(8.05,3.53553390593274,30.0355339059327));
#37151=CARTESIAN_POINT('Origin',(8.,3.53553390593274,30.0355339059327));
#37152=CARTESIAN_POINT('Origin',(8.1,0.,26.5));
#37153=CARTESIAN_POINT('',(8.2,5.5,26.5));
#37154=CARTESIAN_POINT('',(8.2,-5.5,26.5));
#37155=CARTESIAN_POINT('Origin',(8.2,0.,26.5));
#37156=CARTESIAN_POINT('Origin',(8.2,0.,26.5));
#37157=CARTESIAN_POINT('',(8.,5.3,26.5));
#37158=CARTESIAN_POINT('',(8.1,5.4,26.5));
#37159=CARTESIAN_POINT('Origin',(8.,0.,26.5));
#37160=CARTESIAN_POINT('',(8.,-3.60696374383365,30.3832734323853));
#37161=CARTESIAN_POINT('Origin',(8.,0.,26.5));
#37162=CARTESIAN_POINT('',(8.,-3.8832734323853,30.1069637438337));
#37163=CARTESIAN_POINT('Ctrl Pts',(8.,-3.8832734323853,30.1069637438337));
#37164=CARTESIAN_POINT('Ctrl Pts',(8.01789140164973,-3.85288888361848,30.1659651518984));
#37165=CARTESIAN_POINT('Ctrl Pts',(8.0275,-3.81289288959515,30.2213298639475));
#37166=CARTESIAN_POINT('Ctrl Pts',(8.0275,-3.72132986394751,30.3128928895952));
#37167=CARTESIAN_POINT('Ctrl Pts',(8.01789140164973,-3.66596515189844,30.3528888836185));
#37168=CARTESIAN_POINT('Ctrl Pts',(8.,-3.60696374383365,30.3832734323853));
#37169=CARTESIAN_POINT('',(8.,-3.8832734323853,22.8930362561663));
#37170=CARTESIAN_POINT('Origin',(8.,0.,26.5));
#37171=CARTESIAN_POINT('',(8.,-3.60696374383365,22.6167265676147));
#37172=CARTESIAN_POINT('Ctrl Pts',(8.,-3.60696374383365,22.6167265676147));
#37173=CARTESIAN_POINT('Ctrl Pts',(8.01789141230059,-3.66596518702231,22.6471111344696));
#37174=CARTESIAN_POINT('Ctrl Pts',(8.0275,-3.72133011029548,22.6871073567528));
#37175=CARTESIAN_POINT('Ctrl Pts',(8.0275,-3.81289264324719,22.7786698897045));
#37176=CARTESIAN_POINT('Ctrl Pts',(8.01789141230058,-3.85288886553039,22.8340348129777));
#37177=CARTESIAN_POINT('Ctrl Pts',(8.,-3.8832734323853,22.8930362561663));
#37178=CARTESIAN_POINT('',(8.,3.60696374383366,22.6167265676147));
#37179=CARTESIAN_POINT('Origin',(8.,0.,26.5));
#37180=CARTESIAN_POINT('',(8.,3.88327343238529,22.8930362561663));
#37181=CARTESIAN_POINT('Ctrl Pts',(8.,3.88327343238529,22.8930362561663));
#37182=CARTESIAN_POINT('Ctrl Pts',(8.01789140164846,3.85288888362063,22.8340348481058));
#37183=CARTESIAN_POINT('Ctrl Pts',(8.0275,3.81289288962461,22.7786701360819));
#37184=CARTESIAN_POINT('Ctrl Pts',(8.0275,3.72132986391806,22.6871071103754));
#37185=CARTESIAN_POINT('Ctrl Pts',(8.01789140164846,3.66596515189424,22.6471111163794));
#37186=CARTESIAN_POINT('Ctrl Pts',(8.,3.60696374383366,22.6167265676147));
#37187=CARTESIAN_POINT('Origin',(8.,0.,26.5));
#37188=CARTESIAN_POINT('Origin',(8.685,3.53553390593274,30.0355339059327));
#37189=CARTESIAN_POINT('',(9.4,3.53553390593274,29.7305339059327));
#37190=CARTESIAN_POINT('Origin',(9.4,3.53553390593274,30.0355339059327));
#37191=CARTESIAN_POINT('',(8.685,3.53553390593274,29.7305339059327));
#37192=CARTESIAN_POINT('Origin',(8.025,3.53553390593274,22.9644660940673));
#37193=CARTESIAN_POINT('',(8.,3.53553390593274,22.6094660940673));
#37194=CARTESIAN_POINT('Origin',(8.,3.53553390593274,22.9644660940673));
#37195=CARTESIAN_POINT('',(8.05,3.53553390593274,22.6594660940673));
#37196=CARTESIAN_POINT('',(8.025,3.53553390593274,22.6344660940673));
#37197=CARTESIAN_POINT('Origin',(8.05,3.53553390593274,22.9644660940673));
#37198=CARTESIAN_POINT('Origin',(8.,3.53553390593274,22.9644660940673));
#37199=CARTESIAN_POINT('Origin',(8.685,3.53553390593274,22.9644660940673));
#37200=CARTESIAN_POINT('',(9.4,3.53553390593274,22.6594660940673));
#37201=CARTESIAN_POINT('Origin',(9.4,3.53553390593274,22.9644660940673));
#37202=CARTESIAN_POINT('',(8.685,3.53553390593274,22.6594660940673));
#37203=CARTESIAN_POINT('Origin',(21.025,-5.55,4.225));
#37204=CARTESIAN_POINT('',(21.025,10.975,4.225));
#37205=CARTESIAN_POINT('',(21.05,10.95,4.2));
#37206=CARTESIAN_POINT('',(24.4416666666667,7.55833333333329,0.808333333333354));
#37207=CARTESIAN_POINT('',(21.05,-10.95,4.2));
#37208=CARTESIAN_POINT('',(21.05,-5.55,4.2));
#37209=CARTESIAN_POINT('',(21.025,-10.975,4.225));
#37210=CARTESIAN_POINT('',(20.925,-11.075,4.325));
#37211=CARTESIAN_POINT('',(21.,-10.95,4.25));
#37212=CARTESIAN_POINT('',(20.125,-10.075,5.12499999999999));
#37213=CARTESIAN_POINT('',(21.,10.95,4.25));
#37214=CARTESIAN_POINT('',(21.,-5.55,4.25));
#37215=CARTESIAN_POINT('',(18.275,8.22499999999997,6.97499999999998));
#37216=CARTESIAN_POINT('Origin',(20.,0.,4.2));
#37217=CARTESIAN_POINT('',(30.,10.95,4.2));
#37218=CARTESIAN_POINT('',(25.,10.95,4.2));
#37219=CARTESIAN_POINT('',(30.665,10.6784357007116,4.2));
#37220=CARTESIAN_POINT('Origin',(30.,10.,4.2));
#37221=CARTESIAN_POINT('',(30.7,10.6423370590817,4.2));
#37222=CARTESIAN_POINT('Ctrl Pts',(30.7,10.6423370590817,4.2));
#37223=CARTESIAN_POINT('Ctrl Pts',(30.6885903428187,10.6546728503156,4.2));
#37224=CARTESIAN_POINT('Ctrl Pts',(30.6769830660874,10.6666899465601,4.2));
#37225=CARTESIAN_POINT('Ctrl Pts',(30.665,10.6784357007116,4.2));
#37226=CARTESIAN_POINT('',(30.7,-10.6423370590817,4.2));
#37227=CARTESIAN_POINT('',(30.7,0.,4.2));
#37228=CARTESIAN_POINT('',(30.665,-10.6784357007116,4.2));
#37229=CARTESIAN_POINT('Ctrl Pts',(30.665,-10.6784357007116,4.2));
#37230=CARTESIAN_POINT('Ctrl Pts',(30.6769830660874,-10.6666899465601,4.2));
#37231=CARTESIAN_POINT('Ctrl Pts',(30.6885903428187,-10.6546728503156,4.2));
#37232=CARTESIAN_POINT('Ctrl Pts',(30.7,-10.6423370590817,4.2));
#37233=CARTESIAN_POINT('',(30.,-10.95,4.2));
#37234=CARTESIAN_POINT('Origin',(30.,-10.,4.2));
#37235=CARTESIAN_POINT('',(15.,-10.95,4.2));
#37236=CARTESIAN_POINT('',(28.4,9.,4.2));
#37237=CARTESIAN_POINT('',(28.4,9.4,4.2));
#37238=CARTESIAN_POINT('',(28.4,4.5,4.2));
#37239=CARTESIAN_POINT('',(29.6,9.,4.2));
#37240=CARTESIAN_POINT('Origin',(29.,9.,4.2));
#37241=CARTESIAN_POINT('',(29.6,9.4,4.2));
#37242=CARTESIAN_POINT('',(29.6,4.7,4.2));
#37243=CARTESIAN_POINT('Origin',(29.,9.4,4.2));
#37244=CARTESIAN_POINT('',(28.4,-9.4,4.2));
#37245=CARTESIAN_POINT('',(28.4,-9.,4.2));
#37246=CARTESIAN_POINT('',(28.4,-4.7,4.2));
#37247=CARTESIAN_POINT('',(29.6,-9.4,4.2));
#37248=CARTESIAN_POINT('Origin',(29.,-9.4,4.2));
#37249=CARTESIAN_POINT('',(29.6,-9.,4.2));
#37250=CARTESIAN_POINT('',(29.6,-4.5,4.2));
#37251=CARTESIAN_POINT('Origin',(29.,-9.,4.2));
#37252=CARTESIAN_POINT('Origin',(25.,10.975,4.225));
#37253=CARTESIAN_POINT('',(21.05,11.,4.25));
#37254=CARTESIAN_POINT('',(21.05,11.,4.25));
#37255=CARTESIAN_POINT('',(30.,11.,4.25));
#37256=CARTESIAN_POINT('',(25.,11.,4.25));
#37257=CARTESIAN_POINT('',(30.,11.,4.25));
#37258=CARTESIAN_POINT('Origin',(21.025,10.975,4.2));
#37259=CARTESIAN_POINT('',(21.,10.95,4.8));
#37260=CARTESIAN_POINT('',(21.,10.95,4.2));
#37261=CARTESIAN_POINT('',(21.05,11.,4.85));
#37262=CARTESIAN_POINT('',(21.,10.95,4.8));
#37263=CARTESIAN_POINT('',(21.05,11.,4.2));
#37264=CARTESIAN_POINT('Origin',(35.9823223304703,0.,26.5));
#37265=CARTESIAN_POINT('',(35.9646446609407,5.33535533905933,26.5));
#37266=CARTESIAN_POINT('Origin',(35.9646446609407,0.,26.5));
#37267=CARTESIAN_POINT('',(36.,5.25,26.5));
#37268=CARTESIAN_POINT('',(35.9823223304703,5.29267766952966,26.5));
#37269=CARTESIAN_POINT('Origin',(36.,0.,26.5));
#37270=CARTESIAN_POINT('Origin',(35.9,0.,26.5));
#37271=CARTESIAN_POINT('',(35.8353553390593,5.46464466094067,26.5));
#37272=CARTESIAN_POINT('',(35.9,5.4,26.5));
#37273=CARTESIAN_POINT('Origin',(35.8353553390593,0.,26.5));
#37274=CARTESIAN_POINT('Origin',(36.,0.,26.5));
#37275=CARTESIAN_POINT('',(36.,-3.5,26.5));
#37276=CARTESIAN_POINT('Origin',(36.,0.,26.5));
#37277=CARTESIAN_POINT('Ctrl Pts',(34.5,-0.749563950038172,21.0513163163198));
#37278=CARTESIAN_POINT('Ctrl Pts',(34.6078091511127,-0.749563950038172,
21.0513163163198));
#37279=CARTESIAN_POINT('Ctrl Pts',(34.7811032097204,-0.711754547708119,
21.0458589692126));
#37280=CARTESIAN_POINT('Ctrl Pts',(34.974965121707,-0.587314921207312,21.0311479468387));
#37281=CARTESIAN_POINT('Ctrl Pts',(35.0549239124764,-0.507046229905794,
21.0232925177222));
#37282=CARTESIAN_POINT('Ctrl Pts',(35.0977756120755,-0.452152037495066,
21.0186704724503));
#37283=CARTESIAN_POINT('Ctrl Pts',(35.1143542325059,-0.429612298109788,
21.0168443285933));
#37284=CARTESIAN_POINT('Ctrl Pts',(35.1340422591755,-0.400351661687876,
21.0146094007192));
#37285=CARTESIAN_POINT('Ctrl Pts',(35.1557767361487,-0.363704460367538,
21.0120527916887));
#37286=CARTESIAN_POINT('Ctrl Pts',(35.1820502322802,-0.313074653150546,
21.0088643148667));
#37287=CARTESIAN_POINT('Ctrl Pts',(35.2039675401431,-0.260041744395718,
21.0060858902635));
#37288=CARTESIAN_POINT('Ctrl Pts',(35.2212309037757,-0.205721880481172,
21.0038401171032));
#37289=CARTESIAN_POINT('Ctrl Pts',(35.2563431722199,-0.0671819342670894,
20.9991778701227));
#37290=CARTESIAN_POINT('Ctrl Pts',(35.2560871656414,0.0626491158681729,
20.9991981622569));
#37291=CARTESIAN_POINT('Ctrl Pts',(35.2245604862986,0.191862595129649,21.0033883099402));
#37292=CARTESIAN_POINT('Ctrl Pts',(35.214068499096,0.228356974265122,21.004762450079));
#37293=CARTESIAN_POINT('Ctrl Pts',(35.1923007590141,0.291280650338835,21.0075819713019));
#37294=CARTESIAN_POINT('Ctrl Pts',(35.0993946204602,0.481448989298802,21.0190440514598));
#37295=CARTESIAN_POINT('Ctrl Pts',(34.9566260210823,0.614115291433095,21.0340667746151));
#37296=CARTESIAN_POINT('Ctrl Pts',(34.8005645030701,0.686149513350896,21.043032043578));
#37297=CARTESIAN_POINT('Ctrl Pts',(34.7653478169603,0.700689089135733,21.0448800812064));
#37298=CARTESIAN_POINT('Ctrl Pts',(34.702486674947,0.722760619862234,21.0477448745898));
#37299=CARTESIAN_POINT('Ctrl Pts',(34.5716817460195,0.751594137177719,21.0516605025898));
#37300=CARTESIAN_POINT('Ctrl Pts',(34.4466588488531,0.751912455450576,21.0516805007024));
#37301=CARTESIAN_POINT('Ctrl Pts',(34.2979168099864,0.724426508507403,21.0479597951114));
#37302=CARTESIAN_POINT('Ctrl Pts',(34.1711411964527,0.680510140463003,21.0421401113897));
#37303=CARTESIAN_POINT('Ctrl Pts',(34.0254400152268,0.587512193866294,21.0312041853341));
#37304=CARTESIAN_POINT('Ctrl Pts',(33.9119242783867,0.473659340333228,21.019990938314));
#37305=CARTESIAN_POINT('Ctrl Pts',(33.8341349430927,0.352541117917839,21.0109182636443));
#37306=CARTESIAN_POINT('Ctrl Pts',(33.7987498653191,0.266554791315046,21.0064207443541));
#37307=CARTESIAN_POINT('Ctrl Pts',(33.785196053886,0.225933611733011,21.0046676361538));
#37308=CARTESIAN_POINT('Ctrl Pts',(33.7790286911615,0.205467311567983,21.0038613997373));
#37309=CARTESIAN_POINT('Ctrl Pts',(33.7743776719825,0.188304504278709,21.0032490851194));
#37310=CARTESIAN_POINT('Ctrl Pts',(33.7713876543967,0.17624582215462,21.00285311147));
#37311=CARTESIAN_POINT('Ctrl Pts',(33.7697534967433,0.169351646984093,21.0026362335653));
#37312=CARTESIAN_POINT('Ctrl Pts',(33.7436322538446,0.0552211959972136,
20.9991614986988));
#37313=CARTESIAN_POINT('Ctrl Pts',(33.743587569203,-0.0671233551084263,
20.9991689935559));
#37314=CARTESIAN_POINT('Ctrl Pts',(33.7787073248947,-0.20567073339148,21.0038317959733));
#37315=CARTESIAN_POINT('Ctrl Pts',(33.7959736390573,-0.259995325676423,
21.0060780038898));
#37316=CARTESIAN_POINT('Ctrl Pts',(33.8233767787127,-0.326253771531467,
21.0095516426503));
#37317=CARTESIAN_POINT('Ctrl Pts',(33.8580412322199,-0.388632549296444,
21.0137091580996));
#37318=CARTESIAN_POINT('Ctrl Pts',(33.8856030358547,-0.42960122555939,21.0168381467451));
#37319=CARTESIAN_POINT('Ctrl Pts',(33.9021823878193,-0.452140301878644,
21.0186643472973));
#37320=CARTESIAN_POINT('Ctrl Pts',(33.945034720446,-0.507035206264715,21.0232865152258));
#37321=CARTESIAN_POINT('Ctrl Pts',(34.02500542513,-0.587306740554846,21.0311436542917));
#37322=CARTESIAN_POINT('Ctrl Pts',(34.2188700233853,-0.711747372551822,
21.0458550828561));
#37323=CARTESIAN_POINT('Ctrl Pts',(34.3921908488873,-0.749563950038174,
21.0513163163198));
#37324=CARTESIAN_POINT('Ctrl Pts',(34.5,-0.749563950038174,21.0513163163198));
#37325=CARTESIAN_POINT('Ctrl Pts',(34.5,-0.733042633358783,21.0657866512817));
#37326=CARTESIAN_POINT('Ctrl Pts',(34.6057023393761,-0.733042633358783,
21.0657866512817));
#37327=CARTESIAN_POINT('Ctrl Pts',(34.7755983155706,-0.69581787485872,21.060547064769));
#37328=CARTESIAN_POINT('Ctrl Pts',(34.9652246436437,-0.573673233549097,
21.0464470738094));
#37329=CARTESIAN_POINT('Ctrl Pts',(35.0432940001379,-0.495046067925316,
21.0389275943025));
#37330=CARTESIAN_POINT('Ctrl Pts',(35.0850937946794,-0.441336105285769,
21.0345060806934));
#37331=CARTESIAN_POINT('Ctrl Pts',(35.1012616050954,-0.419288232709881,
21.0327594496866));
#37332=CARTESIAN_POINT('Ctrl Pts',(35.1204550010736,-0.390676354751433,
21.0306223291988));
#37333=CARTESIAN_POINT('Ctrl Pts',(35.1416337966199,-0.354858778393741,
21.028178358288));
#37334=CARTESIAN_POINT('Ctrl Pts',(35.1672245914793,-0.305397290800612,
21.0251312396614));
#37335=CARTESIAN_POINT('Ctrl Pts',(35.1885584093061,-0.253620878979568,
21.0224771785701));
#37336=CARTESIAN_POINT('Ctrl Pts',(35.2053550452028,-0.200615260478044,
21.0203325632711));
#37337=CARTESIAN_POINT('Ctrl Pts',(35.2395058919798,-0.0654667973481286,
21.015881422341));
#37338=CARTESIAN_POINT('Ctrl Pts',(35.2392542870293,0.0610529003734771,
21.015901035455));
#37339=CARTESIAN_POINT('Ctrl Pts',(35.2085910301353,0.187098413030655,21.0199014530354));
#37340=CARTESIAN_POINT('Ctrl Pts',(35.1983841264211,0.222704517693513,21.0212135528815));
#37341=CARTESIAN_POINT('Ctrl Pts',(35.1772017415125,0.284115878094912,21.0239064472591));
#37342=CARTESIAN_POINT('Ctrl Pts',(35.086739809034,0.469851258313408,21.0348573742634));
#37343=CARTESIAN_POINT('Ctrl Pts',(34.9473718771303,0.599947262996566,21.0492416495909));
#37344=CARTESIAN_POINT('Ctrl Pts',(34.7945686206459,0.670705966532925,21.0578389402555));
#37345=CARTESIAN_POINT('Ctrl Pts',(34.7600803705086,0.684991273798064,21.0596112517484));
#37346=CARTESIAN_POINT('Ctrl Pts',(34.6985001107118,0.706684122867952,21.0623592585023));
#37347=CARTESIAN_POINT('Ctrl Pts',(34.5702945224947,0.73504254109294,21.0661167286091));
#37348=CARTESIAN_POINT('Ctrl Pts',(34.4476926648849,0.735353817210617,21.0661358844675));
#37349=CARTESIAN_POINT('Ctrl Pts',(34.3018943159103,0.7083223007901,21.0625655773374));
#37350=CARTESIAN_POINT('Ctrl Pts',(34.1776922995948,0.665147105862844,21.0569823906373));
#37351=CARTESIAN_POINT('Ctrl Pts',(34.0351710176682,0.573870276104217,21.0465010716371));
#37352=CARTESIAN_POINT('Ctrl Pts',(33.9243384424563,0.462339732239533,21.0357669569419));
#37353=CARTESIAN_POINT('Ctrl Pts',(33.8485284690001,0.343927579036483,21.0270930625743));
#37354=CARTESIAN_POINT('Ctrl Pts',(33.8140866906283,0.259980124680835,21.0227969523571));
#37355=CARTESIAN_POINT('Ctrl Pts',(33.8008981126124,0.220338324686709,21.0211227123327));
#37356=CARTESIAN_POINT('Ctrl Pts',(33.7948979815476,0.200368717872555,21.0203528356669));
#37357=CARTESIAN_POINT('Ctrl Pts',(33.7903736414347,0.183624806520544,21.0197681873269));
#37358=CARTESIAN_POINT('Ctrl Pts',(33.7874653554772,0.171861616917887,21.0193901307647));
#37359=CARTESIAN_POINT('Ctrl Pts',(33.7858759264221,0.165136687330697,21.019183071464));
#37360=CARTESIAN_POINT('Ctrl Pts',(33.7604707367237,0.0538115303858986,
21.0158657500753));
#37361=CARTESIAN_POINT('Ctrl Pts',(33.7604260304133,-0.0654105160144948,
21.0158728480868));
#37362=CARTESIAN_POINT('Ctrl Pts',(33.7945842900857,-0.200566142677479,
21.0203245347726));
#37363=CARTESIAN_POINT('Ctrl Pts',(33.8113838087165,-0.253576346029871,
21.0224695672281));
#37364=CARTESIAN_POINT('Ctrl Pts',(33.8380574859515,-0.318264908355468,
21.0257877329048));
#37365=CARTESIAN_POINT('Ctrl Pts',(33.8718270287516,-0.379217750812714,
21.0297614242812));
#37366=CARTESIAN_POINT('Ctrl Pts',(33.8986963825208,-0.419278054518851,
21.0327534797157));
#37367=CARTESIAN_POINT('Ctrl Pts',(33.914864910764,-0.4413252762906,21.0345001654573));
#37368=CARTESIAN_POINT('Ctrl Pts',(33.9566653285551,-0.495035919990978,
21.0389217975292));
#37369=CARTESIAN_POINT('Ctrl Pts',(34.0347463980485,-0.573665687092292,
21.0464429283745));
#37370=CARTESIAN_POINT('Ctrl Pts',(34.2243753676715,-0.695811267696493,
21.0605433116086));
#37371=CARTESIAN_POINT('Ctrl Pts',(34.3942976606239,-0.733042633358783,
21.0657866512817));
#37372=CARTESIAN_POINT('Ctrl Pts',(34.5,-0.733042633358783,21.0657866512817));
#37373=CARTESIAN_POINT('Ctrl Pts',(34.5,-0.716521316679393,21.0802569862437));
#37374=CARTESIAN_POINT('Ctrl Pts',(34.6035955276396,-0.716521316679393,
21.0802569862437));
#37375=CARTESIAN_POINT('Ctrl Pts',(34.7700934214207,-0.67988120200932,21.0752351603254));
#37376=CARTESIAN_POINT('Ctrl Pts',(34.9554841655803,-0.560031545890881,
21.06174620078));
#37377=CARTESIAN_POINT('Ctrl Pts',(35.0316640877993,-0.483045905944838,
21.0545626708828));
#37378=CARTESIAN_POINT('Ctrl Pts',(35.0724119772833,-0.430520173076471,
21.0503416889364));
#37379=CARTESIAN_POINT('Ctrl Pts',(35.0881689776849,-0.408964167309974,
21.0486745707798));
#37380=CARTESIAN_POINT('Ctrl Pts',(35.1068677429718,-0.38100104781499,21.0466352576783));
#37381=CARTESIAN_POINT('Ctrl Pts',(35.1274908570911,-0.346013096419943,
21.0443039248873));
#37382=CARTESIAN_POINT('Ctrl Pts',(35.1523989506783,-0.297719928450677,
21.041398164456));
#37383=CARTESIAN_POINT('Ctrl Pts',(35.1731492784692,-0.247200013563418,
21.0388684668766));
#37384=CARTESIAN_POINT('Ctrl Pts',(35.18947918663,-0.195508640474915,21.0368250094389));
#37385=CARTESIAN_POINT('Ctrl Pts',(35.2226686117397,-0.0637516604291672,
21.0325849745592));
#37386=CARTESIAN_POINT('Ctrl Pts',(35.2224214084173,0.0594566848787826,
21.032603908653));
#37387=CARTESIAN_POINT('Ctrl Pts',(35.1926215739719,0.182334230931662,21.0364145961305));
#37388=CARTESIAN_POINT('Ctrl Pts',(35.1826997537462,0.217052061121905,21.0376646556839));
#37389=CARTESIAN_POINT('Ctrl Pts',(35.162102724011,0.276951105850991,21.0402309232163));
#37390=CARTESIAN_POINT('Ctrl Pts',(35.0740849976077,0.458253527328016,21.0506706970671));
#37391=CARTESIAN_POINT('Ctrl Pts',(34.9381177331784,0.585779234560039,21.0644165245667));
#37392=CARTESIAN_POINT('Ctrl Pts',(34.7885727382217,0.655262419714956,21.0726458369329));
#37393=CARTESIAN_POINT('Ctrl Pts',(34.754812924057,0.669293458460397,21.0743424222905));
#37394=CARTESIAN_POINT('Ctrl Pts',(34.6945135464767,0.690607625873672,21.0769736424148));
#37395=CARTESIAN_POINT('Ctrl Pts',(34.5689072989699,0.718490945008162,21.0805729546284));
#37396=CARTESIAN_POINT('Ctrl Pts',(34.4487264809167,0.718795178970658,21.0805912682326));
#37397=CARTESIAN_POINT('Ctrl Pts',(34.3058718218342,0.692218093072797,21.0771713595635));
#37398=CARTESIAN_POINT('Ctrl Pts',(34.184243402737,0.649784071262686,21.0718246698848));
#37399=CARTESIAN_POINT('Ctrl Pts',(34.0449020201095,0.560228358342142,21.0617979579402));
#37400=CARTESIAN_POINT('Ctrl Pts',(33.9367526065258,0.451020124145838,21.0515429755697));
#37401=CARTESIAN_POINT('Ctrl Pts',(33.8629219949076,0.335314040155129,21.0432678615043));
#37402=CARTESIAN_POINT('Ctrl Pts',(33.8294235159375,0.253405458046626,21.0391731603601));
#37403=CARTESIAN_POINT('Ctrl Pts',(33.8166001713389,0.214743037640408,21.0375777885116));
#37404=CARTESIAN_POINT('Ctrl Pts',(33.8107672719337,0.195270124177129,21.0368442715964));
#37405=CARTESIAN_POINT('Ctrl Pts',(33.8063696108869,0.178945108762379,21.0362872895345));
#37406=CARTESIAN_POINT('Ctrl Pts',(33.8035430565577,0.167477411681154,21.0359271500594));
#37407=CARTESIAN_POINT('Ctrl Pts',(33.8019983561009,0.160921727677303,21.0357299093627));
#37408=CARTESIAN_POINT('Ctrl Pts',(33.7773092196027,0.0524018647745844,
21.0325700014518));
#37409=CARTESIAN_POINT('Ctrl Pts',(33.7772644916236,-0.0636976769205621,
21.0325767026177));
#37410=CARTESIAN_POINT('Ctrl Pts',(33.8104612552768,-0.195461551963477,
21.036817273572));
#37411=CARTESIAN_POINT('Ctrl Pts',(33.8267939783758,-0.247157366383319,
21.0388611305665));
#37412=CARTESIAN_POINT('Ctrl Pts',(33.8527381931904,-0.310276045179468,
21.0420238231594));
#37413=CARTESIAN_POINT('Ctrl Pts',(33.8856128252833,-0.369802952328985,
21.0458136904627));
#37414=CARTESIAN_POINT('Ctrl Pts',(33.9117897291869,-0.408954883478312,
21.0486688126864));
#37415=CARTESIAN_POINT('Ctrl Pts',(33.9275474337088,-0.430510250702555,
21.0503359836173));
#37416=CARTESIAN_POINT('Ctrl Pts',(33.9682959366642,-0.483036633717241,
21.0545570798326));
#37417=CARTESIAN_POINT('Ctrl Pts',(34.044487370967,-0.560024633629738,21.0617422024572));
#37418=CARTESIAN_POINT('Ctrl Pts',(34.2298807119576,-0.679875162841163,
21.075231540361));
#37419=CARTESIAN_POINT('Ctrl Pts',(34.3964044723605,-0.716521316679393,
21.0802569862437));
#37420=CARTESIAN_POINT('Ctrl Pts',(34.5,-0.716521316679393,21.0802569862437));
#37421=CARTESIAN_POINT('Ctrl Pts',(34.5,-0.700000000000003,21.0947273212057));
#37422=CARTESIAN_POINT('Ctrl Pts',(34.601488715903,-0.700000000000003,21.0947273212057));
#37423=CARTESIAN_POINT('Ctrl Pts',(34.7645885272708,-0.663944529159921,
21.0899232558818));
#37424=CARTESIAN_POINT('Ctrl Pts',(34.9457436875169,-0.546389858232665,
21.0770453277506));
#37425=CARTESIAN_POINT('Ctrl Pts',(35.0200341754608,-0.47104574396436,21.0701977474631));
#37426=CARTESIAN_POINT('Ctrl Pts',(35.0597301598872,-0.419704240867174,
21.0661772971794));
#37427=CARTESIAN_POINT('Ctrl Pts',(35.0750763502745,-0.398640101910067,
21.064589691873));
#37428=CARTESIAN_POINT('Ctrl Pts',(35.0932804848699,-0.371325740878547,
21.0626481861578));
#37429=CARTESIAN_POINT('Ctrl Pts',(35.1133479175623,-0.337167414446145,
21.0604294914866));
#37430=CARTESIAN_POINT('Ctrl Pts',(35.1375733098774,-0.290042566100743,
21.0576650892507));
#37431=CARTESIAN_POINT('Ctrl Pts',(35.1577401476323,-0.240779148147267,
21.0552597551832));
#37432=CARTESIAN_POINT('Ctrl Pts',(35.1736033280572,-0.190402020471786,
21.0533174556068));
#37433=CARTESIAN_POINT('Ctrl Pts',(35.2058313314997,-0.0620365235102061,
21.0492885267774));
#37434=CARTESIAN_POINT('Ctrl Pts',(35.2055885298052,0.0578604693840868,
21.0493067818511));
#37435=CARTESIAN_POINT('Ctrl Pts',(35.1766521178085,0.177570048832669,21.0529277392257));
#37436=CARTESIAN_POINT('Ctrl Pts',(35.1670153810713,0.211399604550296,21.0541157584863));
#37437=CARTESIAN_POINT('Ctrl Pts',(35.1470037065095,0.269786333607069,21.0565553991735));
#37438=CARTESIAN_POINT('Ctrl Pts',(35.0614301861815,0.446655796342623,21.0664840198707));
#37439=CARTESIAN_POINT('Ctrl Pts',(34.9288635892265,0.571611206123511,21.0795913995426));
#37440=CARTESIAN_POINT('Ctrl Pts',(34.7825768557976,0.639818872896985,21.0874527336103));
#37441=CARTESIAN_POINT('Ctrl Pts',(34.7495454776053,0.653595643122729,21.0890735928326));
#37442=CARTESIAN_POINT('Ctrl Pts',(34.6905269822415,0.67453112887939,21.0915880263274));
#37443=CARTESIAN_POINT('Ctrl Pts',(34.5675200754451,0.701939348923384,21.0950291806477));
#37444=CARTESIAN_POINT('Ctrl Pts',(34.4497602969485,0.7022365407307,21.0950466519978));
#37445=CARTESIAN_POINT('Ctrl Pts',(34.3098493277581,0.676113885355495,21.0917771417895));
#37446=CARTESIAN_POINT('Ctrl Pts',(34.1907945058791,0.634421036662527,21.0866669491324));
#37447=CARTESIAN_POINT('Ctrl Pts',(34.0546330225508,0.546586440580067,21.0770948442432));
#37448=CARTESIAN_POINT('Ctrl Pts',(33.9491667705954,0.439700516052144,21.0673189941975));
#37449=CARTESIAN_POINT('Ctrl Pts',(33.877315520815,0.326700501273774,21.0594426604343));
#37450=CARTESIAN_POINT('Ctrl Pts',(33.8447603412467,0.246830791412416,21.0555493683631));
#37451=CARTESIAN_POINT('Ctrl Pts',(33.8323022300653,0.209147750594108,21.0540328646905));
#37452=CARTESIAN_POINT('Ctrl Pts',(33.8266365623199,0.190171530481702,21.0533357075259));
#37453=CARTESIAN_POINT('Ctrl Pts',(33.8223655803391,0.174265411004215,21.052806391742));
#37454=CARTESIAN_POINT('Ctrl Pts',(33.8196207576382,0.163093206444423,21.052464169354));
#37455=CARTESIAN_POINT('Ctrl Pts',(33.8181207857797,0.156706768023909,21.0522767472613));
#37456=CARTESIAN_POINT('Ctrl Pts',(33.7941477024817,0.050992199163271,21.0492742528283));
#37457=CARTESIAN_POINT('Ctrl Pts',(33.7941029528339,-0.0619848378266299,
21.0492805571486));
#37458=CARTESIAN_POINT('Ctrl Pts',(33.8263382204678,-0.190356961249475,
21.0533100123713));
#37459=CARTESIAN_POINT('Ctrl Pts',(33.8422041480351,-0.240738386736766,
21.0552526939049));
#37460=CARTESIAN_POINT('Ctrl Pts',(33.8674189004292,-0.302287182003468,
21.0582599134139));
#37461=CARTESIAN_POINT('Ctrl Pts',(33.8993986218151,-0.360388153845254,
21.0618659566443));
#37462=CARTESIAN_POINT('Ctrl Pts',(33.9248830758529,-0.398631712437772,
21.064584145657));
#37463=CARTESIAN_POINT('Ctrl Pts',(33.9402299566535,-0.41969522511451,21.0661718017773));
#37464=CARTESIAN_POINT('Ctrl Pts',(33.9799265447732,-0.471037347443503,
21.070192362136));
#37465=CARTESIAN_POINT('Ctrl Pts',(34.0542283438855,-0.546383580167183,
21.07704147654));
#37466=CARTESIAN_POINT('Ctrl Pts',(34.2353860562437,-0.663939057985833,
21.0899197691134));
#37467=CARTESIAN_POINT('Ctrl Pts',(34.398511284097,-0.700000000000003,21.0947273212057));
#37468=CARTESIAN_POINT('Ctrl Pts',(34.5,-0.700000000000003,21.0947273212057));
#37469=CARTESIAN_POINT('',(34.5,-0.749563950038174,21.0513163163198));
#37470=CARTESIAN_POINT('',(34.5,-0.700000000000003,21.0947273212057));
#37471=CARTESIAN_POINT('',(34.5,-0.749563950038172,21.0513163163198));
#37472=CARTESIAN_POINT('',(33.7998534840905,-5.89111502284859E-5,21.049993682322));
#37473=CARTESIAN_POINT('Ctrl Pts',(34.5,-0.700000000000003,21.0947273212057));
#37474=CARTESIAN_POINT('Ctrl Pts',(34.601488715903,-0.700000000000003,21.0947273212057));
#37475=CARTESIAN_POINT('Ctrl Pts',(34.7645885272708,-0.663944529159921,
21.0899232558818));
#37476=CARTESIAN_POINT('Ctrl Pts',(34.9457436875169,-0.546389858232665,
21.0770453277506));
#37477=CARTESIAN_POINT('Ctrl Pts',(35.0200341754608,-0.47104574396436,21.0701977474631));
#37478=CARTESIAN_POINT('Ctrl Pts',(35.0597301598872,-0.419704240867174,
21.0661772971794));
#37479=CARTESIAN_POINT('Ctrl Pts',(35.0750763502745,-0.398640101910067,
21.064589691873));
#37480=CARTESIAN_POINT('Ctrl Pts',(35.0932804848699,-0.371325740878547,
21.0626481861578));
#37481=CARTESIAN_POINT('Ctrl Pts',(35.1133479175623,-0.337167414446145,
21.0604294914866));
#37482=CARTESIAN_POINT('Ctrl Pts',(35.1375733098774,-0.290042566100743,
21.0576650892507));
#37483=CARTESIAN_POINT('Ctrl Pts',(35.1577401476323,-0.240779148147267,
21.0552597551832));
#37484=CARTESIAN_POINT('Ctrl Pts',(35.1736033280572,-0.190402020471786,
21.0533174556068));
#37485=CARTESIAN_POINT('Ctrl Pts',(35.2058313314997,-0.0620365235102061,
21.0492885267774));
#37486=CARTESIAN_POINT('Ctrl Pts',(35.2055885298052,0.0578604693840868,
21.0493067818511));
#37487=CARTESIAN_POINT('Ctrl Pts',(35.1766521178085,0.177570048832669,21.0529277392257));
#37488=CARTESIAN_POINT('Ctrl Pts',(35.1670153810713,0.211399604550296,21.0541157584863));
#37489=CARTESIAN_POINT('Ctrl Pts',(35.1470037065095,0.269786333607069,21.0565553991735));
#37490=CARTESIAN_POINT('Ctrl Pts',(35.0614301861815,0.446655796342623,21.0664840198707));
#37491=CARTESIAN_POINT('Ctrl Pts',(34.9288635892265,0.571611206123511,21.0795913995426));
#37492=CARTESIAN_POINT('Ctrl Pts',(34.7825768557976,0.639818872896985,21.0874527336103));
#37493=CARTESIAN_POINT('Ctrl Pts',(34.7495454776053,0.653595643122729,21.0890735928326));
#37494=CARTESIAN_POINT('Ctrl Pts',(34.6905269822415,0.67453112887939,21.0915880263274));
#37495=CARTESIAN_POINT('Ctrl Pts',(34.5675200754451,0.701939348923384,21.0950291806477));
#37496=CARTESIAN_POINT('Ctrl Pts',(34.4497602969485,0.7022365407307,21.0950466519978));
#37497=CARTESIAN_POINT('Ctrl Pts',(34.3098493277581,0.676113885355495,21.0917771417895));
#37498=CARTESIAN_POINT('Ctrl Pts',(34.1907945058791,0.634421036662527,21.0866669491324));
#37499=CARTESIAN_POINT('Ctrl Pts',(34.0546330225508,0.546586440580067,21.0770948442432));
#37500=CARTESIAN_POINT('Ctrl Pts',(33.9491667705954,0.439700516052144,21.0673189941975));
#37501=CARTESIAN_POINT('Ctrl Pts',(33.877315520815,0.326700501273774,21.0594426604343));
#37502=CARTESIAN_POINT('Ctrl Pts',(33.8447603412467,0.246830791412416,21.0555493683631));
#37503=CARTESIAN_POINT('Ctrl Pts',(33.8323022300653,0.209147750594108,21.0540328646905));
#37504=CARTESIAN_POINT('Ctrl Pts',(33.8266365623199,0.190171530481702,21.0533357075259));
#37505=CARTESIAN_POINT('Ctrl Pts',(33.8223655803391,0.174265411004215,21.052806391742));
#37506=CARTESIAN_POINT('Ctrl Pts',(33.8196207576382,0.163093206444423,21.052464169354));
#37507=CARTESIAN_POINT('Ctrl Pts',(33.8181207857797,0.156706768023909,21.0522767472613));
#37508=CARTESIAN_POINT('Ctrl Pts',(33.8057710155959,0.102247747701762,21.0507300077049));
#37509=CARTESIAN_POINT('Ctrl Pts',(33.7998596786816,0.0502969342747387,
21.0499923790236));
#37510=CARTESIAN_POINT('Ctrl Pts',(33.7998534840905,-5.89111502284807E-5,
21.049993682322));
#37511=CARTESIAN_POINT('Ctrl Pts',(33.7998534840905,-5.89111502284807E-5,
21.049993682322));
#37512=CARTESIAN_POINT('Ctrl Pts',(33.7998472894994,-0.0504147565751959,
21.0499949856204));
#37513=CARTESIAN_POINT('Ctrl Pts',(33.8069970598875,-0.113333687195768,
21.0508923392377));
#37514=CARTESIAN_POINT('Ctrl Pts',(33.8263382204678,-0.190356961249475,
21.0533100123713));
#37515=CARTESIAN_POINT('Ctrl Pts',(33.8422041480351,-0.240738386736766,
21.0552526939049));
#37516=CARTESIAN_POINT('Ctrl Pts',(33.8674189004292,-0.302287182003468,
21.0582599134139));
#37517=CARTESIAN_POINT('Ctrl Pts',(33.8993986218151,-0.360388153845254,
21.0618659566443));
#37518=CARTESIAN_POINT('Ctrl Pts',(33.9248830758529,-0.398631712437772,
21.064584145657));
#37519=CARTESIAN_POINT('Ctrl Pts',(33.9402299566535,-0.41969522511451,21.0661718017773));
#37520=CARTESIAN_POINT('Ctrl Pts',(33.9799265447732,-0.471037347443503,
21.070192362136));
#37521=CARTESIAN_POINT('Ctrl Pts',(34.0542283438855,-0.546383580167183,
21.07704147654));
#37522=CARTESIAN_POINT('Ctrl Pts',(34.2353860562437,-0.663939057985833,
21.0899197691134));
#37523=CARTESIAN_POINT('Ctrl Pts',(34.398511284097,-0.700000000000003,21.0947273212057));
#37524=CARTESIAN_POINT('Ctrl Pts',(34.5,-0.700000000000003,21.0947273212057));
#37525=CARTESIAN_POINT('Ctrl Pts',(34.5,-0.749563950038174,21.0513163163198));
#37526=CARTESIAN_POINT('Ctrl Pts',(34.3921908488873,-0.749563950038174,
21.0513163163198));
#37527=CARTESIAN_POINT('Ctrl Pts',(34.2188700233853,-0.711747372551822,
21.0458550828561));
#37528=CARTESIAN_POINT('Ctrl Pts',(34.02500542513,-0.587306740554846,21.0311436542917));
#37529=CARTESIAN_POINT('Ctrl Pts',(33.945034720446,-0.507035206264715,21.0232865152258));
#37530=CARTESIAN_POINT('Ctrl Pts',(33.9021823878193,-0.452140301878644,
21.0186643472973));
#37531=CARTESIAN_POINT('Ctrl Pts',(33.8856030358547,-0.42960122555939,21.0168381467451));
#37532=CARTESIAN_POINT('Ctrl Pts',(33.8580412322199,-0.388632549296444,
21.0137091580996));
#37533=CARTESIAN_POINT('Ctrl Pts',(33.8233767787127,-0.326253771531467,
21.0095516426503));
#37534=CARTESIAN_POINT('Ctrl Pts',(33.7959736390573,-0.259995325676423,
21.0060780038898));
#37535=CARTESIAN_POINT('Ctrl Pts',(33.7787073248947,-0.20567073339148,21.0038317959733));
#37536=CARTESIAN_POINT('Ctrl Pts',(33.743587569203,-0.0671233551084263,
20.9991689935559));
#37537=CARTESIAN_POINT('Ctrl Pts',(33.7436322538446,0.0552211959972136,
20.9991614986988));
#37538=CARTESIAN_POINT('Ctrl Pts',(33.7697534967433,0.169351646984093,21.0026362335653));
#37539=CARTESIAN_POINT('Ctrl Pts',(33.7713876543967,0.17624582215462,21.00285311147));
#37540=CARTESIAN_POINT('Ctrl Pts',(33.7743776719825,0.188304504278709,21.0032490851194));
#37541=CARTESIAN_POINT('Ctrl Pts',(33.7790286911615,0.205467311567983,21.0038613997373));
#37542=CARTESIAN_POINT('Ctrl Pts',(33.785196053886,0.225933611733011,21.0046676361538));
#37543=CARTESIAN_POINT('Ctrl Pts',(33.7987498653191,0.266554791315046,21.0064207443541));
#37544=CARTESIAN_POINT('Ctrl Pts',(33.8341349430927,0.352541117917839,21.0109182636443));
#37545=CARTESIAN_POINT('Ctrl Pts',(33.9119242783867,0.473659340333228,21.019990938314));
#37546=CARTESIAN_POINT('Ctrl Pts',(34.0254400152268,0.587512193866294,21.0312041853341));
#37547=CARTESIAN_POINT('Ctrl Pts',(34.1711411964527,0.680510140463003,21.0421401113897));
#37548=CARTESIAN_POINT('Ctrl Pts',(34.2979168099864,0.724426508507403,21.0479597951114));
#37549=CARTESIAN_POINT('Ctrl Pts',(34.4466588488531,0.751912455450576,21.0516805007024));
#37550=CARTESIAN_POINT('Ctrl Pts',(34.5716817460195,0.751594137177719,21.0516605025898));
#37551=CARTESIAN_POINT('Ctrl Pts',(34.702486674947,0.722760619862234,21.0477448745898));
#37552=CARTESIAN_POINT('Ctrl Pts',(34.7653478169603,0.700689089135733,21.0448800812064));
#37553=CARTESIAN_POINT('Ctrl Pts',(34.8005645030701,0.686149513350896,21.043032043578));
#37554=CARTESIAN_POINT('Ctrl Pts',(34.9566260210823,0.614115291433095,21.0340667746151));
#37555=CARTESIAN_POINT('Ctrl Pts',(35.0993946204602,0.481448989298802,21.0190440514598));
#37556=CARTESIAN_POINT('Ctrl Pts',(35.1923007590141,0.291280650338835,21.0075819713019));
#37557=CARTESIAN_POINT('Ctrl Pts',(35.214068499096,0.228356974265122,21.004762450079));
#37558=CARTESIAN_POINT('Ctrl Pts',(35.2245604862986,0.191862595129649,21.0033883099402));
#37559=CARTESIAN_POINT('Ctrl Pts',(35.2560871656414,0.0626491158681729,
20.9991981622569));
#37560=CARTESIAN_POINT('Ctrl Pts',(35.2563431722199,-0.0671819342670894,
20.9991778701227));
#37561=CARTESIAN_POINT('Ctrl Pts',(35.2212309037757,-0.205721880481172,
21.0038401171032));
#37562=CARTESIAN_POINT('Ctrl Pts',(35.2039675401431,-0.260041744395718,
21.0060858902635));
#37563=CARTESIAN_POINT('Ctrl Pts',(35.1820502322802,-0.313074653150546,
21.0088643148667));
#37564=CARTESIAN_POINT('Ctrl Pts',(35.1557767361487,-0.363704460367538,
21.0120527916887));
#37565=CARTESIAN_POINT('Ctrl Pts',(35.1340422591755,-0.400351661687876,
21.0146094007192));
#37566=CARTESIAN_POINT('Ctrl Pts',(35.1143542325059,-0.429612298109788,
21.0168443285933));
#37567=CARTESIAN_POINT('Ctrl Pts',(35.0977756120755,-0.452152037495066,
21.0186704724503));
#37568=CARTESIAN_POINT('Ctrl Pts',(35.0549239124764,-0.507046229905794,
21.0232925177222));
#37569=CARTESIAN_POINT('Ctrl Pts',(34.974965121707,-0.587314921207312,21.0311479468387));
#37570=CARTESIAN_POINT('Ctrl Pts',(34.7811032097204,-0.711754547708119,
21.0458589692126));
#37571=CARTESIAN_POINT('Ctrl Pts',(34.6078091511127,-0.749563950038172,
21.0513163163198));
#37572=CARTESIAN_POINT('Ctrl Pts',(34.5,-0.749563950038172,21.0513163163198));
#37573=CARTESIAN_POINT('Origin',(22.,0.,26.5));
#37574=CARTESIAN_POINT('',(35.75,5.5,26.5));
#37575=CARTESIAN_POINT('',(35.75,-5.5,26.5));
#37576=CARTESIAN_POINT('Origin',(35.75,0.,26.5));
#37577=CARTESIAN_POINT('Origin',(35.75,0.,26.5));
#37578=CARTESIAN_POINT('',(22.,-5.5,26.5));
#37579=CARTESIAN_POINT('',(30.8830878247779,3.69831793009931,22.4290732637163));
#37580=CARTESIAN_POINT('',(17.652334347801,3.69831792998691,22.4290732641403));
#37581=CARTESIAN_POINT('',(22.,3.69831792998691,22.4290732641403));
#37582=CARTESIAN_POINT('',(17.5228104013601,3.65742449835961,22.3922943096177));
#37583=CARTESIAN_POINT('Ctrl Pts',(17.652334347801,3.69831792998691,22.4290732641403));
#37584=CARTESIAN_POINT('Ctrl Pts',(17.6306520542537,3.69154163615065,22.4229171992883));
#37585=CARTESIAN_POINT('Ctrl Pts',(17.6089792165843,3.68473366139296,22.4167631015483));
#37586=CARTESIAN_POINT('Ctrl Pts',(17.5873157886876,3.67789386157419,22.410611298869));
#37587=CARTESIAN_POINT('Ctrl Pts',(17.5658049795975,3.67110224813158,22.4045028356273));
#37588=CARTESIAN_POINT('Ctrl Pts',(17.5443035273164,3.66427928145294,22.3983966577005));
#37589=CARTESIAN_POINT('Ctrl Pts',(17.5228113888221,3.65742482201821,22.3922930879342));
#37590=CARTESIAN_POINT('',(17.5228104013601,-3.65742449835961,22.3922943096177));
#37591=CARTESIAN_POINT('Ctrl Pts',(17.5228104013601,3.65742449835962,22.3922943096177));
#37592=CARTESIAN_POINT('Ctrl Pts',(17.4718155231826,3.61371163342318,22.3533731903452));
#37593=CARTESIAN_POINT('Ctrl Pts',(17.4213621793917,3.56860095253652,22.314462944171));
#37594=CARTESIAN_POINT('Ctrl Pts',(17.1786673062269,3.34189405579382,22.1254229108229));
#37595=CARTESIAN_POINT('Ctrl Pts',(16.9998567608571,3.14235547380069,21.9800060560567));
#37596=CARTESIAN_POINT('Ctrl Pts',(16.7079762629281,2.75740413257784,21.7359762518195));
#37597=CARTESIAN_POINT('Ctrl Pts',(16.5729905746261,2.54826816026991,21.6195359147249));
#37598=CARTESIAN_POINT('Ctrl Pts',(16.333784841218,2.09462553853969,21.4083259944966));
#37599=CARTESIAN_POINT('Ctrl Pts',(16.2295518424091,1.85008857261991,21.3136362055264));
#37600=CARTESIAN_POINT('Ctrl Pts',(16.061681316055,1.33934953012783,21.1589004443208));
#37601=CARTESIAN_POINT('Ctrl Pts',(15.9978650437258,1.07266052861995,21.098765657674));
#37602=CARTESIAN_POINT('Ctrl Pts',(15.9139403163524,0.53468492332373,21.0193025010528));
#37603=CARTESIAN_POINT('Ctrl Pts',(15.8938293331417,0.263394893211526,21.));
#37604=CARTESIAN_POINT('Ctrl Pts',(15.8938293331417,0.,21.));
#37605=CARTESIAN_POINT('Ctrl Pts',(15.8938293331417,-0.263394893211527,
21.));
#37606=CARTESIAN_POINT('Ctrl Pts',(15.9139403163524,-0.534684923323731,
21.0193025010528));
#37607=CARTESIAN_POINT('Ctrl Pts',(15.9978650437258,-1.07266052861995,21.098765657674));
#37608=CARTESIAN_POINT('Ctrl Pts',(16.061681316055,-1.33934953012783,21.1589004443208));
#37609=CARTESIAN_POINT('Ctrl Pts',(16.2295518424091,-1.85008857261992,21.3136362055264));
#37610=CARTESIAN_POINT('Ctrl Pts',(16.333784841218,-2.09462553853969,21.4083259944966));
#37611=CARTESIAN_POINT('Ctrl Pts',(16.5729905746261,-2.5482681602699,21.6195359147249));
#37612=CARTESIAN_POINT('Ctrl Pts',(16.7079762629281,-2.75740413257784,21.7359762518195));
#37613=CARTESIAN_POINT('Ctrl Pts',(16.9998567608571,-3.14235547380069,21.9800060560567));
#37614=CARTESIAN_POINT('Ctrl Pts',(17.1786673062269,-3.34189405579382,22.1254229108229));
#37615=CARTESIAN_POINT('Ctrl Pts',(17.4213621793917,-3.56860095253652,22.314462944171));
#37616=CARTESIAN_POINT('Ctrl Pts',(17.4718155231826,-3.61371163342317,22.3533731903451));
#37617=CARTESIAN_POINT('Ctrl Pts',(17.5228104013601,-3.65742449835961,22.3922943096177));
#37618=CARTESIAN_POINT('',(17.652334347801,-3.69831792998691,22.4290732641403));
#37619=CARTESIAN_POINT('Ctrl Pts',(17.5228110788605,-3.65742469016367,22.3922935859358));
#37620=CARTESIAN_POINT('Ctrl Pts',(17.5443017343427,-3.66427868717436,22.3983965430443));
#37621=CARTESIAN_POINT('Ctrl Pts',(17.5658016777307,-3.67110118593092,22.4045021463312));
#37622=CARTESIAN_POINT('Ctrl Pts',(17.5873109511853,-3.67789232535356,22.4106100751017));
#37623=CARTESIAN_POINT('Ctrl Pts',(17.6089760162179,-3.68473265297072,22.4167622435748));
#37624=CARTESIAN_POINT('Ctrl Pts',(17.6306504666714,-3.69154113998894,22.4229167485399));
#37625=CARTESIAN_POINT('Ctrl Pts',(17.652334347801,-3.69831792998691,22.4290732641403));
#37626=CARTESIAN_POINT('',(30.8830878255874,-3.69831792998913,22.4290732641319));
#37627=CARTESIAN_POINT('',(22.,-3.69831792998691,22.4290732641403));
#37628=CARTESIAN_POINT('',(31.3,-3.55458559184835,22.3029866249648));
#37629=CARTESIAN_POINT('Ctrl Pts',(30.8830878256038,-3.69831792998691,22.4290732641403));
#37630=CARTESIAN_POINT('Ctrl Pts',(30.9233724031233,-3.69831792998691,22.4290732641403));
#37631=CARTESIAN_POINT('Ctrl Pts',(30.9634974147365,-3.69473776211815,22.4258129546819));
#37632=CARTESIAN_POINT('Ctrl Pts',(31.0608268115351,-3.67754139921518,22.4102713040562));
#37633=CARTESIAN_POINT('Ctrl Pts',(31.1158542155423,-3.66015163820752,22.3946036369474));
#37634=CARTESIAN_POINT('Ctrl Pts',(31.2213217785344,-3.61140543651387,22.3516419451064));
#37635=CARTESIAN_POINT('Ctrl Pts',(31.2646787460225,-3.58223402584168,22.3264096749149));
#37636=CARTESIAN_POINT('Ctrl Pts',(31.2994908266689,-3.55498492904841,22.3033248609664));
#37637=CARTESIAN_POINT('Ctrl Pts',(31.2997454942081,-3.55478532723142,22.3031557872837));
#37638=CARTESIAN_POINT('Ctrl Pts',(31.3,-3.55458559184835,22.3029866249648));
#37639=CARTESIAN_POINT('',(31.3,3.55458559184835,22.3029866249648));
#37640=CARTESIAN_POINT('Origin',(31.3,0.,26.5));
#37641=CARTESIAN_POINT('Ctrl Pts',(31.3,3.55458559184835,22.3029866249648));
#37642=CARTESIAN_POINT('Ctrl Pts',(31.2997454945137,3.55478532699163,22.3031557870806));
#37643=CARTESIAN_POINT('Ctrl Pts',(31.2994908263624,3.55498492928751,22.3033248611689));
#37644=CARTESIAN_POINT('Ctrl Pts',(31.266221424283,3.58102649708782,22.3253866840674));
#37645=CARTESIAN_POINT('Ctrl Pts',(31.2312555016837,3.60401240458897,22.3452673820714));
#37646=CARTESIAN_POINT('Ctrl Pts',(31.1529671626145,3.64446341500391,22.3807010381468));
#37647=CARTESIAN_POINT('Ctrl Pts',(31.1107407752369,3.66112199589451,22.3955556214492));
#37648=CARTESIAN_POINT('Ctrl Pts',(31.007251686649,3.68975720344199,22.421254208944));
#37649=CARTESIAN_POINT('Ctrl Pts',(30.9454996143513,3.69831792998691,22.4290732641403));
#37650=CARTESIAN_POINT('Ctrl Pts',(30.8830878256038,3.69831792998691,22.4290732641403));
#37651=CARTESIAN_POINT('Origin',(34.5,0.,20.6));
#37652=CARTESIAN_POINT('',(33.8,-8.57252759403151E-17,21.2));
#37653=CARTESIAN_POINT('',(33.8,-8.57252759403151E-17,20.6));
#37654=CARTESIAN_POINT('Origin',(34.5,0.,21.2));
#37655=CARTESIAN_POINT('Origin',(35.7926776695297,0.,26.5));
#37656=CARTESIAN_POINT('',(35.7926776695297,5.48232233047034,26.5));
#37657=CARTESIAN_POINT('Origin',(10.025,4.525,14.25));
#37658=CARTESIAN_POINT('',(10.05,4.5,8.95830089865303));
#37659=CARTESIAN_POINT('',(10.,4.55,8.96086067249887));
#37660=CARTESIAN_POINT('',(10.025,4.525,8.95958078557592));
#37661=CARTESIAN_POINT('',(10.,4.55,6.2));
#37662=CARTESIAN_POINT('',(10.,4.55,14.25));
#37663=CARTESIAN_POINT('',(10.05,4.5,6.2));
#37664=CARTESIAN_POINT('',(13.65,0.900000000000021,6.2));
#37665=CARTESIAN_POINT('',(10.05,4.5,14.25));
#37666=CARTESIAN_POINT('Origin',(10.,0.,14.5));
#37667=CARTESIAN_POINT('',(10.,7.21647899346606,8.96086067249887));
#37668=CARTESIAN_POINT('',(10.,0.,8.96086067249887));
#37669=CARTESIAN_POINT('',(10.,7.94827338858625,6.2));
#37670=CARTESIAN_POINT('',(10.,6.66129870798463,11.0554044768152));
#37671=CARTESIAN_POINT('',(10.,8.,6.2));
#37672=CARTESIAN_POINT('Origin',(29.2841674687199,4.525,6.98243503368624));
#37673=CARTESIAN_POINT('',(11.2601630224385,4.5,13.9818998597663));
#37674=CARTESIAN_POINT('Origin',(29.2841674687199,4.5,6.98243503368624));
#37675=CARTESIAN_POINT('',(11.2135541721682,4.55,14.));
#37676=CARTESIAN_POINT('',(11.2601630224385,4.5,13.9818998597663));
#37677=CARTESIAN_POINT('Origin',(29.2841674687199,4.55,6.98243503368624));
#37678=CARTESIAN_POINT('Ctrl Pts',(30.9997093954044,-10.0241065289954,4.54380411865086));
#37679=CARTESIAN_POINT('Ctrl Pts',(30.999717504114,-10.0237702568947,4.54398835593614));
#37680=CARTESIAN_POINT('Ctrl Pts',(30.9997551851855,-10.0224440653027,4.54471502897839));
#37681=CARTESIAN_POINT('Ctrl Pts',(30.9998913604463,-10.0153494937356,4.54860165528609));
#37682=CARTESIAN_POINT('Ctrl Pts',(30.999969789191,-10.0087553611579,4.5522132400076));
#37683=CARTESIAN_POINT('Ctrl Pts',(31.0000056927207,-10.001666156019,4.55609602391547));
#37684=CARTESIAN_POINT('Ctrl Pts',(31.,-10.0003364131356,4.55682446904928));
#37685=CARTESIAN_POINT('Ctrl Pts',(31.,-10.,4.55700877125496));
#37686=CARTESIAN_POINT('Ctrl Pts',(30.9987342290661,-10.0081103673502,4.51459940199573));
#37687=CARTESIAN_POINT('Ctrl Pts',(30.9987548546594,-10.0075127982384,4.51492503645021));
#37688=CARTESIAN_POINT('Ctrl Pts',(30.998879062242,-10.0045941559398,4.51651823692996));
#37689=CARTESIAN_POINT('Ctrl Pts',(30.9992674697787,-9.99306598674585,4.522824317168));
#37690=CARTESIAN_POINT('Ctrl Pts',(30.9996846757043,-9.98035171628815,4.52977717483027));
#37691=CARTESIAN_POINT('Ctrl Pts',(30.9999513534079,-9.96882779683825,4.53608128171654));
#37692=CARTESIAN_POINT('Ctrl Pts',(31.,-9.96590392822198,4.53767905786143));
#37693=CARTESIAN_POINT('Ctrl Pts',(31.,-9.96530556667556,4.53800584750331));
#37694=CARTESIAN_POINT('Ctrl Pts',(30.9977590627279,-9.99211420570491,4.4853946853406));
#37695=CARTESIAN_POINT('Ctrl Pts',(30.9978068742384,-9.99125477325143,4.48586153734842));
#37696=CARTESIAN_POINT('Ctrl Pts',(30.9981151602182,-9.98842961893862,4.48739695061579));
#37697=CARTESIAN_POINT('Ctrl Pts',(30.9989671002748,-9.96926330090421,4.49792896802917));
#37698=CARTESIAN_POINT('Ctrl Pts',(30.9997226844942,-9.95345281891056,4.50656389269967));
#37699=CARTESIAN_POINT('Ctrl Pts',(30.9999327268108,-9.93430937953765,4.51701465622552));
#37700=CARTESIAN_POINT('Ctrl Pts',(31.,-9.9314714433084,4.51853364667358));
#37701=CARTESIAN_POINT('Ctrl Pts',(31.,-9.93061113335113,4.51900292375165));
#37702=CARTESIAN_POINT('Ctrl Pts',(30.9967838963896,-9.97611804405966,4.45618996868547));
#37703=CARTESIAN_POINT('Ctrl Pts',(30.9968734777971,-9.97499807737716,4.4567968232885));
#37704=CARTESIAN_POINT('Ctrl Pts',(30.9972889013038,-9.97058210687397,4.45918088219282));
#37705=CARTESIAN_POINT('Ctrl Pts',(30.9987939241305,-9.94698231574099,4.47201457241229));
#37706=CARTESIAN_POINT('Ctrl Pts',(30.9996655003134,-9.92505068401682,4.48403716442464));
#37707=CARTESIAN_POINT('Ctrl Pts',(31.0000630457773,-9.9014713472524,4.4969678159358));
#37708=CARTESIAN_POINT('Ctrl Pts',(31.,-9.89703895839481,4.49938823548573));
#37709=CARTESIAN_POINT('Ctrl Pts',(31.,-9.89591670002669,4.5));
#37710=CARTESIAN_POINT('',(31.,-10.,4.55700877125496));
#37711=CARTESIAN_POINT('',(30.9997093954044,-10.0241065289954,4.54380411865086));
#37712=CARTESIAN_POINT('Ctrl Pts',(31.,-10.,4.55700877125496));
#37713=CARTESIAN_POINT('Ctrl Pts',(31.,-10.0001511977844,4.55692593832657));
#37714=CARTESIAN_POINT('Ctrl Pts',(30.99999997723,-10.0003064755069,4.55684087080203));
#37715=CARTESIAN_POINT('Ctrl Pts',(30.9999998614271,-10.0005264462905,4.55672037207584));
#37716=CARTESIAN_POINT('Ctrl Pts',(30.9999997332039,-10.0007700100071,4.55658694927716));
#37717=CARTESIAN_POINT('Ctrl Pts',(30.9999994933958,-10.0010926664444,4.55641020889953));
#37718=CARTESIAN_POINT('Ctrl Pts',(30.9999988481894,-10.0015177680866,4.55617736226788));
#37719=CARTESIAN_POINT('Ctrl Pts',(30.9999981092284,-10.0020046409568,4.55591068085195));
#37720=CARTESIAN_POINT('Ctrl Pts',(30.9999968155925,-10.0026250944535,4.55557084135448));
#37721=CARTESIAN_POINT('Ctrl Pts',(30.9999943960859,-10.0033478047717,4.55517500045817));
#37722=CARTESIAN_POINT('Ctrl Pts',(30.9999912612891,-10.0042841733556,4.55466213524763));
#37723=CARTESIAN_POINT('Ctrl Pts',(30.9999861247383,-10.0053881015756,4.55405750553938));
#37724=CARTESIAN_POINT('Ctrl Pts',(30.9999787444039,-10.0065200261086,4.55343754627602));
#37725=CARTESIAN_POINT('Ctrl Pts',(30.9999728171858,-10.0074290856682,4.55293965098492));
#37726=CARTESIAN_POINT('Ctrl Pts',(30.9999655114504,-10.0083524798443,4.55243390713277));
#37727=CARTESIAN_POINT('Ctrl Pts',(30.9999573089849,-10.0092401411061,4.55194773309642));
#37728=CARTESIAN_POINT('Ctrl Pts',(30.9999505385552,-10.0099728291229,4.55154643824915));
#37729=CARTESIAN_POINT('Ctrl Pts',(30.9999431979467,-10.0106807421438,4.55115871205554));
#37730=CARTESIAN_POINT('Ctrl Pts',(30.9999353410503,-10.011371619,4.55078031184829));
#37731=CARTESIAN_POINT('Ctrl Pts',(30.9999270910272,-10.0120970644781,4.55038297805887));
#37732=CARTESIAN_POINT('Ctrl Pts',(30.9999182331629,-10.0128091740849,4.54999294271822));
#37733=CARTESIAN_POINT('Ctrl Pts',(30.9999082034238,-10.0135493441069,4.54958752483879));
#37734=CARTESIAN_POINT('Ctrl Pts',(30.9998975941431,-10.0143322828788,4.54915868096885));
#37735=CARTESIAN_POINT('Ctrl Pts',(30.9998856313636,-10.0151465414471,4.54871266747929));
#37736=CARTESIAN_POINT('Ctrl Pts',(30.9998723241665,-10.0159792166846,4.54825654888553));
#37737=CARTESIAN_POINT('Ctrl Pts',(30.9998546050825,-10.017087958249,4.54764920808756));
#37738=CARTESIAN_POINT('Ctrl Pts',(30.9998344176981,-10.0182272517748,4.54702510047069));
#37739=CARTESIAN_POINT('Ctrl Pts',(30.9998142444384,-10.0192737287039,4.5464518136809));
#37740=CARTESIAN_POINT('Ctrl Pts',(30.9997977964192,-10.0201269607973,4.54598439134776));
#37741=CARTESIAN_POINT('Ctrl Pts',(30.9997814904077,-10.0209142598129,4.5455530719156));
#37742=CARTESIAN_POINT('Ctrl Pts',(30.9997672645524,-10.0215735191706,4.54519189035887));
#37743=CARTESIAN_POINT('Ctrl Pts',(30.9997549602234,-10.0221437305145,4.54487949460983));
#37744=CARTESIAN_POINT('Ctrl Pts',(30.9997442695991,-10.0226170579556,4.54462017075191));
#37745=CARTESIAN_POINT('Ctrl Pts',(30.9997357958304,-10.0229856158381,4.54441824588489));
#37746=CARTESIAN_POINT('Ctrl Pts',(30.9997282313378,-10.0233146256855,4.54423798852821));
#37747=CARTESIAN_POINT('Ctrl Pts',(30.9997224473027,-10.0235598209633,4.54410364991749));
#37748=CARTESIAN_POINT('Ctrl Pts',(30.9997178906574,-10.023751612567,4.54399857074021));
#37749=CARTESIAN_POINT('Ctrl Pts',(30.999714655592,-10.0238877781751,4.54392396804753));
#37750=CARTESIAN_POINT('Ctrl Pts',(30.9997120192429,-10.0239977171451,4.54386373465786));
#37751=CARTESIAN_POINT('Ctrl Pts',(30.9997093954044,-10.0241065289954,4.54380411865086));
#37752=CARTESIAN_POINT('',(30.9967838963896,-9.97611804405966,4.45618996868547));
#37753=CARTESIAN_POINT('Ctrl Pts',(30.9967838963896,-9.97611804405966,4.45618996868547));
#37754=CARTESIAN_POINT('Ctrl Pts',(30.9977590627279,-9.99211420570491,4.4853946853406));
#37755=CARTESIAN_POINT('Ctrl Pts',(30.9987342290661,-10.0081103673502,4.51459940199573));
#37756=CARTESIAN_POINT('Ctrl Pts',(30.9997093954044,-10.0241065289954,4.54380411865086));
#37757=CARTESIAN_POINT('',(31.,-9.89591670002669,4.5));
#37758=CARTESIAN_POINT('Ctrl Pts',(30.9967838963896,-9.97611804405966,4.45618996868547));
#37759=CARTESIAN_POINT('Ctrl Pts',(30.9968133695279,-9.9757495643299,4.45638962964291));
#37760=CARTESIAN_POINT('Ctrl Pts',(30.996842996836,-9.97537708361651,4.45659147843499));
#37761=CARTESIAN_POINT('Ctrl Pts',(30.9968795362938,-9.97491323183949,4.45684283454683));
#37762=CARTESIAN_POINT('Ctrl Pts',(30.9969179534944,-9.97442554297466,4.45710710771105));
#37763=CARTESIAN_POINT('Ctrl Pts',(30.9969639966797,-9.9738371180411,4.4574259622937));
#37764=CARTESIAN_POINT('Ctrl Pts',(30.9970209278329,-9.97309735320343,4.45782692293292));
#37765=CARTESIAN_POINT('Ctrl Pts',(30.9970817698807,-9.97230677010212,4.45825542762726));
#37766=CARTESIAN_POINT('Ctrl Pts',(30.9971550088046,-9.97134371278461,4.45877750747389));
#37767=CARTESIAN_POINT('Ctrl Pts',(30.9972398674313,-9.97019833928475,4.45939875359796));
#37768=CARTESIAN_POINT('Ctrl Pts',(30.9973345740799,-9.96892004278472,4.46009209663946));
#37769=CARTESIAN_POINT('Ctrl Pts',(30.997443648044,-9.96741519981467,4.46090867672731));
#37770=CARTESIAN_POINT('Ctrl Pts',(30.9975613300434,-9.96572608185513,4.46182599231399));
#37771=CARTESIAN_POINT('Ctrl Pts',(30.9977185936927,-9.96346883898112,4.46305184161574));
#37772=CARTESIAN_POINT('Ctrl Pts',(30.9978907754155,-9.96088399058384,4.46445683844123));
#37773=CARTESIAN_POINT('Ctrl Pts',(30.9980603292894,-9.95815761335659,4.46594063852779));
#37774=CARTESIAN_POINT('Ctrl Pts',(30.9982118909916,-9.95572054504439,4.4672669854971));
#37775=CARTESIAN_POINT('Ctrl Pts',(30.9983610413697,-9.95317546940992,4.46865353040875));
#37776=CARTESIAN_POINT('Ctrl Pts',(30.9984991867338,-9.95065274965857,4.4700294224399));
#37777=CARTESIAN_POINT('Ctrl Pts',(30.9986110688123,-9.94860963274859,4.47114373895232));
#37778=CARTESIAN_POINT('Ctrl Pts',(30.9987158226638,-9.94658204035722,4.47225058167765));
#37779=CARTESIAN_POINT('Ctrl Pts',(30.9988121054087,-9.94460762878096,4.47332931082265));
#37780=CARTESIAN_POINT('Ctrl Pts',(30.9988996657651,-9.9428120819124,4.47431031638482));
#37781=CARTESIAN_POINT('Ctrl Pts',(30.9989802761463,-9.9410609811228,4.47526781120672));
#37782=CARTESIAN_POINT('Ctrl Pts',(30.9990549592769,-9.9393454541988,4.47620648550759));
#37783=CARTESIAN_POINT('Ctrl Pts',(30.9991510543234,-9.93713807967809,4.47741428102861));
#37784=CARTESIAN_POINT('Ctrl Pts',(30.9992376098028,-9.93498836525396,4.47859157980782));
#37785=CARTESIAN_POINT('Ctrl Pts',(30.9993191787092,-9.93278231342343,4.47980026592178));
#37786=CARTESIAN_POINT('Ctrl Pts',(30.9993838570363,-9.9310330716113,4.48075866783194));
#37787=CARTESIAN_POINT('Ctrl Pts',(30.9994453083827,-9.92924717485037,4.48173748465682));
#37788=CARTESIAN_POINT('Ctrl Pts',(30.9995031846701,-9.92741489589081,4.48274188966046));
#37789=CARTESIAN_POINT('Ctrl Pts',(30.9995676886674,-9.92537279328657,4.48386131422348));
#37790=CARTESIAN_POINT('Ctrl Pts',(30.9996276231467,-9.92327363571715,4.4850122227893));
#37791=CARTESIAN_POINT('Ctrl Pts',(30.9996811029328,-9.92115993228124,4.48617116978916));
#37792=CARTESIAN_POINT('Ctrl Pts',(30.9997557460711,-9.91820978103073,4.4877887424736));
#37793=CARTESIAN_POINT('Ctrl Pts',(30.9998173334517,-9.91523262517508,4.48942124714919));
#37794=CARTESIAN_POINT('Ctrl Pts',(30.9998635065226,-9.91244178079622,4.49095138375327));
#37795=CARTESIAN_POINT('Ctrl Pts',(30.9999017819863,-9.91012829242206,4.49221980031967));
#37796=CARTESIAN_POINT('Ctrl Pts',(30.999929592725,-9.90794763352294,4.49341523424628));
#37797=CARTESIAN_POINT('Ctrl Pts',(30.9999490870108,-9.90601712246641,4.49447322866645));
#37798=CARTESIAN_POINT('Ctrl Pts',(30.999964960073,-9.90444521968738,4.49533469193735));
#37799=CARTESIAN_POINT('Ctrl Pts',(30.9999754346307,-9.90303987951068,4.49610464213462));
#37800=CARTESIAN_POINT('Ctrl Pts',(30.9999825498663,-9.90183534326441,4.49676429672001));
#37801=CARTESIAN_POINT('Ctrl Pts',(30.9999891823826,-9.90071252641856,4.49737919833315));
#37802=CARTESIAN_POINT('Ctrl Pts',(30.9999929401154,-9.89976477990244,4.4978979409434));
#37803=CARTESIAN_POINT('Ctrl Pts',(30.9999953264449,-9.89898318387141,4.49832545193876));
#37804=CARTESIAN_POINT('Ctrl Pts',(30.9999975693351,-9.89824856861423,4.49872726577523));
#37805=CARTESIAN_POINT('Ctrl Pts',(30.9999986085518,-9.89766105451709,4.4990483091807));
#37806=CARTESIAN_POINT('Ctrl Pts',(30.9999992167745,-9.89717349943034,4.49931448218875));
#37807=CARTESIAN_POINT('Ctrl Pts',(30.9999998249972,-9.89668594434359,4.49958065519681));
#37808=CARTESIAN_POINT('Ctrl Pts',(31.,-9.89629902896181,4.49979158518045));
#37809=CARTESIAN_POINT('Ctrl Pts',(31.,-9.89591670002669,4.5));
#37810=CARTESIAN_POINT('',(31.,-9.94795835001334,4.52850438562748));
#37811=CARTESIAN_POINT('Ctrl Pts',(30.9967839065843,9.97611791660417,4.45619003774767));
#37812=CARTESIAN_POINT('Ctrl Pts',(30.996873500376,9.97499779333315,4.45679697722312));
#37813=CARTESIAN_POINT('Ctrl Pts',(30.9972889684913,9.97058139404403,4.45918135074556));
#37814=CARTESIAN_POINT('Ctrl Pts',(30.9987938829419,9.94698237497655,4.47201437960008));
#37815=CARTESIAN_POINT('Ctrl Pts',(30.9996653875363,9.92505089721926,4.48403521866371));
#37816=CARTESIAN_POINT('Ctrl Pts',(31.0000630537281,9.90147103509372,4.49696656564785));
#37817=CARTESIAN_POINT('Ctrl Pts',(31.,9.89703887496921,4.49938794717922));
#37818=CARTESIAN_POINT('Ctrl Pts',(31.,9.89591670002669,4.5));
#37819=CARTESIAN_POINT('Ctrl Pts',(30.9977590705465,9.99211407834309,4.4853947546077));
#37820=CARTESIAN_POINT('Ctrl Pts',(30.9978068875849,9.99125454012803,4.48586166403795));
#37821=CARTESIAN_POINT('Ctrl Pts',(30.998073130725,9.98842907687459,4.48738248206113));
#37822=CARTESIAN_POINT('Ctrl Pts',(30.999321036897,9.96926357875824,4.49779643372825));
#37823=CARTESIAN_POINT('Ctrl Pts',(30.9998925790727,9.95345321712367,4.506474317633));
#37824=CARTESIAN_POINT('Ctrl Pts',(31.000104853691,9.93430916936581,4.51698220500682));
#37825=CARTESIAN_POINT('Ctrl Pts',(31.,9.93147138540036,4.51853345740689));
#37826=CARTESIAN_POINT('Ctrl Pts',(31.,9.93061113335113,4.51900292375165));
#37827=CARTESIAN_POINT('Ctrl Pts',(30.9987342345088,10.008110240082,4.51459947146774));
#37828=CARTESIAN_POINT('Ctrl Pts',(30.9987548614373,10.0075126162853,4.51492513567012));
#37829=CARTESIAN_POINT('Ctrl Pts',(30.9989180237843,10.0045936571128,4.51651835890182));
#37830=CARTESIAN_POINT('Ctrl Pts',(30.9993345094708,9.9930603747469,4.52282419804882));
#37831=CARTESIAN_POINT('Ctrl Pts',(30.9997836591977,9.98034689548292,4.5297768367585));
#37832=CARTESIAN_POINT('Ctrl Pts',(30.9999536037935,9.96882556865815,4.53608101051986));
#37833=CARTESIAN_POINT('Ctrl Pts',(31.,9.96590389583151,4.53767896763457));
#37834=CARTESIAN_POINT('Ctrl Pts',(31.,9.96530556667556,4.5380058475033));
#37835=CARTESIAN_POINT('Ctrl Pts',(30.999709398471,10.0241064018209,4.54380418832777));
#37836=CARTESIAN_POINT('Ctrl Pts',(30.9997175072273,10.0237701260067,4.54398842764829));
#37837=CARTESIAN_POINT('Ctrl Pts',(30.9997551883338,10.0224439201123,4.54471510649137));
#37838=CARTESIAN_POINT('Ctrl Pts',(30.9998913599888,10.0153494914902,4.54860164074375));
#37839=CARTESIAN_POINT('Ctrl Pts',(30.9999697880435,10.0087555013957,4.55221317457904));
#37840=CARTESIAN_POINT('Ctrl Pts',(31.0000056930925,10.0016661430369,4.55609605212253));
#37841=CARTESIAN_POINT('Ctrl Pts',(31.,10.0003364062627,4.55682447786224));
#37842=CARTESIAN_POINT('Ctrl Pts',(31.,10.,4.55700877125496));
#37843=CARTESIAN_POINT('',(31.,9.89591670002669,4.5));
#37844=CARTESIAN_POINT('',(30.9967839065843,9.97611791660417,4.45619003774767));
#37845=CARTESIAN_POINT('Ctrl Pts',(31.,9.89591670002669,4.5));
#37846=CARTESIAN_POINT('Ctrl Pts',(31.,9.8962858594512,4.49979865432873));
#37847=CARTESIAN_POINT('Ctrl Pts',(30.9999998340188,9.89665901681545,4.49959511613558));
#37848=CARTESIAN_POINT('Ctrl Pts',(30.9999992772054,9.89712348211803,4.49934145900802));
#37849=CARTESIAN_POINT('Ctrl Pts',(30.9999986917831,9.89761181151393,4.49907476905039));
#37850=CARTESIAN_POINT('Ctrl Pts',(30.9999976809336,9.89820080553401,4.49875282346015));
#37851=CARTESIAN_POINT('Ctrl Pts',(30.9999954505896,9.89894103516699,4.4983478421473));
#37852=CARTESIAN_POINT('Ctrl Pts',(30.9999930670703,9.89973210217239,4.49791504759257));
#37853=CARTESIAN_POINT('Ctrl Pts',(30.9999892819254,9.90069551898937,4.49738762293931));
#37854=CARTESIAN_POINT('Ctrl Pts',(30.9999825049737,9.90184112663191,4.49676013739004));
#37855=CARTESIAN_POINT('Ctrl Pts',(30.999974941968,9.90311961249728,4.49605987023428));
#37856=CARTESIAN_POINT('Ctrl Pts',(30.9999635890354,9.90462446354965,4.49523527848236));
#37857=CARTESIAN_POINT('Ctrl Pts',(30.9999460260694,9.90631345761313,4.49430953032038));
#37858=CARTESIAN_POINT('Ctrl Pts',(30.9999225661086,9.90856955346075,4.49307295013971));
#37859=CARTESIAN_POINT('Ctrl Pts',(30.9998876845076,9.91115273554961,4.4916566847344));
#37860=CARTESIAN_POINT('Ctrl Pts',(30.9998386709666,9.91387735661048,4.49016275480571));
#37861=CARTESIAN_POINT('Ctrl Pts',(30.9997948164941,9.91631518943797,4.4888260729917));
#37862=CARTESIAN_POINT('Ctrl Pts',(30.9997397438994,9.91886117398248,4.48743000956264));
#37863=CARTESIAN_POINT('Ctrl Pts',(30.9996753159154,9.92138482445032,4.48604632553787));
#37864=CARTESIAN_POINT('Ctrl Pts',(30.9996231515921,9.9234281061253,4.48492602134052));
#37865=CARTESIAN_POINT('Ctrl Pts',(30.9995650155982,9.9254558861659,4.48381430249766));
#37866=CARTESIAN_POINT('Ctrl Pts',(30.9995026119473,9.9274304796577,4.48273195330263));
#37867=CARTESIAN_POINT('Ctrl Pts',(30.9994458642117,9.92922610712186,4.48174770213982));
#37868=CARTESIAN_POINT('Ctrl Pts',(30.9993856809681,9.93097728810924,4.48078798814601));
#37869=CARTESIAN_POINT('Ctrl Pts',(30.9993224038945,9.93269285298828,4.47984811356608));
#37870=CARTESIAN_POINT('Ctrl Pts',(30.9992409740201,9.93490057569886,4.47863860964085));
#37871=CARTESIAN_POINT('Ctrl Pts',(30.9991545968578,9.93705051945132,4.47746129227476));
#37872=CARTESIAN_POINT('Ctrl Pts',(30.9990587546962,9.93925671489986,4.47625423743952));
#37873=CARTESIAN_POINT('Ctrl Pts',(30.9989827667415,9.94100588537807,4.47529723035079));
#37874=CARTESIAN_POINT('Ctrl Pts',(30.9989006378005,9.94279166942895,4.47432085377575));
#37875=CARTESIAN_POINT('Ctrl Pts',(30.998811268279,9.94462383248334,4.47331993348054));
#37876=CARTESIAN_POINT('Ctrl Pts',(30.9987116713683,9.94666566707282,4.47220446852495));
#37877=CARTESIAN_POINT('Ctrl Pts',(30.9986029986771,9.9487645445695,4.47105883546725));
#37878=CARTESIAN_POINT('Ctrl Pts',(30.9984867998044,9.95087798782649,4.46990630726323));
#37879=CARTESIAN_POINT('Ctrl Pts',(30.9983246182708,9.95382777090777,4.46829769620369));
#37880=CARTESIAN_POINT('Ctrl Pts',(30.9981474066052,9.95680460084669,4.46667643445956));
#37881=CARTESIAN_POINT('Ctrl Pts',(30.9979698970121,9.95959518572774,4.4651583514365));
#37882=CARTESIAN_POINT('Ctrl Pts',(30.997822707114,9.96190912210162,4.46389956602938));
#37883=CARTESIAN_POINT('Ctrl Pts',(30.9976758219154,9.96409019555147,4.46271431184688));
#37884=CARTESIAN_POINT('Ctrl Pts',(30.9975407431566,9.96602096117105,4.46166586166561));
#37885=CARTESIAN_POINT('Ctrl Pts',(30.9974307583231,9.96759304354012,4.46081218474691));
#37886=CARTESIAN_POINT('Ctrl Pts',(30.9973287715482,9.96899846147698,4.46004957610609));
#37887=CARTESIAN_POINT('Ctrl Pts',(30.9972395295677,9.97020292453311,4.45939628019056));
#37888=CARTESIAN_POINT('Ctrl Pts',(30.997156345061,9.9713256323057,4.45878732801188));
#37889=CARTESIAN_POINT('Ctrl Pts',(30.9970843243445,9.97227315069866,4.45827366363859));
#37890=CARTESIAN_POINT('Ctrl Pts',(30.9970242344315,9.97305438911936,4.45785021755219));
#37891=CARTESIAN_POINT('Ctrl Pts',(30.9969677512095,9.9737887363813,4.4574521873659));
#37892=CARTESIAN_POINT('Ctrl Pts',(30.9969218432233,9.97437583963493,4.45713404448338));
#37893=CARTESIAN_POINT('Ctrl Pts',(30.996883501682,9.9748628795096,4.45687012138836));
#37894=CARTESIAN_POINT('Ctrl Pts',(30.9968451601406,9.97534991938426,4.45660619829334));
#37895=CARTESIAN_POINT('Ctrl Pts',(30.9968144373045,9.97573621414996,4.45639686345456));
#37896=CARTESIAN_POINT('Ctrl Pts',(30.9967839065843,9.97611791660417,4.45619003774767));
#37897=CARTESIAN_POINT('',(30.999709398471,10.0241064018209,4.54380418832777));
#37898=CARTESIAN_POINT('Ctrl Pts',(30.999709398471,10.0241064018209,4.54380418832777));
#37899=CARTESIAN_POINT('Ctrl Pts',(30.9987342345088,10.008110240082,4.51459947146774));
#37900=CARTESIAN_POINT('Ctrl Pts',(30.9977590705465,9.99211407834309,4.4853947546077));
#37901=CARTESIAN_POINT('Ctrl Pts',(30.9967839065843,9.97611791660417,4.45619003774767));
#37902=CARTESIAN_POINT('',(31.,10.,4.55700877125496));
#37903=CARTESIAN_POINT('Ctrl Pts',(30.999709398471,10.0241064018209,4.54380418832777));
#37904=CARTESIAN_POINT('Ctrl Pts',(30.9997130428061,10.0239552686882,4.54388699138558));
#37905=CARTESIAN_POINT('Ctrl Pts',(30.9997167627365,10.023800056336,4.5439720292231));
#37906=CARTESIAN_POINT('Ctrl Pts',(30.9997219491925,10.0235801675738,4.54409250214455));
#37907=CARTESIAN_POINT('Ctrl Pts',(30.9997276919049,10.0233366953556,4.54422589599848));
#37908=CARTESIAN_POINT('Ctrl Pts',(30.999735229715,10.0230141512577,4.54440261195368));
#37909=CARTESIAN_POINT('Ctrl Pts',(30.9997448318797,10.022589181701,4.54463544076275));
#37910=CARTESIAN_POINT('Ctrl Pts',(30.9997558292583,10.0221024632103,4.54490210006752));
#37911=CARTESIAN_POINT('Ctrl Pts',(30.999769492307,10.0214821908588,4.54524192519073));
#37912=CARTESIAN_POINT('Ctrl Pts',(30.9997844949796,10.0207596627717,4.54563775929827));
#37913=CARTESIAN_POINT('Ctrl Pts',(30.9998039339552,10.019823482515,4.54615064188795));
#37914=CARTESIAN_POINT('Ctrl Pts',(30.9998254114386,10.0187197227466,4.54675531137161));
#37915=CARTESIAN_POINT('Ctrl Pts',(30.9998453206045,10.0175879181613,4.54737531334839));
#37916=CARTESIAN_POINT('Ctrl Pts',(30.9998613095551,10.0166789716193,4.54787323380225));
#37917=CARTESIAN_POINT('Ctrl Pts',(30.9998762659289,10.0157556608402,4.54837900388194));
#37918=CARTESIAN_POINT('Ctrl Pts',(30.9998894643458,10.0148680560327,4.54886519675767));
#37919=CARTESIAN_POINT('Ctrl Pts',(30.9999003583534,10.0141354247211,4.54926650161903));
#37920=CARTESIAN_POINT('Ctrl Pts',(30.999910085082,10.0134275501846,4.54965423314624));
#37921=CARTESIAN_POINT('Ctrl Pts',(30.9999188849585,10.0127366990778,4.55003263098948));
#37922=CARTESIAN_POINT('Ctrl Pts',(30.9999281253946,10.0120112609951,4.55042997305517));
#37923=CARTESIAN_POINT('Ctrl Pts',(30.9999364365931,10.0112991469223,4.55082000725131));
#37924=CARTESIAN_POINT('Ctrl Pts',(30.9999442526988,10.0105589532913,4.5512254177633));
#37925=CARTESIAN_POINT('Ctrl Pts',(30.999952520276,10.0097760048231,4.55165424547276));
#37926=CARTESIAN_POINT('Ctrl Pts',(30.9999601897866,10.0089617150539,4.55210023538587));
#37927=CARTESIAN_POINT('Ctrl Pts',(30.9999669593025,10.0081289792326,4.55255632838156));
#37928=CARTESIAN_POINT('Ctrl Pts',(30.999975972948,10.0070201871626,4.55316361857347));
#37929=CARTESIAN_POINT('Ctrl Pts',(30.9999832557419,10.0058807899388,4.55378767133347));
#37930=CARTESIAN_POINT('Ctrl Pts',(30.9999883153679,10.0048341625656,4.55436091900646));
#37931=CARTESIAN_POINT('Ctrl Pts',(30.9999924409198,10.0039807564914,4.55482833755362));
#37932=CARTESIAN_POINT('Ctrl Pts',(30.9999951189592,10.0031932621774,4.55525965958809));
#37933=CARTESIAN_POINT('Ctrl Pts',(30.9999967898708,10.0025338208551,4.55562085125733));
#37934=CARTESIAN_POINT('Ctrl Pts',(30.9999982350687,10.0019634595778,4.55593325167095));
#37935=CARTESIAN_POINT('Ctrl Pts',(30.9999989579243,10.0014899908439,4.55619258717302));
#37936=CARTESIAN_POINT('Ctrl Pts',(30.9999993713266,10.0011213146157,4.55639453011206));
#37937=CARTESIAN_POINT('Ctrl Pts',(30.9999997403671,10.0007922006482,4.55657480276531));
#37938=CARTESIAN_POINT('Ctrl Pts',(30.9999998688457,10.0005469190199,4.55670916222024));
#37939=CARTESIAN_POINT('Ctrl Pts',(30.999999936968,10.0003550550437,4.55681426554227));
#37940=CARTESIAN_POINT('Ctrl Pts',(30.9999999853322,10.0002188389849,4.55688888486672));
#37941=CARTESIAN_POINT('Ctrl Pts',(31.,10.0001088559445,4.55694913671912));
#37942=CARTESIAN_POINT('Ctrl Pts',(31.,10.,4.55700877125496));
#37943=CARTESIAN_POINT('',(31.,9.94795835001335,4.52850438562748));
#37944=CARTESIAN_POINT('Ctrl Pts',(30.7,10.6423370590817,4.2));
#37945=CARTESIAN_POINT('Ctrl Pts',(30.7965969380826,10.5378992444231,4.19999999999999));
#37946=CARTESIAN_POINT('Ctrl Pts',(30.9345468167719,10.3169335076792,4.27686267954766));
#37947=CARTESIAN_POINT('Ctrl Pts',(30.9889170802925,10.0744708831481,4.40289742302579));
#37948=CARTESIAN_POINT('Ctrl Pts',(30.9967839065843,9.97611791660417,4.45619003774767));
#37949=CARTESIAN_POINT('Ctrl Pts',(30.7112855175711,10.6546595286708,4.21735899290232));
#37950=CARTESIAN_POINT('Ctrl Pts',(30.806790559886,10.5514291562489,4.22117275213537));
#37951=CARTESIAN_POINT('Ctrl Pts',(30.9417901498282,10.332363796979,4.30380302692461));
#37952=CARTESIAN_POINT('Ctrl Pts',(30.9917239673576,10.0904674824508,4.4319041792042));
#37953=CARTESIAN_POINT('Ctrl Pts',(30.9977590705465,9.99211407834309,4.4853947546077));
#37954=CARTESIAN_POINT('Ctrl Pts',(30.7225710351422,10.66698199826,4.23471798580464));
#37955=CARTESIAN_POINT('Ctrl Pts',(30.8169841816893,10.5649590680747,4.24234550427075));
#37956=CARTESIAN_POINT('Ctrl Pts',(30.9490334828845,10.3477940862788,4.33074337430155));
#37957=CARTESIAN_POINT('Ctrl Pts',(30.9945308544227,10.1064640817536,4.46091093538261));
#37958=CARTESIAN_POINT('Ctrl Pts',(30.9987342345088,10.008110240082,4.51459947146774));
#37959=CARTESIAN_POINT('Ctrl Pts',(30.7338565527132,10.6793044678492,4.25207697870696));
#37960=CARTESIAN_POINT('Ctrl Pts',(30.8271778034927,10.5784889799005,4.26351825640613));
#37961=CARTESIAN_POINT('Ctrl Pts',(30.9562768159408,10.3632243755785,4.3576837216785));
#37962=CARTESIAN_POINT('Ctrl Pts',(30.9973377414878,10.1224606810563,4.48991769156102));
#37963=CARTESIAN_POINT('Ctrl Pts',(30.999709398471,10.0241064018209,4.54380418832777));
#37964=CARTESIAN_POINT('Ctrl Pts',(30.9967839065843,9.97611791660417,4.45619003774767));
#37965=CARTESIAN_POINT('Ctrl Pts',(30.9889170802925,10.0744708831481,4.40289742302579));
#37966=CARTESIAN_POINT('Ctrl Pts',(30.9345468167719,10.3169335076792,4.27686267954766));
#37967=CARTESIAN_POINT('Ctrl Pts',(30.7965969380826,10.5378992444231,4.19999999999999));
#37968=CARTESIAN_POINT('Ctrl Pts',(30.7,10.6423370590817,4.2));
#37969=CARTESIAN_POINT('',(30.7338565527132,10.6793044678492,4.25207697870696));
#37970=CARTESIAN_POINT('',(30.7,10.6423370590817,4.2));
#37971=CARTESIAN_POINT('Ctrl Pts',(30.7338565527132,10.6793044678492,4.25207697870696));
#37972=CARTESIAN_POINT('Ctrl Pts',(30.8271778034927,10.5784889799005,4.26351825640613));
#37973=CARTESIAN_POINT('Ctrl Pts',(30.9562768159408,10.3632243755785,4.3576837216785));
#37974=CARTESIAN_POINT('Ctrl Pts',(30.9973377414878,10.1224606810563,4.48991769156102));
#37975=CARTESIAN_POINT('Ctrl Pts',(30.999709398471,10.0241064018209,4.54380418832777));
#37976=CARTESIAN_POINT('Origin',(15.,-10.975,4.225));
#37977=CARTESIAN_POINT('',(30.,-11.,4.25));
#37978=CARTESIAN_POINT('',(30.,-10.95,4.2));
#37979=CARTESIAN_POINT('',(21.05,-11.,4.25));
#37980=CARTESIAN_POINT('',(15.,-11.,4.25));
#37981=CARTESIAN_POINT('',(21.05,-11.,4.25));
#37982=CARTESIAN_POINT('Origin',(21.025,-10.975,4.2));
#37983=CARTESIAN_POINT('',(21.05,-11.,4.85));
#37984=CARTESIAN_POINT('',(21.05,-11.,4.2));
#37985=CARTESIAN_POINT('',(21.,-10.95,4.8));
#37986=CARTESIAN_POINT('',(21.05,-11.,4.85));
#37987=CARTESIAN_POINT('',(21.,-10.95,4.2));
#37988=CARTESIAN_POINT('Origin',(18.95,-11.,4.25));
#37989=CARTESIAN_POINT('',(19.,-10.95,4.25));
#37990=CARTESIAN_POINT('',(18.95,-10.95,4.2));
#37991=CARTESIAN_POINT('',(19.,-10.95,4.25));
#37992=CARTESIAN_POINT('',(18.95,-11.,4.25));
#37993=CARTESIAN_POINT('',(18.95,-11.,4.25));
#37994=CARTESIAN_POINT('',(18.95,-10.95,4.2));
#37995=CARTESIAN_POINT('Origin',(18.975,-10.975,4.2));
#37996=CARTESIAN_POINT('',(18.95,-11.,4.85));
#37997=CARTESIAN_POINT('',(18.95,-11.,4.2));
#37998=CARTESIAN_POINT('',(19.,-10.95,4.8));
#37999=CARTESIAN_POINT('',(19.,-10.95,4.2));
#38000=CARTESIAN_POINT('',(19.,-10.95,4.8));
#38001=CARTESIAN_POINT('Origin',(18.95,11.,4.25));
#38002=CARTESIAN_POINT('',(18.95,10.95,4.2));
#38003=CARTESIAN_POINT('',(19.,10.95,4.25));
#38004=CARTESIAN_POINT('',(18.95,10.95,4.2));
#38005=CARTESIAN_POINT('',(18.95,11.,4.25));
#38006=CARTESIAN_POINT('',(18.95,11.,4.25));
#38007=CARTESIAN_POINT('',(19.,10.95,4.25));
#38008=CARTESIAN_POINT('Origin',(25.,10.975,4.225));
#38009=CARTESIAN_POINT('',(10.,10.95,4.2));
#38010=CARTESIAN_POINT('',(10.,11.,4.25));
#38011=CARTESIAN_POINT('',(10.,10.95,4.2));
#38012=CARTESIAN_POINT('',(25.,11.,4.25));
#38013=CARTESIAN_POINT('',(25.,10.95,4.2));
#38014=CARTESIAN_POINT('Origin',(10.,10.,4.225));
#38015=CARTESIAN_POINT('',(9.05,10.,4.2));
#38016=CARTESIAN_POINT('',(9.,10.,4.25));
#38017=CARTESIAN_POINT('',(9.05,10.,4.2));
#38018=CARTESIAN_POINT('Origin',(10.,10.,4.25));
#38019=CARTESIAN_POINT('Origin',(10.,10.,4.2));
#38020=CARTESIAN_POINT('Origin',(9.025,5.,4.225));
#38021=CARTESIAN_POINT('',(9.05,-10.,4.2));
#38022=CARTESIAN_POINT('',(9.,-10.,4.25));
#38023=CARTESIAN_POINT('',(9.05,-10.,4.2));
#38024=CARTESIAN_POINT('',(9.,5.,4.25));
#38025=CARTESIAN_POINT('',(9.05,5.,4.2));
#38026=CARTESIAN_POINT('Origin',(10.,-10.,4.225));
#38027=CARTESIAN_POINT('',(10.,-10.95,4.2));
#38028=CARTESIAN_POINT('',(10.,-11.,4.25));
#38029=CARTESIAN_POINT('',(10.,-10.95,4.2));
#38030=CARTESIAN_POINT('Origin',(10.,-10.,4.25));
#38031=CARTESIAN_POINT('Origin',(10.,-10.,4.2));
#38032=CARTESIAN_POINT('Origin',(15.,-10.975,4.225));
#38033=CARTESIAN_POINT('',(15.,-10.95,4.2));
#38034=CARTESIAN_POINT('',(15.,-11.,4.25));
#38035=CARTESIAN_POINT('Origin',(18.975,10.975,4.2));
#38036=CARTESIAN_POINT('',(19.,10.95,4.8));
#38037=CARTESIAN_POINT('',(19.,10.95,4.2));
#38038=CARTESIAN_POINT('',(18.95,11.,4.85));
#38039=CARTESIAN_POINT('',(18.95,11.,4.2));
#38040=CARTESIAN_POINT('',(18.95,11.,4.85));
#38041=CARTESIAN_POINT('Origin',(18.975,5.55,4.225));
#38042=CARTESIAN_POINT('',(18.95,5.55,4.2));
#38043=CARTESIAN_POINT('',(19.,5.55,4.25));
#38044=CARTESIAN_POINT('Origin',(25.,10.975,4.825));
#38045=CARTESIAN_POINT('',(25.,10.95,4.8));
#38046=CARTESIAN_POINT('',(25.,11.,4.85));
#38047=CARTESIAN_POINT('Origin',(15.,-10.975,4.825));
#38048=CARTESIAN_POINT('',(15.,-11.,4.85));
#38049=CARTESIAN_POINT('',(15.,-10.95,4.8));
#38050=CARTESIAN_POINT('Origin',(30.,10.,4.225));
#38051=CARTESIAN_POINT('',(30.7,10.7141428428543,4.25));
#38052=CARTESIAN_POINT('Origin',(30.,10.,4.25));
#38053=CARTESIAN_POINT('',(30.7,10.7141428428543,4.25));
#38054=CARTESIAN_POINT('Origin',(30.,-10.,4.225));
#38055=CARTESIAN_POINT('',(30.7,-10.7141428428543,4.25));
#38056=CARTESIAN_POINT('',(30.665,-10.6784357007116,4.2));
#38057=CARTESIAN_POINT('Origin',(30.,-10.,4.25));
#38058=CARTESIAN_POINT('Ctrl Pts',(30.7338565527132,10.6793044678492,4.25207697870696));
#38059=CARTESIAN_POINT('Ctrl Pts',(30.7228338070625,10.6912124038448,4.25072557918173));
#38060=CARTESIAN_POINT('Ctrl Pts',(30.7115415847052,10.7028298270137,4.25));
#38061=CARTESIAN_POINT('Ctrl Pts',(30.7,10.7141428428543,4.25));
#38062=CARTESIAN_POINT('Ctrl Pts',(30.7225710351422,10.66698199826,4.23471798580464));
#38063=CARTESIAN_POINT('Ctrl Pts',(30.7114193189812,10.6790325526684,4.23381705278782));
#38064=CARTESIAN_POINT('Ctrl Pts',(30.7000220784993,10.6907832001958,4.23333333333333));
#38065=CARTESIAN_POINT('Ctrl Pts',(30.6883333333333,10.70224046214,4.23333333333333));
#38066=CARTESIAN_POINT('Ctrl Pts',(30.7112855175711,10.6546595286708,4.21735899290232));
#38067=CARTESIAN_POINT('Ctrl Pts',(30.7000048309,10.666852701492,4.21690852639391));
#38068=CARTESIAN_POINT('Ctrl Pts',(30.6885025722933,10.678736573378,4.21666666666667));
#38069=CARTESIAN_POINT('Ctrl Pts',(30.6766666666667,10.6903380814258,4.21666666666667));
#38070=CARTESIAN_POINT('Ctrl Pts',(30.7,10.6423370590817,4.2));
#38071=CARTESIAN_POINT('Ctrl Pts',(30.6885903428187,10.6546728503156,4.2));
#38072=CARTESIAN_POINT('Ctrl Pts',(30.6769830660874,10.6666899465601,4.2));
#38073=CARTESIAN_POINT('Ctrl Pts',(30.665,10.6784357007116,4.2));
#38074=CARTESIAN_POINT('Ctrl Pts',(30.7,10.7141428428543,4.25));
#38075=CARTESIAN_POINT('Ctrl Pts',(30.7115415847052,10.7028298270137,4.25));
#38076=CARTESIAN_POINT('Ctrl Pts',(30.7228338070625,10.6912124038448,4.25072557918173));
#38077=CARTESIAN_POINT('Ctrl Pts',(30.7338565527132,10.6793044678492,4.25207697870696));
#38078=CARTESIAN_POINT('Ctrl Pts',(30.9967838963896,-9.97611804405966,4.45618996868547));
#38079=CARTESIAN_POINT('Ctrl Pts',(30.9889170789375,-10.0744707456924,4.40289749968711));
#38080=CARTESIAN_POINT('Ctrl Pts',(30.9345467803032,-10.3169335644504,4.27686265785453));
#38081=CARTESIAN_POINT('Ctrl Pts',(30.7965969202196,-10.5378992637361,4.19999999999999));
#38082=CARTESIAN_POINT('Ctrl Pts',(30.7,-10.6423370590817,4.2));
#38083=CARTESIAN_POINT('Ctrl Pts',(30.9977590627279,-9.99211420570491,4.4853946853406));
#38084=CARTESIAN_POINT('Ctrl Pts',(30.9917239593499,-10.0904675123771,4.4319041637732));
#38085=CARTESIAN_POINT('Ctrl Pts',(30.9417901139861,-10.3323638606833,4.30380299959424));
#38086=CARTESIAN_POINT('Ctrl Pts',(30.8067905422249,-10.5514291753386,4.22117275143012));
#38087=CARTESIAN_POINT('Ctrl Pts',(30.7112855175711,-10.6546595286708,4.21735899290232));
#38088=CARTESIAN_POINT('Ctrl Pts',(30.9987342290661,-10.0081103673502,4.51459940199573));
#38089=CARTESIAN_POINT('Ctrl Pts',(30.9945308397623,-10.1064642790619,4.46091082785928));
#38090=CARTESIAN_POINT('Ctrl Pts',(30.9490334476689,-10.3477941569161,4.33074334133394));
#38091=CARTESIAN_POINT('Ctrl Pts',(30.8169841642302,-10.5649590869411,4.24234550286025));
#38092=CARTESIAN_POINT('Ctrl Pts',(30.7225710351422,-10.66698199826,4.23471798580464));
#38093=CARTESIAN_POINT('Ctrl Pts',(30.9997093954044,-10.0241065289954,4.54380411865086));
#38094=CARTESIAN_POINT('Ctrl Pts',(30.9973377201748,-10.1224610457467,4.48991749194537));
#38095=CARTESIAN_POINT('Ctrl Pts',(30.9562767813518,-10.363224453149,4.35768368307365));
#38096=CARTESIAN_POINT('Ctrl Pts',(30.8271777862355,-10.5784889985436,4.26351825429037));
#38097=CARTESIAN_POINT('Ctrl Pts',(30.7338565527132,-10.6793044678492,4.25207697870696));
#38098=CARTESIAN_POINT('',(30.7338565527132,-10.6793044678492,4.25207697870696));
#38099=CARTESIAN_POINT('Ctrl Pts',(30.9997093954044,-10.0241065289954,4.54380411865086));
#38100=CARTESIAN_POINT('Ctrl Pts',(30.9973377201748,-10.1224610457467,4.48991749194537));
#38101=CARTESIAN_POINT('Ctrl Pts',(30.9562767813518,-10.363224453149,4.35768368307365));
#38102=CARTESIAN_POINT('Ctrl Pts',(30.8271777862355,-10.5784889985436,4.26351825429037));
#38103=CARTESIAN_POINT('Ctrl Pts',(30.7338565527132,-10.6793044678492,4.25207697870696));
#38104=CARTESIAN_POINT('',(30.7338565527132,-10.6793044678492,4.25207697870696));
#38105=CARTESIAN_POINT('Ctrl Pts',(30.7,-10.6423370590817,4.2));
#38106=CARTESIAN_POINT('Ctrl Pts',(30.7965969202196,-10.5378992637361,4.19999999999999));
#38107=CARTESIAN_POINT('Ctrl Pts',(30.9345467803032,-10.3169335644504,4.27686265785453));
#38108=CARTESIAN_POINT('Ctrl Pts',(30.9889170789375,-10.0744707456924,4.40289749968711));
#38109=CARTESIAN_POINT('Ctrl Pts',(30.9967838963896,-9.97611804405966,4.45618996868547));
#38110=CARTESIAN_POINT('Ctrl Pts',(30.7,-10.7141428428543,4.25));
#38111=CARTESIAN_POINT('Ctrl Pts',(30.7115415847052,-10.7028298270137,4.25));
#38112=CARTESIAN_POINT('Ctrl Pts',(30.7228338070625,-10.6912124038448,4.25072557918172));
#38113=CARTESIAN_POINT('Ctrl Pts',(30.7338565527132,-10.6793044678492,4.25207697870696));
#38114=CARTESIAN_POINT('Ctrl Pts',(30.6883333333333,-10.70224046214,4.23333333333333));
#38115=CARTESIAN_POINT('Ctrl Pts',(30.7000220784993,-10.6907832001958,4.23333333333333));
#38116=CARTESIAN_POINT('Ctrl Pts',(30.7114193189812,-10.6790325526684,4.23381705278782));
#38117=CARTESIAN_POINT('Ctrl Pts',(30.7225710351422,-10.66698199826,4.23471798580464));
#38118=CARTESIAN_POINT('Ctrl Pts',(30.6766666666667,-10.6903380814258,4.21666666666667));
#38119=CARTESIAN_POINT('Ctrl Pts',(30.6885025722933,-10.678736573378,4.21666666666667));
#38120=CARTESIAN_POINT('Ctrl Pts',(30.7000048309,-10.666852701492,4.21690852639391));
#38121=CARTESIAN_POINT('Ctrl Pts',(30.7112855175711,-10.6546595286708,4.21735899290232));
#38122=CARTESIAN_POINT('Ctrl Pts',(30.665,-10.6784357007116,4.2));
#38123=CARTESIAN_POINT('Ctrl Pts',(30.6769830660874,-10.6666899465601,4.2));
#38124=CARTESIAN_POINT('Ctrl Pts',(30.6885903428187,-10.6546728503156,4.2));
#38125=CARTESIAN_POINT('Ctrl Pts',(30.7,-10.6423370590817,4.2));
#38126=CARTESIAN_POINT('Ctrl Pts',(30.7338565527132,-10.6793044678492,4.25207697870696));
#38127=CARTESIAN_POINT('Ctrl Pts',(30.7228338070625,-10.6912124038448,4.25072557918172));
#38128=CARTESIAN_POINT('Ctrl Pts',(30.7115415847052,-10.7028298270137,4.25));
#38129=CARTESIAN_POINT('Ctrl Pts',(30.7,-10.7141428428543,4.25));
#38130=CARTESIAN_POINT('Origin',(10.,-11.,4.2));
#38131=CARTESIAN_POINT('',(30.,-11.,6.15));
#38132=CARTESIAN_POINT('',(30.,-11.,4.2));
#38133=CARTESIAN_POINT('',(10.,-11.,6.15));
#38134=CARTESIAN_POINT('',(15.,-11.,6.15));
#38135=CARTESIAN_POINT('',(10.,-11.,4.2));
#38136=CARTESIAN_POINT('Origin',(30.,-10.,4.2));
#38137=CARTESIAN_POINT('',(31.,-10.,5.84299122874504));
#38138=CARTESIAN_POINT('',(31.,-10.,4.2));
#38139=CARTESIAN_POINT('',(30.9997094022748,-10.0241062440753,5.85619572522048));
#38140=CARTESIAN_POINT('Ctrl Pts',(30.9997094022748,-10.0241062440753,5.85619572522048));
#38141=CARTESIAN_POINT('Ctrl Pts',(30.9997130467291,-10.0239551050077,5.85611291886692));
#38142=CARTESIAN_POINT('Ctrl Pts',(30.9997167667759,-10.0237998867075,5.8560278777443));
#38143=CARTESIAN_POINT('Ctrl Pts',(30.9997219533132,-10.023579992868,5.85590740213001));
#38144=CARTESIAN_POINT('Ctrl Pts',(30.9997276961238,-10.0233365146857,5.8557740051069));
#38145=CARTESIAN_POINT('Ctrl Pts',(30.9997352339929,-10.0230139654796,5.85559728658946));
#38146=CARTESIAN_POINT('Ctrl Pts',(30.9997448361474,-10.0225889928205,5.85536445634685));
#38147=CARTESIAN_POINT('Ctrl Pts',(30.9997558335613,-10.0221022686959,5.85509779426031));
#38148=CARTESIAN_POINT('Ctrl Pts',(30.9997694965754,-10.0214819922295,5.85475796721774));
#38149=CARTESIAN_POINT('Ctrl Pts',(30.9997844991176,-10.020759463484,5.85436213274578));
#38150=CARTESIAN_POINT('Ctrl Pts',(30.9998039371891,-10.0198233177775,5.85384926907949));
#38151=CARTESIAN_POINT('Ctrl Pts',(30.9998254134561,-10.0187196114834,5.8532446282723));
#38152=CARTESIAN_POINT('Ctrl Pts',(30.9998453215427,-10.017587864828,5.85262465607974));
#38153=CARTESIAN_POINT('Ctrl Pts',(30.9998613100668,-10.0166789397704,5.85212674582915));
#38154=CARTESIAN_POINT('Ctrl Pts',(30.9998762660452,-10.0157556522058,5.85162098603055));
#38155=CARTESIAN_POINT('Ctrl Pts',(30.9998894641422,-10.0148680697274,5.85113480211444));
#38156=CARTESIAN_POINT('Ctrl Pts',(30.9999003578812,-10.014135457153,5.85073350481631));
#38157=CARTESIAN_POINT('Ctrl Pts',(30.9999100843927,-10.0134276007098,5.85034577993147));
#38158=CARTESIAN_POINT('Ctrl Pts',(30.999918884115,-10.0127367653004,5.84996738720872));
#38159=CARTESIAN_POINT('Ctrl Pts',(30.9999281242885,-10.0120113516037,5.84957005484841));
#38160=CARTESIAN_POINT('Ctrl Pts',(30.9999364353128,-10.0112992590878,5.84918002861482));
#38161=CARTESIAN_POINT('Ctrl Pts',(30.9999442513311,-10.0105590828167,5.84877462429034));
#38162=CARTESIAN_POINT('Ctrl Pts',(30.9999525187802,-10.0097761560831,5.84834580497266));
#38163=CARTESIAN_POINT('Ctrl Pts',(30.9999601882674,-10.0089618835122,5.84789982155921));
#38164=CARTESIAN_POINT('Ctrl Pts',(30.9999669578405,-10.0081291590671,5.84744373291581));
#38165=CARTESIAN_POINT('Ctrl Pts',(30.9999759712677,-10.0070204183844,5.84683646836768));
#38166=CARTESIAN_POINT('Ctrl Pts',(30.9999832541069,-10.0058810641504,5.84621243851916));
#38167=CARTESIAN_POINT('Ctrl Pts',(30.999988313939,-10.0048344581344,5.84563920390379));
#38168=CARTESIAN_POINT('Ctrl Pts',(30.9999924398875,-10.003981022191,5.84517177010603));
#38169=CARTESIAN_POINT('Ctrl Pts',(30.999995118254,-10.0031934906294,5.84474043007898));
#38170=CARTESIAN_POINT('Ctrl Pts',(30.9999967893852,-10.0025340125065,5.84437922167547));
#38171=CARTESIAN_POINT('Ctrl Pts',(30.9999982347598,-10.0019636246513,5.84406680966457));
#38172=CARTESIAN_POINT('Ctrl Pts',(30.9999989577288,-10.0014901279877,5.84380746257457));
#38173=CARTESIAN_POINT('Ctrl Pts',(30.9999993711998,-10.001121427621,5.84360551058622));
#38174=CARTESIAN_POINT('Ctrl Pts',(30.9999997402998,-10.0007922938583,5.84342523081487));
#38175=CARTESIAN_POINT('Ctrl Pts',(30.9999998688065,-10.0005469945696,5.84329086577593));
#38176=CARTESIAN_POINT('Ctrl Pts',(30.9999999369451,-10.0003551195025,5.84318576061118));
#38177=CARTESIAN_POINT('Ctrl Pts',(30.9999999853286,-10.000218873612,5.84311112795059));
#38178=CARTESIAN_POINT('Ctrl Pts',(31.,-10.0001088728919,5.84305086948946));
#38179=CARTESIAN_POINT('Ctrl Pts',(31.,-10.,5.84299122874504));
#38180=CARTESIAN_POINT('',(30.7338565527125,-10.6793044678499,6.14792302129313));
#38181=CARTESIAN_POINT('Ctrl Pts',(30.7338565527125,-10.6793044678499,6.14792302129313));
#38182=CARTESIAN_POINT('Ctrl Pts',(30.7622591025997,-10.6486210286339,6.14444084056899));
#38183=CARTESIAN_POINT('Ctrl Pts',(30.7899347430608,-10.6147354943559,6.13657883580837));
#38184=CARTESIAN_POINT('Ctrl Pts',(30.8465633390414,-10.5350521462962,6.11173493670335));
#38185=CARTESIAN_POINT('Ctrl Pts',(30.8872065032282,-10.4658719010602,6.08407025994295));
#38186=CARTESIAN_POINT('Ctrl Pts',(30.9368867620569,-10.3553346508213,6.03274417903868));
#38187=CARTESIAN_POINT('Ctrl Pts',(30.9615371967044,-10.2795901391215,5.99406746301422));
#38188=CARTESIAN_POINT('Ctrl Pts',(30.989705810262,-10.1599951404466,5.93078512444313));
#38189=CARTESIAN_POINT('Ctrl Pts',(30.9981384709031,-10.0892542969071,5.89188916163067));
#38190=CARTESIAN_POINT('Ctrl Pts',(30.9997094022748,-10.0241062440753,5.85619572522048));
#38191=CARTESIAN_POINT('',(30.7,-10.7141428428543,6.15));
#38192=CARTESIAN_POINT('Ctrl Pts',(30.7,-10.7141428428543,6.15));
#38193=CARTESIAN_POINT('Ctrl Pts',(30.7112905851662,-10.7030758557726,6.15));
#38194=CARTESIAN_POINT('Ctrl Pts',(30.7226212987117,-10.6914419778475,6.14930047455236));
#38195=CARTESIAN_POINT('Ctrl Pts',(30.7338565527125,-10.6793044678499,6.14792302129313));
#38196=CARTESIAN_POINT('Origin',(30.,-10.,6.15));
#38197=CARTESIAN_POINT('Origin',(31.,0.,14.5));
#38198=CARTESIAN_POINT('',(31.,0.,4.5));
#38199=CARTESIAN_POINT('',(31.,10.,5.84299122874504));
#38200=CARTESIAN_POINT('',(31.,10.,4.2));
#38201=CARTESIAN_POINT('',(31.,9.89591670002669,5.9));
#38202=CARTESIAN_POINT('',(31.,9.94795835001334,5.87149561437252));
#38203=CARTESIAN_POINT('',(31.,7.76915840380663,5.9));
#38204=CARTESIAN_POINT('',(31.,0.,5.9));
#38205=CARTESIAN_POINT('',(31.,3.52895676585423,21.8971243613659));
#38206=CARTESIAN_POINT('',(31.,6.41964359742627,10.9913513149805));
#38207=CARTESIAN_POINT('',(31.,-3.52895676585423,21.8971243613659));
#38208=CARTESIAN_POINT('Origin',(31.,0.,26.5));
#38209=CARTESIAN_POINT('',(31.,-7.76915840380663,5.9));
#38210=CARTESIAN_POINT('',(31.,-4.21964359742627,19.2913513149805));
#38211=CARTESIAN_POINT('',(31.,-9.89591670002669,5.9));
#38212=CARTESIAN_POINT('',(31.,0.,5.9));
#38213=CARTESIAN_POINT('',(31.,-9.94795835001334,5.87149561437252));
#38214=CARTESIAN_POINT('',(31.,-4.8,14.));
#38215=CARTESIAN_POINT('',(31.,-4.8,5.9));
#38216=CARTESIAN_POINT('',(31.,-4.8,10.35));
#38217=CARTESIAN_POINT('',(31.,4.8,14.));
#38218=CARTESIAN_POINT('Origin',(31.,0.,14.));
#38219=CARTESIAN_POINT('',(31.,4.8,5.9));
#38220=CARTESIAN_POINT('',(31.,4.8,14.25));
#38221=CARTESIAN_POINT('',(31.,0.,5.9));
#38222=CARTESIAN_POINT('Origin',(30.7,0.,4.5));
#38223=CARTESIAN_POINT('Origin',(19.,11.1,4.2));
#38224=CARTESIAN_POINT('',(19.,11.1,4.8));
#38225=CARTESIAN_POINT('Origin',(21.,-11.1,4.2));
#38226=CARTESIAN_POINT('',(21.,-11.1,4.8));
#38227=CARTESIAN_POINT('Origin',(20.,0.,4.8));
#38228=CARTESIAN_POINT('Origin',(20.,0.,4.2));
#38229=CARTESIAN_POINT('',(10.4,9.,4.2));
#38230=CARTESIAN_POINT('',(10.4,9.4,4.2));
#38231=CARTESIAN_POINT('',(10.4,4.5,4.2));
#38232=CARTESIAN_POINT('',(11.6,9.,4.2));
#38233=CARTESIAN_POINT('Origin',(11.,9.,4.2));
#38234=CARTESIAN_POINT('',(11.6,9.4,4.2));
#38235=CARTESIAN_POINT('',(11.6,4.7,4.2));
#38236=CARTESIAN_POINT('Origin',(11.,9.4,4.2));
#38237=CARTESIAN_POINT('',(10.4,-9.4,4.2));
#38238=CARTESIAN_POINT('',(10.4,-9.,4.2));
#38239=CARTESIAN_POINT('',(10.4,-4.7,4.2));
#38240=CARTESIAN_POINT('',(11.6,-9.4,4.2));
#38241=CARTESIAN_POINT('Origin',(11.,-9.4,4.2));
#38242=CARTESIAN_POINT('',(11.6,-9.,4.2));
#38243=CARTESIAN_POINT('',(11.6,-4.5,4.2));
#38244=CARTESIAN_POINT('Origin',(11.,-9.,4.2));
#38245=CARTESIAN_POINT('Origin',(28.425,-4.7,4.225));
#38246=CARTESIAN_POINT('',(28.45,-9.4,4.25));
#38247=CARTESIAN_POINT('',(28.45,-9.4,4.25));
#38248=CARTESIAN_POINT('',(28.45,-9.,4.25));
#38249=CARTESIAN_POINT('',(28.4,-9.,4.2));
#38250=CARTESIAN_POINT('',(28.45,-4.7,4.25));
#38251=CARTESIAN_POINT('Origin',(29.,-9.4,4.225));
#38252=CARTESIAN_POINT('',(29.55,-9.4,4.25));
#38253=CARTESIAN_POINT('',(29.55,-9.4,4.25));
#38254=CARTESIAN_POINT('Origin',(29.,-9.4,4.25));
#38255=CARTESIAN_POINT('Origin',(29.575,-4.5,4.225));
#38256=CARTESIAN_POINT('',(29.55,-9.,4.25));
#38257=CARTESIAN_POINT('',(29.55,-9.,4.25));
#38258=CARTESIAN_POINT('',(29.55,-4.5,4.25));
#38259=CARTESIAN_POINT('Origin',(29.,-9.,4.225));
#38260=CARTESIAN_POINT('Origin',(29.,-9.,4.25));
#38261=CARTESIAN_POINT('Origin',(29.,-9.4,6.2));
#38262=CARTESIAN_POINT('',(28.45,-9.4,6.15));
#38263=CARTESIAN_POINT('',(28.45,-9.4,6.2));
#38264=CARTESIAN_POINT('',(29.55,-9.4,6.15));
#38265=CARTESIAN_POINT('Origin',(29.,-9.4,6.15));
#38266=CARTESIAN_POINT('',(29.55,-9.4,6.2));
#38267=CARTESIAN_POINT('Origin',(28.45,-9.4,6.2));
#38268=CARTESIAN_POINT('',(28.45,-9.,6.15));
#38269=CARTESIAN_POINT('',(28.45,-9.,6.2));
#38270=CARTESIAN_POINT('',(28.45,-4.7,6.15));
#38271=CARTESIAN_POINT('Origin',(10.425,4.5,4.225));
#38272=CARTESIAN_POINT('',(10.45,9.,4.25));
#38273=CARTESIAN_POINT('',(10.45,9.,4.25));
#38274=CARTESIAN_POINT('',(10.45,9.4,4.25));
#38275=CARTESIAN_POINT('',(10.4,9.4,4.2));
#38276=CARTESIAN_POINT('',(10.45,4.5,4.25));
#38277=CARTESIAN_POINT('Origin',(11.,9.,4.225));
#38278=CARTESIAN_POINT('',(11.55,9.,4.25));
#38279=CARTESIAN_POINT('',(11.55,9.,4.25));
#38280=CARTESIAN_POINT('Origin',(11.,9.,4.25));
#38281=CARTESIAN_POINT('Origin',(11.575,4.7,4.225));
#38282=CARTESIAN_POINT('',(11.55,9.4,4.25));
#38283=CARTESIAN_POINT('',(11.55,9.4,4.25));
#38284=CARTESIAN_POINT('',(11.55,4.7,4.25));
#38285=CARTESIAN_POINT('Origin',(11.,9.4,4.225));
#38286=CARTESIAN_POINT('Origin',(11.,9.4,4.25));
#38287=CARTESIAN_POINT('Origin',(11.,9.,6.2));
#38288=CARTESIAN_POINT('',(10.45,9.,6.15));
#38289=CARTESIAN_POINT('',(10.45,9.,6.2));
#38290=CARTESIAN_POINT('',(11.55,9.,6.15));
#38291=CARTESIAN_POINT('Origin',(11.,9.,6.15));
#38292=CARTESIAN_POINT('',(11.55,9.,6.2));
#38293=CARTESIAN_POINT('Origin',(10.45,9.,6.2));
#38294=CARTESIAN_POINT('',(10.45,9.4,6.15));
#38295=CARTESIAN_POINT('',(10.45,9.4,6.2));
#38296=CARTESIAN_POINT('',(10.45,4.5,6.15));
#38297=CARTESIAN_POINT('Origin',(10.425,-4.7,4.225));
#38298=CARTESIAN_POINT('',(10.45,-9.4,4.25));
#38299=CARTESIAN_POINT('',(10.45,-9.4,4.25));
#38300=CARTESIAN_POINT('',(10.45,-9.,4.25));
#38301=CARTESIAN_POINT('',(10.4,-9.,4.2));
#38302=CARTESIAN_POINT('',(10.45,-4.7,4.25));
#38303=CARTESIAN_POINT('Origin',(11.,-9.4,4.225));
#38304=CARTESIAN_POINT('',(11.55,-9.4,4.25));
#38305=CARTESIAN_POINT('',(11.55,-9.4,4.25));
#38306=CARTESIAN_POINT('Origin',(11.,-9.4,4.25));
#38307=CARTESIAN_POINT('Origin',(11.575,-4.5,4.225));
#38308=CARTESIAN_POINT('',(11.55,-9.,4.25));
#38309=CARTESIAN_POINT('',(11.55,-9.,4.25));
#38310=CARTESIAN_POINT('',(11.55,-4.5,4.25));
#38311=CARTESIAN_POINT('Origin',(11.,-9.,4.225));
#38312=CARTESIAN_POINT('Origin',(11.,-9.,4.25));
#38313=CARTESIAN_POINT('Origin',(11.,-9.4,6.2));
#38314=CARTESIAN_POINT('',(10.45,-9.4,6.15));
#38315=CARTESIAN_POINT('',(10.45,-9.4,6.2));
#38316=CARTESIAN_POINT('',(11.55,-9.4,6.15));
#38317=CARTESIAN_POINT('Origin',(11.,-9.4,6.15));
#38318=CARTESIAN_POINT('',(11.55,-9.4,6.2));
#38319=CARTESIAN_POINT('Origin',(10.45,-9.4,6.2));
#38320=CARTESIAN_POINT('',(10.45,-9.,6.15));
#38321=CARTESIAN_POINT('',(10.45,-9.,6.2));
#38322=CARTESIAN_POINT('',(10.45,-4.7,6.15));
#38323=CARTESIAN_POINT('Origin',(28.425,4.5,4.225));
#38324=CARTESIAN_POINT('',(28.45,9.,4.25));
#38325=CARTESIAN_POINT('',(28.45,9.,4.25));
#38326=CARTESIAN_POINT('',(28.45,9.4,4.25));
#38327=CARTESIAN_POINT('',(28.4,9.4,4.2));
#38328=CARTESIAN_POINT('',(28.45,4.5,4.25));
#38329=CARTESIAN_POINT('Origin',(29.,9.,4.225));
#38330=CARTESIAN_POINT('',(29.55,9.,4.25));
#38331=CARTESIAN_POINT('',(29.55,9.,4.25));
#38332=CARTESIAN_POINT('Origin',(29.,9.,4.25));
#38333=CARTESIAN_POINT('Origin',(29.575,4.7,4.225));
#38334=CARTESIAN_POINT('',(29.55,9.4,4.25));
#38335=CARTESIAN_POINT('',(29.55,9.4,4.25));
#38336=CARTESIAN_POINT('',(29.55,4.7,4.25));
#38337=CARTESIAN_POINT('Origin',(29.,9.4,4.225));
#38338=CARTESIAN_POINT('Origin',(29.,9.4,4.25));
#38339=CARTESIAN_POINT('Origin',(29.,9.,6.2));
#38340=CARTESIAN_POINT('',(28.45,9.,6.15));
#38341=CARTESIAN_POINT('',(28.45,9.,6.2));
#38342=CARTESIAN_POINT('',(29.55,9.,6.15));
#38343=CARTESIAN_POINT('Origin',(29.,9.,6.15));
#38344=CARTESIAN_POINT('',(29.55,9.,6.2));
#38345=CARTESIAN_POINT('Origin',(28.45,9.,6.2));
#38346=CARTESIAN_POINT('',(28.45,9.4,6.15));
#38347=CARTESIAN_POINT('',(28.45,9.4,6.2));
#38348=CARTESIAN_POINT('',(28.45,4.5,6.15));
#38349=CARTESIAN_POINT('Origin',(8.025,-3.53553390593274,30.0355339059327));
#38350=CARTESIAN_POINT('',(8.,-3.53553390593274,30.3905339059327));
#38351=CARTESIAN_POINT('Origin',(8.,-3.53553390593274,30.0355339059327));
#38352=CARTESIAN_POINT('',(8.05,-3.53553390593274,30.3405339059327));
#38353=CARTESIAN_POINT('',(8.025,-3.53553390593274,30.3655339059327));
#38354=CARTESIAN_POINT('',(8.05,-3.53553390593274,29.7305339059327));
#38355=CARTESIAN_POINT('Origin',(8.05,-3.53553390593274,30.0355339059327));
#38356=CARTESIAN_POINT('Origin',(8.05,-3.53553390593274,30.0355339059327));
#38357=CARTESIAN_POINT('Origin',(8.,-3.53553390593274,30.0355339059327));
#38358=CARTESIAN_POINT('Origin',(8.685,-3.53553390593274,30.0355339059327));
#38359=CARTESIAN_POINT('',(9.4,-3.53553390593274,29.7305339059327));
#38360=CARTESIAN_POINT('Origin',(9.4,-3.53553390593274,30.0355339059327));
#38361=CARTESIAN_POINT('',(8.685,-3.53553390593274,29.7305339059327));
#38362=CARTESIAN_POINT('Origin',(8.025,-3.53553390593274,22.9644660940673));
#38363=CARTESIAN_POINT('',(8.,-3.53553390593274,22.6094660940673));
#38364=CARTESIAN_POINT('Origin',(8.,-3.53553390593274,22.9644660940673));
#38365=CARTESIAN_POINT('',(8.05,-3.53553390593274,22.6594660940673));
#38366=CARTESIAN_POINT('',(8.025,-3.53553390593274,22.6344660940673));
#38367=CARTESIAN_POINT('Origin',(8.05,-3.53553390593274,22.9644660940673));
#38368=CARTESIAN_POINT('Origin',(8.,-3.53553390593274,22.9644660940673));
#38369=CARTESIAN_POINT('Origin',(8.685,-3.53553390593274,22.9644660940673));
#38370=CARTESIAN_POINT('',(9.4,-3.53553390593274,22.6594660940673));
#38371=CARTESIAN_POINT('Origin',(9.4,-3.53553390593274,22.9644660940673));
#38372=CARTESIAN_POINT('',(8.685,-3.53553390593274,22.6594660940673));
#38373=CARTESIAN_POINT('Origin',(28.425,4.5,6.175));
#38374=CARTESIAN_POINT('',(28.4,9.4,6.2));
#38375=CARTESIAN_POINT('',(28.45,9.4,6.15));
#38376=CARTESIAN_POINT('',(28.4,9.,6.2));
#38377=CARTESIAN_POINT('',(28.4,4.5,6.2));
#38378=CARTESIAN_POINT('',(28.4,9.,6.2));
#38379=CARTESIAN_POINT('Origin',(29.,9.4,6.175));
#38380=CARTESIAN_POINT('',(29.55,9.4,6.15));
#38381=CARTESIAN_POINT('',(29.6,9.4,6.2));
#38382=CARTESIAN_POINT('',(29.55,9.4,6.15));
#38383=CARTESIAN_POINT('Origin',(29.,9.4,6.2));
#38384=CARTESIAN_POINT('Origin',(29.,9.4,6.15));
#38385=CARTESIAN_POINT('Origin',(29.575,4.7,6.175));
#38386=CARTESIAN_POINT('',(29.6,9.,6.2));
#38387=CARTESIAN_POINT('',(29.55,9.,6.15));
#38388=CARTESIAN_POINT('',(29.6,4.7,6.2));
#38389=CARTESIAN_POINT('',(29.55,4.7,6.15));
#38390=CARTESIAN_POINT('Origin',(29.,9.,6.175));
#38391=CARTESIAN_POINT('Origin',(29.,9.,6.2));
#38392=CARTESIAN_POINT('Origin',(29.,9.4,6.2));
#38393=CARTESIAN_POINT('',(29.55,9.4,6.2));
#38394=CARTESIAN_POINT('Origin',(20.,0.,6.2));
#38395=CARTESIAN_POINT('',(30.6999999999995,-10.6423370590827,6.2));
#38396=CARTESIAN_POINT('',(30.665,-10.6784357007116,6.2));
#38397=CARTESIAN_POINT('Ctrl Pts',(30.6999999999992,-10.6423370590825,6.2));
#38398=CARTESIAN_POINT('Ctrl Pts',(30.6883703751711,-10.6549106729719,6.2));
#38399=CARTESIAN_POINT('Ctrl Pts',(30.6767224654731,-10.6669453862552,6.2));
#38400=CARTESIAN_POINT('Ctrl Pts',(30.665,-10.6784357007116,6.2));
#38401=CARTESIAN_POINT('',(30.7,-8.,6.2));
#38402=CARTESIAN_POINT('',(30.7,0.,6.2));
#38403=CARTESIAN_POINT('',(10.05,-8.,6.2));
#38404=CARTESIAN_POINT('',(10.,-8.,6.2));
#38405=CARTESIAN_POINT('',(10.,-7.94827338858625,6.2));
#38406=CARTESIAN_POINT('',(9.57006962784493,-7.50349656267753,6.2));
#38407=CARTESIAN_POINT('',(10.,-4.55,6.2));
#38408=CARTESIAN_POINT('',(10.,-4.5,6.2));
#38409=CARTESIAN_POINT('',(10.05,-4.5,6.2));
#38410=CARTESIAN_POINT('',(13.65,-0.900000000000021,6.2));
#38411=CARTESIAN_POINT('',(30.7,-4.5,6.2));
#38412=CARTESIAN_POINT('',(10.,-4.5,6.2));
#38413=CARTESIAN_POINT('',(30.7,4.5,6.2));
#38414=CARTESIAN_POINT('',(30.7,0.,6.2));
#38415=CARTESIAN_POINT('',(10.,4.5,6.2));
#38416=CARTESIAN_POINT('',(10.05,8.,6.2));
#38417=CARTESIAN_POINT('',(10.1197528260391,8.07216154655071,6.2));
#38418=CARTESIAN_POINT('',(30.7,8.,6.2));
#38419=CARTESIAN_POINT('',(10.,8.,6.2));
#38420=CARTESIAN_POINT('',(30.6999999999995,10.6423370590827,6.2));
#38421=CARTESIAN_POINT('',(30.7,0.,6.2));
#38422=CARTESIAN_POINT('',(30.665,10.6784357007116,6.2));
#38423=CARTESIAN_POINT('Ctrl Pts',(30.665,10.6784357007116,6.2));
#38424=CARTESIAN_POINT('Ctrl Pts',(30.6767224654731,10.6669453862552,6.2));
#38425=CARTESIAN_POINT('Ctrl Pts',(30.6883703751711,10.6549106729719,6.2));
#38426=CARTESIAN_POINT('Ctrl Pts',(30.6999999999992,10.6423370590825,6.2));
#38427=CARTESIAN_POINT('',(30.,10.95,6.2));
#38428=CARTESIAN_POINT('Origin',(30.,10.,6.2));
#38429=CARTESIAN_POINT('',(10.,10.95,6.2));
#38430=CARTESIAN_POINT('',(25.,10.95,6.2));
#38431=CARTESIAN_POINT('',(9.05,10.,6.2));
#38432=CARTESIAN_POINT('Origin',(10.,10.,6.2));
#38433=CARTESIAN_POINT('',(9.05,-10.,6.2));
#38434=CARTESIAN_POINT('',(9.05,5.,6.2));
#38435=CARTESIAN_POINT('',(10.,-10.95,6.2));
#38436=CARTESIAN_POINT('Origin',(10.,-10.,6.2));
#38437=CARTESIAN_POINT('',(30.,-10.95,6.2));
#38438=CARTESIAN_POINT('',(15.,-10.95,6.2));
#38439=CARTESIAN_POINT('Origin',(30.,-10.,6.2));
#38440=CARTESIAN_POINT('',(10.4,-9.,6.2));
#38441=CARTESIAN_POINT('',(10.4,-9.4,6.2));
#38442=CARTESIAN_POINT('',(10.4,-4.7,6.2));
#38443=CARTESIAN_POINT('',(11.6,-9.,6.2));
#38444=CARTESIAN_POINT('Origin',(11.,-9.,6.2));
#38445=CARTESIAN_POINT('',(11.6,-9.4,6.2));
#38446=CARTESIAN_POINT('',(11.6,-4.5,6.2));
#38447=CARTESIAN_POINT('Origin',(11.,-9.4,6.2));
#38448=CARTESIAN_POINT('',(28.4,-9.,6.2));
#38449=CARTESIAN_POINT('',(28.4,-9.4,6.2));
#38450=CARTESIAN_POINT('',(28.4,-4.7,6.2));
#38451=CARTESIAN_POINT('',(29.6,-9.,6.2));
#38452=CARTESIAN_POINT('Origin',(29.,-9.,6.2));
#38453=CARTESIAN_POINT('',(29.6,-9.4,6.2));
#38454=CARTESIAN_POINT('',(29.6,-4.5,6.2));
#38455=CARTESIAN_POINT('Origin',(29.,-9.4,6.2));
#38456=CARTESIAN_POINT('',(10.4,9.4,6.2));
#38457=CARTESIAN_POINT('',(10.4,9.,6.2));
#38458=CARTESIAN_POINT('',(10.4,4.5,6.2));
#38459=CARTESIAN_POINT('',(11.6,9.4,6.2));
#38460=CARTESIAN_POINT('Origin',(11.,9.4,6.2));
#38461=CARTESIAN_POINT('',(11.6,9.,6.2));
#38462=CARTESIAN_POINT('',(11.6,4.7,6.2));
#38463=CARTESIAN_POINT('Origin',(11.,9.,6.2));
#38464=CARTESIAN_POINT('Origin',(10.425,-4.7,6.175));
#38465=CARTESIAN_POINT('',(10.45,-9.,6.15));
#38466=CARTESIAN_POINT('',(10.4,-9.4,6.2));
#38467=CARTESIAN_POINT('Origin',(11.,-9.,6.175));
#38468=CARTESIAN_POINT('',(11.55,-9.,6.15));
#38469=CARTESIAN_POINT('',(11.55,-9.,6.15));
#38470=CARTESIAN_POINT('Origin',(11.,-9.,6.15));
#38471=CARTESIAN_POINT('Origin',(11.575,-4.5,6.175));
#38472=CARTESIAN_POINT('',(11.55,-9.4,6.15));
#38473=CARTESIAN_POINT('',(11.55,-4.5,6.15));
#38474=CARTESIAN_POINT('Origin',(11.,-9.4,6.175));
#38475=CARTESIAN_POINT('Origin',(11.,-9.,6.2));
#38476=CARTESIAN_POINT('',(11.55,-9.,6.2));
#38477=CARTESIAN_POINT('Origin',(10.425,4.5,6.175));
#38478=CARTESIAN_POINT('',(10.45,9.4,6.15));
#38479=CARTESIAN_POINT('',(10.4,9.,6.2));
#38480=CARTESIAN_POINT('Origin',(11.,9.4,6.175));
#38481=CARTESIAN_POINT('',(11.55,9.4,6.15));
#38482=CARTESIAN_POINT('',(11.55,9.4,6.15));
#38483=CARTESIAN_POINT('Origin',(11.,9.4,6.15));
#38484=CARTESIAN_POINT('Origin',(11.575,4.7,6.175));
#38485=CARTESIAN_POINT('',(11.55,9.,6.15));
#38486=CARTESIAN_POINT('',(11.55,4.7,6.15));
#38487=CARTESIAN_POINT('Origin',(11.,9.,6.175));
#38488=CARTESIAN_POINT('Origin',(11.,9.4,6.2));
#38489=CARTESIAN_POINT('',(11.55,9.4,6.2));
#38490=CARTESIAN_POINT('Origin',(28.425,-4.7,6.175));
#38491=CARTESIAN_POINT('',(28.45,-9.,6.15));
#38492=CARTESIAN_POINT('',(28.4,-9.4,6.2));
#38493=CARTESIAN_POINT('Origin',(29.,-9.,6.175));
#38494=CARTESIAN_POINT('',(29.55,-9.,6.15));
#38495=CARTESIAN_POINT('',(29.55,-9.,6.15));
#38496=CARTESIAN_POINT('Origin',(29.,-9.,6.15));
#38497=CARTESIAN_POINT('Origin',(29.575,-4.5,6.175));
#38498=CARTESIAN_POINT('',(29.55,-9.4,6.15));
#38499=CARTESIAN_POINT('',(29.55,-4.5,6.15));
#38500=CARTESIAN_POINT('Origin',(29.,-9.4,6.175));
#38501=CARTESIAN_POINT('Origin',(29.,-9.,6.2));
#38502=CARTESIAN_POINT('',(29.55,-9.,6.2));
#38503=CARTESIAN_POINT('Ctrl Pts',(30.9967839207979,-9.97611773894901,5.94380986596425));
#38504=CARTESIAN_POINT('Ctrl Pts',(30.9968735332431,-9.97499738060725,5.94320279876029));
#38505=CARTESIAN_POINT('Ctrl Pts',(30.9972890756224,-9.9705803344265,5.94081795655504));
#38506=CARTESIAN_POINT('Ctrl Pts',(30.9987938608894,-9.94698237002212,5.92798567506077));
#38507=CARTESIAN_POINT('Ctrl Pts',(30.9996652546658,-9.92505107393448,5.91596719019954));
#38508=CARTESIAN_POINT('Ctrl Pts',(31.0000630673885,-9.90147072833049,5.90303515049092));
#38509=CARTESIAN_POINT('Ctrl Pts',(31.,-9.89703879482902,5.90061245162622));
#38510=CARTESIAN_POINT('Ctrl Pts',(31.,-9.89591670002669,5.9));
#38511=CARTESIAN_POINT('Ctrl Pts',(30.9977590812902,-9.99211390732443,5.91460515238299));
#38512=CARTESIAN_POINT('Ctrl Pts',(30.9978069161407,-9.99125420879031,5.91413815597096));
#38513=CARTESIAN_POINT('Ctrl Pts',(30.9980732319381,-9.98842826990598,5.91261689806809));
#38514=CARTESIAN_POINT('Ctrl Pts',(30.999321009672,-9.96926387849275,5.90220348853136));
#38515=CARTESIAN_POINT('Ctrl Pts',(30.9998924434135,-9.95345363247024,5.89352772308427));
#38516=CARTESIAN_POINT('Ctrl Pts',(31.0001048667676,-9.93430897921292,5.88301910115843));
#38517=CARTESIAN_POINT('Ctrl Pts',(31.,-9.93147133203902,5.88146680533134));
#38518=CARTESIAN_POINT('Ctrl Pts',(31.,-9.93061113335113,5.88099707624835));
#38519=CARTESIAN_POINT('Ctrl Pts',(30.9987342417825,-10.0081100756998,5.88540043880173));
#38520=CARTESIAN_POINT('Ctrl Pts',(30.9987548737402,-10.0075123659462,5.88507472775089));
#38521=CARTESIAN_POINT('Ctrl Pts',(30.9989180472781,-10.0045931974246,5.88348145728224));
#38522=CARTESIAN_POINT('Ctrl Pts',(30.9993345295876,-9.99306004052342,5.87717591947565));
#38523=CARTESIAN_POINT('Ctrl Pts',(30.9997836739084,-9.98034680751244,5.8702235696389));
#38524=CARTESIAN_POINT('Ctrl Pts',(30.9999536075356,-9.96882546804112,5.86391936825949));
#38525=CARTESIAN_POINT('Ctrl Pts',(31.,-9.96590386924902,5.86232115903647));
#38526=CARTESIAN_POINT('Ctrl Pts',(31.,-9.96530556667556,5.8619941524967));
#38527=CARTESIAN_POINT('Ctrl Pts',(30.9997094022748,-10.0241062440753,5.85619572522048));
#38528=CARTESIAN_POINT('Ctrl Pts',(30.9997175112483,-10.0237699570528,5.85601147966085));
#38529=CARTESIAN_POINT('Ctrl Pts',(30.9997551934488,-10.0224437131072,5.85528478208135));
#38530=CARTESIAN_POINT('Ctrl Pts',(30.9998913609518,-10.0153494616369,5.8513983439133));
#38531=CARTESIAN_POINT('Ctrl Pts',(30.999969787671,-10.0087556517074,5.84778686339001));
#38532=CARTESIAN_POINT('Ctrl Pts',(31.000005693946,-10.0016661590036,5.84390391661895));
#38533=CARTESIAN_POINT('Ctrl Pts',(31.,-10.000336406459,5.84317551274159));
#38534=CARTESIAN_POINT('Ctrl Pts',(31.,-10.,5.84299122874504));
#38535=CARTESIAN_POINT('',(30.9967839207979,-9.97611773894901,5.94380986596425));
#38536=CARTESIAN_POINT('Ctrl Pts',(31.,-9.89591670002669,5.9));
#38537=CARTESIAN_POINT('Ctrl Pts',(31.,-9.89628582891983,5.90020147459058));
#38538=CARTESIAN_POINT('Ctrl Pts',(30.999999833778,-9.89665895570928,5.90040514179247));
#38539=CARTESIAN_POINT('Ctrl Pts',(30.9999992763601,-9.89712339088896,5.90065892594312));
#38540=CARTESIAN_POINT('Ctrl Pts',(30.9999986903024,-9.89761168848563,5.90092574937998));
#38541=CARTESIAN_POINT('Ctrl Pts',(30.9999976784015,-9.89820065116803,5.90124782620294));
#38542=CARTESIAN_POINT('Ctrl Pts',(30.9999954463192,-9.89894085089812,5.90165293306493));
#38543=CARTESIAN_POINT('Ctrl Pts',(30.9999930609434,-9.89973188558847,5.90208586159504));
#38544=CARTESIAN_POINT('Ctrl Pts',(30.9999892731396,-9.90069527159664,5.90261341361232));
#38545=CARTESIAN_POINT('Ctrl Pts',(30.9999824925249,-9.90184085130876,5.90324101505058));
#38546=CARTESIAN_POINT('Ctrl Pts',(30.9999749254477,-9.90311930326004,5.90394141003391));
#38547=CARTESIAN_POINT('Ctrl Pts',(30.9999635671848,-9.90462412305264,5.9047661147155));
#38548=CARTESIAN_POINT('Ctrl Pts',(30.9999459978991,-9.9063130903906,5.90569195435123));
#38549=CARTESIAN_POINT('Ctrl Pts',(30.9999225298142,-9.90856912000303,5.90692863998015));
#38550=CARTESIAN_POINT('Ctrl Pts',(30.9998876385962,-9.91115223536192,5.90834496729864));
#38551=CARTESIAN_POINT('Ctrl Pts',(30.9998386164076,-9.91387679834281,5.9098389080064));
#38552=CARTESIAN_POINT('Ctrl Pts',(30.9997947529335,-9.91631464947568,5.91117563799665));
#38553=CARTESIAN_POINT('Ctrl Pts',(30.9997396715424,-9.91886066572249,5.91257171207271));
#38554=CARTESIAN_POINT('Ctrl Pts',(30.9996752373026,-9.92138435056691,5.91395536268362));
#38555=CARTESIAN_POINT('Ctrl Pts',(30.9996230683389,-9.92342764344206,5.91507563070807));
#38556=CARTESIAN_POINT('Ctrl Pts',(30.9995649295049,-9.92545543660446,5.91618728468542));
#38557=CARTESIAN_POINT('Ctrl Pts',(30.9995025257403,-9.92743003826348,5.91726954183405));
#38558=CARTESIAN_POINT('Ctrl Pts',(30.9994457779765,-9.92922567077687,5.91825370798981));
#38559=CARTESIAN_POINT('Ctrl Pts',(30.999385596974,-9.93097685281939,5.91921331456944));
#38560=CARTESIAN_POINT('Ctrl Pts',(30.9993223246179,-9.93269240748663,5.92015306391949));
#38561=CARTESIAN_POINT('Ctrl Pts',(30.9992408992974,-9.93490015818756,5.92136242922035));
#38562=CARTESIAN_POINT('Ctrl Pts',(30.9991545307602,-9.93705010559649,5.92253957558285));
#38563=CARTESIAN_POINT('Ctrl Pts',(30.9990586997045,-9.93925628042519,5.92374645512596));
#38564=CARTESIAN_POINT('Ctrl Pts',(30.9989827215795,-9.94100541097352,5.92470331033505));
#38565=CARTESIAN_POINT('Ctrl Pts',(30.9989006040821,-9.94279114085914,5.92567953304286));
#38566=CARTESIAN_POINT('Ctrl Pts',(30.9988112465986,-9.94462324232011,5.92668030933487));
#38567=CARTESIAN_POINT('Ctrl Pts',(30.9987116641645,-9.94666498651151,5.92779560192353));
#38568=CARTESIAN_POINT('Ctrl Pts',(30.9986030068889,-9.94876376320262,5.92894107424351));
#38569=CARTESIAN_POINT('Ctrl Pts',(30.9984868228399,-9.95087710858715,5.93009346425666));
#38570=CARTESIAN_POINT('Ctrl Pts',(30.9983246628225,-9.95382674002892,5.9317018742406));
#38571=CARTESIAN_POINT('Ctrl Pts',(30.9981474716006,-9.95680342456077,5.93332297948874));
#38572=CARTESIAN_POINT('Ctrl Pts',(30.9979699769605,-9.95959391161321,5.93484096482843));
#38573=CARTESIAN_POINT('Ctrl Pts',(30.9978227927092,-9.96190787302162,5.93609972698306));
#38574=CARTESIAN_POINT('Ctrl Pts',(30.9976759093371,-9.96408899229249,5.93728499112343));
#38575=CARTESIAN_POINT('Ctrl Pts',(30.9975408287681,-9.96601982372525,5.93833347383131));
#38576=CARTESIAN_POINT('Ctrl Pts',(30.9974308421475,-9.9675919641583,5.9391871796652));
#38577=CARTESIAN_POINT('Ctrl Pts',(30.9973288512699,-9.96899745226107,5.93994983139551));
#38578=CARTESIAN_POINT('Ctrl Pts',(30.9972396036754,-9.97020199451459,5.94060317730052));
#38579=CARTESIAN_POINT('Ctrl Pts',(30.9971564144503,-9.97132476916394,5.94121217230859));
#38580=CARTESIAN_POINT('Ctrl Pts',(30.9970843875899,-9.97227236442104,5.94172588660037));
#38581=CARTESIAN_POINT('Ctrl Pts',(30.9970242908726,-9.97305368650373,5.94214938471251));
#38582=CARTESIAN_POINT('Ctrl Pts',(30.9969678010577,-9.97378811496787,5.9425474651904));
#38583=CARTESIAN_POINT('Ctrl Pts',(30.9969218859903,-9.97437530434443,5.94286565959656));
#38584=CARTESIAN_POINT('Ctrl Pts',(30.9968835373317,-9.97486243255521,5.94312963321655));
#38585=CARTESIAN_POINT('Ctrl Pts',(30.9968451886732,-9.97534956076599,5.94339360683654));
#38586=CARTESIAN_POINT('Ctrl Pts',(30.996814458702,-9.9757359460458,5.94360299112644));
#38587=CARTESIAN_POINT('Ctrl Pts',(30.9967839207979,-9.97611773894901,5.94380986596425));
#38588=CARTESIAN_POINT('Ctrl Pts',(30.9997094022748,-10.0241062440753,5.85619572522048));
#38589=CARTESIAN_POINT('Ctrl Pts',(30.9987342417825,-10.0081100756998,5.88540043880173));
#38590=CARTESIAN_POINT('Ctrl Pts',(30.9977590812902,-9.99211390732443,5.91460515238299));
#38591=CARTESIAN_POINT('Ctrl Pts',(30.9967839207979,-9.97611773894901,5.94380986596425));
#38592=CARTESIAN_POINT('Ctrl Pts',(30.9997094013184,10.0241062837382,5.85619574695114));
#38593=CARTESIAN_POINT('Ctrl Pts',(30.9997175103186,10.0237699961624,5.85601150108837));
#38594=CARTESIAN_POINT('Ctrl Pts',(30.9997551926432,10.0224437500347,5.85528480231412));
#38595=CARTESIAN_POINT('Ctrl Pts',(30.9998913605943,10.0153494868895,5.851398357763));
#38596=CARTESIAN_POINT('Ctrl Pts',(30.9999697875716,10.0087556661136,5.84778687129035));
#38597=CARTESIAN_POINT('Ctrl Pts',(31.0000056939647,10.0016661617464,5.84390391812109));
#38598=CARTESIAN_POINT('Ctrl Pts',(31.,10.0003364070128,5.84317551304497));
#38599=CARTESIAN_POINT('Ctrl Pts',(31.,10.,5.84299122874504));
#38600=CARTESIAN_POINT('Ctrl Pts',(30.9987342400859,10.008110115381,5.8854004604625));
#38601=CARTESIAN_POINT('Ctrl Pts',(30.9987548720843,10.0075124050725,5.8850747491106));
#38602=CARTESIAN_POINT('Ctrl Pts',(30.9988790936942,10.0045934168424,5.88348147745615));
#38603=CARTESIAN_POINT('Ctrl Pts',(30.9992674936025,9.99306545616,5.87717593328547));
#38604=CARTESIAN_POINT('Ctrl Pts',(30.9996846877919,9.98035159735118,5.87022357752267));
#38605=CARTESIAN_POINT('Ctrl Pts',(30.9999513575747,9.96882758392452,5.86391936975968));
#38606=CARTESIAN_POINT('Ctrl Pts',(31.,9.96590386980433,5.8623211593403));
#38607=CARTESIAN_POINT('Ctrl Pts',(31.,9.96530556667556,5.8619941524967));
#38608=CARTESIAN_POINT('Ctrl Pts',(30.9977590788535,9.9921139470237,5.91460517397386));
#38609=CARTESIAN_POINT('Ctrl Pts',(30.9978069137501,9.99125424793223,5.91413817726242));
#38610=CARTESIAN_POINT('Ctrl Pts',(30.9981152685796,9.98842830684885,5.91260201951091));
#38611=CARTESIAN_POINT('Ctrl Pts',(30.998967089605,9.96926390369661,5.90207109306701));
#38612=CARTESIAN_POINT('Ctrl Pts',(30.999722710576,9.95345364685531,5.89343987431005));
#38613=CARTESIAN_POINT('Ctrl Pts',(30.9999328116104,9.93430898196904,5.88298760002662));
#38614=CARTESIAN_POINT('Ctrl Pts',(31.,9.93147133259584,5.88146680563563));
#38615=CARTESIAN_POINT('Ctrl Pts',(31.,9.93061113335113,5.88099707624835));
#38616=CARTESIAN_POINT('Ctrl Pts',(30.9967839176211,9.97611777866644,5.94380988748522));
#38617=CARTESIAN_POINT('Ctrl Pts',(30.9968735301548,9.97499741976691,5.94320281998623));
#38618=CARTESIAN_POINT('Ctrl Pts',(30.9972890729406,9.97058037138577,5.94081797664114));
#38619=CARTESIAN_POINT('Ctrl Pts',(30.9987938596804,9.94698239524001,5.92798568903476));
#38620=CARTESIAN_POINT('Ctrl Pts',(30.9996652543314,9.92505108832951,5.91596719818983));
#38621=CARTESIAN_POINT('Ctrl Pts',(31.0000630674513,9.90147073109231,5.90303515199838));
#38622=CARTESIAN_POINT('Ctrl Pts',(31.,9.89703879538735,5.90061245193096));
#38623=CARTESIAN_POINT('Ctrl Pts',(31.,9.89591670002669,5.9));
#38624=CARTESIAN_POINT('',(30.9997094013184,10.0241062837382,5.85619574695114));
#38625=CARTESIAN_POINT('Ctrl Pts',(31.,10.,5.84299122874504));
#38626=CARTESIAN_POINT('Ctrl Pts',(31.,10.0001511918942,5.84307405190661));
#38627=CARTESIAN_POINT('Ctrl Pts',(30.9999999772324,10.0003064637474,5.8431591096781));
#38628=CARTESIAN_POINT('Ctrl Pts',(30.999999861436,10.0005264293687,5.84327959945591));
#38629=CARTESIAN_POINT('Ctrl Pts',(30.9999997332202,10.0007699868055,5.84341301203768));
#38630=CARTESIAN_POINT('Ctrl Pts',(30.9999994934254,10.0010926374677,5.84358974299168));
#38631=CARTESIAN_POINT('Ctrl Pts',(30.9999988482408,10.001517734162,5.84382258165775));
#38632=CARTESIAN_POINT('Ctrl Pts',(30.9999981093085,10.0020045990926,5.84408925270587));
#38633=CARTESIAN_POINT('Ctrl Pts',(30.9999968157179,10.0026250445202,5.8444290830952));
#38634=CARTESIAN_POINT('Ctrl Pts',(30.9999943962796,10.0033477469247,5.84482491679361));
#38635=CARTESIAN_POINT('Ctrl Pts',(30.9999912614642,10.0042841372279,5.84533779019007));
#38636=CARTESIAN_POINT('Ctrl Pts',(30.9999861247826,10.0053880993547,5.84594243788284));
#38637=CARTESIAN_POINT('Ctrl Pts',(30.9999787442318,10.006520052495,5.84656241544142));
#38638=CARTESIAN_POINT('Ctrl Pts',(30.9999728168381,10.007429135317,5.84706032558318));
#38639=CARTESIAN_POINT('Ctrl Pts',(30.9999655108804,10.0083525487905,5.84756608417289));
#38640=CARTESIAN_POINT('Ctrl Pts',(30.9999573082866,10.0092402166771,5.84805226739278));
#38641=CARTESIAN_POINT('Ctrl Pts',(30.9999505378773,10.0099728964872,5.84845356233046));
#38642=CARTESIAN_POINT('Ctrl Pts',(30.9999431973787,10.010680793641,5.84884128535465));
#38643=CARTESIAN_POINT('Ctrl Pts',(30.999935340759,10.0113716446136,5.84921967705076));
#38644=CARTESIAN_POINT('Ctrl Pts',(30.9999270907856,10.0120970840919,5.84961701350323));
#38645=CARTESIAN_POINT('Ctrl Pts',(30.9999182331384,10.0128091746617,5.85000704445293));
#38646=CARTESIAN_POINT('Ctrl Pts',(30.9999082037282,10.0135493216438,5.85041245473004));
#38647=CARTESIAN_POINT('Ctrl Pts',(30.9998975951077,10.0143322129912,5.85084127793111));
#38648=CARTESIAN_POINT('Ctrl Pts',(30.999885633187,10.0151464182939,5.85128726641096));
#38649=CARTESIAN_POINT('Ctrl Pts',(30.9998723269432,10.0159790429398,5.85174335999862));
#38650=CARTESIAN_POINT('Ctrl Pts',(30.9998546101357,10.0170876541093,5.85235063297346));
#38651=CARTESIAN_POINT('Ctrl Pts',(30.9998344254974,10.0182268187928,5.85297467101968));
#38652=CARTESIAN_POINT('Ctrl Pts',(30.9998142545149,10.0192732059832,5.85354790811658));
#38653=CARTESIAN_POINT('Ctrl Pts',(30.9997978064791,10.020126462085,5.85401534316856));
#38654=CARTESIAN_POINT('Ctrl Pts',(30.9997815001227,10.0209137965484,5.85444668062929));
#38655=CARTESIAN_POINT('Ctrl Pts',(30.9997672737566,10.0215730926237,5.85480788085582));
#38656=CARTESIAN_POINT('Ctrl Pts',(30.9997549692658,10.0221433227436,5.85512028564048));
#38657=CARTESIAN_POINT('Ctrl Pts',(30.9997442782914,10.02261667411,5.85537962133272));
#38658=CARTESIAN_POINT('Ctrl Pts',(30.9997358041127,10.022985255601,5.85558155824545));
#38659=CARTESIAN_POINT('Ctrl Pts',(30.9997282393264,10.0233142833877,5.85576182463725));
#38660=CARTESIAN_POINT('Ctrl Pts',(30.9997224549186,10.023559497923,5.85589617331858));
#38661=CARTESIAN_POINT('Ctrl Pts',(30.9997178979514,10.0237513055548,5.85600126110009));
#38662=CARTESIAN_POINT('Ctrl Pts',(30.9997146623179,10.0238874968375,5.85607587773361));
#38663=CARTESIAN_POINT('Ctrl Pts',(30.9997120255593,10.0239974540913,5.85613612116171));
#38664=CARTESIAN_POINT('Ctrl Pts',(30.9997094013184,10.0241062837382,5.85619574695114));
#38665=CARTESIAN_POINT('',(30.9967839176211,9.97611777866644,5.94380988748522));
#38666=CARTESIAN_POINT('Ctrl Pts',(30.9967839176211,9.97611777866644,5.94380988748522));
#38667=CARTESIAN_POINT('Ctrl Pts',(30.9977590788535,9.9921139470237,5.91460517397386));
#38668=CARTESIAN_POINT('Ctrl Pts',(30.9987342400859,10.008110115381,5.8854004604625));
#38669=CARTESIAN_POINT('Ctrl Pts',(30.9997094013184,10.0241062837382,5.85619574695114));
#38670=CARTESIAN_POINT('Ctrl Pts',(30.9967839176211,9.97611777866644,5.94380988748522));
#38671=CARTESIAN_POINT('Ctrl Pts',(30.9968134018443,9.97574915933943,5.94361015076422));
#38672=CARTESIAN_POINT('Ctrl Pts',(30.9968430401383,9.97537653919476,5.94340822589068));
#38673=CARTESIAN_POINT('Ctrl Pts',(30.9968795901821,9.97491255559319,5.94315679475268));
#38674=CARTESIAN_POINT('Ctrl Pts',(30.9969180186502,9.97442472638109,5.94289244175932));
#38675=CARTESIAN_POINT('Ctrl Pts',(30.9969640726959,9.9738361687824,5.94257350817652));
#38676=CARTESIAN_POINT('Ctrl Pts',(30.9970210134522,9.9730962847434,5.94217247405404));
#38677=CARTESIAN_POINT('Ctrl Pts',(30.9970818661454,9.97230556928001,5.94174388813345));
#38678=CARTESIAN_POINT('Ctrl Pts',(30.9971551144017,9.97134239280946,5.94122173226927));
#38679=CARTESIAN_POINT('Ctrl Pts',(30.9972399797972,9.97019691789268,5.94060042376811));
#38680=CARTESIAN_POINT('Ctrl Pts',(30.9973346959385,9.96891848204248,5.93990699691933));
#38681=CARTESIAN_POINT('Ctrl Pts',(30.9974437767348,9.96741351252657,5.93909034512013));
#38682=CARTESIAN_POINT('Ctrl Pts',(30.9975614612863,9.96572428712655,5.93817298465127));
#38683=CARTESIAN_POINT('Ctrl Pts',(30.9977187535123,9.96346653944293,5.9369468791987));
#38684=CARTESIAN_POINT('Ctrl Pts',(30.997890960601,9.96088111561884,5.93554161766041));
#38685=CARTESIAN_POINT('Ctrl Pts',(30.9980605279584,9.95815419184684,5.93405762283485));
#38686=CARTESIAN_POINT('Ctrl Pts',(30.9982120464402,9.95571752386853,5.93273158552184));
#38687=CARTESIAN_POINT('Ctrl Pts',(30.9983611461551,9.95317295204375,5.93134545148876));
#38688=CARTESIAN_POINT('Ctrl Pts',(30.9984992420485,9.950650745604,5.92997002663428));
#38689=CARTESIAN_POINT('Ctrl Pts',(30.9986110968974,9.94860780998098,5.92885596063726));
#38690=CARTESIAN_POINT('Ctrl Pts',(30.9987158226232,9.94658040822982,5.92774940674337));
#38691=CARTESIAN_POINT('Ctrl Pts',(30.9988120790596,9.94460617109134,5.92667098438524));
#38692=CARTESIAN_POINT('Ctrl Pts',(30.9988996170218,9.94281075145494,5.92569024066385));
#38693=CARTESIAN_POINT('Ctrl Pts',(30.998980206257,9.94105976594183,5.9247330233031));
#38694=CARTESIAN_POINT('Ctrl Pts',(30.9990548712986,9.93934432696308,5.92379462024413));
#38695=CARTESIAN_POINT('Ctrl Pts',(30.9991509420324,9.937137089442,5.9225871867724));
#38696=CARTESIAN_POINT('Ctrl Pts',(30.9992374788123,9.9349874579584,5.92141023471798));
#38697=CARTESIAN_POINT('Ctrl Pts',(30.9993190367815,9.93278144537767,5.9202018370499));
#38698=CARTESIAN_POINT('Ctrl Pts',(30.9993837070938,9.93103221689773,5.91924365411179));
#38699=CARTESIAN_POINT('Ctrl Pts',(30.9994451550484,9.92924631016809,5.91826502154007));
#38700=CARTESIAN_POINT('Ctrl Pts',(30.9995030320591,9.92741401288569,5.91726075859807));
#38701=CARTESIAN_POINT('Ctrl Pts',(30.9995675372626,9.92537187720048,5.91614148542615));
#38702=CARTESIAN_POINT('Ctrl Pts',(30.9996274779878,9.92327267550311,5.91499067542366));
#38703=CARTESIAN_POINT('Ctrl Pts',(30.999680967104,9.92115893283402,5.91383177340819));
#38704=CARTESIAN_POINT('Ctrl Pts',(30.999755623503,9.91820871740275,5.91221425834385));
#38705=CARTESIAN_POINT('Ctrl Pts',(30.9998172298906,9.91523150762811,5.91058170643131));
#38706=CARTESIAN_POINT('Ctrl Pts',(30.9998634213129,9.91244064827058,5.90905143958214));
#38707=CARTESIAN_POINT('Ctrl Pts',(30.9999017108032,9.91012721913319,5.9077829543368));
#38708=CARTESIAN_POINT('Ctrl Pts',(30.9999295357067,9.90794663757022,5.90658739090527));
#38709=CARTESIAN_POINT('Ctrl Pts',(30.9999490418999,9.90601621618389,5.90552921905091));
#38710=CARTESIAN_POINT('Ctrl Pts',(30.9999649247195,9.90444438029831,5.90466760795109));
#38711=CARTESIAN_POINT('Ctrl Pts',(30.9999754075208,9.90303911622973,5.90389747901719));
#38712=CARTESIAN_POINT('Ctrl Pts',(30.9999825291478,9.9018346606426,5.90323762352747));
#38713=CARTESIAN_POINT('Ctrl Pts',(30.9999891676432,9.90071191538349,5.90262253266759));
#38714=CARTESIAN_POINT('Ctrl Pts',(30.9999929297512,9.89976424545327,5.90210358223555));
#38715=CARTESIAN_POINT('Ctrl Pts',(30.9999953191642,9.89898272703063,5.90167585189123));
#38716=CARTESIAN_POINT('Ctrl Pts',(30.9999975649231,9.8982481943387,5.90127383715666));
#38717=CARTESIAN_POINT('Ctrl Pts',(30.9999986059227,9.89766075970279,5.90095258053825));
#38718=CARTESIAN_POINT('Ctrl Pts',(30.999999215242,9.89717328034114,5.90068618816431));
#38719=CARTESIAN_POINT('Ctrl Pts',(30.9999998245612,9.89668580097949,5.90041979579038));
#38720=CARTESIAN_POINT('Ctrl Pts',(31.,9.89629895748635,5.90020864030589));
#38721=CARTESIAN_POINT('Ctrl Pts',(31.,9.89591670002669,5.9));
#38722=CARTESIAN_POINT('Ctrl Pts',(30.9967839176211,9.97611777866644,5.94380988748522));
#38723=CARTESIAN_POINT('Ctrl Pts',(30.9917066333316,10.0395952901576,5.97820523540357));
#38724=CARTESIAN_POINT('Ctrl Pts',(30.9741529037903,10.1426508202057,6.03285941899933));
#38725=CARTESIAN_POINT('Ctrl Pts',(30.9167083241675,10.3130060581232,6.11306762286303));
#38726=CARTESIAN_POINT('Ctrl Pts',(30.8426027988904,10.4638132796915,6.17352191726238));
#38727=CARTESIAN_POINT('Ctrl Pts',(30.7487057189956,10.5896778448846,6.20000000000012));
#38728=CARTESIAN_POINT('Ctrl Pts',(30.6999999999992,10.6423370590825,6.2));
#38729=CARTESIAN_POINT('Ctrl Pts',(30.9977590788535,9.9921139470237,5.91460517397386));
#38730=CARTESIAN_POINT('Ctrl Pts',(30.9938642295286,10.055582164711,5.94912303971441));
#38731=CARTESIAN_POINT('Ctrl Pts',(30.978201146713,10.1584856199577,6.00440333149542));
#38732=CARTESIAN_POINT('Ctrl Pts',(30.9236435535527,10.3281478102022,6.08691292609801));
#38733=CARTESIAN_POINT('Ctrl Pts',(30.8518449662238,10.4779872265877,6.15042656152703));
#38734=CARTESIAN_POINT('Ctrl Pts',(30.7594406852812,10.6026091261344,6.18071804878039));
#38735=CARTESIAN_POINT('Ctrl Pts',(30.7112855175703,10.6546595286716,6.18264100709771));
#38736=CARTESIAN_POINT('Ctrl Pts',(30.9987342400859,10.008110115381,5.8854004604625));
#38737=CARTESIAN_POINT('Ctrl Pts',(30.9960218257256,10.0715690392644,5.92004084402524));
#38738=CARTESIAN_POINT('Ctrl Pts',(30.9822493896356,10.1743204197098,5.97594724399151));
#38739=CARTESIAN_POINT('Ctrl Pts',(30.9305787829379,10.3432895622813,6.06075822933298));
#38740=CARTESIAN_POINT('Ctrl Pts',(30.8610871335572,10.4921611734839,6.12733120579168));
#38741=CARTESIAN_POINT('Ctrl Pts',(30.7701756515669,10.6155404073841,6.16143609756066));
#38742=CARTESIAN_POINT('Ctrl Pts',(30.7225710351414,10.6669819982608,6.16528201419542));
#38743=CARTESIAN_POINT('Ctrl Pts',(30.9997094013184,10.0241062837382,5.85619574695114));
#38744=CARTESIAN_POINT('Ctrl Pts',(30.9981794219226,10.0875559138178,5.89095864833608));
#38745=CARTESIAN_POINT('Ctrl Pts',(30.9862976325583,10.1901552194618,5.94749115648761));
#38746=CARTESIAN_POINT('Ctrl Pts',(30.937514012323,10.3584313143604,6.03460353256796));
#38747=CARTESIAN_POINT('Ctrl Pts',(30.8703293008906,10.5063351203802,6.10423585005633));
#38748=CARTESIAN_POINT('Ctrl Pts',(30.7809106178525,10.6284716886339,6.14215414634093));
#38749=CARTESIAN_POINT('Ctrl Pts',(30.7338565527125,10.6793044678499,6.14792302129313));
#38750=CARTESIAN_POINT('',(30.7338565527125,10.6793044678499,6.14792302129313));
#38751=CARTESIAN_POINT('Ctrl Pts',(30.9997094013184,10.0241062837382,5.85619574695114));
#38752=CARTESIAN_POINT('Ctrl Pts',(30.9981794219226,10.0875559138178,5.89095864833608));
#38753=CARTESIAN_POINT('Ctrl Pts',(30.9862976325583,10.1901552194618,5.94749115648761));
#38754=CARTESIAN_POINT('Ctrl Pts',(30.937514012323,10.3584313143604,6.03460353256796));
#38755=CARTESIAN_POINT('Ctrl Pts',(30.8703293008906,10.5063351203802,6.10423585005633));
#38756=CARTESIAN_POINT('Ctrl Pts',(30.7809106178525,10.6284716886339,6.14215414634093));
#38757=CARTESIAN_POINT('Ctrl Pts',(30.7338565527125,10.6793044678499,6.14792302129313));
#38758=CARTESIAN_POINT('',(30.7338565527125,10.6793044678499,6.14792302129313));
#38759=CARTESIAN_POINT('Ctrl Pts',(30.6999999999992,10.6423370590825,6.2));
#38760=CARTESIAN_POINT('Ctrl Pts',(30.7487057189956,10.5896778448846,6.20000000000012));
#38761=CARTESIAN_POINT('Ctrl Pts',(30.8426027988904,10.4638132796915,6.17352191726238));
#38762=CARTESIAN_POINT('Ctrl Pts',(30.9167083241675,10.3130060581232,6.11306762286303));
#38763=CARTESIAN_POINT('Ctrl Pts',(30.9741529037903,10.1426508202057,6.03285941899933));
#38764=CARTESIAN_POINT('Ctrl Pts',(30.9917066333316,10.0395952901576,5.97820523540357));
#38765=CARTESIAN_POINT('Ctrl Pts',(30.9967839176211,9.97611777866644,5.94380988748522));
#38766=CARTESIAN_POINT('Origin',(30.,10.,6.175));
#38767=CARTESIAN_POINT('',(30.,11.,6.15));
#38768=CARTESIAN_POINT('',(30.,11.,6.15));
#38769=CARTESIAN_POINT('',(30.7,10.7141428428543,6.15));
#38770=CARTESIAN_POINT('',(30.665,10.6784357007116,6.2));
#38771=CARTESIAN_POINT('Origin',(30.,10.,6.15));
#38772=CARTESIAN_POINT('Origin',(25.,10.975,6.175));
#38773=CARTESIAN_POINT('',(10.,11.,6.15));
#38774=CARTESIAN_POINT('',(10.,11.,6.15));
#38775=CARTESIAN_POINT('',(25.,11.,6.15));
#38776=CARTESIAN_POINT('Origin',(10.,10.,6.175));
#38777=CARTESIAN_POINT('',(9.,10.,6.15));
#38778=CARTESIAN_POINT('',(9.,10.,6.15));
#38779=CARTESIAN_POINT('Origin',(10.,10.,6.15));
#38780=CARTESIAN_POINT('Origin',(9.025,5.,6.175));
#38781=CARTESIAN_POINT('',(9.,-10.,6.15));
#38782=CARTESIAN_POINT('',(9.,-10.,6.15));
#38783=CARTESIAN_POINT('',(9.,5.,6.15));
#38784=CARTESIAN_POINT('Origin',(10.,-10.,6.175));
#38785=CARTESIAN_POINT('',(10.,-11.,6.15));
#38786=CARTESIAN_POINT('Origin',(10.,-10.,6.15));
#38787=CARTESIAN_POINT('Origin',(15.,-10.975,6.175));
#38788=CARTESIAN_POINT('',(30.,-11.,6.15));
#38789=CARTESIAN_POINT('Origin',(30.,-10.,6.175));
#38790=CARTESIAN_POINT('',(30.7,-10.7141428428543,6.15));
#38791=CARTESIAN_POINT('Ctrl Pts',(30.6999999999992,10.6423370590825,6.2));
#38792=CARTESIAN_POINT('Ctrl Pts',(30.6883703751711,10.6549106729719,6.2));
#38793=CARTESIAN_POINT('Ctrl Pts',(30.6767224654731,10.6669453862552,6.2));
#38794=CARTESIAN_POINT('Ctrl Pts',(30.665,10.6784357007116,6.2));
#38795=CARTESIAN_POINT('Ctrl Pts',(30.7112855175703,10.6546595286716,6.18264100709771));
#38796=CARTESIAN_POINT('Ctrl Pts',(30.6997873496846,10.6670877745971,6.18310015818412));
#38797=CARTESIAN_POINT('Ctrl Pts',(30.6882451720374,10.6789888760943,6.18333333333333));
#38798=CARTESIAN_POINT('Ctrl Pts',(30.6766666666667,10.6903380814258,6.18333333333333));
#38799=CARTESIAN_POINT('Ctrl Pts',(30.7225710351414,10.6669819982608,6.16528201419542));
#38800=CARTESIAN_POINT('Ctrl Pts',(30.7112043241981,10.6792648762223,6.16620031636824));
#38801=CARTESIAN_POINT('Ctrl Pts',(30.6997678786018,10.6910323659335,6.16666666666667));
#38802=CARTESIAN_POINT('Ctrl Pts',(30.6883333333333,10.70224046214,6.16666666666667));
#38803=CARTESIAN_POINT('Ctrl Pts',(30.7338565527125,10.6793044678499,6.14792302129313));
#38804=CARTESIAN_POINT('Ctrl Pts',(30.7226212987117,10.6914419778475,6.14930047455236));
#38805=CARTESIAN_POINT('Ctrl Pts',(30.7112905851662,10.7030758557726,6.15));
#38806=CARTESIAN_POINT('Ctrl Pts',(30.7,10.7141428428543,6.15));
#38807=CARTESIAN_POINT('Ctrl Pts',(30.7338565527125,10.6793044678499,6.14792302129313));
#38808=CARTESIAN_POINT('Ctrl Pts',(30.7226212987117,10.6914419778475,6.14930047455236));
#38809=CARTESIAN_POINT('Ctrl Pts',(30.7112905851662,10.7030758557726,6.15));
#38810=CARTESIAN_POINT('Ctrl Pts',(30.7,10.7141428428543,6.15));
#38811=CARTESIAN_POINT('Ctrl Pts',(30.6999999999992,-10.6423370590825,6.2));
#38812=CARTESIAN_POINT('Ctrl Pts',(30.7293995132925,-10.6105511559129,6.20000000000007));
#38813=CARTESIAN_POINT('Ctrl Pts',(30.7582382311623,-10.5755441820079,6.19560373930292));
#38814=CARTESIAN_POINT('Ctrl Pts',(30.8178826904194,-10.4935177749275,6.17800728102166));
#38815=CARTESIAN_POINT('Ctrl Pts',(30.8614297222427,-10.4226084466948,6.15570478058127));
#38816=CARTESIAN_POINT('Ctrl Pts',(30.9162763309817,-10.3099389124345,6.11112745456547));
#38817=CARTESIAN_POINT('Ctrl Pts',(30.9447582561879,-10.2331375716414,6.07591295728));
#38818=CARTESIAN_POINT('Ctrl Pts',(30.9792320402833,-10.1123553378356,6.01669471341596));
#38819=CARTESIAN_POINT('Ctrl Pts',(30.9915707246235,-10.0412944876546,5.97912594754713));
#38820=CARTESIAN_POINT('Ctrl Pts',(30.9967839207979,-9.97611773894901,5.94380986596425));
#38821=CARTESIAN_POINT('Ctrl Pts',(30.7112855175703,-10.6546595286716,6.18264100709771));
#38822=CARTESIAN_POINT('Ctrl Pts',(30.7403530419617,-10.6232428387308,6.1814758827751));
#38823=CARTESIAN_POINT('Ctrl Pts',(30.7688042988717,-10.5886067472929,6.17593248602285));
#38824=CARTESIAN_POINT('Ctrl Pts',(30.8274420633668,-10.5073652408122,6.15590971324675));
#38825=CARTESIAN_POINT('Ctrl Pts',(30.8700216323188,-10.437031263705,6.13182321060776));
#38826=CARTESIAN_POINT('Ctrl Pts',(30.9231458705104,-10.3250728058919,6.08499529598356));
#38827=CARTESIAN_POINT('Ctrl Pts',(30.9503483536313,-10.2486255880964,6.04862265724997));
#38828=CARTESIAN_POINT('Ctrl Pts',(30.9827269941712,-10.1282330114988,5.98806638775668));
#38829=CARTESIAN_POINT('Ctrl Pts',(30.9937578217055,-10.0572879383963,5.95003794609275));
#38830=CARTESIAN_POINT('Ctrl Pts',(30.9977590812902,-9.99211390732443,5.91460515238299));
#38831=CARTESIAN_POINT('Ctrl Pts',(30.7225710351414,-10.6669819982608,6.16528201419542));
#38832=CARTESIAN_POINT('Ctrl Pts',(30.7513055739305,-10.635929345816,6.16296495779396));
#38833=CARTESIAN_POINT('Ctrl Pts',(30.7793686753514,-10.6016729290708,6.15625008908845));
#38834=CARTESIAN_POINT('Ctrl Pts',(30.837003966094,-10.5212046804115,6.13383250447826));
#38835=CARTESIAN_POINT('Ctrl Pts',(30.878614593152,-10.45144908405,6.10795182991645));
#38836=CARTESIAN_POINT('Ctrl Pts',(30.9300172225282,-10.3402007573639,6.05887633762058));
#38837=CARTESIAN_POINT('Ctrl Pts',(30.955947099261,-10.2641021226664,6.02135776304424));
#38838=CARTESIAN_POINT('Ctrl Pts',(30.9862108563741,-10.1441174667834,5.95941345010241));
#38839=CARTESIAN_POINT('Ctrl Pts',(30.9959513738211,-10.0732608461654,5.92097716308504));
#38840=CARTESIAN_POINT('Ctrl Pts',(30.9987342417825,-10.0081100756998,5.88540043880173));
#38841=CARTESIAN_POINT('Ctrl Pts',(30.7338565527125,-10.6793044678499,6.14792302129313));
#38842=CARTESIAN_POINT('Ctrl Pts',(30.7622591025997,-10.6486210286339,6.14444084056899));
#38843=CARTESIAN_POINT('Ctrl Pts',(30.7899347430608,-10.6147354943559,6.13657883580837));
#38844=CARTESIAN_POINT('Ctrl Pts',(30.8465633390414,-10.5350521462962,6.11173493670335));
#38845=CARTESIAN_POINT('Ctrl Pts',(30.8872065032282,-10.4658719010602,6.08407025994295));
#38846=CARTESIAN_POINT('Ctrl Pts',(30.9368867620569,-10.3553346508213,6.03274417903868));
#38847=CARTESIAN_POINT('Ctrl Pts',(30.9615371967044,-10.2795901391215,5.99406746301422));
#38848=CARTESIAN_POINT('Ctrl Pts',(30.989705810262,-10.1599951404466,5.93078512444313));
#38849=CARTESIAN_POINT('Ctrl Pts',(30.9981384709031,-10.0892542969071,5.89188916163067));
#38850=CARTESIAN_POINT('Ctrl Pts',(30.9997094022748,-10.0241062440753,5.85619572522048));
#38851=CARTESIAN_POINT('Ctrl Pts',(30.9967839207979,-9.97611773894901,5.94380986596425));
#38852=CARTESIAN_POINT('Ctrl Pts',(30.9915707246235,-10.0412944876546,5.97912594754713));
#38853=CARTESIAN_POINT('Ctrl Pts',(30.9792320402833,-10.1123553378356,6.01669471341596));
#38854=CARTESIAN_POINT('Ctrl Pts',(30.9447582561879,-10.2331375716414,6.07591295728));
#38855=CARTESIAN_POINT('Ctrl Pts',(30.9162763309817,-10.3099389124345,6.11112745456547));
#38856=CARTESIAN_POINT('Ctrl Pts',(30.8614297222427,-10.4226084466948,6.15570478058127));
#38857=CARTESIAN_POINT('Ctrl Pts',(30.8178826904194,-10.4935177749275,6.17800728102166));
#38858=CARTESIAN_POINT('Ctrl Pts',(30.7582382311623,-10.5755441820079,6.19560373930292));
#38859=CARTESIAN_POINT('Ctrl Pts',(30.7293995132925,-10.6105511559129,6.20000000000007));
#38860=CARTESIAN_POINT('Ctrl Pts',(30.6999999999992,-10.6423370590825,6.2));
#38861=CARTESIAN_POINT('',(30.6999999999995,-10.6423370590827,6.2));
#38862=CARTESIAN_POINT('Ctrl Pts',(30.665,-10.6784357007116,6.2));
#38863=CARTESIAN_POINT('Ctrl Pts',(30.6767224654731,-10.6669453862552,6.2));
#38864=CARTESIAN_POINT('Ctrl Pts',(30.6883703751711,-10.6549106729719,6.2));
#38865=CARTESIAN_POINT('Ctrl Pts',(30.6999999999992,-10.6423370590825,6.2));
#38866=CARTESIAN_POINT('Ctrl Pts',(30.6766666666667,-10.6903380814258,6.18333333333333));
#38867=CARTESIAN_POINT('Ctrl Pts',(30.6882451720374,-10.6789888760944,6.18333333333333));
#38868=CARTESIAN_POINT('Ctrl Pts',(30.6997873496846,-10.6670877745971,6.18310015818412));
#38869=CARTESIAN_POINT('Ctrl Pts',(30.7112855175703,-10.6546595286716,6.18264100709771));
#38870=CARTESIAN_POINT('Ctrl Pts',(30.6883333333333,-10.70224046214,6.16666666666667));
#38871=CARTESIAN_POINT('Ctrl Pts',(30.6997678786018,-10.6910323659335,6.16666666666667));
#38872=CARTESIAN_POINT('Ctrl Pts',(30.7112043241981,-10.6792648762223,6.16620031636824));
#38873=CARTESIAN_POINT('Ctrl Pts',(30.7225710351414,-10.6669819982608,6.16528201419542));
#38874=CARTESIAN_POINT('Ctrl Pts',(30.7,-10.7141428428543,6.15));
#38875=CARTESIAN_POINT('Ctrl Pts',(30.7112905851662,-10.7030758557726,6.15));
#38876=CARTESIAN_POINT('Ctrl Pts',(30.7226212987117,-10.6914419778475,6.14930047455236));
#38877=CARTESIAN_POINT('Ctrl Pts',(30.7338565527125,-10.6793044678499,6.14792302129313));
#38878=CARTESIAN_POINT('Origin',(30.7,0.,5.9));
#38879=CARTESIAN_POINT('Origin',(30.7,-7.76915840380663,5.9));
#38880=CARTESIAN_POINT('Origin',(10.,-10.,4.2));
#38881=CARTESIAN_POINT('',(9.,-10.,4.2));
#38882=CARTESIAN_POINT('Origin',(9.,10.,4.2));
#38883=CARTESIAN_POINT('',(9.,10.,4.2));
#38884=CARTESIAN_POINT('Origin',(10.,10.,4.2));
#38885=CARTESIAN_POINT('',(10.,11.,4.2));
#38886=CARTESIAN_POINT('Origin',(30.,11.,4.2));
#38887=CARTESIAN_POINT('',(30.,11.,4.2));
#38888=CARTESIAN_POINT('Origin',(10.025,-4.525,10.35));
#38889=CARTESIAN_POINT('',(10.05,-4.5,8.95830089865305));
#38890=CARTESIAN_POINT('',(10.05,-4.5,10.35));
#38891=CARTESIAN_POINT('',(10.,-4.55,8.96086067249887));
#38892=CARTESIAN_POINT('',(10.,-4.55,10.35));
#38893=CARTESIAN_POINT('Ctrl Pts',(10.,-4.55,8.96086067249887));
#38894=CARTESIAN_POINT('Ctrl Pts',(10.0166666720695,-4.53333332793054,8.96000796626512));
#38895=CARTESIAN_POINT('Ctrl Pts',(10.0333333561696,-4.51666664383039,8.95915470813818));
#38896=CARTESIAN_POINT('Ctrl Pts',(10.05,-4.5,8.95830089865305));
#38897=CARTESIAN_POINT('Origin',(29.2841674687199,-4.525,6.98243503368624));
#38898=CARTESIAN_POINT('',(11.2135541721682,-4.55,14.));
#38899=CARTESIAN_POINT('Origin',(29.2841674687199,-4.55,6.98243503368624));
#38900=CARTESIAN_POINT('',(11.2601630224385,-4.5,13.9818998597663));
#38901=CARTESIAN_POINT('',(11.2135541721682,-4.55,14.));
#38902=CARTESIAN_POINT('Origin',(29.2841674687199,-4.5,6.98243503368624));
#38903=CARTESIAN_POINT('Ctrl Pts',(11.2672025025441,-4.5,14.));
#38904=CARTESIAN_POINT('Ctrl Pts',(11.391959999534,-4.5,14.3203062297749));
#38905=CARTESIAN_POINT('Ctrl Pts',(11.668054446774,-4.4303581677262,14.9774819072439));
#38906=CARTESIAN_POINT('Ctrl Pts',(12.1316598081387,-4.10683395243209,15.9286468865022));
#38907=CARTESIAN_POINT('Ctrl Pts',(12.524997260418,-3.67159465412862,16.6376752255481));
#38908=CARTESIAN_POINT('Ctrl Pts',(12.8177228984641,-3.24811960222038,17.1263128398011));
#38909=CARTESIAN_POINT('Ctrl Pts',(13.0898330833522,-2.78494101931705,17.5607918840079));
#38910=CARTESIAN_POINT('Ctrl Pts',(13.4127915844491,-2.06816050302593,18.0433746309751));
#38911=CARTESIAN_POINT('Ctrl Pts',(13.6504781966751,-1.17371806751399,18.3757567399041));
#38912=CARTESIAN_POINT('Ctrl Pts',(13.7448250712003,-0.34677769024255,18.5049230225636));
#38913=CARTESIAN_POINT('Ctrl Pts',(13.7445858103348,0.346816939957277,18.5045458836767));
#38914=CARTESIAN_POINT('Ctrl Pts',(13.6373623529499,1.29192272955491,18.3578766190094));
#38915=CARTESIAN_POINT('Ctrl Pts',(13.3722017145503,2.17594495900127,17.9861325476814));
#38916=CARTESIAN_POINT('Ctrl Pts',(13.0443130403164,2.86199680217774,17.4880641812068));
#38917=CARTESIAN_POINT('Ctrl Pts',(12.8178440847237,3.24806162865946,17.1265367900342));
#38918=CARTESIAN_POINT('Ctrl Pts',(12.5249752388355,3.67157303457683,16.6376360062934));
#38919=CARTESIAN_POINT('Ctrl Pts',(12.1317232805211,4.10675982821366,15.928729275166));
#38920=CARTESIAN_POINT('Ctrl Pts',(11.6680306338885,4.43037992268562,14.9774496711636));
#38921=CARTESIAN_POINT('Ctrl Pts',(11.391959999534,4.5,14.3203062297749));
#38922=CARTESIAN_POINT('Ctrl Pts',(11.2672025025441,4.5,14.));
#38923=CARTESIAN_POINT('Ctrl Pts',(11.2516950047624,-4.51665435240168,14.006107294649));
#38924=CARTESIAN_POINT('Ctrl Pts',(11.3769625715924,-4.51621852393914,14.3277191173693));
#38925=CARTESIAN_POINT('Ctrl Pts',(11.6541843464077,-4.44533549720252,14.9873034081241));
#38926=CARTESIAN_POINT('Ctrl Pts',(12.119584202532,-4.119207886609,15.9409930517025));
#38927=CARTESIAN_POINT('Ctrl Pts',(12.5143327076105,-3.68158280890167,16.6511544706723));
#38928=CARTESIAN_POINT('Ctrl Pts',(12.8080550666115,-3.25627951505913,17.1402234548367));
#38929=CARTESIAN_POINT('Ctrl Pts',(13.0810645349093,-2.79136044400086,17.5748911978179));
#38930=CARTESIAN_POINT('Ctrl Pts',(13.405044673385,-2.07240378878844,18.0573316981621));
#38931=CARTESIAN_POINT('Ctrl Pts',(13.6434562871566,-1.17593865460604,18.3893328785638));
#38932=CARTESIAN_POINT('Ctrl Pts',(13.7380888018818,-0.347413383593392,
18.5183095858136));
#38933=CARTESIAN_POINT('Ctrl Pts',(13.7378488054313,0.347453340477631,18.5179320837059));
#38934=CARTESIAN_POINT('Ctrl Pts',(13.6303006408794,1.29436558132429,18.3714809661723));
#38935=CARTESIAN_POINT('Ctrl Pts',(13.364330921006,2.18046915754007,18.0001463863418));
#38936=CARTESIAN_POINT('Ctrl Pts',(13.035394038305,2.86870807689454,17.5021311417631));
#38937=CARTESIAN_POINT('Ctrl Pts',(12.8081766935965,3.25622047982334,17.1404479014005));
#38938=CARTESIAN_POINT('Ctrl Pts',(12.5143106100714,3.68156157484352,16.6511151239475));
#38939=CARTESIAN_POINT('Ctrl Pts',(12.1196478076241,4.11913346993114,15.9410753393783));
#38940=CARTESIAN_POINT('Ctrl Pts',(11.6541604800616,4.44535739714532,14.9872711896631));
#38941=CARTESIAN_POINT('Ctrl Pts',(11.3769625715924,4.51621852393914,14.3277191173693));
#38942=CARTESIAN_POINT('Ctrl Pts',(11.2516950047624,4.51665435240168,14.0061072946491));
#38943=CARTESIAN_POINT('Ctrl Pts',(11.2361875069806,-4.53330870480335,14.0122145892981));
#38944=CARTESIAN_POINT('Ctrl Pts',(11.3619651436507,-4.53243704787828,14.3351320049637));
#38945=CARTESIAN_POINT('Ctrl Pts',(11.6403142460414,-4.46031282667885,14.9971249090043));
#38946=CARTESIAN_POINT('Ctrl Pts',(12.1075085969253,-4.1315818207859,15.9533392169029));
#38947=CARTESIAN_POINT('Ctrl Pts',(12.503668154803,-3.69157096367473,16.6646337157966));
#38948=CARTESIAN_POINT('Ctrl Pts',(12.798387234759,-3.26443942789788,17.1541340698723));
#38949=CARTESIAN_POINT('Ctrl Pts',(13.0722959864663,-2.79777986868466,17.588990511628));
#38950=CARTESIAN_POINT('Ctrl Pts',(13.3972977623209,-2.07664707455095,18.071288765349));
#38951=CARTESIAN_POINT('Ctrl Pts',(13.6364343776382,-1.1781592416981,18.4029090172236));
#38952=CARTESIAN_POINT('Ctrl Pts',(13.7313525325633,-0.348049076944234,
18.5316961490636));
#38953=CARTESIAN_POINT('Ctrl Pts',(13.7311118005278,0.348089740997986,18.5313182837351));
#38954=CARTESIAN_POINT('Ctrl Pts',(13.6232389288088,1.29680843309367,18.3850853133351));
#38955=CARTESIAN_POINT('Ctrl Pts',(13.3564601274617,2.18499335607887,18.0141602250022));
#38956=CARTESIAN_POINT('Ctrl Pts',(13.0264750362935,2.87541935161135,17.5161981023194));
#38957=CARTESIAN_POINT('Ctrl Pts',(12.7985093024693,3.26437933098722,17.1543590127667));
#38958=CARTESIAN_POINT('Ctrl Pts',(12.5036459813074,3.6915501151102,16.6645942416017));
#38959=CARTESIAN_POINT('Ctrl Pts',(12.1075723347271,4.13150711164862,15.9534214035907));
#38960=CARTESIAN_POINT('Ctrl Pts',(11.6402903262347,4.46033487160503,14.9970927081627));
#38961=CARTESIAN_POINT('Ctrl Pts',(11.3619651436507,4.53243704787828,14.3351320049637));
#38962=CARTESIAN_POINT('Ctrl Pts',(11.2361875069806,4.53330870480335,14.0122145892981));
#38963=CARTESIAN_POINT('Ctrl Pts',(11.2206800091989,-4.54996305720503,14.0183218839471));
#38964=CARTESIAN_POINT('Ctrl Pts',(11.346967715709,-4.54865557181743,14.342544892558));
#38965=CARTESIAN_POINT('Ctrl Pts',(11.6264441456752,-4.47529015615518,15.0069464098845));
#38966=CARTESIAN_POINT('Ctrl Pts',(12.0954329913186,-4.14395575496281,15.9656853821032));
#38967=CARTESIAN_POINT('Ctrl Pts',(12.4930036019956,-3.70155911844778,16.6781129609208));
#38968=CARTESIAN_POINT('Ctrl Pts',(12.7887194029065,-3.27259934073663,17.1680446849079));
#38969=CARTESIAN_POINT('Ctrl Pts',(13.0635274380233,-2.80419929336847,17.6030898254381));
#38970=CARTESIAN_POINT('Ctrl Pts',(13.3895508512568,-2.08089036031346,18.0852458325359));
#38971=CARTESIAN_POINT('Ctrl Pts',(13.6294124681197,-1.18037982879015,18.4164851558833));
#38972=CARTESIAN_POINT('Ctrl Pts',(13.7246162632449,-0.348684770295076,
18.5450827123137));
#38973=CARTESIAN_POINT('Ctrl Pts',(13.7243747956243,0.34872614151834,18.5447044837643));
#38974=CARTESIAN_POINT('Ctrl Pts',(13.6161772167383,1.29925128486305,18.3986896604979));
#38975=CARTESIAN_POINT('Ctrl Pts',(13.3485893339173,2.18951755461767,18.0281740636625));
#38976=CARTESIAN_POINT('Ctrl Pts',(13.017556034282,2.88213062632815,17.5302650628756));
#38977=CARTESIAN_POINT('Ctrl Pts',(12.7888419113421,3.2725381821511,17.168270124133));
#38978=CARTESIAN_POINT('Ctrl Pts',(12.4929813525433,3.70153865537689,16.6780733592558));
#38979=CARTESIAN_POINT('Ctrl Pts',(12.0954968618301,4.14388075336609,15.965767467803));
#38980=CARTESIAN_POINT('Ctrl Pts',(11.6264201724079,4.47531234606473,15.0069142266622));
#38981=CARTESIAN_POINT('Ctrl Pts',(11.3469677157091,4.54865557181743,14.342544892558));
#38982=CARTESIAN_POINT('Ctrl Pts',(11.2206800091989,4.54996305720503,14.0183218839471));
#38983=CARTESIAN_POINT('',(11.2672025025441,-4.5,14.));
#38984=CARTESIAN_POINT('',(11.2206800091989,-4.54996305720503,14.0183218839471));
#38985=CARTESIAN_POINT('',(11.2672025025441,-4.5,14.));
#38986=CARTESIAN_POINT('',(11.2206800091989,4.54996305720503,14.0183218839471));
#38987=CARTESIAN_POINT('Ctrl Pts',(11.2206800091989,-4.54996305720503,14.0183218839471));
#38988=CARTESIAN_POINT('Ctrl Pts',(11.346967715709,-4.54865557181743,14.342544892558));
#38989=CARTESIAN_POINT('Ctrl Pts',(11.6264441456752,-4.47529015615518,15.0069464098845));
#38990=CARTESIAN_POINT('Ctrl Pts',(12.0954329913186,-4.14395575496281,15.9656853821032));
#38991=CARTESIAN_POINT('Ctrl Pts',(12.4930036019956,-3.70155911844778,16.6781129609208));
#38992=CARTESIAN_POINT('Ctrl Pts',(12.7887194029065,-3.27259934073663,17.1680446849079));
#38993=CARTESIAN_POINT('Ctrl Pts',(13.0635274380233,-2.80419929336847,17.6030898254381));
#38994=CARTESIAN_POINT('Ctrl Pts',(13.3895508512568,-2.08089036031346,18.0852458325359));
#38995=CARTESIAN_POINT('Ctrl Pts',(13.6294124681197,-1.18037982879015,18.4164851558833));
#38996=CARTESIAN_POINT('Ctrl Pts',(13.7246162632449,-0.348684770295076,
18.5450827123137));
#38997=CARTESIAN_POINT('Ctrl Pts',(13.7243747956243,0.34872614151834,18.5447044837643));
#38998=CARTESIAN_POINT('Ctrl Pts',(13.6161772167383,1.29925128486305,18.3986896604979));
#38999=CARTESIAN_POINT('Ctrl Pts',(13.3485893339173,2.18951755461767,18.0281740636625));
#39000=CARTESIAN_POINT('Ctrl Pts',(13.017556034282,2.88213062632815,17.5302650628756));
#39001=CARTESIAN_POINT('Ctrl Pts',(12.7888419113421,3.2725381821511,17.168270124133));
#39002=CARTESIAN_POINT('Ctrl Pts',(12.4929813525433,3.70153865537689,16.6780733592558));
#39003=CARTESIAN_POINT('Ctrl Pts',(12.0954968618301,4.14388075336609,15.965767467803));
#39004=CARTESIAN_POINT('Ctrl Pts',(11.6264201724079,4.47531234606473,15.0069142266622));
#39005=CARTESIAN_POINT('Ctrl Pts',(11.3469677157091,4.54865557181743,14.342544892558));
#39006=CARTESIAN_POINT('Ctrl Pts',(11.2206800091989,4.54996305720503,14.0183218839471));
#39007=CARTESIAN_POINT('',(11.2672025025441,4.5,14.));
#39008=CARTESIAN_POINT('',(11.2206800091989,4.54996305720503,14.0183218839471));
#39009=CARTESIAN_POINT('Ctrl Pts',(11.2672025025441,4.5,14.));
#39010=CARTESIAN_POINT('Ctrl Pts',(11.391959999534,4.5,14.3203062297749));
#39011=CARTESIAN_POINT('Ctrl Pts',(11.6680306338885,4.43037992268562,14.9774496711636));
#39012=CARTESIAN_POINT('Ctrl Pts',(12.1317232805211,4.10675982821366,15.928729275166));
#39013=CARTESIAN_POINT('Ctrl Pts',(12.5249752388355,3.67157303457683,16.6376360062934));
#39014=CARTESIAN_POINT('Ctrl Pts',(12.8178440847237,3.24806162865946,17.1265367900342));
#39015=CARTESIAN_POINT('Ctrl Pts',(13.0443130403164,2.86199680217774,17.4880641812068));
#39016=CARTESIAN_POINT('Ctrl Pts',(13.3722017145503,2.17594495900127,17.9861325476814));
#39017=CARTESIAN_POINT('Ctrl Pts',(13.6373623529499,1.29192272955491,18.3578766190094));
#39018=CARTESIAN_POINT('Ctrl Pts',(13.7445858103348,0.346816939957277,18.5045458836767));
#39019=CARTESIAN_POINT('Ctrl Pts',(13.7448250712003,-0.34677769024255,18.5049230225636));
#39020=CARTESIAN_POINT('Ctrl Pts',(13.6504781966751,-1.17371806751399,18.3757567399041));
#39021=CARTESIAN_POINT('Ctrl Pts',(13.4127915844491,-2.06816050302593,18.0433746309751));
#39022=CARTESIAN_POINT('Ctrl Pts',(13.0898330833522,-2.78494101931705,17.5607918840079));
#39023=CARTESIAN_POINT('Ctrl Pts',(12.8177228984641,-3.24811960222038,17.1263128398011));
#39024=CARTESIAN_POINT('Ctrl Pts',(12.524997260418,-3.67159465412862,16.6376752255481));
#39025=CARTESIAN_POINT('Ctrl Pts',(12.1316598081387,-4.10683395243209,15.9286468865022));
#39026=CARTESIAN_POINT('Ctrl Pts',(11.668054446774,-4.4303581677262,14.9774819072439));
#39027=CARTESIAN_POINT('Ctrl Pts',(11.391959999534,-4.5,14.3203062297749));
#39028=CARTESIAN_POINT('Ctrl Pts',(11.2672025025441,-4.5,14.));
#39029=CARTESIAN_POINT('Ctrl Pts',(11.2601630224385,-4.5,13.9818998597663));
#39030=CARTESIAN_POINT('Ctrl Pts',(11.2625048863574,-4.5,13.9879302873398));
#39031=CARTESIAN_POINT('Ctrl Pts',(11.2648513789474,-4.5,13.9939636530615));
#39032=CARTESIAN_POINT('Ctrl Pts',(11.2672025025441,-4.5,14.));
#39033=CARTESIAN_POINT('Ctrl Pts',(11.244626739015,-4.51666666666667,13.9879332398442));
#39034=CARTESIAN_POINT('Ctrl Pts',(11.2469781779907,-4.51666666666667,13.9939883237121));
#39035=CARTESIAN_POINT('Ctrl Pts',(11.2493342686192,-4.51666256582858,14.000046343094));
#39036=CARTESIAN_POINT('Ctrl Pts',(11.2516950047624,-4.51665435240168,14.006107294649));
#39037=CARTESIAN_POINT('Ctrl Pts',(11.2290904555916,-4.53333333333333,13.9939666199221));
#39038=CARTESIAN_POINT('Ctrl Pts',(11.2314514696241,-4.53333333333333,14.0000463600845));
#39039=CARTESIAN_POINT('Ctrl Pts',(11.233817158291,-4.53332513165716,14.0061290331264));
#39040=CARTESIAN_POINT('Ctrl Pts',(11.2361875069806,-4.53330870480335,14.0122145892981));
#39041=CARTESIAN_POINT('Ctrl Pts',(11.2135541721682,-4.55,14.));
#39042=CARTESIAN_POINT('Ctrl Pts',(11.2159247612574,-4.55,14.0061043964569));
#39043=CARTESIAN_POINT('Ctrl Pts',(11.2183000479628,-4.54998769748575,14.0122117231589));
#39044=CARTESIAN_POINT('Ctrl Pts',(11.2206800091989,-4.54996305720503,14.0183218839471));
#39045=CARTESIAN_POINT('Ctrl Pts',(11.2672025025441,-4.5,14.));
#39046=CARTESIAN_POINT('Ctrl Pts',(11.2648513789474,-4.5,13.9939636530615));
#39047=CARTESIAN_POINT('Ctrl Pts',(11.2625048863574,-4.5,13.9879302873398));
#39048=CARTESIAN_POINT('Ctrl Pts',(11.2601630224385,-4.5,13.9818998597663));
#39049=CARTESIAN_POINT('Ctrl Pts',(11.2135541721682,-4.55,14.));
#39050=CARTESIAN_POINT('Ctrl Pts',(11.2159247612574,-4.55,14.0061043964569));
#39051=CARTESIAN_POINT('Ctrl Pts',(11.2183000479628,-4.54998769748575,14.0122117231589));
#39052=CARTESIAN_POINT('Ctrl Pts',(11.2206800091989,-4.54996305720503,14.0183218839471));
#39053=CARTESIAN_POINT('Ctrl Pts',(11.2672025025441,4.5,14.));
#39054=CARTESIAN_POINT('Ctrl Pts',(11.2648513789474,4.5,13.9939636530615));
#39055=CARTESIAN_POINT('Ctrl Pts',(11.2625048863574,4.5,13.9879302873398));
#39056=CARTESIAN_POINT('Ctrl Pts',(11.2601630224385,4.5,13.9818998597663));
#39057=CARTESIAN_POINT('Ctrl Pts',(11.2516950047624,4.51665435240168,14.0061072946491));
#39058=CARTESIAN_POINT('Ctrl Pts',(11.2493342686192,4.51666256582858,14.000046343094));
#39059=CARTESIAN_POINT('Ctrl Pts',(11.2469781779907,4.51666666666667,13.9939883237121));
#39060=CARTESIAN_POINT('Ctrl Pts',(11.244626739015,4.51666666666667,13.9879332398442));
#39061=CARTESIAN_POINT('Ctrl Pts',(11.2361875069806,4.53330870480335,14.0122145892981));
#39062=CARTESIAN_POINT('Ctrl Pts',(11.233817158291,4.53332513165716,14.0061290331264));
#39063=CARTESIAN_POINT('Ctrl Pts',(11.2314514696241,4.53333333333333,14.0000463600845));
#39064=CARTESIAN_POINT('Ctrl Pts',(11.2290904555916,4.53333333333333,13.9939666199221));
#39065=CARTESIAN_POINT('Ctrl Pts',(11.2206800091989,4.54996305720503,14.0183218839471));
#39066=CARTESIAN_POINT('Ctrl Pts',(11.2183000479628,4.54998769748575,14.0122117231589));
#39067=CARTESIAN_POINT('Ctrl Pts',(11.2159247612574,4.55,14.0061043964569));
#39068=CARTESIAN_POINT('Ctrl Pts',(11.2135541721682,4.55,14.));
#39069=CARTESIAN_POINT('Ctrl Pts',(11.2601630224385,4.5,13.9818998597663));
#39070=CARTESIAN_POINT('Ctrl Pts',(11.2625048863574,4.5,13.9879302873398));
#39071=CARTESIAN_POINT('Ctrl Pts',(11.2648513789474,4.5,13.9939636530615));
#39072=CARTESIAN_POINT('Ctrl Pts',(11.2672025025441,4.5,14.));
#39073=CARTESIAN_POINT('Ctrl Pts',(11.2206800091989,4.54996305720503,14.0183218839471));
#39074=CARTESIAN_POINT('Ctrl Pts',(11.2183000479628,4.54998769748575,14.0122117231589));
#39075=CARTESIAN_POINT('Ctrl Pts',(11.2159247612574,4.55,14.0061043964569));
#39076=CARTESIAN_POINT('Ctrl Pts',(11.2135541721682,4.55,14.));
#39077=CARTESIAN_POINT('Origin',(10.,-4.5,6.2));
#39078=CARTESIAN_POINT('',(30.7,-4.5,14.));
#39079=CARTESIAN_POINT('',(10.,-4.5,14.));
#39080=CARTESIAN_POINT('',(30.7,-4.5,10.35));
#39081=CARTESIAN_POINT('Origin',(10.,0.,14.));
#39082=CARTESIAN_POINT('',(30.7,4.5,14.));
#39083=CARTESIAN_POINT('',(10.,4.5,14.));
#39084=CARTESIAN_POINT('Origin',(30.7,0.,14.));
#39085=CARTESIAN_POINT('Origin',(10.,4.5,14.));
#39086=CARTESIAN_POINT('',(30.7,4.5,14.25));
#39087=CARTESIAN_POINT('Origin',(10.025,-4.48546421904046,19.3618097929987));
#39088=CARTESIAN_POINT('',(10.,-7.21647899346606,8.96086067249887));
#39089=CARTESIAN_POINT('',(10.,-4.46129870798463,19.3554044768152));
#39090=CARTESIAN_POINT('',(10.05,-7.26883964150479,8.95846862523193));
#39091=CARTESIAN_POINT('',(10.05,-4.5096297300963,19.3682151091821));
#39092=CARTESIAN_POINT('',(10.0000172096761,-7.21645233550652,8.96102841378919));
#39093=CARTESIAN_POINT('Ctrl Pts',(10.0499999997418,-7.26883964123718,8.95846862523692));
#39094=CARTESIAN_POINT('Ctrl Pts',(10.041668961232,-7.26010965815917,8.95888836093242));
#39095=CARTESIAN_POINT('Ctrl Pts',(10.0333384789044,-7.25137933806241,8.95931153454445));
#39096=CARTESIAN_POINT('Ctrl Pts',(10.0250085549945,-7.24264868518276,8.95973813882635));
#39097=CARTESIAN_POINT('Ctrl Pts',(10.0166689007691,-7.23390783388976,8.96016524143145));
#39098=CARTESIAN_POINT('Ctrl Pts',(10.0083297538089,-7.22516658949489,8.96059579976206));
#39099=CARTESIAN_POINT('Ctrl Pts',(10.0000172232168,-7.21645233580055,8.96102841200166));
#39100=CARTESIAN_POINT('Origin',(29.2841674687199,-27.6909737118631,6.98243503368624));
#39101=CARTESIAN_POINT('Ctrl Pts',(17.652334347801,-3.69831792998691,22.4290732641403));
#39102=CARTESIAN_POINT('Ctrl Pts',(16.7444852861922,-3.87955529520026,21.7453141135627));
#39103=CARTESIAN_POINT('Ctrl Pts',(15.0497308464295,-4.28458970814565,20.2172297374505));
#39104=CARTESIAN_POINT('Ctrl Pts',(12.715241047622,-5.08051171703884,17.2144330675353));
#39105=CARTESIAN_POINT('Ctrl Pts',(10.8707604156826,-6.07967020878362,13.4448805759527));
#39106=CARTESIAN_POINT('Ctrl Pts',(10.204866996482,-6.8692113042336,10.4661573522096));
#39107=CARTESIAN_POINT('Ctrl Pts',(10.05,-7.26883964150479,8.95846862523193));
#39108=CARTESIAN_POINT('Ctrl Pts',(17.6399944278817,-3.67849079088921,22.4402019872628));
#39109=CARTESIAN_POINT('Ctrl Pts',(16.7312990590247,-3.85991565088488,21.7556121939904));
#39110=CARTESIAN_POINT('Ctrl Pts',(15.0350589231358,-4.26536148427094,20.225717321171));
#39111=CARTESIAN_POINT('Ctrl Pts',(12.6988460476652,-5.06205511383136,17.2195925305481));
#39112=CARTESIAN_POINT('Ctrl Pts',(10.8534507340507,-6.06212749181112,13.4462167968078));
#39113=CARTESIAN_POINT('Ctrl Pts',(10.1876458579098,-6.85234295886588,10.4648029623686));
#39114=CARTESIAN_POINT('Ctrl Pts',(10.0329820767251,-7.25230186474275,8.95583316773031));
#39115=CARTESIAN_POINT('Ctrl Pts',(17.6276545079625,-3.65866365179151,22.4513307103853));
#39116=CARTESIAN_POINT('Ctrl Pts',(16.7181128318572,-3.8402760065695,21.7659102744182));
#39117=CARTESIAN_POINT('Ctrl Pts',(15.0203869998421,-4.24613326039624,20.2342049048915));
#39118=CARTESIAN_POINT('Ctrl Pts',(12.6824510477084,-5.04359851062388,17.2247519935608));
#39119=CARTESIAN_POINT('Ctrl Pts',(10.8361410524188,-6.04458477483863,13.4475530176629));
#39120=CARTESIAN_POINT('Ctrl Pts',(10.1704247193375,-6.83547461349816,10.4634485725276));
#39121=CARTESIAN_POINT('Ctrl Pts',(10.0159641534501,-7.23576408798071,8.95319771022869));
#39122=CARTESIAN_POINT('Ctrl Pts',(17.6153145880432,-3.63883651269381,22.4624594335078));
#39123=CARTESIAN_POINT('Ctrl Pts',(16.7049266046897,-3.82063636225412,21.776208354846));
#39124=CARTESIAN_POINT('Ctrl Pts',(15.0057150765484,-4.22690503652154,20.242692488612));
#39125=CARTESIAN_POINT('Ctrl Pts',(12.6660560477516,-5.02514190741641,17.2299114565736));
#39126=CARTESIAN_POINT('Ctrl Pts',(10.8188313707869,-6.02704205786613,13.448889238518));
#39127=CARTESIAN_POINT('Ctrl Pts',(10.1532035807653,-6.81860626813044,10.4620941826865));
#39128=CARTESIAN_POINT('Ctrl Pts',(9.99894623017517,-7.21922631121867,8.95056225272706));
#39129=CARTESIAN_POINT('Ctrl Pts',(10.05,-7.26883964150479,8.95846862523193));
#39130=CARTESIAN_POINT('Ctrl Pts',(10.204866996482,-6.8692113042336,10.4661573522096));
#39131=CARTESIAN_POINT('Ctrl Pts',(10.8707604156826,-6.07967020878362,13.4448805759527));
#39132=CARTESIAN_POINT('Ctrl Pts',(12.715241047622,-5.08051171703884,17.2144330675353));
#39133=CARTESIAN_POINT('Ctrl Pts',(15.0497308464295,-4.28458970814565,20.2172297374505));
#39134=CARTESIAN_POINT('Ctrl Pts',(16.7444852861922,-3.87955529520026,21.7453141135627));
#39135=CARTESIAN_POINT('Ctrl Pts',(17.652334347801,-3.69831792998691,22.4290732641403));
#39136=CARTESIAN_POINT('Ctrl Pts',(17.5228110256662,-3.65742470091966,22.3922935453347));
#39137=CARTESIAN_POINT('Ctrl Pts',(16.6473289621003,-3.83444881028949,21.7240714551034));
#39138=CARTESIAN_POINT('Ctrl Pts',(14.9818879132372,-4.23503430666294,20.2120102290229));
#39139=CARTESIAN_POINT('Ctrl Pts',(12.6660560477516,-5.02514190741641,17.2299114565736));
#39140=CARTESIAN_POINT('Ctrl Pts',(10.8203817853331,-6.02620114198486,13.4520627300372));
#39141=CARTESIAN_POINT('Ctrl Pts',(10.1547408409013,-6.81677931654233,10.4689877869414));
#39142=CARTESIAN_POINT('Ctrl Pts',(10.0000172232168,-7.21645233580054,8.96102841200167));
#39143=CARTESIAN_POINT('Origin',(10.,0.,14.5));
#39144=CARTESIAN_POINT('',(10.,0.,8.96086067249887));
#39145=CARTESIAN_POINT('Origin',(29.2841674687199,0.,6.98243503368624));
#39146=CARTESIAN_POINT('',(10.0000172098585,7.21645233533023,8.96102841374249));
#39147=CARTESIAN_POINT('Ctrl Pts',(10.0000172182924,7.21645233578529,8.96102841204531));
#39148=CARTESIAN_POINT('Ctrl Pts',(10.1159693818364,6.91692872721562,10.0911257931426));
#39149=CARTESIAN_POINT('Ctrl Pts',(10.5478144953569,6.32240188608982,12.3343975511604));
#39150=CARTESIAN_POINT('Ctrl Pts',(11.9121133386251,5.37960601026696,15.8921642658605));
#39151=CARTESIAN_POINT('Ctrl Pts',(14.169114976772,4.45071152571792,19.397921706989));
#39152=CARTESIAN_POINT('Ctrl Pts',(16.3452550272053,3.89553380888615,21.4934907341451));
#39153=CARTESIAN_POINT('Ctrl Pts',(17.5228113952696,3.6574248207145,22.3922930928554));
#39154=CARTESIAN_POINT('Origin',(29.2841674687199,27.6909737118635,6.98243503368624));
#39155=CARTESIAN_POINT('Origin',(10.025,6.68546421904046,11.0618097929987));
#39156=CARTESIAN_POINT('',(10.05,7.2688396415048,8.9584686252319));
#39157=CARTESIAN_POINT('',(10.05,6.7096297300963,11.0682151091822));
#39158=CARTESIAN_POINT('Ctrl Pts',(10.0000172182908,7.21645233578921,8.9610284120305));
#39159=CARTESIAN_POINT('Ctrl Pts',(10.0083297493438,7.2251665882511,8.96059579984804));
#39160=CARTESIAN_POINT('Ctrl Pts',(10.0166689056817,7.23390784118624,8.96016524108607));
#39161=CARTESIAN_POINT('Ctrl Pts',(10.0250085688505,7.24264870099244,8.95973813806369));
#39162=CARTESIAN_POINT('Ctrl Pts',(10.0333385064594,7.25137936737065,8.95931153312091));
#39163=CARTESIAN_POINT('Ctrl Pts',(10.0416689753296,7.26010967292925,8.95888836022941));
#39164=CARTESIAN_POINT('Ctrl Pts',(10.0499999999962,7.26883964150102,8.95846862523143));
#39165=CARTESIAN_POINT('Ctrl Pts',(10.05,7.2688396415048,8.9584686252319));
#39166=CARTESIAN_POINT('Ctrl Pts',(10.1661502473615,6.9691183885514,10.0892351704652));
#39167=CARTESIAN_POINT('Ctrl Pts',(10.5984429848576,6.37513989100329,12.3301540475785));
#39168=CARTESIAN_POINT('Ctrl Pts',(11.9625932588821,5.43398809923566,15.8808630801564));
#39169=CARTESIAN_POINT('Ctrl Pts',(14.2362718966461,4.49906819572165,19.4080608979592));
#39170=CARTESIAN_POINT('Ctrl Pts',(16.4418689323227,3.93996775027137,21.5173943967035));
#39171=CARTESIAN_POINT('Ctrl Pts',(17.652334347801,3.69831792998691,22.4290732641403));
#39172=CARTESIAN_POINT('Ctrl Pts',(10.0329820767251,7.25230186474276,8.95583316773028));
#39173=CARTESIAN_POINT('Ctrl Pts',(10.1489799126136,6.9523326853351,10.087560513709));
#39174=CARTESIAN_POINT('Ctrl Pts',(10.5811465692894,6.35785097057932,12.3304726305192));
#39175=CARTESIAN_POINT('Ctrl Pts',(11.9457666187964,5.4158607362461,15.8846301420578));
#39176=CARTESIAN_POINT('Ctrl Pts',(14.2209166065999,4.4800558859075,19.4156012755794));
#39177=CARTESIAN_POINT('Ctrl Pts',(16.4284006027391,3.92039060421677,21.527415596233));
#39178=CARTESIAN_POINT('Ctrl Pts',(17.6399944278817,3.67849079088921,22.4402019872628));
#39179=CARTESIAN_POINT('Ctrl Pts',(10.0159641534501,7.23576408798071,8.95319771022866));
#39180=CARTESIAN_POINT('Ctrl Pts',(10.1318095778657,6.9355469821188,10.0858858569528));
#39181=CARTESIAN_POINT('Ctrl Pts',(10.5638501537211,6.34056205015536,12.3307912134598));
#39182=CARTESIAN_POINT('Ctrl Pts',(11.9289399787108,5.39773337325653,15.8883972039592));
#39183=CARTESIAN_POINT('Ctrl Pts',(14.2055613165538,4.46104357609334,19.4231416531995));
#39184=CARTESIAN_POINT('Ctrl Pts',(16.4149322731554,3.90081345816216,21.5374367957625));
#39185=CARTESIAN_POINT('Ctrl Pts',(17.6276545079625,3.65866365179151,22.4513307103853));
#39186=CARTESIAN_POINT('Ctrl Pts',(9.99894623017517,7.21922631121867,8.95056225272703));
#39187=CARTESIAN_POINT('Ctrl Pts',(10.1146392431178,6.9187612789025,10.0842112001966));
#39188=CARTESIAN_POINT('Ctrl Pts',(10.5465537381528,6.3232731297314,12.3311097964004));
#39189=CARTESIAN_POINT('Ctrl Pts',(11.9121133386251,5.37960601026696,15.8921642658605));
#39190=CARTESIAN_POINT('Ctrl Pts',(14.1902060265076,4.44203126627919,19.4306820308196));
#39191=CARTESIAN_POINT('Ctrl Pts',(16.4014639435718,3.88123631210755,21.5474579952921));
#39192=CARTESIAN_POINT('Ctrl Pts',(17.6153145880432,3.63883651269381,22.4624594335078));
#39193=CARTESIAN_POINT('Ctrl Pts',(17.652334347801,3.69831792998691,22.4290732641403));
#39194=CARTESIAN_POINT('Ctrl Pts',(16.4418689323227,3.93996775027137,21.5173943967035));
#39195=CARTESIAN_POINT('Ctrl Pts',(14.2362718966461,4.49906819572165,19.4080608979592));
#39196=CARTESIAN_POINT('Ctrl Pts',(11.9625932588821,5.43398809923566,15.8808630801564));
#39197=CARTESIAN_POINT('Ctrl Pts',(10.5984429848576,6.37513989100329,12.3301540475785));
#39198=CARTESIAN_POINT('Ctrl Pts',(10.1661502473615,6.9691183885514,10.0892351704652));
#39199=CARTESIAN_POINT('Ctrl Pts',(10.05,7.2688396415048,8.9584686252319));
#39200=CARTESIAN_POINT('Origin',(10.,8.,6.2));
#39201=CARTESIAN_POINT('',(30.7,3.81894289852426,21.9739881555676));
#39202=CARTESIAN_POINT('Ctrl Pts',(30.7,3.81894289852426,21.9739881555676));
#39203=CARTESIAN_POINT('Ctrl Pts',(30.7,3.78282920367073,22.1102352770604));
#39204=CARTESIAN_POINT('Ctrl Pts',(30.7525414730858,3.73863720875327,22.2769596215218));
#39205=CARTESIAN_POINT('Ctrl Pts',(30.8616200595593,3.70421517668381,22.4068245606929));
#39206=CARTESIAN_POINT('Ctrl Pts',(30.883201857851,3.69834545349182,22.4289694254627));
#39207=CARTESIAN_POINT('',(30.7,6.7096297300963,11.0682151091821));
#39208=CARTESIAN_POINT('Origin',(30.7,6.41964359742627,10.9913513149805));
#39209=CARTESIAN_POINT('Origin',(30.7,3.52895676585423,21.8971243613659));
#39210=CARTESIAN_POINT('Origin',(30.7,7.76915840380663,5.9));
#39211=CARTESIAN_POINT('Ctrl Pts',(30.7,3.81894289852426,21.9739881555676));
#39212=CARTESIAN_POINT('Ctrl Pts',(30.7,3.78282920367073,22.1102352770604));
#39213=CARTESIAN_POINT('Ctrl Pts',(30.7715940999863,3.72261227565378,22.3374173236698));
#39214=CARTESIAN_POINT('Ctrl Pts',(31.0187900704284,3.66370490435624,22.5596587699287));
#39215=CARTESIAN_POINT('Ctrl Pts',(31.206032048618,3.65068523769029,22.6087784214412));
#39216=CARTESIAN_POINT('Ctrl Pts',(31.3,3.65068523769029,22.6087784214412));
#39217=CARTESIAN_POINT('Ctrl Pts',(30.7897597901026,3.81894289852426,21.9739881555676));
#39218=CARTESIAN_POINT('Ctrl Pts',(30.7848964349226,3.78727672262178,22.0927550475032));
#39219=CARTESIAN_POINT('Ctrl Pts',(30.8394512775623,3.73340196864192,22.296531662366));
#39220=CARTESIAN_POINT('Ctrl Pts',(31.0522093360623,3.67909470247398,22.5008277705934));
#39221=CARTESIAN_POINT('Ctrl Pts',(31.2172125765626,3.66718808492154,22.5465176796142));
#39222=CARTESIAN_POINT('Ctrl Pts',(31.3,3.66718808492154,22.5465176796142));
#39223=CARTESIAN_POINT('Ctrl Pts',(30.9451341282606,3.74609392831331,21.9546787899695));
#39224=CARTESIAN_POINT('Ctrl Pts',(30.9324919958102,3.73076953859995,22.045697702757));
#39225=CARTESIAN_POINT('Ctrl Pts',(30.9576800464939,3.70077983961214,22.2119544443171));
#39226=CARTESIAN_POINT('Ctrl Pts',(31.1107940637027,3.66738281103999,22.3880924247951));
#39227=CARTESIAN_POINT('Ctrl Pts',(31.2366864832781,3.65961053535241,22.4282347250844));
#39228=CARTESIAN_POINT('Ctrl Pts',(31.3,3.65961053535241,22.4282347250844));
#39229=CARTESIAN_POINT('Ctrl Pts',(31.,3.59402950185702,21.9143725564509));
#39230=CARTESIAN_POINT('Ctrl Pts',(30.9943394443927,3.5941157545723,21.9980577360181));
#39231=CARTESIAN_POINT('Ctrl Pts',(31.0222220993468,3.59316689985222,22.1457612036113));
#39232=CARTESIAN_POINT('Ctrl Pts',(31.1487007374675,3.5918369340252,22.2993482759741));
#39233=CARTESIAN_POINT('Ctrl Pts',(31.2494296143552,3.59144914920715,22.3342075571237));
#39234=CARTESIAN_POINT('Ctrl Pts',(31.3,3.59144914920715,22.3342075571237));
#39235=CARTESIAN_POINT('Ctrl Pts',(31.,3.52895676585423,21.8971243613659));
#39236=CARTESIAN_POINT('Ctrl Pts',(31.,3.53242173859483,21.9817483837486));
#39237=CARTESIAN_POINT('Ctrl Pts',(31.0357970499931,3.54051530807604,22.1255567476876));
#39238=CARTESIAN_POINT('Ctrl Pts',(31.1593950352142,3.55173936013825,22.2704611196166));
#39239=CARTESIAN_POINT('Ctrl Pts',(31.253016024309,3.55458559184835,22.3029866249648));
#39240=CARTESIAN_POINT('Ctrl Pts',(31.3,3.55458559184835,22.3029866249648));
#39241=CARTESIAN_POINT('Ctrl Pts',(31.3,3.55458559184835,22.3029866249648));
#39242=CARTESIAN_POINT('Ctrl Pts',(31.2756424398013,3.55458559184835,22.3029866249648));
#39243=CARTESIAN_POINT('Ctrl Pts',(31.251325303224,3.5542555152723,22.2986589576326));
#39244=CARTESIAN_POINT('Ctrl Pts',(31.2278365577763,3.55358711671133,22.2904495989342));
#39245=CARTESIAN_POINT('Ctrl Pts',(31.21687917868,3.55327531221602,22.2866199752705));
#39246=CARTESIAN_POINT('Ctrl Pts',(31.2061028246701,3.55288981741005,22.2819458574035));
#39247=CARTESIAN_POINT('Ctrl Pts',(31.1955904369623,3.55242800636988,22.2764746103786));
#39248=CARTESIAN_POINT('Ctrl Pts',(31.1851646913517,3.55197000153227,22.27104845685));
#39249=CARTESIAN_POINT('Ctrl Pts',(31.1749846707102,3.55145727885839,22.2648486445406));
#39250=CARTESIAN_POINT('Ctrl Pts',(31.1651324221987,3.55089593171273,22.2579251705824));
#39251=CARTESIAN_POINT('Ctrl Pts',(31.1440506461922,3.54969476481436,22.243110366936));
#39252=CARTESIAN_POINT('Ctrl Pts',(31.1244713735838,3.54827125610268,22.2249790389089));
#39253=CARTESIAN_POINT('Ctrl Pts',(31.1067914803827,3.54673218450983,22.204390880169));
#39254=CARTESIAN_POINT('Ctrl Pts',(31.1039119222156,3.54648151296309,22.2010376472072));
#39255=CARTESIAN_POINT('Ctrl Pts',(31.1010826937327,3.54622776561751,22.1976193381469));
#39256=CARTESIAN_POINT('Ctrl Pts',(31.0983054351552,3.54597138811509,22.1941397675718));
#39257=CARTESIAN_POINT('Ctrl Pts',(31.0849112824948,3.54473493162016,22.1773585071401));
#39258=CARTESIAN_POINT('Ctrl Pts',(31.0726984287011,3.54343307339863,22.159116102809));
#39259=CARTESIAN_POINT('Ctrl Pts',(31.0618470492513,3.54212767814902,22.139817606453));
#39260=CARTESIAN_POINT('Ctrl Pts',(31.0476338473508,3.54041786362005,22.1145403201548));
#39261=CARTESIAN_POINT('Ctrl Pts',(31.0357565901788,3.53870186217841,22.0874512813291));
#39262=CARTESIAN_POINT('Ctrl Pts',(31.0263360245292,3.53705605792282,22.0592732093212));
#39263=CARTESIAN_POINT('Ctrl Pts',(31.0146072529624,3.53500700239098,22.0241910091578));
#39264=CARTESIAN_POINT('Ctrl Pts',(31.0067007874871,3.53305164285664,21.9874657655656));
#39265=CARTESIAN_POINT('Ctrl Pts',(31.0028067335223,3.53130572162164,21.9504036863965));
#39266=CARTESIAN_POINT('Ctrl Pts',(31.0009438970831,3.53047050831289,21.9326739394002));
#39267=CARTESIAN_POINT('Ctrl Pts',(31.,3.52968323549415,21.9148667182822));
#39268=CARTESIAN_POINT('Ctrl Pts',(31.,3.52895676585423,21.8971243613659));
#39269=CARTESIAN_POINT('Ctrl Pts',(31.3,-3.65068523769029,22.6087784214412));
#39270=CARTESIAN_POINT('Ctrl Pts',(31.2060320492444,-3.65068523769029,22.6087784214412));
#39271=CARTESIAN_POINT('Ctrl Pts',(31.0661575833834,-3.66040229491942,22.5721186146222));
#39272=CARTESIAN_POINT('Ctrl Pts',(30.7974922692494,-3.7104074533064,22.3834627897986));
#39273=CARTESIAN_POINT('Ctrl Pts',(30.7,-3.77079130527928,22.1556509846282));
#39274=CARTESIAN_POINT('Ctrl Pts',(30.7,-3.81894289852426,21.9739881555676));
#39275=CARTESIAN_POINT('Ctrl Pts',(31.3,-3.66718808492154,22.5465176796142));
#39276=CARTESIAN_POINT('Ctrl Pts',(31.2172125771145,-3.66718808492154,22.5465176796142));
#39277=CARTESIAN_POINT('Ctrl Pts',(31.0940449626308,-3.67606150627315,22.5124376348801));
#39278=CARTESIAN_POINT('Ctrl Pts',(30.8609238321856,-3.7222672059363,22.3387523169962));
#39279=CARTESIAN_POINT('Ctrl Pts',(30.7832753165149,-3.77672133056048,22.1323440118337));
#39280=CARTESIAN_POINT('Ctrl Pts',(30.7897597901026,-3.81894289852426,21.9739881555676));
#39281=CARTESIAN_POINT('Ctrl Pts',(31.3,-3.65961053535241,22.4282347250844));
#39282=CARTESIAN_POINT('Ctrl Pts',(31.2366864837002,-3.65961053535241,22.4282347250844));
#39283=CARTESIAN_POINT('Ctrl Pts',(31.1429041474226,-3.66539136745645,22.3983436223796));
#39284=CARTESIAN_POINT('Ctrl Pts',(30.9713984134312,-3.69396820322993,22.2480618211276));
#39285=CARTESIAN_POINT('Ctrl Pts',(30.9282779516226,-3.72566140865002,22.0760373406227));
#39286=CARTESIAN_POINT('Ctrl Pts',(30.9451341282606,-3.74609392831331,21.9546787899695));
#39287=CARTESIAN_POINT('Ctrl Pts',(31.3,-3.59144914920716,22.3342075571237));
#39288=CARTESIAN_POINT('Ctrl Pts',(31.2494296146924,-3.59144914920716,22.3342075571237));
#39289=CARTESIAN_POINT('Ctrl Pts',(31.174304730506,-3.59174798363142,22.308273695567));
#39290=CARTESIAN_POINT('Ctrl Pts',(31.0343816236694,-3.59285979234815,22.1772532407699));
#39291=CARTESIAN_POINT('Ctrl Pts',(30.9924525925068,-3.59414450547755,22.025952796122));
#39292=CARTESIAN_POINT('Ctrl Pts',(31.,-3.59402950185703,21.9143725564509));
#39293=CARTESIAN_POINT('Ctrl Pts',(31.3,-3.55458559184835,22.3029866249648));
#39294=CARTESIAN_POINT('Ctrl Pts',(31.2530160246223,-3.55458559184835,22.3029866249648));
#39295=CARTESIAN_POINT('Ctrl Pts',(31.1830787916917,-3.55250612095037,22.2787754248841));
#39296=CARTESIAN_POINT('Ctrl Pts',(31.0487461346247,-3.5426930738467,22.155375588576));
#39297=CARTESIAN_POINT('Ctrl Pts',(31.,-3.53357672951851,22.0099563914605));
#39298=CARTESIAN_POINT('Ctrl Pts',(31.,-3.52895676585423,21.8971243613659));
#39299=CARTESIAN_POINT('',(30.7,-3.81894289852426,21.9739881555676));
#39300=CARTESIAN_POINT('Origin',(30.7,-3.52895676585423,21.8971243613659));
#39301=CARTESIAN_POINT('Ctrl Pts',(31.,-3.52895676585423,21.8971243613659));
#39302=CARTESIAN_POINT('Ctrl Pts',(31.,-3.53357672951851,22.0099563914605));
#39303=CARTESIAN_POINT('Ctrl Pts',(31.0487461346247,-3.5426930738467,22.155375588576));
#39304=CARTESIAN_POINT('Ctrl Pts',(31.1830787916917,-3.55250612095037,22.2787754248841));
#39305=CARTESIAN_POINT('Ctrl Pts',(31.2530160246223,-3.55458559184835,22.3029866249648));
#39306=CARTESIAN_POINT('Ctrl Pts',(31.3,-3.55458559184835,22.3029866249648));
#39307=CARTESIAN_POINT('Ctrl Pts',(30.8832668539234,-3.69836097281072,22.428910875305));
#39308=CARTESIAN_POINT('Ctrl Pts',(30.7656075273914,-3.73048633809753,22.3077106335411));
#39309=CARTESIAN_POINT('Ctrl Pts',(30.7,-3.77478001583655,22.1406026675257));
#39310=CARTESIAN_POINT('Ctrl Pts',(30.7,-3.81894289852426,21.9739881555676));
#39311=CARTESIAN_POINT('Origin',(30.7,-4.21964359742627,19.2913513149805));
#39312=CARTESIAN_POINT('',(30.7,-4.5096297300963,19.3682151091822));
#39313=CARTESIAN_POINT('Origin',(10.,-3.6,22.8));
#39314=CARTESIAN_POINT('Origin',(30.7,-4.8,10.35));
#39315=CARTESIAN_POINT('Origin',(30.7,-4.8,14.));
#39316=CARTESIAN_POINT('Origin',(30.7,-4.8,5.9));
#39317=CARTESIAN_POINT('Origin',(30.7,0.,5.9));
#39318=CARTESIAN_POINT('Origin',(30.7,4.8,5.9));
#39319=CARTESIAN_POINT('Origin',(30.7,0.,14.));
#39320=CARTESIAN_POINT('Origin',(30.7,4.8,14.));
#39321=CARTESIAN_POINT('Origin',(30.7,4.8,14.25));
#39322=CARTESIAN_POINT('Origin',(30.7,0.,5.9));
#39323=CARTESIAN_POINT('Origin',(30.,10.,4.2));
#39324=CARTESIAN_POINT('Origin',(31.3,0.,26.5));
#39325=CARTESIAN_POINT('Origin',(29.55,9.4,6.2));
#39326=CARTESIAN_POINT('Origin',(11.55,-9.,6.2));
#39327=CARTESIAN_POINT('Origin',(11.55,9.4,6.2));
#39328=CARTESIAN_POINT('Origin',(29.55,-9.,6.2));
#39329=CARTESIAN_POINT('Origin',(9.4916312444017,3.53553390593274,22.9644660940673));
#39330=CARTESIAN_POINT('',(9.58326248880341,3.53553390593274,22.9644660940673));
#39331=CARTESIAN_POINT('',(9.4916312444017,3.53553390593274,22.8119660940673));
#39332=CARTESIAN_POINT('Origin',(9.4916312444017,-3.53553390593274,22.9644660940673));
#39333=CARTESIAN_POINT('',(9.58326248880341,-3.53553390593274,22.9644660940673));
#39334=CARTESIAN_POINT('',(9.4916312444017,-3.53553390593274,22.8119660940673));
#39335=CARTESIAN_POINT('Origin',(9.4916312444017,-3.53553390593274,30.0355339059327));
#39336=CARTESIAN_POINT('',(9.58326248880341,-3.53553390593274,30.0355339059327));
#39337=CARTESIAN_POINT('',(9.4916312444017,-3.53553390593274,29.8830339059327));
#39338=CARTESIAN_POINT('Origin',(9.4916312444017,3.53553390593274,30.0355339059327));
#39339=CARTESIAN_POINT('',(9.58326248880341,3.53553390593274,30.0355339059327));
#39340=CARTESIAN_POINT('',(9.4916312444017,3.53553390593274,29.8830339059327));
#39341=CARTESIAN_POINT('Origin',(34.905,0.,21.2));
#39342=CARTESIAN_POINT('',(34.095,-4.95981953654679E-17,21.2));
#39343=CARTESIAN_POINT('Origin',(34.5,0.,21.2));
#39344=CARTESIAN_POINT('Origin',(34.5,0.,22.4));
#39345=CARTESIAN_POINT('',(34.095,-5.94935672022701E-17,23.));
#39346=CARTESIAN_POINT('',(34.095,-4.95981953654679E-17,22.4));
#39347=CARTESIAN_POINT('',(34.5,-0.405000000000001,23.0235111103298));
#39348=CARTESIAN_POINT('Ctrl Pts',(34.5,-0.405000000000001,23.0235111103298));
#39349=CARTESIAN_POINT('Ctrl Pts',(34.449098166481,-0.405000000000001,23.0235111103298));
#39350=CARTESIAN_POINT('Ctrl Pts',(34.3948349045423,-0.39481791137655,23.0222778822844));
#39351=CARTESIAN_POINT('Ctrl Pts',(34.2950649266667,-0.353472062708214,
23.0178325988594));
#39352=CARTESIAN_POINT('Ctrl Pts',(34.2495542896821,-0.322310782443173,
23.0146857230619));
#39353=CARTESIAN_POINT('Ctrl Pts',(34.177689437535,-0.250445930296054,23.0087857886416));
#39354=CARTESIAN_POINT('Ctrl Pts',(34.1465279851107,-0.204935197396313,
23.0056481306998));
#39355=CARTESIAN_POINT('Ctrl Pts',(34.1051820095339,-0.105164895936886,
23.0012239616958));
#39356=CARTESIAN_POINT('Ctrl Pts',(34.095,-0.0509015218992326,23.));
#39357=CARTESIAN_POINT('Ctrl Pts',(34.095,-5.55111512312578E-17,23.));
#39358=CARTESIAN_POINT('Ctrl Pts',(34.095,-6.93889390390723E-17,23.));
#39359=CARTESIAN_POINT('Ctrl Pts',(34.095,0.0509015218992325,23.));
#39360=CARTESIAN_POINT('Ctrl Pts',(34.1051820095339,0.105164895936886,23.0012239616958));
#39361=CARTESIAN_POINT('Ctrl Pts',(34.1465279851107,0.204935197396313,23.0056481306998));
#39362=CARTESIAN_POINT('Ctrl Pts',(34.177689437535,0.250445930296054,23.0087857886416));
#39363=CARTESIAN_POINT('Ctrl Pts',(34.2495542896821,0.322310782443173,23.0146857230619));
#39364=CARTESIAN_POINT('Ctrl Pts',(34.2950649266667,0.353472062708214,23.0178325988594));
#39365=CARTESIAN_POINT('Ctrl Pts',(34.3948349045423,0.39481791137655,23.0222778822844));
#39366=CARTESIAN_POINT('Ctrl Pts',(34.449098166481,0.405000000000001,23.0235111103298));
#39367=CARTESIAN_POINT('Ctrl Pts',(34.550901833519,0.405000000000001,23.0235111103298));
#39368=CARTESIAN_POINT('Ctrl Pts',(34.6051650954577,0.39481791137655,23.0222778822844));
#39369=CARTESIAN_POINT('Ctrl Pts',(34.7049350733333,0.353472062708214,23.0178325988594));
#39370=CARTESIAN_POINT('Ctrl Pts',(34.7504457103179,0.322310782443173,23.0146857230619));
#39371=CARTESIAN_POINT('Ctrl Pts',(34.822310562465,0.250445930296054,23.0087857886416));
#39372=CARTESIAN_POINT('Ctrl Pts',(34.8534720148893,0.204935197396313,23.0056481306998));
#39373=CARTESIAN_POINT('Ctrl Pts',(34.8948179904661,0.105164895936886,23.0012239616958));
#39374=CARTESIAN_POINT('Ctrl Pts',(34.905,0.0509015218992327,23.));
#39375=CARTESIAN_POINT('Ctrl Pts',(34.905,-0.0509015218992325,23.));
#39376=CARTESIAN_POINT('Ctrl Pts',(34.8948179904661,-0.105164895936886,
23.0012239616958));
#39377=CARTESIAN_POINT('Ctrl Pts',(34.8534720148893,-0.204935197396313,
23.0056481306998));
#39378=CARTESIAN_POINT('Ctrl Pts',(34.822310562465,-0.250445930296054,23.0087857886416));
#39379=CARTESIAN_POINT('Ctrl Pts',(34.7504457103179,-0.322310782443173,
23.0146857230619));
#39380=CARTESIAN_POINT('Ctrl Pts',(34.7049350733333,-0.353472062708218,
23.0178325988594));
#39381=CARTESIAN_POINT('Ctrl Pts',(34.6051650954577,-0.394817911376552,
23.0222778822844));
#39382=CARTESIAN_POINT('Ctrl Pts',(34.550901833519,-0.405000000000001,23.0235111103298));
#39383=CARTESIAN_POINT('Ctrl Pts',(34.5,-0.405000000000002,23.0235111103298));
#39384=CARTESIAN_POINT('Origin',(33.5,0.,30.4));
#39385=CARTESIAN_POINT('',(33.5,-1.005,29.8526071944086));
#39386=CARTESIAN_POINT('',(32.495,-2.14194167543114E-16,30.));
#39387=CARTESIAN_POINT('Ctrl Pts',(33.5,-1.005,29.8526071944086));
#39388=CARTESIAN_POINT('Ctrl Pts',(33.6269804671999,-1.005,29.8526071944086));
#39389=CARTESIAN_POINT('Ctrl Pts',(33.761899912268,-0.979475933914398,29.8605754646619));
#39390=CARTESIAN_POINT('Ctrl Pts',(34.0092777665881,-0.876698892882462,
29.8888404369081));
#39391=CARTESIAN_POINT('Ctrl Pts',(34.1218034634525,-0.799481166732521,
29.9086744581332));
#39392=CARTESIAN_POINT('Ctrl Pts',(34.2994591208888,-0.621825509296123,
29.9455131183184));
#39393=CARTESIAN_POINT('Ctrl Pts',(34.3766939521777,-0.509290792165725,
29.9649839652991));
#39394=CARTESIAN_POINT('Ctrl Pts',(34.479483580312,-0.261880374230206,29.9924074303405));
#39395=CARTESIAN_POINT('Ctrl Pts',(34.505,-0.126948956307063,30.));
#39396=CARTESIAN_POINT('Ctrl Pts',(34.505,0.126948956307063,30.));
#39397=CARTESIAN_POINT('Ctrl Pts',(34.479483580312,0.261880374230207,29.9924074303405));
#39398=CARTESIAN_POINT('Ctrl Pts',(34.3766939521777,0.509290792165726,29.9649839652991));
#39399=CARTESIAN_POINT('Ctrl Pts',(34.2994591208888,0.621825509296123,29.9455131183184));
#39400=CARTESIAN_POINT('Ctrl Pts',(34.1218034634525,0.799481166732521,29.9086744581332));
#39401=CARTESIAN_POINT('Ctrl Pts',(34.0092777665881,0.876698892882462,29.8888404369081));
#39402=CARTESIAN_POINT('Ctrl Pts',(33.761899912268,0.979475933914398,29.8605754646619));
#39403=CARTESIAN_POINT('Ctrl Pts',(33.6269804671999,1.005,29.8526071944086));
#39404=CARTESIAN_POINT('Ctrl Pts',(33.3730195328001,1.005,29.8526071944086));
#39405=CARTESIAN_POINT('Ctrl Pts',(33.238100087732,0.979475933914398,29.8605754646619));
#39406=CARTESIAN_POINT('Ctrl Pts',(32.9907222334119,0.876698892882462,29.8888404369081));
#39407=CARTESIAN_POINT('Ctrl Pts',(32.8781965365475,0.799481166732521,29.9086744581332));
#39408=CARTESIAN_POINT('Ctrl Pts',(32.7005408791112,0.621825509296124,29.9455131183184));
#39409=CARTESIAN_POINT('Ctrl Pts',(32.6233060478223,0.509290792165726,29.9649839652991));
#39410=CARTESIAN_POINT('Ctrl Pts',(32.520516419688,0.261880374230206,29.9924074303405));
#39411=CARTESIAN_POINT('Ctrl Pts',(32.495,0.126948956307063,30.));
#39412=CARTESIAN_POINT('Ctrl Pts',(32.495,3.88578058618805E-16,30.));
#39413=CARTESIAN_POINT('Ctrl Pts',(32.495,-2.4980018054066E-16,30.));
#39414=CARTESIAN_POINT('Ctrl Pts',(32.495,-0.126948956307063,30.));
#39415=CARTESIAN_POINT('Ctrl Pts',(32.520516419688,-0.261880374230207,29.9924074303405));
#39416=CARTESIAN_POINT('Ctrl Pts',(32.6233060478223,-0.509290792165726,
29.9649839652991));
#39417=CARTESIAN_POINT('Ctrl Pts',(32.7005408791112,-0.621825509296123,
29.9455131183184));
#39418=CARTESIAN_POINT('Ctrl Pts',(32.8781965365475,-0.799481166732521,
29.9086744581332));
#39419=CARTESIAN_POINT('Ctrl Pts',(32.9907222334119,-0.876698892882462,
29.8888404369081));
#39420=CARTESIAN_POINT('Ctrl Pts',(33.238100087732,-0.979475933914398,29.8605754646619));
#39421=CARTESIAN_POINT('Ctrl Pts',(33.3730195328001,-1.005,29.8526071944086));
#39422=CARTESIAN_POINT('Ctrl Pts',(33.5,-1.005,29.8526071944086));
#39423=CARTESIAN_POINT('',(32.495,-1.23077003314309E-16,31.8));
#39424=CARTESIAN_POINT('',(32.495,-1.23077003314309E-16,30.4));
#39425=CARTESIAN_POINT('Origin',(33.5,0.,31.8));
#39426=CARTESIAN_POINT('Origin',(34.105,0.,31.8));
#39427=CARTESIAN_POINT('',(32.895,-7.40911313484154E-17,31.8));
#39428=CARTESIAN_POINT('Origin',(33.5,0.,31.8));
#39429=CARTESIAN_POINT('Origin',(33.5,0.,32.65));
#39430=CARTESIAN_POINT('',(32.895,-7.40911313484154E-17,32.65));
#39431=CARTESIAN_POINT('Origin',(22.,0.,26.5));
#39432=CARTESIAN_POINT('',(8.,-3.5,26.5));
#39433=CARTESIAN_POINT('Origin',(8.,0.,26.5));
#39434=CARTESIAN_POINT('',(22.,-3.5,26.5));
#39435=CARTESIAN_POINT('Origin',(8.,5.5,26.5));
#39436=CARTESIAN_POINT('',(0.,0.,0.));
#39437=CARTESIAN_POINT('Origin',(38.9767641234007,0.,26.5));
#39438=CARTESIAN_POINT('',(39.,3.05,26.5));
#39439=CARTESIAN_POINT('Origin',(39.,0.,26.5));
#39440=CARTESIAN_POINT('',(38.9535282468013,3.11844928601987,26.5));
#39441=CARTESIAN_POINT('',(38.9767641234007,3.08422464300993,26.5));
#39442=CARTESIAN_POINT('',(38.9535282468013,-3.11844928601987,26.5));
#39443=CARTESIAN_POINT('Origin',(38.9535282468013,0.,26.5));
#39444=CARTESIAN_POINT('Origin',(38.9535282468013,0.,26.5));
#39445=CARTESIAN_POINT('Origin',(38.5,0.,26.5));
#39446=CARTESIAN_POINT('',(38.,-3.497,26.5));
#39447=CARTESIAN_POINT('',(38.5,-3.2985,26.5));
#39448=CARTESIAN_POINT('Origin',(38.,0.,26.5));
#39449=CARTESIAN_POINT('Origin',(39.,1.64335,26.5));
#39450=CARTESIAN_POINT('',(39.,-1.64335,26.5));
#39451=CARTESIAN_POINT('Origin',(39.,0.,26.5));
#39452=CARTESIAN_POINT('Origin',(27.97,0.2,30.097));
#39453=CARTESIAN_POINT('',(27.97,0.2,29.9912761277218));
#39454=CARTESIAN_POINT('',(28.03,0.2,29.9912761277218));
#39455=CARTESIAN_POINT('',(24.05,0.2,29.9912761277218));
#39456=CARTESIAN_POINT('',(27.97,0.2,29.957));
#39457=CARTESIAN_POINT('',(27.97,0.2,30.097));
#39458=CARTESIAN_POINT('',(28.03,0.2,29.957));
#39459=CARTESIAN_POINT('',(28.03,0.2,29.957));
#39460=CARTESIAN_POINT('',(28.03,0.2,30.097));
#39461=CARTESIAN_POINT('Origin',(28.03,0.2,30.097));
#39462=CARTESIAN_POINT('',(28.03,-0.2,29.9912761277218));
#39463=CARTESIAN_POINT('Origin',(28.03,0.,26.5));
#39464=CARTESIAN_POINT('',(28.03,-0.2,29.957));
#39465=CARTESIAN_POINT('',(28.03,-0.2,29.957));
#39466=CARTESIAN_POINT('',(28.03,-0.2,30.097));
#39467=CARTESIAN_POINT('Origin',(28.03,-0.2,30.097));
#39468=CARTESIAN_POINT('',(27.97,-0.2,29.9912761277218));
#39469=CARTESIAN_POINT('',(24.05,-0.2,29.9912761277218));
#39470=CARTESIAN_POINT('',(27.97,-0.2,29.957));
#39471=CARTESIAN_POINT('',(27.97,-0.2,29.957));
#39472=CARTESIAN_POINT('',(27.97,-0.2,30.097));
#39473=CARTESIAN_POINT('Origin',(27.97,-0.2,30.097));
#39474=CARTESIAN_POINT('Origin',(27.97,0.,26.5));
#39475=CARTESIAN_POINT('',(27.97,0.2,29.957));
#39476=CARTESIAN_POINT('Origin',(28.,0.,29.957));
#39477=CARTESIAN_POINT('Origin',(28.97,0.2,30.097));
#39478=CARTESIAN_POINT('',(28.97,0.2,29.9912761277218));
#39479=CARTESIAN_POINT('',(29.03,0.2,29.9912761277218));
#39480=CARTESIAN_POINT('',(24.05,0.2,29.9912761277218));
#39481=CARTESIAN_POINT('',(28.97,0.2,29.957));
#39482=CARTESIAN_POINT('',(28.97,0.2,30.097));
#39483=CARTESIAN_POINT('',(29.03,0.2,29.957));
#39484=CARTESIAN_POINT('',(29.03,0.2,29.957));
#39485=CARTESIAN_POINT('',(29.03,0.2,30.097));
#39486=CARTESIAN_POINT('Origin',(29.03,0.2,30.097));
#39487=CARTESIAN_POINT('',(29.03,-0.2,29.9912761277218));
#39488=CARTESIAN_POINT('Origin',(29.03,0.,26.5));
#39489=CARTESIAN_POINT('',(29.03,-0.2,29.957));
#39490=CARTESIAN_POINT('',(29.03,-0.2,29.957));
#39491=CARTESIAN_POINT('',(29.03,-0.2,30.097));
#39492=CARTESIAN_POINT('Origin',(29.03,-0.2,30.097));
#39493=CARTESIAN_POINT('',(28.97,-0.2,29.9912761277218));
#39494=CARTESIAN_POINT('',(24.05,-0.2,29.9912761277218));
#39495=CARTESIAN_POINT('',(28.97,-0.2,29.957));
#39496=CARTESIAN_POINT('',(28.97,-0.2,29.957));
#39497=CARTESIAN_POINT('',(28.97,-0.2,30.097));
#39498=CARTESIAN_POINT('Origin',(28.97,-0.2,30.097));
#39499=CARTESIAN_POINT('Origin',(28.97,0.,26.5));
#39500=CARTESIAN_POINT('',(28.97,0.2,29.957));
#39501=CARTESIAN_POINT('Origin',(29.,0.,29.957));
#39502=CARTESIAN_POINT('Origin',(29.97,0.2,30.097));
#39503=CARTESIAN_POINT('',(29.97,0.2,29.9912761277218));
#39504=CARTESIAN_POINT('',(30.03,0.2,29.9912761277218));
#39505=CARTESIAN_POINT('',(24.05,0.2,29.9912761277218));
#39506=CARTESIAN_POINT('',(29.97,0.2,29.957));
#39507=CARTESIAN_POINT('',(29.97,0.2,30.097));
#39508=CARTESIAN_POINT('',(30.03,0.2,29.957));
#39509=CARTESIAN_POINT('',(30.03,0.2,29.957));
#39510=CARTESIAN_POINT('',(30.03,0.2,30.097));
#39511=CARTESIAN_POINT('Origin',(30.03,0.2,30.097));
#39512=CARTESIAN_POINT('',(30.03,-0.2,29.9912761277218));
#39513=CARTESIAN_POINT('Origin',(30.03,0.,26.5));
#39514=CARTESIAN_POINT('',(30.03,-0.2,29.957));
#39515=CARTESIAN_POINT('',(30.03,-0.2,29.957));
#39516=CARTESIAN_POINT('',(30.03,-0.2,30.097));
#39517=CARTESIAN_POINT('Origin',(30.03,-0.2,30.097));
#39518=CARTESIAN_POINT('',(29.97,-0.2,29.9912761277218));
#39519=CARTESIAN_POINT('',(24.05,-0.2,29.9912761277218));
#39520=CARTESIAN_POINT('',(29.97,-0.2,29.957));
#39521=CARTESIAN_POINT('',(29.97,-0.2,29.957));
#39522=CARTESIAN_POINT('',(29.97,-0.2,30.097));
#39523=CARTESIAN_POINT('Origin',(29.97,-0.2,30.097));
#39524=CARTESIAN_POINT('Origin',(29.97,0.,26.5));
#39525=CARTESIAN_POINT('',(29.97,0.2,29.957));
#39526=CARTESIAN_POINT('Origin',(30.,0.,29.957));
#39527=CARTESIAN_POINT('Origin',(30.97,0.2,30.097));
#39528=CARTESIAN_POINT('',(30.97,0.2,29.9912761277218));
#39529=CARTESIAN_POINT('',(31.03,0.2,29.9912761277218));
#39530=CARTESIAN_POINT('',(24.05,0.2,29.9912761277218));
#39531=CARTESIAN_POINT('',(30.97,0.2,29.957));
#39532=CARTESIAN_POINT('',(30.97,0.2,30.097));
#39533=CARTESIAN_POINT('',(31.03,0.2,29.957));
#39534=CARTESIAN_POINT('',(31.03,0.2,29.957));
#39535=CARTESIAN_POINT('',(31.03,0.2,30.097));
#39536=CARTESIAN_POINT('Origin',(31.03,0.2,30.097));
#39537=CARTESIAN_POINT('',(31.03,-0.2,29.9912761277218));
#39538=CARTESIAN_POINT('Origin',(31.03,0.,26.5));
#39539=CARTESIAN_POINT('',(31.03,-0.2,29.957));
#39540=CARTESIAN_POINT('',(31.03,-0.2,29.957));
#39541=CARTESIAN_POINT('',(31.03,-0.2,30.097));
#39542=CARTESIAN_POINT('Origin',(31.03,-0.2,30.097));
#39543=CARTESIAN_POINT('',(30.97,-0.2,29.9912761277218));
#39544=CARTESIAN_POINT('',(24.05,-0.2,29.9912761277218));
#39545=CARTESIAN_POINT('',(30.97,-0.2,29.957));
#39546=CARTESIAN_POINT('',(30.97,-0.2,29.957));
#39547=CARTESIAN_POINT('',(30.97,-0.2,30.097));
#39548=CARTESIAN_POINT('Origin',(30.97,-0.2,30.097));
#39549=CARTESIAN_POINT('Origin',(30.97,0.,26.5));
#39550=CARTESIAN_POINT('',(30.97,0.2,29.957));
#39551=CARTESIAN_POINT('Origin',(31.,0.,29.957));
#39552=CARTESIAN_POINT('Origin',(31.97,0.2,30.097));
#39553=CARTESIAN_POINT('',(31.97,0.2,29.9912761277218));
#39554=CARTESIAN_POINT('',(32.03,0.2,29.9912761277218));
#39555=CARTESIAN_POINT('',(24.05,0.2,29.9912761277218));
#39556=CARTESIAN_POINT('',(31.97,0.2,29.957));
#39557=CARTESIAN_POINT('',(31.97,0.2,30.097));
#39558=CARTESIAN_POINT('',(32.03,0.2,29.957));
#39559=CARTESIAN_POINT('',(32.03,0.2,29.957));
#39560=CARTESIAN_POINT('',(32.03,0.2,30.097));
#39561=CARTESIAN_POINT('Origin',(32.03,0.2,30.097));
#39562=CARTESIAN_POINT('',(32.03,-0.2,29.9912761277218));
#39563=CARTESIAN_POINT('Origin',(32.03,0.,26.5));
#39564=CARTESIAN_POINT('',(32.03,-0.2,29.957));
#39565=CARTESIAN_POINT('',(32.03,-0.2,29.957));
#39566=CARTESIAN_POINT('',(32.03,-0.2,30.097));
#39567=CARTESIAN_POINT('Origin',(32.03,-0.2,30.097));
#39568=CARTESIAN_POINT('',(31.97,-0.2,29.9912761277218));
#39569=CARTESIAN_POINT('',(24.05,-0.2,29.9912761277218));
#39570=CARTESIAN_POINT('',(31.97,-0.2,29.957));
#39571=CARTESIAN_POINT('',(31.97,-0.2,29.957));
#39572=CARTESIAN_POINT('',(31.97,-0.2,30.097));
#39573=CARTESIAN_POINT('Origin',(31.97,-0.2,30.097));
#39574=CARTESIAN_POINT('Origin',(31.97,0.,26.5));
#39575=CARTESIAN_POINT('',(31.97,0.2,29.957));
#39576=CARTESIAN_POINT('Origin',(32.,0.,29.957));
#39577=CARTESIAN_POINT('Origin',(32.47,0.35,30.097));
#39578=CARTESIAN_POINT('',(32.47,0.35,29.9794409033636));
#39579=CARTESIAN_POINT('',(32.53,0.35,29.9794409033636));
#39580=CARTESIAN_POINT('',(24.05,0.35,29.9794409033636));
#39581=CARTESIAN_POINT('',(32.47,0.35,29.957));
#39582=CARTESIAN_POINT('',(32.47,0.35,30.097));
#39583=CARTESIAN_POINT('',(32.53,0.35,29.957));
#39584=CARTESIAN_POINT('',(32.53,0.35,29.957));
#39585=CARTESIAN_POINT('',(32.53,0.35,30.097));
#39586=CARTESIAN_POINT('Origin',(32.53,0.35,30.097));
#39587=CARTESIAN_POINT('',(32.53,-0.35,29.9794409033636));
#39588=CARTESIAN_POINT('Origin',(32.53,0.,26.5));
#39589=CARTESIAN_POINT('',(32.53,-0.35,29.957));
#39590=CARTESIAN_POINT('',(32.53,-0.35,29.957));
#39591=CARTESIAN_POINT('',(32.53,-0.35,30.097));
#39592=CARTESIAN_POINT('Origin',(32.53,-0.35,30.097));
#39593=CARTESIAN_POINT('',(32.47,-0.35,29.9794409033636));
#39594=CARTESIAN_POINT('',(24.05,-0.35,29.9794409033636));
#39595=CARTESIAN_POINT('',(32.47,-0.35,29.957));
#39596=CARTESIAN_POINT('',(32.47,-0.35,29.957));
#39597=CARTESIAN_POINT('',(32.47,-0.35,30.097));
#39598=CARTESIAN_POINT('Origin',(32.47,-0.35,30.097));
#39599=CARTESIAN_POINT('Origin',(32.47,0.,26.5));
#39600=CARTESIAN_POINT('',(32.47,0.35,29.957));
#39601=CARTESIAN_POINT('Origin',(32.5,0.,29.957));
#39602=CARTESIAN_POINT('Origin',(33.47,0.35,30.097));
#39603=CARTESIAN_POINT('',(33.47,0.35,29.9794409033636));
#39604=CARTESIAN_POINT('',(33.53,0.35,29.9794409033636));
#39605=CARTESIAN_POINT('',(24.05,0.35,29.9794409033636));
#39606=CARTESIAN_POINT('',(33.47,0.35,29.957));
#39607=CARTESIAN_POINT('',(33.47,0.35,30.097));
#39608=CARTESIAN_POINT('',(33.53,0.35,29.957));
#39609=CARTESIAN_POINT('',(33.53,0.35,29.957));
#39610=CARTESIAN_POINT('',(33.53,0.35,30.097));
#39611=CARTESIAN_POINT('Origin',(33.53,0.35,30.097));
#39612=CARTESIAN_POINT('',(33.53,-0.35,29.9794409033636));
#39613=CARTESIAN_POINT('Origin',(33.53,0.,26.5));
#39614=CARTESIAN_POINT('',(33.53,-0.35,29.957));
#39615=CARTESIAN_POINT('',(33.53,-0.35,29.957));
#39616=CARTESIAN_POINT('',(33.53,-0.35,30.097));
#39617=CARTESIAN_POINT('Origin',(33.53,-0.35,30.097));
#39618=CARTESIAN_POINT('',(33.47,-0.35,29.9794409033636));
#39619=CARTESIAN_POINT('',(24.05,-0.35,29.9794409033636));
#39620=CARTESIAN_POINT('',(33.47,-0.35,29.957));
#39621=CARTESIAN_POINT('',(33.47,-0.35,29.957));
#39622=CARTESIAN_POINT('',(33.47,-0.35,30.097));
#39623=CARTESIAN_POINT('Origin',(33.47,-0.35,30.097));
#39624=CARTESIAN_POINT('Origin',(33.47,0.,26.5));
#39625=CARTESIAN_POINT('',(33.47,0.35,29.957));
#39626=CARTESIAN_POINT('Origin',(33.5,0.,29.957));
#39627=CARTESIAN_POINT('Origin',(34.47,0.35,30.097));
#39628=CARTESIAN_POINT('',(34.47,0.35,29.9794409033636));
#39629=CARTESIAN_POINT('',(34.53,0.35,29.9794409033636));
#39630=CARTESIAN_POINT('',(24.05,0.35,29.9794409033636));
#39631=CARTESIAN_POINT('',(34.47,0.35,29.957));
#39632=CARTESIAN_POINT('',(34.47,0.35,30.097));
#39633=CARTESIAN_POINT('',(34.53,0.35,29.957));
#39634=CARTESIAN_POINT('',(34.53,0.35,29.957));
#39635=CARTESIAN_POINT('',(34.53,0.35,30.097));
#39636=CARTESIAN_POINT('Origin',(34.53,0.35,30.097));
#39637=CARTESIAN_POINT('',(34.53,-0.35,29.9794409033636));
#39638=CARTESIAN_POINT('Origin',(34.53,0.,26.5));
#39639=CARTESIAN_POINT('',(34.53,-0.35,29.957));
#39640=CARTESIAN_POINT('',(34.53,-0.35,29.957));
#39641=CARTESIAN_POINT('',(34.53,-0.35,30.097));
#39642=CARTESIAN_POINT('Origin',(34.53,-0.35,30.097));
#39643=CARTESIAN_POINT('',(34.47,-0.35,29.9794409033636));
#39644=CARTESIAN_POINT('',(24.05,-0.35,29.9794409033636));
#39645=CARTESIAN_POINT('',(34.47,-0.35,29.957));
#39646=CARTESIAN_POINT('',(34.47,-0.35,29.957));
#39647=CARTESIAN_POINT('',(34.47,-0.35,30.097));
#39648=CARTESIAN_POINT('Origin',(34.47,-0.35,30.097));
#39649=CARTESIAN_POINT('Origin',(34.47,0.,26.5));
#39650=CARTESIAN_POINT('',(34.47,0.35,29.957));
#39651=CARTESIAN_POINT('Origin',(34.5,0.,29.957));
#39652=CARTESIAN_POINT('Origin',(35.47,0.35,30.097));
#39653=CARTESIAN_POINT('',(35.47,0.35,29.9794409033636));
#39654=CARTESIAN_POINT('',(35.53,0.35,29.9794409033636));
#39655=CARTESIAN_POINT('',(24.05,0.35,29.9794409033636));
#39656=CARTESIAN_POINT('',(35.47,0.35,29.957));
#39657=CARTESIAN_POINT('',(35.47,0.35,30.097));
#39658=CARTESIAN_POINT('',(35.53,0.35,29.957));
#39659=CARTESIAN_POINT('',(35.53,0.35,29.957));
#39660=CARTESIAN_POINT('',(35.53,0.35,30.097));
#39661=CARTESIAN_POINT('Origin',(35.53,0.35,30.097));
#39662=CARTESIAN_POINT('',(35.53,-0.35,29.9794409033636));
#39663=CARTESIAN_POINT('Origin',(35.53,0.,26.5));
#39664=CARTESIAN_POINT('',(35.53,-0.35,29.957));
#39665=CARTESIAN_POINT('',(35.53,-0.35,29.957));
#39666=CARTESIAN_POINT('',(35.53,-0.35,30.097));
#39667=CARTESIAN_POINT('Origin',(35.53,-0.35,30.097));
#39668=CARTESIAN_POINT('',(35.47,-0.35,29.9794409033636));
#39669=CARTESIAN_POINT('',(24.05,-0.35,29.9794409033636));
#39670=CARTESIAN_POINT('',(35.47,-0.35,29.957));
#39671=CARTESIAN_POINT('',(35.47,-0.35,29.957));
#39672=CARTESIAN_POINT('',(35.47,-0.35,30.097));
#39673=CARTESIAN_POINT('Origin',(35.47,-0.35,30.097));
#39674=CARTESIAN_POINT('Origin',(35.47,0.,26.5));
#39675=CARTESIAN_POINT('',(35.47,0.35,29.957));
#39676=CARTESIAN_POINT('Origin',(35.5,0.,29.957));
#39677=CARTESIAN_POINT('Origin',(36.47,0.35,30.097));
#39678=CARTESIAN_POINT('',(36.47,0.35,29.9794409033636));
#39679=CARTESIAN_POINT('',(36.53,0.35,29.9794409033636));
#39680=CARTESIAN_POINT('',(24.05,0.35,29.9794409033636));
#39681=CARTESIAN_POINT('',(36.47,0.35,29.957));
#39682=CARTESIAN_POINT('',(36.47,0.35,30.097));
#39683=CARTESIAN_POINT('',(36.53,0.35,29.957));
#39684=CARTESIAN_POINT('',(36.53,0.35,29.957));
#39685=CARTESIAN_POINT('',(36.53,0.35,30.097));
#39686=CARTESIAN_POINT('Origin',(36.53,0.35,30.097));
#39687=CARTESIAN_POINT('',(36.53,-0.35,29.9794409033636));
#39688=CARTESIAN_POINT('Origin',(36.53,0.,26.5));
#39689=CARTESIAN_POINT('',(36.53,-0.35,29.957));
#39690=CARTESIAN_POINT('',(36.53,-0.35,29.957));
#39691=CARTESIAN_POINT('',(36.53,-0.35,30.097));
#39692=CARTESIAN_POINT('Origin',(36.53,-0.35,30.097));
#39693=CARTESIAN_POINT('',(36.47,-0.35,29.9794409033636));
#39694=CARTESIAN_POINT('',(24.05,-0.35,29.9794409033636));
#39695=CARTESIAN_POINT('',(36.47,-0.35,29.957));
#39696=CARTESIAN_POINT('',(36.47,-0.35,29.957));
#39697=CARTESIAN_POINT('',(36.47,-0.35,30.097));
#39698=CARTESIAN_POINT('Origin',(36.47,-0.35,30.097));
#39699=CARTESIAN_POINT('Origin',(36.47,0.,26.5));
#39700=CARTESIAN_POINT('',(36.47,0.35,29.957));
#39701=CARTESIAN_POINT('Origin',(36.5,0.,29.957));
#39702=CARTESIAN_POINT('Origin',(36.97,0.2,30.097));
#39703=CARTESIAN_POINT('',(36.97,0.2,29.9912761277218));
#39704=CARTESIAN_POINT('',(37.03,0.2,29.9912761277218));
#39705=CARTESIAN_POINT('',(24.05,0.2,29.9912761277218));
#39706=CARTESIAN_POINT('',(36.97,0.2,29.957));
#39707=CARTESIAN_POINT('',(36.97,0.2,30.097));
#39708=CARTESIAN_POINT('',(37.03,0.2,29.957));
#39709=CARTESIAN_POINT('',(37.03,0.2,29.957));
#39710=CARTESIAN_POINT('',(37.03,0.2,30.097));
#39711=CARTESIAN_POINT('Origin',(37.03,0.2,30.097));
#39712=CARTESIAN_POINT('',(37.03,-0.2,29.9912761277218));
#39713=CARTESIAN_POINT('Origin',(37.03,0.,26.5));
#39714=CARTESIAN_POINT('',(37.03,-0.2,29.957));
#39715=CARTESIAN_POINT('',(37.03,-0.2,29.957));
#39716=CARTESIAN_POINT('',(37.03,-0.2,30.097));
#39717=CARTESIAN_POINT('Origin',(37.03,-0.2,30.097));
#39718=CARTESIAN_POINT('',(36.97,-0.2,29.9912761277218));
#39719=CARTESIAN_POINT('',(24.05,-0.2,29.9912761277218));
#39720=CARTESIAN_POINT('',(36.97,-0.2,29.957));
#39721=CARTESIAN_POINT('',(36.97,-0.2,29.957));
#39722=CARTESIAN_POINT('',(36.97,-0.2,30.097));
#39723=CARTESIAN_POINT('Origin',(36.97,-0.2,30.097));
#39724=CARTESIAN_POINT('Origin',(36.97,0.,26.5));
#39725=CARTESIAN_POINT('',(36.97,0.2,29.957));
#39726=CARTESIAN_POINT('Origin',(37.,0.,29.957));
#39727=CARTESIAN_POINT('Origin',(35.97,0.2,30.097));
#39728=CARTESIAN_POINT('',(35.97,0.2,29.9912761277218));
#39729=CARTESIAN_POINT('',(36.03,0.2,29.9912761277218));
#39730=CARTESIAN_POINT('',(24.05,0.2,29.9912761277218));
#39731=CARTESIAN_POINT('',(35.97,0.2,29.957));
#39732=CARTESIAN_POINT('',(35.97,0.2,30.097));
#39733=CARTESIAN_POINT('',(36.03,0.2,29.957));
#39734=CARTESIAN_POINT('',(36.03,0.2,29.957));
#39735=CARTESIAN_POINT('',(36.03,0.2,30.097));
#39736=CARTESIAN_POINT('Origin',(36.03,0.2,30.097));
#39737=CARTESIAN_POINT('',(36.03,-0.2,29.9912761277218));
#39738=CARTESIAN_POINT('Origin',(36.03,0.,26.5));
#39739=CARTESIAN_POINT('',(36.03,-0.2,29.957));
#39740=CARTESIAN_POINT('',(36.03,-0.2,29.957));
#39741=CARTESIAN_POINT('',(36.03,-0.2,30.097));
#39742=CARTESIAN_POINT('Origin',(36.03,-0.2,30.097));
#39743=CARTESIAN_POINT('',(35.97,-0.2,29.9912761277218));
#39744=CARTESIAN_POINT('',(24.05,-0.2,29.9912761277218));
#39745=CARTESIAN_POINT('',(35.97,-0.2,29.957));
#39746=CARTESIAN_POINT('',(35.97,-0.2,29.957));
#39747=CARTESIAN_POINT('',(35.97,-0.2,30.097));
#39748=CARTESIAN_POINT('Origin',(35.97,-0.2,30.097));
#39749=CARTESIAN_POINT('Origin',(35.97,0.,26.5));
#39750=CARTESIAN_POINT('',(35.97,0.2,29.957));
#39751=CARTESIAN_POINT('Origin',(36.,0.,29.957));
#39752=CARTESIAN_POINT('Origin',(34.97,0.2,30.097));
#39753=CARTESIAN_POINT('',(34.97,0.2,29.9912761277218));
#39754=CARTESIAN_POINT('',(35.03,0.2,29.9912761277218));
#39755=CARTESIAN_POINT('',(24.05,0.2,29.9912761277218));
#39756=CARTESIAN_POINT('',(34.97,0.2,29.957));
#39757=CARTESIAN_POINT('',(34.97,0.2,30.097));
#39758=CARTESIAN_POINT('',(35.03,0.2,29.957));
#39759=CARTESIAN_POINT('',(35.03,0.2,29.957));
#39760=CARTESIAN_POINT('',(35.03,0.2,30.097));
#39761=CARTESIAN_POINT('Origin',(35.03,0.2,30.097));
#39762=CARTESIAN_POINT('',(35.03,-0.2,29.9912761277218));
#39763=CARTESIAN_POINT('Origin',(35.03,0.,26.5));
#39764=CARTESIAN_POINT('',(35.03,-0.2,29.957));
#39765=CARTESIAN_POINT('',(35.03,-0.2,29.957));
#39766=CARTESIAN_POINT('',(35.03,-0.2,30.097));
#39767=CARTESIAN_POINT('Origin',(35.03,-0.2,30.097));
#39768=CARTESIAN_POINT('',(34.97,-0.2,29.9912761277218));
#39769=CARTESIAN_POINT('',(24.05,-0.2,29.9912761277218));
#39770=CARTESIAN_POINT('',(34.97,-0.2,29.957));
#39771=CARTESIAN_POINT('',(34.97,-0.2,29.957));
#39772=CARTESIAN_POINT('',(34.97,-0.2,30.097));
#39773=CARTESIAN_POINT('Origin',(34.97,-0.2,30.097));
#39774=CARTESIAN_POINT('Origin',(34.97,0.,26.5));
#39775=CARTESIAN_POINT('',(34.97,0.2,29.957));
#39776=CARTESIAN_POINT('Origin',(35.,0.,29.957));
#39777=CARTESIAN_POINT('Origin',(33.97,0.2,30.097));
#39778=CARTESIAN_POINT('',(33.97,0.2,29.9912761277218));
#39779=CARTESIAN_POINT('',(34.03,0.2,29.9912761277218));
#39780=CARTESIAN_POINT('',(24.05,0.2,29.9912761277218));
#39781=CARTESIAN_POINT('',(33.97,0.2,29.957));
#39782=CARTESIAN_POINT('',(33.97,0.2,30.097));
#39783=CARTESIAN_POINT('',(34.03,0.2,29.957));
#39784=CARTESIAN_POINT('',(34.03,0.2,29.957));
#39785=CARTESIAN_POINT('',(34.03,0.2,30.097));
#39786=CARTESIAN_POINT('Origin',(34.03,0.2,30.097));
#39787=CARTESIAN_POINT('',(34.03,-0.2,29.9912761277218));
#39788=CARTESIAN_POINT('Origin',(34.03,0.,26.5));
#39789=CARTESIAN_POINT('',(34.03,-0.2,29.957));
#39790=CARTESIAN_POINT('',(34.03,-0.2,29.957));
#39791=CARTESIAN_POINT('',(34.03,-0.2,30.097));
#39792=CARTESIAN_POINT('Origin',(34.03,-0.2,30.097));
#39793=CARTESIAN_POINT('',(33.97,-0.2,29.9912761277218));
#39794=CARTESIAN_POINT('',(24.05,-0.2,29.9912761277218));
#39795=CARTESIAN_POINT('',(33.97,-0.2,29.957));
#39796=CARTESIAN_POINT('',(33.97,-0.2,29.957));
#39797=CARTESIAN_POINT('',(33.97,-0.2,30.097));
#39798=CARTESIAN_POINT('Origin',(33.97,-0.2,30.097));
#39799=CARTESIAN_POINT('Origin',(33.97,0.,26.5));
#39800=CARTESIAN_POINT('',(33.97,0.2,29.957));
#39801=CARTESIAN_POINT('Origin',(34.,0.,29.957));
#39802=CARTESIAN_POINT('Origin',(32.97,0.2,30.097));
#39803=CARTESIAN_POINT('',(32.97,0.2,29.9912761277218));
#39804=CARTESIAN_POINT('',(33.03,0.2,29.9912761277218));
#39805=CARTESIAN_POINT('',(24.05,0.2,29.9912761277218));
#39806=CARTESIAN_POINT('',(32.97,0.2,29.957));
#39807=CARTESIAN_POINT('',(32.97,0.2,30.097));
#39808=CARTESIAN_POINT('',(33.03,0.2,29.957));
#39809=CARTESIAN_POINT('',(33.03,0.2,29.957));
#39810=CARTESIAN_POINT('',(33.03,0.2,30.097));
#39811=CARTESIAN_POINT('Origin',(33.03,0.2,30.097));
#39812=CARTESIAN_POINT('',(33.03,-0.2,29.9912761277218));
#39813=CARTESIAN_POINT('Origin',(33.03,0.,26.5));
#39814=CARTESIAN_POINT('',(33.03,-0.2,29.957));
#39815=CARTESIAN_POINT('',(33.03,-0.2,29.957));
#39816=CARTESIAN_POINT('',(33.03,-0.2,30.097));
#39817=CARTESIAN_POINT('Origin',(33.03,-0.2,30.097));
#39818=CARTESIAN_POINT('',(32.97,-0.2,29.9912761277218));
#39819=CARTESIAN_POINT('',(24.05,-0.2,29.9912761277218));
#39820=CARTESIAN_POINT('',(32.97,-0.2,29.957));
#39821=CARTESIAN_POINT('',(32.97,-0.2,29.957));
#39822=CARTESIAN_POINT('',(32.97,-0.2,30.097));
#39823=CARTESIAN_POINT('Origin',(32.97,-0.2,30.097));
#39824=CARTESIAN_POINT('Origin',(32.97,0.,26.5));
#39825=CARTESIAN_POINT('',(32.97,0.2,29.957));
#39826=CARTESIAN_POINT('Origin',(33.,0.,29.957));
#39827=CARTESIAN_POINT('Origin',(37.47,0.35,30.097));
#39828=CARTESIAN_POINT('',(37.47,0.35,29.9794409033636));
#39829=CARTESIAN_POINT('',(37.53,0.35,29.9794409033636));
#39830=CARTESIAN_POINT('',(24.05,0.35,29.9794409033636));
#39831=CARTESIAN_POINT('',(37.47,0.35,29.957));
#39832=CARTESIAN_POINT('',(37.47,0.35,30.097));
#39833=CARTESIAN_POINT('',(37.53,0.35,29.957));
#39834=CARTESIAN_POINT('',(37.53,0.35,29.957));
#39835=CARTESIAN_POINT('',(37.53,0.35,30.097));
#39836=CARTESIAN_POINT('Origin',(37.53,0.35,30.097));
#39837=CARTESIAN_POINT('',(37.53,-0.35,29.9794409033636));
#39838=CARTESIAN_POINT('Origin',(37.53,0.,26.5));
#39839=CARTESIAN_POINT('',(37.53,-0.35,29.957));
#39840=CARTESIAN_POINT('',(37.53,-0.35,29.957));
#39841=CARTESIAN_POINT('',(37.53,-0.35,30.097));
#39842=CARTESIAN_POINT('Origin',(37.53,-0.35,30.097));
#39843=CARTESIAN_POINT('',(37.47,-0.35,29.9794409033636));
#39844=CARTESIAN_POINT('',(24.05,-0.35,29.9794409033636));
#39845=CARTESIAN_POINT('',(37.47,-0.35,29.957));
#39846=CARTESIAN_POINT('',(37.47,-0.35,29.957));
#39847=CARTESIAN_POINT('',(37.47,-0.35,30.097));
#39848=CARTESIAN_POINT('Origin',(37.47,-0.35,30.097));
#39849=CARTESIAN_POINT('Origin',(37.47,0.,26.5));
#39850=CARTESIAN_POINT('',(37.47,0.35,29.957));
#39851=CARTESIAN_POINT('Origin',(37.5,0.,29.957));
#39852=CARTESIAN_POINT('Origin',(31.47,0.35,30.097));
#39853=CARTESIAN_POINT('',(31.47,0.35,29.9794409033636));
#39854=CARTESIAN_POINT('',(31.53,0.35,29.9794409033636));
#39855=CARTESIAN_POINT('',(24.05,0.35,29.9794409033636));
#39856=CARTESIAN_POINT('',(31.47,0.35,29.957));
#39857=CARTESIAN_POINT('',(31.47,0.35,30.097));
#39858=CARTESIAN_POINT('',(31.53,0.35,29.957));
#39859=CARTESIAN_POINT('',(31.53,0.35,29.957));
#39860=CARTESIAN_POINT('',(31.53,0.35,30.097));
#39861=CARTESIAN_POINT('Origin',(31.53,0.35,30.097));
#39862=CARTESIAN_POINT('',(31.53,-0.35,29.9794409033636));
#39863=CARTESIAN_POINT('Origin',(31.53,0.,26.5));
#39864=CARTESIAN_POINT('',(31.53,-0.35,29.957));
#39865=CARTESIAN_POINT('',(31.53,-0.35,29.957));
#39866=CARTESIAN_POINT('',(31.53,-0.35,30.097));
#39867=CARTESIAN_POINT('Origin',(31.53,-0.35,30.097));
#39868=CARTESIAN_POINT('',(31.47,-0.35,29.9794409033636));
#39869=CARTESIAN_POINT('',(24.05,-0.35,29.9794409033636));
#39870=CARTESIAN_POINT('',(31.47,-0.35,29.957));
#39871=CARTESIAN_POINT('',(31.47,-0.35,29.957));
#39872=CARTESIAN_POINT('',(31.47,-0.35,30.097));
#39873=CARTESIAN_POINT('Origin',(31.47,-0.35,30.097));
#39874=CARTESIAN_POINT('Origin',(31.47,0.,26.5));
#39875=CARTESIAN_POINT('',(31.47,0.35,29.957));
#39876=CARTESIAN_POINT('Origin',(31.5,0.,29.957));
#39877=CARTESIAN_POINT('Origin',(30.47,0.35,30.097));
#39878=CARTESIAN_POINT('',(30.47,0.35,29.9794409033636));
#39879=CARTESIAN_POINT('',(30.53,0.35,29.9794409033636));
#39880=CARTESIAN_POINT('',(24.05,0.35,29.9794409033636));
#39881=CARTESIAN_POINT('',(30.47,0.35,29.957));
#39882=CARTESIAN_POINT('',(30.47,0.35,30.097));
#39883=CARTESIAN_POINT('',(30.53,0.35,29.957));
#39884=CARTESIAN_POINT('',(30.53,0.35,29.957));
#39885=CARTESIAN_POINT('',(30.53,0.35,30.097));
#39886=CARTESIAN_POINT('Origin',(30.53,0.35,30.097));
#39887=CARTESIAN_POINT('',(30.53,-0.35,29.9794409033636));
#39888=CARTESIAN_POINT('Origin',(30.53,0.,26.5));
#39889=CARTESIAN_POINT('',(30.53,-0.35,29.957));
#39890=CARTESIAN_POINT('',(30.53,-0.35,29.957));
#39891=CARTESIAN_POINT('',(30.53,-0.35,30.097));
#39892=CARTESIAN_POINT('Origin',(30.53,-0.35,30.097));
#39893=CARTESIAN_POINT('',(30.47,-0.35,29.9794409033636));
#39894=CARTESIAN_POINT('',(24.05,-0.35,29.9794409033636));
#39895=CARTESIAN_POINT('',(30.47,-0.35,29.957));
#39896=CARTESIAN_POINT('',(30.47,-0.35,29.957));
#39897=CARTESIAN_POINT('',(30.47,-0.35,30.097));
#39898=CARTESIAN_POINT('Origin',(30.47,-0.35,30.097));
#39899=CARTESIAN_POINT('Origin',(30.47,0.,26.5));
#39900=CARTESIAN_POINT('',(30.47,0.35,29.957));
#39901=CARTESIAN_POINT('Origin',(30.5,0.,29.957));
#39902=CARTESIAN_POINT('Origin',(29.47,0.35,30.097));
#39903=CARTESIAN_POINT('',(29.47,0.35,29.9794409033636));
#39904=CARTESIAN_POINT('',(29.53,0.35,29.9794409033636));
#39905=CARTESIAN_POINT('',(24.05,0.35,29.9794409033636));
#39906=CARTESIAN_POINT('',(29.47,0.35,29.957));
#39907=CARTESIAN_POINT('',(29.47,0.35,30.097));
#39908=CARTESIAN_POINT('',(29.53,0.35,29.957));
#39909=CARTESIAN_POINT('',(29.53,0.35,29.957));
#39910=CARTESIAN_POINT('',(29.53,0.35,30.097));
#39911=CARTESIAN_POINT('Origin',(29.53,0.35,30.097));
#39912=CARTESIAN_POINT('',(29.53,-0.35,29.9794409033636));
#39913=CARTESIAN_POINT('Origin',(29.53,0.,26.5));
#39914=CARTESIAN_POINT('',(29.53,-0.35,29.957));
#39915=CARTESIAN_POINT('',(29.53,-0.35,29.957));
#39916=CARTESIAN_POINT('',(29.53,-0.35,30.097));
#39917=CARTESIAN_POINT('Origin',(29.53,-0.35,30.097));
#39918=CARTESIAN_POINT('',(29.47,-0.35,29.9794409033636));
#39919=CARTESIAN_POINT('',(24.05,-0.35,29.9794409033636));
#39920=CARTESIAN_POINT('',(29.47,-0.35,29.957));
#39921=CARTESIAN_POINT('',(29.47,-0.35,29.957));
#39922=CARTESIAN_POINT('',(29.47,-0.35,30.097));
#39923=CARTESIAN_POINT('Origin',(29.47,-0.35,30.097));
#39924=CARTESIAN_POINT('Origin',(29.47,0.,26.5));
#39925=CARTESIAN_POINT('',(29.47,0.35,29.957));
#39926=CARTESIAN_POINT('Origin',(29.5,0.,29.957));
#39927=CARTESIAN_POINT('Origin',(28.47,0.35,30.097));
#39928=CARTESIAN_POINT('',(28.47,0.35,29.9794409033636));
#39929=CARTESIAN_POINT('',(28.53,0.35,29.9794409033636));
#39930=CARTESIAN_POINT('',(24.05,0.35,29.9794409033636));
#39931=CARTESIAN_POINT('',(28.47,0.35,29.957));
#39932=CARTESIAN_POINT('',(28.47,0.35,30.097));
#39933=CARTESIAN_POINT('',(28.53,0.35,29.957));
#39934=CARTESIAN_POINT('',(28.53,0.35,29.957));
#39935=CARTESIAN_POINT('',(28.53,0.35,30.097));
#39936=CARTESIAN_POINT('Origin',(28.53,0.35,30.097));
#39937=CARTESIAN_POINT('',(28.53,-0.35,29.9794409033636));
#39938=CARTESIAN_POINT('Origin',(28.53,0.,26.5));
#39939=CARTESIAN_POINT('',(28.53,-0.35,29.957));
#39940=CARTESIAN_POINT('',(28.53,-0.35,29.957));
#39941=CARTESIAN_POINT('',(28.53,-0.35,30.097));
#39942=CARTESIAN_POINT('Origin',(28.53,-0.35,30.097));
#39943=CARTESIAN_POINT('',(28.47,-0.35,29.9794409033636));
#39944=CARTESIAN_POINT('',(24.05,-0.35,29.9794409033636));
#39945=CARTESIAN_POINT('',(28.47,-0.35,29.957));
#39946=CARTESIAN_POINT('',(28.47,-0.35,29.957));
#39947=CARTESIAN_POINT('',(28.47,-0.35,30.097));
#39948=CARTESIAN_POINT('Origin',(28.47,-0.35,30.097));
#39949=CARTESIAN_POINT('Origin',(28.47,0.,26.5));
#39950=CARTESIAN_POINT('',(28.47,0.35,29.957));
#39951=CARTESIAN_POINT('Origin',(28.5,0.,29.957));
#39952=CARTESIAN_POINT('Origin',(27.47,0.35,30.097));
#39953=CARTESIAN_POINT('',(27.47,0.35,29.9794409033636));
#39954=CARTESIAN_POINT('',(27.53,0.35,29.9794409033636));
#39955=CARTESIAN_POINT('',(24.05,0.35,29.9794409033636));
#39956=CARTESIAN_POINT('',(27.47,0.35,29.957));
#39957=CARTESIAN_POINT('',(27.47,0.35,30.097));
#39958=CARTESIAN_POINT('',(27.53,0.35,29.957));
#39959=CARTESIAN_POINT('',(27.53,0.35,29.957));
#39960=CARTESIAN_POINT('',(27.53,0.35,30.097));
#39961=CARTESIAN_POINT('Origin',(27.53,0.35,30.097));
#39962=CARTESIAN_POINT('',(27.53,-0.35,29.9794409033636));
#39963=CARTESIAN_POINT('Origin',(27.53,0.,26.5));
#39964=CARTESIAN_POINT('',(27.53,-0.35,29.957));
#39965=CARTESIAN_POINT('',(27.53,-0.35,29.957));
#39966=CARTESIAN_POINT('',(27.53,-0.35,30.097));
#39967=CARTESIAN_POINT('Origin',(27.53,-0.35,30.097));
#39968=CARTESIAN_POINT('',(27.47,-0.35,29.9794409033636));
#39969=CARTESIAN_POINT('',(24.05,-0.35,29.9794409033636));
#39970=CARTESIAN_POINT('',(27.47,-0.35,29.957));
#39971=CARTESIAN_POINT('',(27.47,-0.35,29.957));
#39972=CARTESIAN_POINT('',(27.47,-0.35,30.097));
#39973=CARTESIAN_POINT('Origin',(27.47,-0.35,30.097));
#39974=CARTESIAN_POINT('Origin',(27.47,0.,26.5));
#39975=CARTESIAN_POINT('',(27.47,0.35,29.957));
#39976=CARTESIAN_POINT('Origin',(27.5,0.,29.957));
#39977=CARTESIAN_POINT('Origin',(23.8,0.3,23.303));
#39978=CARTESIAN_POINT('',(35.2,0.3,23.0158919362339));
#39979=CARTESIAN_POINT('',(23.8,0.3,23.0158919362339));
#39980=CARTESIAN_POINT('',(24.05,0.3,23.0158919362339));
#39981=CARTESIAN_POINT('',(35.2,0.3,23.303));
#39982=CARTESIAN_POINT('',(35.2,0.3,23.303));
#39983=CARTESIAN_POINT('',(23.8,0.3,23.303));
#39984=CARTESIAN_POINT('',(35.2,0.3,23.303));
#39985=CARTESIAN_POINT('',(23.8,0.3,23.303));
#39986=CARTESIAN_POINT('Origin',(23.8,0.,23.303));
#39987=CARTESIAN_POINT('',(23.8,-0.3,23.0158919362339));
#39988=CARTESIAN_POINT('Ctrl Pts',(23.8,0.3,23.0158919362339));
#39989=CARTESIAN_POINT('Ctrl Pts',(23.7623114146691,0.3,23.0158919362339));
#39990=CARTESIAN_POINT('Ctrl Pts',(23.7221234046193,0.292464132564535,23.0152174188699));
#39991=CARTESIAN_POINT('Ctrl Pts',(23.6482151108805,0.261842283181441,23.0127828394877));
#39992=CARTESIAN_POINT('Ctrl Pts',(23.6144932470194,0.238757315731349,23.0110581162707));
#39993=CARTESIAN_POINT('Ctrl Pts',(23.5612427332329,0.185506801944792,23.0078219192499));
#39994=CARTESIAN_POINT('Ctrl Pts',(23.5381577277572,0.151784916482474,23.0060999692551));
#39995=CARTESIAN_POINT('Ctrl Pts',(23.5075358494518,0.0778765510139039,
23.0036717361649));
#39996=CARTESIAN_POINT('Ctrl Pts',(23.5,0.0376885160210923,23.003));
#39997=CARTESIAN_POINT('Ctrl Pts',(23.5,-0.0376885160210922,23.003));
#39998=CARTESIAN_POINT('Ctrl Pts',(23.5075358494518,-0.0778765510139039,
23.0036717361649));
#39999=CARTESIAN_POINT('Ctrl Pts',(23.5381577277572,-0.151784916482474,
23.0060999692551));
#40000=CARTESIAN_POINT('Ctrl Pts',(23.5612427332329,-0.185506801944792,
23.0078219192499));
#40001=CARTESIAN_POINT('Ctrl Pts',(23.6144932470194,-0.238757315731349,
23.0110581162707));
#40002=CARTESIAN_POINT('Ctrl Pts',(23.6482151108805,-0.261842283181441,
23.0127828394877));
#40003=CARTESIAN_POINT('Ctrl Pts',(23.7221234046193,-0.292464132564535,
23.0152174188699));
#40004=CARTESIAN_POINT('Ctrl Pts',(23.7623114146691,-0.299999999999999,
23.0158919362339));
#40005=CARTESIAN_POINT('Ctrl Pts',(23.8,-0.3,23.0158919362339));
#40006=CARTESIAN_POINT('',(23.8,-0.3,23.303));
#40007=CARTESIAN_POINT('Origin',(23.8,0.,23.303));
#40008=CARTESIAN_POINT('',(23.8,-0.3,23.303));
#40009=CARTESIAN_POINT('Origin',(35.2,-0.3,23.303));
#40010=CARTESIAN_POINT('',(35.2,-0.3,23.0158919362339));
#40011=CARTESIAN_POINT('',(24.05,-0.3,23.0158919362339));
#40012=CARTESIAN_POINT('',(35.2,-0.3,23.303));
#40013=CARTESIAN_POINT('',(23.8,-0.3,23.303));
#40014=CARTESIAN_POINT('',(35.2,-0.3,23.303));
#40015=CARTESIAN_POINT('Origin',(35.2,2.77555756156289E-17,23.303));
#40016=CARTESIAN_POINT('Ctrl Pts',(35.2,-0.3,23.0158919362339));
#40017=CARTESIAN_POINT('Ctrl Pts',(35.2376885853309,-0.3,23.0158919362339));
#40018=CARTESIAN_POINT('Ctrl Pts',(35.2778765953807,-0.292464132564536,
23.0152174188699));
#40019=CARTESIAN_POINT('Ctrl Pts',(35.3517848891195,-0.261842283181445,
23.0127828394877));
#40020=CARTESIAN_POINT('Ctrl Pts',(35.3855067529806,-0.238757315731349,
23.0110581162707));
#40021=CARTESIAN_POINT('Ctrl Pts',(35.4387572667671,-0.185506801944793,
23.0078219192499));
#40022=CARTESIAN_POINT('Ctrl Pts',(35.4618422722428,-0.151784916482478,
23.0060999692551));
#40023=CARTESIAN_POINT('Ctrl Pts',(35.4924641505482,-0.0778765510139092,
23.0036717361649));
#40024=CARTESIAN_POINT('Ctrl Pts',(35.5,-0.0376885160210925,23.003));
#40025=CARTESIAN_POINT('Ctrl Pts',(35.5,0.0376885160210923,23.003));
#40026=CARTESIAN_POINT('Ctrl Pts',(35.4924641505482,0.077876551013909,23.0036717361649));
#40027=CARTESIAN_POINT('Ctrl Pts',(35.4618422722428,0.151784916482478,23.0060999692551));
#40028=CARTESIAN_POINT('Ctrl Pts',(35.4387572667671,0.185506801944793,23.0078219192499));
#40029=CARTESIAN_POINT('Ctrl Pts',(35.3855067529806,0.238757315731349,23.0110581162707));
#40030=CARTESIAN_POINT('Ctrl Pts',(35.3517848891195,0.261842283181443,23.0127828394877));
#40031=CARTESIAN_POINT('Ctrl Pts',(35.2778765953807,0.292464132564536,23.0152174188699));
#40032=CARTESIAN_POINT('Ctrl Pts',(35.2376885853309,0.3,23.0158919362339));
#40033=CARTESIAN_POINT('Ctrl Pts',(35.2,0.3,23.0158919362339));
#40034=CARTESIAN_POINT('Origin',(35.2,2.77555756156289E-17,23.303));
#40035=CARTESIAN_POINT('Origin',(29.5,0.,23.303));
#40036=CARTESIAN_POINT('Origin',(12.5,0.,26.5));
#40037=CARTESIAN_POINT('',(15.,-2.,26.5));
#40038=CARTESIAN_POINT('Origin',(15.,0.,26.5));
#40039=CARTESIAN_POINT('',(10.,-2.,26.5));
#40040=CARTESIAN_POINT('',(12.5,-2.,26.5));
#40041=CARTESIAN_POINT('Origin',(10.,0.,26.5));
#40042=CARTESIAN_POINT('Origin',(10.,3.397,26.5));
#40043=CARTESIAN_POINT('',(10.,-3.397,26.5));
#40044=CARTESIAN_POINT('Origin',(10.,0.,26.5));
#40045=CARTESIAN_POINT('Origin',(10.05,0.,26.5));
#40046=CARTESIAN_POINT('',(10.1,-3.497,26.5));
#40047=CARTESIAN_POINT('Origin',(10.1,0.,26.5));
#40048=CARTESIAN_POINT('',(10.05,-3.447,26.5));
#40049=CARTESIAN_POINT('Origin',(24.05,0.,26.5));
#40050=CARTESIAN_POINT('',(24.05,-3.497,26.5));
#40051=CARTESIAN_POINT('Origin',(38.96,0.,26.5));
#40052=CARTESIAN_POINT('',(38.92,-1.5612724,26.5));
#40053=CARTESIAN_POINT('',(38.96,-1.6023112,26.5));
#40054=CARTESIAN_POINT('Origin',(38.92,0.,26.5));
#40055=CARTESIAN_POINT('Origin',(33.06,0.,26.5));
#40056=CARTESIAN_POINT('',(27.2,-1.256904,26.5));
#40057=CARTESIAN_POINT('',(33.06,-1.4090882,26.5));
#40058=CARTESIAN_POINT('Origin',(27.2,0.,26.5));
#40059=CARTESIAN_POINT('Origin',(27.2,1.1,26.5));
#40060=CARTESIAN_POINT('',(27.2,-1.1,26.5));
#40061=CARTESIAN_POINT('Origin',(27.2,0.,26.5));
#40062=CARTESIAN_POINT('Origin',(21.1,0.,26.5));
#40063=CARTESIAN_POINT('',(15.,-1.1,26.5));
#40064=CARTESIAN_POINT('',(21.1,-1.1,26.5));
#40065=CARTESIAN_POINT('Origin',(15.,0.,26.5));
#40066=CARTESIAN_POINT('Origin',(15.,2.,26.5));
#40067=CARTESIAN_POINT('',(0.,0.,0.));
#40068=CARTESIAN_POINT('Origin',(42.1471445284648,0.,26.5));
#40069=CARTESIAN_POINT('',(42.1937865301836,1.62016810220205,26.5));
#40070=CARTESIAN_POINT('',(42.1937865301836,-1.62016810220206,26.5));
#40071=CARTESIAN_POINT('Origin',(42.1937865301836,0.,26.5));
#40072=CARTESIAN_POINT('Origin',(42.1937865301836,0.,26.5));
#40073=CARTESIAN_POINT('',(42.100502526746,1.64385418552926,26.5));
#40074=CARTESIAN_POINT('',(42.1471445284648,1.63201114386566,26.5));
#40075=CARTESIAN_POINT('',(42.100502526746,-1.64385418552926,26.5));
#40076=CARTESIAN_POINT('Origin',(42.100502526746,0.,26.5));
#40077=CARTESIAN_POINT('Origin',(42.100502526746,0.,26.5));
#40078=CARTESIAN_POINT('Origin',(40.5752426299972,0.,26.5));
#40079=CARTESIAN_POINT('',(39.,-1.56235,26.5));
#40080=CARTESIAN_POINT('',(40.5752426299972,-1.60375905110103,26.5));
#40081=CARTESIAN_POINT('Origin',(39.,0.,26.5));
#40082=CARTESIAN_POINT('Origin',(42.1504852599944,0.,26.5));
#40083=CARTESIAN_POINT('',(45.,0.,26.5));
#40084=CARTESIAN_POINT('',(42.1504852599944,-1.64516810220205,26.5));
#40085=CARTESIAN_POINT('Origin',(27.25,1.1792801,26.5));
#40086=CARTESIAN_POINT('',(27.25,-1.1792801,26.5));
#40087=CARTESIAN_POINT('Origin',(27.25,0.,26.5));
#40088=CARTESIAN_POINT('Origin',(27.29,0.,26.5));
#40089=CARTESIAN_POINT('',(27.33,-1.2592801,26.5));
#40090=CARTESIAN_POINT('Origin',(27.33,0.,26.5));
#40091=CARTESIAN_POINT('',(27.29,-1.2192801,26.5));
#40092=CARTESIAN_POINT('Origin',(33.165,0.,26.5));
#40093=CARTESIAN_POINT('',(33.165,-1.41081505,26.5));
#40094=CARTESIAN_POINT('',(0.,0.,0.));
#40095=CARTESIAN_POINT('Origin',(18.,0.,26.5));
#40096=CARTESIAN_POINT('',(9.77216677763621,-0.992506281688296,26.4999529602842));
#40097=CARTESIAN_POINT('',(9.62783322236381,-0.992554123075758,26.4999819653825));
#40098=CARTESIAN_POINT('',(18.,-0.9925,26.5));
#40099=CARTESIAN_POINT('',(9.6,0.899181451069001,26.9202569089796));
#40100=CARTESIAN_POINT('Ctrl Pts',(9.77216677763621,-0.992506281688296,
26.4999529602842));
#40101=CARTESIAN_POINT('Ctrl Pts',(9.76849906417681,-0.992322713406021,
26.5573892908763));
#40102=CARTESIAN_POINT('Ctrl Pts',(9.7648313507174,-0.98724997471646,26.6148019975283));
#40103=CARTESIAN_POINT('Ctrl Pts',(9.761163637258,-0.977330565296219,26.6712121339029));
#40104=CARTESIAN_POINT('Ctrl Pts',(9.75057810175747,-0.948701758350262,
26.8340196999224));
#40105=CARTESIAN_POINT('Ctrl Pts',(9.73999256625695,-0.879701126231576,
26.9884760503927));
#40106=CARTESIAN_POINT('Ctrl Pts',(9.72940703075642,-0.777206743663004,
27.1174316127062));
#40107=CARTESIAN_POINT('Ctrl Pts',(9.71882149525589,-0.674712361094432,
27.2463871750197));
#40108=CARTESIAN_POINT('Ctrl Pts',(9.70823595975535,-0.538724228075975,
27.3498419491765));
#40109=CARTESIAN_POINT('Ctrl Pts',(9.69765042425482,-0.386683814844797,
27.4142439267999));
#40110=CARTESIAN_POINT('Ctrl Pts',(9.68706488875429,-0.234643401613619,
27.4786459044233));
#40111=CARTESIAN_POINT('Ctrl Pts',(9.67647935325376,-0.0665507081697208,
27.5039950855134));
#40112=CARTESIAN_POINT('Ctrl Pts',(9.66589381775323,0.0975834738780521,
27.4877049736369));
#40113=CARTESIAN_POINT('Ctrl Pts',(9.65530828225269,0.261717655925824,27.4714148617604));
#40114=CARTESIAN_POINT('Ctrl Pts',(9.64472274675216,0.421893326577472,27.4134854569173));
#40115=CARTESIAN_POINT('Ctrl Pts',(9.63413721125163,0.558332210706581,27.3207204680017));
#40116=CARTESIAN_POINT('Ctrl Pts',(9.6235516757511,0.694771094835691,27.2279554790861));
#40117=CARTESIAN_POINT('Ctrl Pts',(9.61296614025056,0.807473192442262,27.1003549060981));
#40118=CARTESIAN_POINT('Ctrl Pts',(9.60238060475003,0.882858904166957,26.9535801505133));
#40119=CARTESIAN_POINT('Ctrl Pts',(9.60158706983336,0.888510124595916,26.9425773161798));
#40120=CARTESIAN_POINT('Ctrl Pts',(9.60079353491668,0.893951641373926,26.9314667303586));
#40121=CARTESIAN_POINT('Ctrl Pts',(9.6,0.899181451069001,26.9202569089796));
#40122=CARTESIAN_POINT('',(9.6,-0.89914483070475,26.9202318686356));
#40123=CARTESIAN_POINT('Origin',(9.6,0.,26.5));
#40124=CARTESIAN_POINT('Ctrl Pts',(9.59999999999999,-0.899144830704751,
26.9202318686356));
#40125=CARTESIAN_POINT('Ctrl Pts',(9.60927774078793,-0.960387074776627,
26.7891955258737));
#40126=CARTESIAN_POINT('Ctrl Pts',(9.61855548157587,-0.992405952059857,
26.6445725249488));
#40127=CARTESIAN_POINT('Ctrl Pts',(9.62783322236381,-0.992554123075758,
26.4999819653825));
#40128=CARTESIAN_POINT('Origin',(18.,0.,26.5));
#40129=CARTESIAN_POINT('',(10.1721667776362,-0.992592959832253,26.4996174405759));
#40130=CARTESIAN_POINT('',(10.0278332223638,-0.992418708717116,26.5000088356422));
#40131=CARTESIAN_POINT('',(18.,-0.9925,26.5));
#40132=CARTESIAN_POINT('Ctrl Pts',(10.1721667776362,-0.992592959832253,
26.4996174405759));
#40133=CARTESIAN_POINT('Ctrl Pts',(10.1621921568499,-0.992517835256568,
26.654933495308));
#40134=CARTESIAN_POINT('Ctrl Pts',(10.1522175360635,-0.955345472933135,
26.8110036453976));
#40135=CARTESIAN_POINT('Ctrl Pts',(10.1422429152772,-0.884928666211468,
26.9497422894547));
#40136=CARTESIAN_POINT('Ctrl Pts',(10.1316573797766,-0.810199047577096,
27.0969782469332));
#40137=CARTESIAN_POINT('Ctrl Pts',(10.1210718442761,-0.698028039439853,
27.2246946822847));
#40138=CARTESIAN_POINT('Ctrl Pts',(10.1104863087756,-0.562037531190435,
27.3180407059247));
#40139=CARTESIAN_POINT('Ctrl Pts',(10.099900773275,-0.426047022941016,27.4113867295647));
#40140=CARTESIAN_POINT('Ctrl Pts',(10.0893152377745,-0.266237014579421,
27.4703623414932));
#40141=CARTESIAN_POINT('Ctrl Pts',(10.078729702274,-0.102133462578573,27.4873735628633));
#40142=CARTESIAN_POINT('Ctrl Pts',(10.0681441667734,0.0619700894222737,
27.5043847842334));
#40143=CARTESIAN_POINT('Ctrl Pts',(10.0575586312729,0.230367185062373,27.4794316150452));
#40144=CARTESIAN_POINT('Ctrl Pts',(10.0469730957724,0.382615538030601,27.4158249371804));
#40145=CARTESIAN_POINT('Ctrl Pts',(10.0363875602718,0.534863890998829,27.3522182593157));
#40146=CARTESIAN_POINT('Ctrl Pts',(10.0258020247713,0.670963501295187,27.2499580727743));
#40147=CARTESIAN_POINT('Ctrl Pts',(10.0152164892708,0.774192304741247,27.1212600859187));
#40148=CARTESIAN_POINT('Ctrl Pts',(10.0046309537702,0.877421108187307,26.9925620990631));
#40149=CARTESIAN_POINT('Ctrl Pts',(9.99404541826972,0.94777910478307,26.8374263118932));
#40150=CARTESIAN_POINT('Ctrl Pts',(9.98345988276919,0.976946047547642,26.6750804300979));
#40151=CARTESIAN_POINT('Ctrl Pts',(9.97287434726865,1.00611299031222,26.5127345483026));
#40152=CARTESIAN_POINT('Ctrl Pts',(9.96228881176813,0.994088879245598,26.3431785718819));
#40153=CARTESIAN_POINT('Ctrl Pts',(9.95170327626759,0.941865063348462,26.186540053417));
#40154=CARTESIAN_POINT('Ctrl Pts',(9.94111774076706,0.889641247451325,26.029901534952));
#40155=CARTESIAN_POINT('Ctrl Pts',(9.93053220526652,0.79721772672367,25.8861804744428));
#40156=CARTESIAN_POINT('Ctrl Pts',(9.91994666976599,0.676736285578297,25.7738447556785));
#40157=CARTESIAN_POINT('Ctrl Pts',(9.90936113426546,0.556254844432921,25.6615090369141));
#40158=CARTESIAN_POINT('Ctrl Pts',(9.89877559876493,0.407715482869826,25.5805586598948));
#40159=CARTESIAN_POINT('Ctrl Pts',(9.8881900632644,0.247669345390617,25.5391945047519));
#40160=CARTESIAN_POINT('Ctrl Pts',(9.87760452776387,0.0876232079114112,
25.4978303496091));
#40161=CARTESIAN_POINT('Ctrl Pts',(9.86701899226333,-0.0839297054839095,
25.4960524163428));
#40162=CARTESIAN_POINT('Ctrl Pts',(9.8564334567628,-0.243606213188065,25.5367364336125));
#40163=CARTESIAN_POINT('Ctrl Pts',(9.83526238576173,-0.562959228596377,
25.6181044681518));
#40164=CARTESIAN_POINT('Ctrl Pts',(9.81409131476069,-0.834806621240028,
25.869320304835));
#40165=CARTESIAN_POINT('Ctrl Pts',(9.79292024375962,-0.941079776423611,
26.1812706258213));
#40166=CARTESIAN_POINT('Ctrl Pts',(9.78600242171848,-0.975805406282986,
26.2832029657652));
#40167=CARTESIAN_POINT('Ctrl Pts',(9.77908459967735,-0.992852517217116,
26.3916199844045));
#40168=CARTESIAN_POINT('Ctrl Pts',(9.77216677763621,-0.992506281688296,
26.4999529602842));
#40169=CARTESIAN_POINT('Ctrl Pts',(9.62783322236381,-0.992554123075758,
26.4999819653825));
#40170=CARTESIAN_POINT('Ctrl Pts',(9.62916468447414,-0.99257538731433,26.4792315633208));
#40171=CARTESIAN_POINT('Ctrl Pts',(9.63049614658447,-0.99194025718962,26.4584818294063));
#40172=CARTESIAN_POINT('Ctrl Pts',(9.6318276086948,-0.99064090797148,26.4377730175542));
#40173=CARTESIAN_POINT('Ctrl Pts',(9.64243681159308,-0.980287583318831,
26.27276345024));
#40174=CARTESIAN_POINT('Ctrl Pts',(9.65304601449135,-0.927762739923163,
26.1103520399749));
#40175=CARTESIAN_POINT('Ctrl Pts',(9.66365521738962,-0.839546534340743,
25.970484223423));
#40176=CARTESIAN_POINT('Ctrl Pts',(9.6742644202879,-0.751330328758322,25.830616406871));
#40177=CARTESIAN_POINT('Ctrl Pts',(9.68487362318617,-0.627422760989149,
25.7132921840321));
#40178=CARTESIAN_POINT('Ctrl Pts',(9.69548282608444,-0.482965038876526,
25.6328393738232));
#40179=CARTESIAN_POINT('Ctrl Pts',(9.70609202898271,-0.338507316763903,
25.5523865636142));
#40180=CARTESIAN_POINT('Ctrl Pts',(9.71670123188098,-0.17349944030783,25.5088051660352));
#40181=CARTESIAN_POINT('Ctrl Pts',(9.72731043477925,-0.00814936056770701,
25.5074454729942));
#40182=CARTESIAN_POINT('Ctrl Pts',(9.73791963767753,0.157200719172416,25.5060857799532));
#40183=CARTESIAN_POINT('Ctrl Pts',(9.7485288405758,0.322893002196589,25.5469477914503));
#40184=CARTESIAN_POINT('Ctrl Pts',(9.75913804347408,0.468654544911551,25.6250217681518));
#40185=CARTESIAN_POINT('Ctrl Pts',(9.76974724637235,0.614416087626514,25.7030957448533));
#40186=CARTESIAN_POINT('Ctrl Pts',(9.78035644927062,0.740246890032266,25.8183816867594));
#40187=CARTESIAN_POINT('Ctrl Pts',(9.79096565216889,0.830742853754316,25.9567740422393));
#40188=CARTESIAN_POINT('Ctrl Pts',(9.80157485506716,0.921238817476365,26.0951663977193));
#40189=CARTESIAN_POINT('Ctrl Pts',(9.81218405796544,0.976399942514714,26.2566651667731));
#40190=CARTESIAN_POINT('Ctrl Pts',(9.82279326086371,0.989476757850026,26.4215017995226));
#40191=CARTESIAN_POINT('Ctrl Pts',(9.83340246376199,1.00255357318534,26.5863384322722));
#40192=CARTESIAN_POINT('Ctrl Pts',(9.84401166666025,0.973546078817614,26.7545129287174));
#40193=CARTESIAN_POINT('Ctrl Pts',(9.85462086955853,0.90600360183791,26.9054433464652));
#40194=CARTESIAN_POINT('Ctrl Pts',(9.8652300724568,0.838461124858205,27.056373764213));
#40195=CARTESIAN_POINT('Ctrl Pts',(9.87583927535507,0.73238366526652,27.1900601032633));
#40196=CARTESIAN_POINT('Ctrl Pts',(9.88644847825334,0.600754761208242,27.2901395554777));
#40197=CARTESIAN_POINT('Ctrl Pts',(9.89705768115162,0.469125857149964,27.3902190076921));
#40198=CARTESIAN_POINT('Ctrl Pts',(9.90766688404989,0.311945508625094,27.4566915730705));
#40199=CARTESIAN_POINT('Ctrl Pts',(9.91827608694816,0.148451062000284,27.4814218980271));
#40200=CARTESIAN_POINT('Ctrl Pts',(9.92888528984643,-0.0150433846245255,
27.5061522229836));
#40201=CARTESIAN_POINT('Ctrl Pts',(9.9394944927447,-0.184851929349274,27.4891403075182));
#40202=CARTESIAN_POINT('Ctrl Pts',(9.95010369564298,-0.340191224912641,
27.4324680853709));
#40203=CARTESIAN_POINT('Ctrl Pts',(9.96071289854125,-0.495530520476008,
27.3757958632236));
#40204=CARTESIAN_POINT('Ctrl Pts',(9.97132210143953,-0.636400566877995,
27.2794633343944));
#40205=CARTESIAN_POINT('Ctrl Pts',(9.9819313043378,-0.745560074739528,27.1552609281509));
#40206=CARTESIAN_POINT('Ctrl Pts',(9.99254050723607,-0.854719582601061,
27.0310585219074));
#40207=CARTESIAN_POINT('Ctrl Pts',(10.0031497101343,-0.932168551922139,
26.8789862382495));
#40208=CARTESIAN_POINT('Ctrl Pts',(10.0137589130326,-0.968427809645741,
26.7176564531269));
#40209=CARTESIAN_POINT('Ctrl Pts',(10.0184503494763,-0.984461813777658,
26.6463157086204));
#40210=CARTESIAN_POINT('Ctrl Pts',(10.0231417859201,-0.992441385989991,
26.5731647082902));
#40211=CARTESIAN_POINT('Ctrl Pts',(10.0278332223638,-0.992418708717116,
26.5000088356422));
#40212=CARTESIAN_POINT('Origin',(18.,0.,26.5));
#40213=CARTESIAN_POINT('',(10.5721667776362,-0.992503945737967,26.5001013395173));
#40214=CARTESIAN_POINT('',(10.4278332223638,-0.992585626431949,26.5000017565761));
#40215=CARTESIAN_POINT('',(18.,-0.9925,26.5));
#40216=CARTESIAN_POINT('Ctrl Pts',(10.5721667776362,-0.992503945737967,
26.5001013395173));
#40217=CARTESIAN_POINT('Ctrl Pts',(10.5664707850234,-0.992439806685457,
26.5888593811617));
#40218=CARTESIAN_POINT('Ctrl Pts',(10.5607747924107,-0.980556995371912,
26.67759125854));
#40219=CARTESIAN_POINT('Ctrl Pts',(10.5550787997979,-0.956986725286291,
26.7631600087317));
#40220=CARTESIAN_POINT('Ctrl Pts',(10.5444932642974,-0.913183309848331,
26.9221825188488));
#40221=CARTESIAN_POINT('Ctrl Pts',(10.5339077287969,-0.829014711658026,
27.0702804807433));
#40222=CARTESIAN_POINT('Ctrl Pts',(10.5233221932963,-0.714514616847861,
27.1890621572086));
#40223=CARTESIAN_POINT('Ctrl Pts',(10.5127366577958,-0.600014522037695,
27.3078438336738));
#40224=CARTESIAN_POINT('Ctrl Pts',(10.5021511222953,-0.455182930607668,
27.3973092247099));
#40225=CARTESIAN_POINT('Ctrl Pts',(10.4915655867947,-0.297783039914208,
27.4468132006782));
#40226=CARTESIAN_POINT('Ctrl Pts',(10.4809800512942,-0.140383149220748,
27.4963171766466));
#40227=CARTESIAN_POINT('Ctrl Pts',(10.4703945157937,0.029585040736145,27.5058597375472));
#40228=CARTESIAN_POINT('Ctrl Pts',(10.4598089802931,0.191462890804785,27.4740019279372));
#40229=CARTESIAN_POINT('Ctrl Pts',(10.4492234447926,0.353340740873424,27.4421441183272));
#40230=CARTESIAN_POINT('Ctrl Pts',(10.4386379092921,0.507128251053811,27.3688859382066));
#40231=CARTESIAN_POINT('Ctrl Pts',(10.4280523737915,0.634070607296442,27.2635648286469));
#40232=CARTESIAN_POINT('Ctrl Pts',(10.417466838291,0.761012963539074,27.1582437190873));
#40233=CARTESIAN_POINT('Ctrl Pts',(10.4068813027905,0.861110165843951,27.0208596800887));
#40234=CARTESIAN_POINT('Ctrl Pts',(10.3962957672899,0.922146658222156,26.8674403530521));
#40235=CARTESIAN_POINT('Ctrl Pts',(10.3857102317894,0.983183150600361,26.7140210260155));
#40236=CARTESIAN_POINT('Ctrl Pts',(10.3751246962889,1.00515893305189,26.5445664109409));
#40237=CARTESIAN_POINT('Ctrl Pts',(10.3645391607883,0.985453047942944,26.3810219498978));
#40238=CARTESIAN_POINT('Ctrl Pts',(10.3539536252878,0.965747162833992,26.2174774888548));
#40239=CARTESIAN_POINT('Ctrl Pts',(10.3433680897873,0.904359610164555,26.0598431818432));
#40240=CARTESIAN_POINT('Ctrl Pts',(10.3327825542867,0.80865874018317,25.9250578875996));
#40241=CARTESIAN_POINT('Ctrl Pts',(10.3221970187862,0.712957870201786,25.790272593356));
#40242=CARTESIAN_POINT('Ctrl Pts',(10.3116114832857,0.582943682908454,25.6783363118803));
#40243=CARTESIAN_POINT('Ctrl Pts',(10.3010259477851,0.434639808109102,25.6065189153853));
#40244=CARTESIAN_POINT('Ctrl Pts',(10.2798548767841,0.138032058510397,25.4628841223952));
#40245=CARTESIAN_POINT('Ctrl Pts',(10.258683805783,-0.231734441112391,25.479724869328));
#40246=CARTESIAN_POINT('Ctrl Pts',(10.237512734782,-0.514057839417016,25.6497266620276));
#40247=CARTESIAN_POINT('Ctrl Pts',(10.2269271992814,-0.655219538569327,
25.7347275583773));
#40248=CARTESIAN_POINT('Ctrl Pts',(10.2163416637809,-0.774520462392098,
25.8580187161688));
#40249=CARTESIAN_POINT('Ctrl Pts',(10.2057561282804,-0.857573150452479,
26.000945211532));
#40250=CARTESIAN_POINT('Ctrl Pts',(10.1951705927798,-0.94062583851286,26.1438717068953));
#40251=CARTESIAN_POINT('Ctrl Pts',(10.1845850572793,-0.987430290810851,
26.3064335398303));
#40252=CARTESIAN_POINT('Ctrl Pts',(10.1739995217788,-0.992188402394096,
26.4710921961006));
#40253=CARTESIAN_POINT('Ctrl Pts',(10.1733886070646,-0.992463003558845,
26.4805950120826));
#40254=CARTESIAN_POINT('Ctrl Pts',(10.1727776923504,-0.992597560980474,
26.490104811954));
#40255=CARTESIAN_POINT('Ctrl Pts',(10.1721667776362,-0.992592959832253,
26.4996174405759));
#40256=CARTESIAN_POINT('Ctrl Pts',(10.0278332223638,-0.992418708717116,
26.5000088356422));
#40257=CARTESIAN_POINT('Ctrl Pts',(10.0337509888184,-0.992390103660582,
26.4077301968285));
#40258=CARTESIAN_POINT('Ctrl Pts',(10.0396687552729,-0.979628929082159,
26.315443805554));
#40259=CARTESIAN_POINT('Ctrl Pts',(10.0455865217274,-0.95423991719696,26.2267731381084));
#40260=CARTESIAN_POINT('Ctrl Pts',(10.0561957246257,-0.908723220898453,
26.0678068947998));
#40261=CARTESIAN_POINT('Ctrl Pts',(10.066804927524,-0.822620282175313,25.92046169477));
#40262=CARTESIAN_POINT('Ctrl Pts',(10.0774141304222,-0.7064693994913,25.8027713948326));
#40263=CARTESIAN_POINT('Ctrl Pts',(10.0880233333205,-0.590318516807288,
25.6850810948951));
#40264=CARTESIAN_POINT('Ctrl Pts',(10.0986325362188,-0.444119690162403,
25.5970456950502));
#40265=CARTESIAN_POINT('Ctrl Pts',(10.1092417391171,-0.28576649020178,25.5494400305557));
#40266=CARTESIAN_POINT('Ctrl Pts',(10.1198509420153,-0.127413290241156,
25.5018343660612));
#40267=CARTESIAN_POINT('Ctrl Pts',(10.1304601449136,0.0430942830352055,
25.4946584369172));
#40268=CARTESIAN_POINT('Ctrl Pts',(10.1410693478119,0.204887472275318,25.5287905151852));
#40269=CARTESIAN_POINT('Ctrl Pts',(10.1516785507101,0.366680661515429,25.5629225934533));
#40270=CARTESIAN_POINT('Ctrl Pts',(10.1622877536084,0.519759466719291,25.6383626791333));
#40271=CARTESIAN_POINT('Ctrl Pts',(10.1728969565067,0.645388267268235,25.7458775125298));
#40272=CARTESIAN_POINT('Ctrl Pts',(10.183506159405,0.77101706781718,25.8533923459262));
#40273=CARTESIAN_POINT('Ctrl Pts',(10.1941153623032,0.869195863711207,25.9929819270389));
#40274=CARTESIAN_POINT('Ctrl Pts',(10.2047245652015,0.927908358035644,26.1475616086697));
#40275=CARTESIAN_POINT('Ctrl Pts',(10.2153337680998,0.986620852360081,26.3021412903005));
#40276=CARTESIAN_POINT('Ctrl Pts',(10.2259429709981,1.00586704511493,26.4717110724493));
#40277=CARTESIAN_POINT('Ctrl Pts',(10.2365521738963,0.983291356083112,26.6355169733609));
#40278=CARTESIAN_POINT('Ctrl Pts',(10.2471613767946,0.960715667051297,26.7993228742725));
#40279=CARTESIAN_POINT('Ctrl Pts',(10.2577705796929,0.896318096232822,26.9573648939469));
#40280=CARTESIAN_POINT('Ctrl Pts',(10.2683797825912,0.797980390449239,27.0902999554258));
#40281=CARTESIAN_POINT('Ctrl Pts',(10.2789889854894,0.699642684665656,27.2232350169047));
#40282=CARTESIAN_POINT('Ctrl Pts',(10.2895981883877,0.567364843916966,27.331063120188));
#40283=CARTESIAN_POINT('Ctrl Pts',(10.300207391286,0.417336615681909,27.4005869697607));
#40284=CARTESIAN_POINT('Ctrl Pts',(10.3108165941842,0.267308387446851,27.4701108193334));
#40285=CARTESIAN_POINT('Ctrl Pts',(10.3214257970825,0.0995297717254275,
27.5013304151955));
#40286=CARTESIAN_POINT('Ctrl Pts',(10.3320349999808,-0.0654644734564326,
27.4904247289211));
#40287=CARTESIAN_POINT('Ctrl Pts',(10.3426442028791,-0.230458718638292,
27.4795190426466));
#40288=CARTESIAN_POINT('Ctrl Pts',(10.3532534057773,-0.392668593280588,
27.4264880742357));
#40289=CARTESIAN_POINT('Ctrl Pts',(10.3638626086756,-0.532240908742537,
27.3378223892708));
#40290=CARTESIAN_POINT('Ctrl Pts',(10.3744718115739,-0.671813224204487,
27.2491567043058));
#40291=CARTESIAN_POINT('Ctrl Pts',(10.3850810144721,-0.788747980486091,
27.1248563027868));
#40292=CARTESIAN_POINT('Ctrl Pts',(10.3956902173704,-0.868733300534966,
26.9801345576685));
#40293=CARTESIAN_POINT('Ctrl Pts',(10.4062994202687,-0.94871862058384,26.8354128125502));
#40294=CARTESIAN_POINT('Ctrl Pts',(10.416908623167,-0.991754504399986,26.6702697238326));
#40295=CARTESIAN_POINT('Ctrl Pts',(10.4275178260652,-0.992573704711812,
26.5049174821022));
#40296=CARTESIAN_POINT('Ctrl Pts',(10.4276229581648,-0.992581822593009,
26.5032789208926));
#40297=CARTESIAN_POINT('Ctrl Pts',(10.4277280902643,-0.992585794856245,
26.5016403391444));
#40298=CARTESIAN_POINT('Ctrl Pts',(10.4278332223638,-0.992585626431949,
26.5000017565761));
#40299=CARTESIAN_POINT('Origin',(18.,0.,26.5));
#40300=CARTESIAN_POINT('',(10.9721667776362,-0.9925,26.5));
#40301=CARTESIAN_POINT('',(10.8278332223638,-0.992422357680272,26.4999883264764));
#40302=CARTESIAN_POINT('',(18.,-0.9925,26.5));
#40303=CARTESIAN_POINT('Ctrl Pts',(10.9721667776362,-0.992583538475113,
26.5000383753598));
#40304=CARTESIAN_POINT('Ctrl Pts',(10.970749413197,-0.992612646059146,26.5221334010504));
#40305=CARTESIAN_POINT('Ctrl Pts',(10.9693320487579,-0.991897265306533,
26.5442263779092));
#40306=CARTESIAN_POINT('Ctrl Pts',(10.9679146843187,-0.990427353666401,
26.5662680261881));
#40307=CARTESIAN_POINT('Ctrl Pts',(10.9573291488181,-0.979449371279416,
26.7308852861515));
#40308=CARTESIAN_POINT('Ctrl Pts',(10.9467436133176,-0.926385197682136,
26.8926395428142));
#40309=CARTESIAN_POINT('Ctrl Pts',(10.9361580778171,-0.837954139517956,
27.0319425118404));
#40310=CARTESIAN_POINT('Ctrl Pts',(10.9255725423166,-0.749523081353776,
27.1712454808666));
#40311=CARTESIAN_POINT('Ctrl Pts',(10.914987006816,-0.625725138622696,27.2880971622564));
#40312=CARTESIAN_POINT('Ctrl Pts',(10.9044014713155,-0.48142731992349,27.3680815225639));
#40313=CARTESIAN_POINT('Ctrl Pts',(10.8938159358149,-0.337129501224285,
27.4480658828714));
#40314=CARTESIAN_POINT('Ctrl Pts',(10.8832304003144,-0.172331806556954,
27.4911829220966));
#40315=CARTESIAN_POINT('Ctrl Pts',(10.8726448648139,-0.00739179261613836,
27.4924828179735));
#40316=CARTESIAN_POINT('Ctrl Pts',(10.8620593293134,0.157548221324677,27.4937827138503));
#40317=CARTESIAN_POINT('Ctrl Pts',(10.8514737938128,0.322630554538978,27.4532654663788));
#40318=CARTESIAN_POINT('Ctrl Pts',(10.8408882583123,0.468184939661327,27.3753112215794));
#40319=CARTESIAN_POINT('Ctrl Pts',(10.8303027228118,0.613739324783676,27.29735697678));
#40320=CARTESIAN_POINT('Ctrl Pts',(10.8197171873112,0.739765761814074,27.1819657346527));
#40321=CARTESIAN_POINT('Ctrl Pts',(10.8091316518107,0.830115089366124,27.0442264459477));
#40322=CARTESIAN_POINT('Ctrl Pts',(10.7985461163102,0.920464416918174,26.9064871572428));
#40323=CARTESIAN_POINT('Ctrl Pts',(10.7879605808096,0.975136634991876,26.7463998219603));
#40324=CARTESIAN_POINT('Ctrl Pts',(10.7773750453091,0.988846963069828,26.581664400842));
#40325=CARTESIAN_POINT('Ctrl Pts',(10.7667895098086,1.00255729114778,26.4169289797236));
#40326=CARTESIAN_POINT('Ctrl Pts',(10.756203974308,0.975305729229982,26.2475454727695));
#40327=CARTESIAN_POINT('Ctrl Pts',(10.7456184388075,0.908211509398971,26.097045826974));
#40328=CARTESIAN_POINT('Ctrl Pts',(10.7244473678064,0.774023069736951,25.7960465353831));
#40329=CARTESIAN_POINT('Ctrl Pts',(10.7032762968054,0.480463998422085,25.5705826884271));
#40330=CARTESIAN_POINT('Ctrl Pts',(10.6821052258043,0.155036732944931,25.5185807099911));
#40331=CARTESIAN_POINT('Ctrl Pts',(10.6715196903038,-0.00767689979364622,
25.4925797207731));
#40332=CARTESIAN_POINT('Ctrl Pts',(10.6609341548032,-0.178357581072796,
25.5099441986851));
#40333=CARTESIAN_POINT('Ctrl Pts',(10.6503486193027,-0.333981058544879,
25.5656852547077));
#40334=CARTESIAN_POINT('Ctrl Pts',(10.6397630838022,-0.489604536016962,
25.6214263107303));
#40335=CARTESIAN_POINT('Ctrl Pts',(10.6291775483016,-0.630170809681978,
25.7155439448637));
#40336=CARTESIAN_POINT('Ctrl Pts',(10.6185920128011,-0.739942200305901,
25.8383663957533));
#40337=CARTESIAN_POINT('Ctrl Pts',(10.6080064773006,-0.849713590929822,
25.961188846643));
#40338=CARTESIAN_POINT('Ctrl Pts',(10.5974209418001,-0.928690098512649,
26.1127161142891));
#40339=CARTESIAN_POINT('Ctrl Pts',(10.5868354062995,-0.966459235961256,
26.273453277282));
#40340=CARTESIAN_POINT('Ctrl Pts',(10.5819458634118,-0.983905100403322,
26.3476990489836));
#40341=CARTESIAN_POINT('Ctrl Pts',(10.577056320524,-0.992559003858536,26.423909834233));
#40342=CARTESIAN_POINT('Ctrl Pts',(10.5721667776362,-0.992503945737967,
26.5001013395173));
#40343=CARTESIAN_POINT('Ctrl Pts',(10.4278332223638,-0.992585626431949,
26.5000017565761));
#40344=CARTESIAN_POINT('Ctrl Pts',(10.4383372931626,-0.992568798643581,
26.3362859420382));
#40345=CARTESIAN_POINT('Ctrl Pts',(10.4488413639613,-0.951217054403849,
26.1725619396382));
#40346=CARTESIAN_POINT('Ctrl Pts',(10.4593454347601,-0.873447975304868,
26.028496685744));
#40347=CARTESIAN_POINT('Ctrl Pts',(10.4699546376583,-0.794900528778586,
25.8829895258591));
#40348=CARTESIAN_POINT('Ctrl Pts',(10.4805638405566,-0.679203118918512,
25.7575366008324));
#40349=CARTESIAN_POINT('Ctrl Pts',(10.4911730434549,-0.540516181474807,
25.6674923432889));
#40350=CARTESIAN_POINT('Ctrl Pts',(10.5017822463531,-0.401829244031103,
25.5774480857455));
#40351=CARTESIAN_POINT('Ctrl Pts',(10.5123914492514,-0.24015277900377,25.5228124956853));
#40352=CARTESIAN_POINT('Ctrl Pts',(10.5230006521497,-0.0752746900067089,
25.5102725314703));
#40353=CARTESIAN_POINT('Ctrl Pts',(10.533609855048,0.0896033989903517,25.4977325672554));
#40354=CARTESIAN_POINT('Ctrl Pts',(10.5442190579462,0.257683111957139,25.5272882288857));
#40355=CARTESIAN_POINT('Ctrl Pts',(10.5548282608445,0.408392839046391,25.5953221402432));
#40356=CARTESIAN_POINT('Ctrl Pts',(10.5654374637428,0.559102566135641,25.6633560516006));
#40357=CARTESIAN_POINT('Ctrl Pts',(10.5760466666411,0.692442307347355,25.7698682126851));
#40358=CARTESIAN_POINT('Ctrl Pts',(10.5866558695393,0.792092346966023,25.9018223885868));
#40359=CARTESIAN_POINT('Ctrl Pts',(10.5972650724376,0.891742386584692,26.0337765644886));
#40360=CARTESIAN_POINT('Ctrl Pts',(10.6078742753359,0.957702724610315,26.1911727552075));
#40361=CARTESIAN_POINT('Ctrl Pts',(10.6184834782341,0.981900344286195,26.3547469284009));
#40362=CARTESIAN_POINT('Ctrl Pts',(10.6290926811324,1.00609796396208,26.5183211015943));
#40363=CARTESIAN_POINT('Ctrl Pts',(10.6397018840307,0.988532865288214,26.6880732572622));
#40364=CARTESIAN_POINT('Ctrl Pts',(10.650311086929,0.93135487557259,26.8432270919747));
#40365=CARTESIAN_POINT('Ctrl Pts',(10.6609202898272,0.874176885856967,26.9983809266871));
#40366=CARTESIAN_POINT('Ctrl Pts',(10.6715294927255,0.777386005099581,27.1389364404442));
#40367=CARTESIAN_POINT('Ctrl Pts',(10.6821386956238,0.652828661405759,27.2476907647988));
#40368=CARTESIAN_POINT('Ctrl Pts',(10.6927478985221,0.528271317711936,27.3564450891534));
#40369=CARTESIAN_POINT('Ctrl Pts',(10.7033571014203,0.375947511081676,27.4333982241057));
#40370=CARTESIAN_POINT('Ctrl Pts',(10.7139663043186,0.214500454696508,27.4691317226535));
#40371=CARTESIAN_POINT('Ctrl Pts',(10.7245755072169,0.0530533983113431,
27.5048652212012));
#40372=CARTESIAN_POINT('Ctrl Pts',(10.7351847101151,-0.11751690782873,27.4993790833445));
#40373=CARTESIAN_POINT('Ctrl Pts',(10.7457939130134,-0.27633402523292,27.4533447683901));
#40374=CARTESIAN_POINT('Ctrl Pts',(10.7564031159117,-0.43515114263711,27.4073104534357));
#40375=CARTESIAN_POINT('Ctrl Pts',(10.76701231881,-0.582215071305418,27.3207279613836));
#40376=CARTESIAN_POINT('Ctrl Pts',(10.7776215217082,-0.699526364965285,
27.2041942953736));
#40377=CARTESIAN_POINT('Ctrl Pts',(10.7882307246065,-0.816837658625152,
27.0876606293635));
#40378=CARTESIAN_POINT('Ctrl Pts',(10.7988399275048,-0.904396317276578,
26.9411757893955));
#40379=CARTESIAN_POINT('Ctrl Pts',(10.809449130403,-0.951485862811279,26.782668345926));
#40380=CARTESIAN_POINT('Ctrl Pts',(10.8155771610566,-0.978685472552665,
26.6911121299014));
#40381=CARTESIAN_POINT('Ctrl Pts',(10.8217051917102,-0.992383022265051,
26.5955447087458));
#40382=CARTESIAN_POINT('Ctrl Pts',(10.8278332223638,-0.992422357680272,
26.4999883264764));
#40383=CARTESIAN_POINT('Origin',(18.,0.,26.5));
#40384=CARTESIAN_POINT('',(11.3721667776362,-0.9925,26.5));
#40385=CARTESIAN_POINT('',(11.2278332223638,-0.992543914931681,26.5000214785174));
#40386=CARTESIAN_POINT('',(18.,-0.9925,26.5));
#40387=CARTESIAN_POINT('Ctrl Pts',(11.3721667776362,-0.9925,26.5));
#40388=CARTESIAN_POINT('Ctrl Pts',(11.3554259338597,-0.992500000000001,
26.7609923249229));
#40389=CARTESIAN_POINT('Ctrl Pts',(11.3386850900831,-0.884539443097409,
27.0203491301747));
#40390=CARTESIAN_POINT('Ctrl Pts',(11.3219442463066,-0.699346033936908,
27.2042523516586));
#40391=CARTESIAN_POINT('Ctrl Pts',(11.3052034025301,-0.514152624776407,
27.3881555731426));
#40392=CARTESIAN_POINT('Ctrl Pts',(11.2884625587535,-0.254047408344448,
27.4943003359057));
#40393=CARTESIAN_POINT('Ctrl Pts',(11.271721714977,0.00693853867348876,
27.4924757461425));
#40394=CARTESIAN_POINT('Ctrl Pts',(11.2549808712005,0.267924485691426,27.4906511563793));
#40395=CARTESIAN_POINT('Ctrl Pts',(11.238240027424,0.52652020388806,27.3808800818309));
#40396=CARTESIAN_POINT('Ctrl Pts',(11.2214991836474,0.709124249559321,27.1944055361868));
#40397=CARTESIAN_POINT('Ctrl Pts',(11.2047583398709,0.891728295230581,27.0079309905428));
#40398=CARTESIAN_POINT('Ctrl Pts',(11.1880174960943,0.996052076106193,26.7470900753838));
#40399=CARTESIAN_POINT('Ctrl Pts',(11.1712766523178,0.992402985755318,26.486123261769));
#40400=CARTESIAN_POINT('Ctrl Pts',(11.1545358085413,0.988753895404444,26.2251564481542));
#40401=CARTESIAN_POINT('Ctrl Pts',(11.1377949647647,0.877177668191511,25.9673344556903));
#40402=CARTESIAN_POINT('Ctrl Pts',(11.1210541209882,0.689431099871663,25.7860385104715));
#40403=CARTESIAN_POINT('Ctrl Pts',(11.1043132772117,0.501684531551814,25.6047425652527));
#40404=CARTESIAN_POINT('Ctrl Pts',(11.0875724334351,0.240120666075684,25.5022448650135));
#40405=CARTESIAN_POINT('Ctrl Pts',(11.0708315896586,-0.0208142595729385,
25.5077182776054));
#40406=CARTESIAN_POINT('Ctrl Pts',(11.0540907458821,-0.281749185221561,
25.5131916901973));
#40407=CARTESIAN_POINT('Ctrl Pts',(11.0373499021056,-0.538784851090619,
25.6265676168678));
#40408=CARTESIAN_POINT('Ctrl Pts',(11.020609058329,-0.718763835149583,25.8155770318867));
#40409=CARTESIAN_POINT('Ctrl Pts',(11.0044616314314,-0.892363059118819,
25.9978865828696));
#40410=CARTESIAN_POINT('Ctrl Pts',(10.9883142045338,-0.9925,26.248259135335));
#40411=CARTESIAN_POINT('Ctrl Pts',(10.9721667776362,-0.9925,26.5));
#40412=CARTESIAN_POINT('Ctrl Pts',(10.8278332223638,-0.992422357680272,
26.4999883264764));
#40413=CARTESIAN_POINT('Ctrl Pts',(10.8323143946085,-0.992451122022502,
26.4301119449382));
#40414=CARTESIAN_POINT('Ctrl Pts',(10.8367955668532,-0.985176313957699,
26.360241466317));
#40415=CARTESIAN_POINT('Ctrl Pts',(10.8412767390979,-0.970536872194566,
26.2919497161044));
#40416=CARTESIAN_POINT('Ctrl Pts',(10.8518859419961,-0.935877903625177,
26.1302685767232));
#40417=CARTESIAN_POINT('Ctrl Pts',(10.8624951448944,-0.859939534068422,
25.9774363449317));
#40418=CARTESIAN_POINT('Ctrl Pts',(10.8731043477927,-0.752016011374463,
25.8521584610766));
#40419=CARTESIAN_POINT('Ctrl Pts',(10.883713550691,-0.644092488680505,25.7268805772214));
#40420=CARTESIAN_POINT('Ctrl Pts',(10.8943227535892,-0.504183812849344,
25.6291570413026));
#40421=CARTESIAN_POINT('Ctrl Pts',(10.9049319564875,-0.34941368454973,25.5709484309428));
#40422=CARTESIAN_POINT('Ctrl Pts',(10.9155411593858,-0.194643556250115,
25.512739820583));
#40423=CARTESIAN_POINT('Ctrl Pts',(10.926150362284,-0.0250119754820468,
25.4940461357822));
#40424=CARTESIAN_POINT('Ctrl Pts',(10.9367595651823,0.138719511726088,25.5171553337456));
#40425=CARTESIAN_POINT('Ctrl Pts',(10.9473687680806,0.302450998934223,25.540264531709));
#40426=CARTESIAN_POINT('Ctrl Pts',(10.9579779709789,0.460282392582425,25.6051766124364));
#40427=CARTESIAN_POINT('Ctrl Pts',(10.9685871738771,0.592896394976983,25.7039468574639));
#40428=CARTESIAN_POINT('Ctrl Pts',(10.9791963767754,0.72551039737154,25.8027171024914));
#40429=CARTESIAN_POINT('Ctrl Pts',(10.9898055796737,0.832907008512454,25.935345511819));
#40430=CARTESIAN_POINT('Ctrl Pts',(11.0004147825719,0.901941743891598,26.0855994310525));
#40431=CARTESIAN_POINT('Ctrl Pts',(11.0110239854702,0.970976479270744,26.235853350286));
#40432=CARTESIAN_POINT('Ctrl Pts',(11.0216331883685,1.00164933888812,26.4037327794254));
#40433=CARTESIAN_POINT('Ctrl Pts',(11.0322423912668,0.990206210544303,26.5686906217598));
#40434=CARTESIAN_POINT('Ctrl Pts',(11.042851594165,0.978763082200488,26.7336484640941));
#40435=CARTESIAN_POINT('Ctrl Pts',(11.0534607970633,0.925203965895484,26.8956847196234));
#40436=CARTESIAN_POINT('Ctrl Pts',(11.0640699999616,0.836084068232749,27.034967449258));
#40437=CARTESIAN_POINT('Ctrl Pts',(11.0746792028599,0.746964170570011,27.1742501788927));
#40438=CARTESIAN_POINT('Ctrl Pts',(11.0852884057581,0.622283491549541,27.2907793826328));
#40439=CARTESIAN_POINT('Ctrl Pts',(11.0958976086564,0.477301947070334,27.3702928198262));
#40440=CARTESIAN_POINT('Ctrl Pts',(11.1065068115547,0.332320402591129,27.4498062570197));
#40441=CARTESIAN_POINT('Ctrl Pts',(11.1171160144529,0.167037992653186,27.4923039276666));
#40442=CARTESIAN_POINT('Ctrl Pts',(11.1277252173512,0.00168395963031208,
27.4925844574636));
#40443=CARTESIAN_POINT('Ctrl Pts',(11.1383344202495,-0.163670073392562,
27.4928649872605));
#40444=CARTESIAN_POINT('Ctrl Pts',(11.1489436231478,-0.329095729500368,
27.4509283762076));
#40445=CARTESIAN_POINT('Ctrl Pts',(11.159552826046,-0.474346234136107,27.3719073294102));
#40446=CARTESIAN_POINT('Ctrl Pts',(11.1701620289443,-0.619596738771846,
27.2928862826127));
#40447=CARTESIAN_POINT('Ctrl Pts',(11.1807712318426,-0.744672091935519,
27.1767808000708));
#40448=CARTESIAN_POINT('Ctrl Pts',(11.1913804347409,-0.834264072775994,
27.0378012623576));
#40449=CARTESIAN_POINT('Ctrl Pts',(11.2019896376391,-0.92385605361647,26.8988217246444));
#40450=CARTESIAN_POINT('Ctrl Pts',(11.2125988405374,-0.977964662133747,
26.7369681317599));
#40451=CARTESIAN_POINT('Ctrl Pts',(11.2232080434357,-0.989967438281312,
26.5720500663497));
#40452=CARTESIAN_POINT('Ctrl Pts',(11.224749769745,-0.991711678253884,26.5480842205861));
#40453=CARTESIAN_POINT('Ctrl Pts',(11.2262914960544,-0.992566734892839,
26.5240536598473));
#40454=CARTESIAN_POINT('Ctrl Pts',(11.2278332223638,-0.992543914931681,
26.5000214785174));
#40455=CARTESIAN_POINT('Origin',(18.,0.,26.5));
#40456=CARTESIAN_POINT('',(11.7721667776362,-0.992366447419476,26.5000655238227));
#40457=CARTESIAN_POINT('',(11.6278332223638,-0.992471224471742,26.4999749790724));
#40458=CARTESIAN_POINT('',(18.,-0.9925,26.5));
#40459=CARTESIAN_POINT('Ctrl Pts',(11.7721667776362,-0.9925,26.5));
#40460=CARTESIAN_POINT('Ctrl Pts',(11.7554259338597,-0.992499999999996,
26.7609923249229));
#40461=CARTESIAN_POINT('Ctrl Pts',(11.7386850900831,-0.8845394430974,27.0203491301747));
#40462=CARTESIAN_POINT('Ctrl Pts',(11.7219442463066,-0.699346033936895,
27.2042523516586));
#40463=CARTESIAN_POINT('Ctrl Pts',(11.7052034025301,-0.514152624776391,
27.3881555731426));
#40464=CARTESIAN_POINT('Ctrl Pts',(11.6884625587535,-0.25404740834443,27.4943003359057));
#40465=CARTESIAN_POINT('Ctrl Pts',(11.671721714977,0.00693853867350669,
27.4924757461425));
#40466=CARTESIAN_POINT('Ctrl Pts',(11.6549808712005,0.267924485691444,27.4906511563793));
#40467=CARTESIAN_POINT('Ctrl Pts',(11.6382400274239,0.526520203888076,27.3808800818308));
#40468=CARTESIAN_POINT('Ctrl Pts',(11.6214991836474,0.709124249559333,27.1944055361868));
#40469=CARTESIAN_POINT('Ctrl Pts',(11.6047583398709,0.89172829523059,27.0079309905428));
#40470=CARTESIAN_POINT('Ctrl Pts',(11.5880174960943,0.996052076106197,26.7470900753838));
#40471=CARTESIAN_POINT('Ctrl Pts',(11.5712766523178,0.992402985755318,26.486123261769));
#40472=CARTESIAN_POINT('Ctrl Pts',(11.5545358085413,0.988753895404439,26.2251564481542));
#40473=CARTESIAN_POINT('Ctrl Pts',(11.5377949647647,0.877177668191501,25.9673344556903));
#40474=CARTESIAN_POINT('Ctrl Pts',(11.5210541209882,0.68943109987165,25.7860385104715));
#40475=CARTESIAN_POINT('Ctrl Pts',(11.5043132772117,0.501684531551798,25.6047425652527));
#40476=CARTESIAN_POINT('Ctrl Pts',(11.4875724334351,0.240120666075666,25.5022448650134));
#40477=CARTESIAN_POINT('Ctrl Pts',(11.4708315896586,-0.0208142595729564,
25.5077182776054));
#40478=CARTESIAN_POINT('Ctrl Pts',(11.4540907458821,-0.281749185221578,
25.5131916901973));
#40479=CARTESIAN_POINT('Ctrl Pts',(11.4373499021055,-0.538784851090635,
25.6265676168679));
#40480=CARTESIAN_POINT('Ctrl Pts',(11.420609058329,-0.718763835149595,25.8155770318867));
#40481=CARTESIAN_POINT('Ctrl Pts',(11.4044616314314,-0.892363059118823,
25.9978865828696));
#40482=CARTESIAN_POINT('Ctrl Pts',(11.3883142045338,-0.9925,26.248259135335));
#40483=CARTESIAN_POINT('Ctrl Pts',(11.3721667776362,-0.9925,26.5));
#40484=CARTESIAN_POINT('Ctrl Pts',(11.2278332223638,-0.992543914931681,
26.5000214785174));
#40485=CARTESIAN_POINT('Ctrl Pts',(11.2369006989527,-0.992409702093583,
26.3586791142707));
#40486=CARTESIAN_POINT('Ctrl Pts',(11.2459681755416,-0.961909195313563,
26.217280692776));
#40487=CARTESIAN_POINT('Ctrl Pts',(11.2550356521305,-0.903342642445217,
26.0886621689434));
#40488=CARTESIAN_POINT('Ctrl Pts',(11.2656448550288,-0.834818126683708,
25.9381748748832));
#40489=CARTESIAN_POINT('Ctrl Pts',(11.276254057927,-0.727872151382838,25.8051828246989));
#40490=CARTESIAN_POINT('Ctrl Pts',(11.2868632608253,-0.595594046835387,
25.7059631795109));
#40491=CARTESIAN_POINT('Ctrl Pts',(11.2974724637236,-0.463315942287936,
25.6067435343229));
#40492=CARTESIAN_POINT('Ctrl Pts',(11.3080816666219,-0.305705708493902,
25.5412962941313));
#40493=CARTESIAN_POINT('Ctrl Pts',(11.3186908695201,-0.142053574953264,
25.5176316766298));
#40494=CARTESIAN_POINT('Ctrl Pts',(11.3293000724184,0.0215985585873745,
25.4939670591282));
#40495=CARTESIAN_POINT('Ctrl Pts',(11.3399092753167,0.191292591874618,25.5120850643167));
#40496=CARTESIAN_POINT('Ctrl Pts',(11.3505184782149,0.346259335192242,25.5697681935611));
#40497=CARTESIAN_POINT('Ctrl Pts',(11.3611276811132,0.501226078509868,25.6274513228055));
#40498=CARTESIAN_POINT('Ctrl Pts',(11.3717368840115,0.641465531857871,25.7246995761059));
#40499=CARTESIAN_POINT('Ctrl Pts',(11.3823460869098,0.749813510050352,25.8496105466229));
#40500=CARTESIAN_POINT('Ctrl Pts',(11.392955289808,0.858161488242832,25.9745215171399));
#40501=CARTESIAN_POINT('Ctrl Pts',(11.4035644927063,0.934617991279787,26.1270952048736));
#40502=CARTESIAN_POINT('Ctrl Pts',(11.4141736956046,0.969825355925495,26.288657813198));
#40503=CARTESIAN_POINT('Ctrl Pts',(11.4247828985028,1.0050327205712,26.4502204215225));
#40504=CARTESIAN_POINT('Ctrl Pts',(11.4353921014011,0.998990946825663,26.6207719504377));
#40505=CARTESIAN_POINT('Ctrl Pts',(11.4460013042994,0.952439499375482,26.7794382596347));
#40506=CARTESIAN_POINT('Ctrl Pts',(11.4566105071977,0.9058880519253,26.9381045688316));
#40507=CARTESIAN_POINT('Ctrl Pts',(11.4672197100959,0.818826930770477,27.0848856583103));
#40508=CARTESIAN_POINT('Ctrl Pts',(11.4778289129942,0.70191171941707,27.2018166990484));
#40509=CARTESIAN_POINT('Ctrl Pts',(11.4884381158925,0.584996508063663,27.3187477397865));
#40510=CARTESIAN_POINT('Ctrl Pts',(11.4990473187907,0.438227206511674,27.4058287317839));
#40511=CARTESIAN_POINT('Ctrl Pts',(11.509656521689,0.279567201035806,27.4524016595026));
#40512=CARTESIAN_POINT('Ctrl Pts',(11.5202657245873,0.120907195559937,27.4989745872213));
#40513=CARTESIAN_POINT('Ctrl Pts',(11.5308749274856,-0.0496435138398082,
27.5050394506614));
#40514=CARTESIAN_POINT('Ctrl Pts',(11.5414841303839,-0.211210887156589,
27.4698539591427));
#40515=CARTESIAN_POINT('Ctrl Pts',(11.5520933332821,-0.372778260473371,
27.434668467624));
#40516=CARTESIAN_POINT('Ctrl Pts',(11.5627025361804,-0.52536229770719,27.3582326211465));
#40517=CARTESIAN_POINT('Ctrl Pts',(11.5733117390787,-0.650287935536204,
27.2499015547486));
#40518=CARTESIAN_POINT('Ctrl Pts',(11.5839209419769,-0.775213573365219,
27.1415704883507));
#40519=CARTESIAN_POINT('Ctrl Pts',(11.5945301448752,-0.87248081178943,27.0013442020323));
#40520=CARTESIAN_POINT('Ctrl Pts',(11.6051393477735,-0.930184920342645,
26.8463852694405));
#40521=CARTESIAN_POINT('Ctrl Pts',(11.6127039726369,-0.971329381285666,
26.7358957062249));
#40522=CARTESIAN_POINT('Ctrl Pts',(11.6202685975004,-0.992359773820853,
26.617916001154));
#40523=CARTESIAN_POINT('Ctrl Pts',(11.6278332223638,-0.992471224471742,
26.4999749790724));
#40524=CARTESIAN_POINT('Origin',(18.,0.,26.5));
#40525=CARTESIAN_POINT('',(12.1721667776362,-0.992619537425882,26.499861786204));
#40526=CARTESIAN_POINT('',(12.0278332223638,-0.992474254593845,26.5000252858765));
#40527=CARTESIAN_POINT('',(18.,-0.9925,26.5));
#40528=CARTESIAN_POINT('Ctrl Pts',(12.1721667776362,-0.992619537425882,
26.499861786204));
#40529=CARTESIAN_POINT('Ctrl Pts',(12.1624142267167,-0.992445382879524,
26.6520503547924));
#40530=CARTESIAN_POINT('Ctrl Pts',(12.1526616757972,-0.956798863523656,
26.8045819639399));
#40531=CARTESIAN_POINT('Ctrl Pts',(12.1429091248777,-0.889466903262642,
26.9405929119523));
#40532=CARTESIAN_POINT('Ctrl Pts',(12.1323235893772,-0.81638398766988,27.0882208228991));
#40533=CARTESIAN_POINT('Ctrl Pts',(12.1217380538767,-0.705971847579991,
27.2163854267011));
#40534=CARTESIAN_POINT('Ctrl Pts',(12.1111525183761,-0.570822728387213,
27.3115718104357));
#40535=CARTESIAN_POINT('Ctrl Pts',(12.1005669828756,-0.435673609194435,
27.4067581941702));
#40536=CARTESIAN_POINT('Ctrl Pts',(12.0899814473751,-0.275787510898768,
27.4689663578372));
#40537=CARTESIAN_POINT('Ctrl Pts',(12.0793959118745,-0.11202748104491,27.4872537945506));
#40538=CARTESIAN_POINT('Ctrl Pts',(12.0582248408735,0.21549257866281,27.5238286679774));
#40539=CARTESIAN_POINT('Ctrl Pts',(12.0370537698724,0.558508364603297,27.3847206335896));
#40540=CARTESIAN_POINT('Ctrl Pts',(12.0158826988714,0.768036748408632,27.1303489227862));
#40541=CARTESIAN_POINT('Ctrl Pts',(12.0052971633708,0.872800940311296,27.0031630673845));
#40542=CARTESIAN_POINT('Ctrl Pts',(11.9947116278703,0.944193281680175,26.8471612928789));
#40543=CARTESIAN_POINT('Ctrl Pts',(11.9841260923698,0.974865815542366,26.6847269131019));
#40544=CARTESIAN_POINT('Ctrl Pts',(11.9735405568692,1.00553834940456,26.522292533325));
#40545=CARTESIAN_POINT('Ctrl Pts',(11.9629550213687,0.99549107576006,26.3534255482768));
#40546=CARTESIAN_POINT('Ctrl Pts',(11.9523694858682,0.945102312316298,26.1965941574118));
#40547=CARTESIAN_POINT('Ctrl Pts',(11.9417839503676,0.894713548872537,26.0397627665468));
#40548=CARTESIAN_POINT('Ctrl Pts',(11.9311984148671,0.803983295629513,25.894966969865));
#40549=CARTESIAN_POINT('Ctrl Pts',(11.9206128793666,0.684457208950646,25.7810527130143));
#40550=CARTESIAN_POINT('Ctrl Pts',(11.910027343866,0.564931122271776,25.6671384561637));
#40551=CARTESIAN_POINT('Ctrl Pts',(11.8994418083655,0.416609202157062,25.5841057391443));
#40552=CARTESIAN_POINT('Ctrl Pts',(11.888856272865,0.257283901945971,25.541416786935));
#40553=CARTESIAN_POINT('Ctrl Pts',(11.8782707373644,0.0979586017348822,
25.4987278347256));
#40554=CARTESIAN_POINT('Ctrl Pts',(11.8676852018639,-0.0723700785725825,
25.4963826473263));
#40555=CARTESIAN_POINT('Ctrl Pts',(11.8570996663634,-0.232761627146138,
25.5350337730709));
#40556=CARTESIAN_POINT('Ctrl Pts',(11.8465141308628,-0.393153175719694,
25.5736848988155));
#40557=CARTESIAN_POINT('Ctrl Pts',(11.8359285953623,-0.543607592559341,
25.653332337704));
#40558=CARTESIAN_POINT('Ctrl Pts',(11.8253430598618,-0.6659545777768,25.7640417972626));
#40559=CARTESIAN_POINT('Ctrl Pts',(11.8147575243612,-0.788301562994261,
25.8747512568212));
#40560=CARTESIAN_POINT('Ctrl Pts',(11.8041719888607,-0.882541116589533,
26.0165227370498));
#40561=CARTESIAN_POINT('Ctrl Pts',(11.7935864533602,-0.93697823267869,26.1722659833465));
#40562=CARTESIAN_POINT('Ctrl Pts',(11.7864465614522,-0.973695801160667,
26.2773140410383));
#40563=CARTESIAN_POINT('Ctrl Pts',(11.7793066695442,-0.992305503429818,
26.3887184649872));
#40564=CARTESIAN_POINT('Ctrl Pts',(11.7721667776362,-0.992366447419476,
26.5000655238227));
#40565=CARTESIAN_POINT('Ctrl Pts',(11.6278332223638,-0.992471224471742,
26.4999749790724));
#40566=CARTESIAN_POINT('Ctrl Pts',(11.6308778003986,-0.992516080655597,
26.4525065782307));
#40567=CARTESIAN_POINT('Ctrl Pts',(11.6339223784335,-0.989172345930418,
26.4050444435199));
#40568=CARTESIAN_POINT('Ctrl Pts',(11.6369669564683,-0.982387545983623,
26.3580794221597));
#40569=CARTESIAN_POINT('Ctrl Pts',(11.6475761593666,-0.958745084389168,
26.1944240863357));
#40570=CARTESIAN_POINT('Ctrl Pts',(11.6581853622648,-0.893319182518039,
26.036804993553));
#40571=CARTESIAN_POINT('Ctrl Pts',(11.6687945651631,-0.794117446424462,
25.9045134575807));
#40572=CARTESIAN_POINT('Ctrl Pts',(11.6794037680614,-0.694915710330884,
25.7722219216083));
#40573=CARTESIAN_POINT('Ctrl Pts',(11.6900129709597,-0.561938140014856,
25.6652579424464));
#40574=CARTESIAN_POINT('Ctrl Pts',(11.7006221738579,-0.411460124377188,
25.596713053916));
#40575=CARTESIAN_POINT('Ctrl Pts',(11.7112313767562,-0.260982108739517,
25.5281681653856));
#40576=CARTESIAN_POINT('Ctrl Pts',(11.7218405796545,-0.093003647780212,
25.4980423674867));
#40577=CARTESIAN_POINT('Ctrl Pts',(11.7324497825527,0.0719160410885499,
25.5100228164486));
#40578=CARTESIAN_POINT('Ctrl Pts',(11.743058985451,0.236835729957307,25.5220032654105));
#40579=CARTESIAN_POINT('Ctrl Pts',(11.7536681883493,0.398696646735515,25.5760899612332));
#40580=CARTESIAN_POINT('Ctrl Pts',(11.7642773912476,0.537688312391664,25.6656631258085));
#40581=CARTESIAN_POINT('Ctrl Pts',(11.7748865941458,0.676679978047811,25.7552362903837));
#40582=CARTESIAN_POINT('Ctrl Pts',(11.7854957970441,0.792802392581904,25.8802959237115));
#40583=CARTESIAN_POINT('Ctrl Pts',(11.7961049999424,0.871843103080623,26.0255357289226));
#40584=CARTESIAN_POINT('Ctrl Pts',(11.8067142028407,0.950883813579343,26.1707755341337));
#40585=CARTESIAN_POINT('Ctrl Pts',(11.8173234057389,0.992842820042693,26.3361955112281));
#40586=CARTESIAN_POINT('Ctrl Pts',(11.8279326086372,0.99258467634649,26.5015495807145));
#40587=CARTESIAN_POINT('Ctrl Pts',(11.8385418115355,0.992326532650287,26.666903650201));
#40588=CARTESIAN_POINT('Ctrl Pts',(11.8491510144337,0.949851238794532,26.8321918120795));
#40589=CARTESIAN_POINT('Ctrl Pts',(11.859760217332,0.870357430342617,26.9771841199848));
#40590=CARTESIAN_POINT('Ctrl Pts',(11.8703694202303,0.790863621890701,27.1221764278901));
#40591=CARTESIAN_POINT('Ctrl Pts',(11.8809786231286,0.674351298842628,27.2468728818222));
#40592=CARTESIAN_POINT('Ctrl Pts',(11.8915878260268,0.535080635789019,27.3360116351594));
#40593=CARTESIAN_POINT('Ctrl Pts',(11.9021970289251,0.395809972735412,27.4251503884966));
#40594=CARTESIAN_POINT('Ctrl Pts',(11.9128062318234,0.233780969676272,27.4787314412388));
#40595=CARTESIAN_POINT('Ctrl Pts',(11.9234154347217,0.0688246780568229,
27.4901969019385));
#40596=CARTESIAN_POINT('Ctrl Pts',(11.9340246376199,-0.0961316135626239,
27.5016623626382));
#40597=CARTESIAN_POINT('Ctrl Pts',(11.9446338405182,-0.264015193742381,
27.4710122312954));
#40598=CARTESIAN_POINT('Ctrl Pts',(11.9552430434165,-0.414278457717283,
27.4019978383509));
#40599=CARTESIAN_POINT('Ctrl Pts',(11.9658522463147,-0.564541721692185,
27.3329834454063));
#40600=CARTESIAN_POINT('Ctrl Pts',(11.976461449213,-0.697184669462232,27.22560479086));
#40601=CARTESIAN_POINT('Ctrl Pts',(11.9870706521113,-0.795972867244521,
27.0930041614768));
#40602=CARTESIAN_POINT('Ctrl Pts',(11.9976798550096,-0.894761065026811,
26.9604035320936));
#40603=CARTESIAN_POINT('Ctrl Pts',(12.0082890579078,-0.959694512821341,
26.8025809278734));
#40604=CARTESIAN_POINT('Ctrl Pts',(12.0188982608061,-0.982825877006247,
26.6388525707546));
#40605=CARTESIAN_POINT('Ctrl Pts',(12.0218765813253,-0.989319542670898,
26.5928891246537));
#40606=CARTESIAN_POINT('Ctrl Pts',(12.0248549018446,-0.992518816247691,
26.5464602504224));
#40607=CARTESIAN_POINT('Ctrl Pts',(12.0278332223638,-0.992474254593845,
26.5000252858765));
#40608=CARTESIAN_POINT('Origin',(18.,0.,26.5));
#40609=CARTESIAN_POINT('',(12.5721667776362,-0.992298354748071,26.4996276611265));
#40610=CARTESIAN_POINT('',(12.4278332223638,-0.992540878678463,26.4999779426563));
#40611=CARTESIAN_POINT('',(18.,-0.9925,26.5));
#40612=CARTESIAN_POINT('Ctrl Pts',(12.5721667776362,-0.992298354748071,
26.4996276611265));
#40613=CARTESIAN_POINT('Ctrl Pts',(12.5666928548903,-0.992202803623357,
26.5847133847472));
#40614=CARTESIAN_POINT('Ctrl Pts',(12.5612189321444,-0.981239055656051,
26.6698717450131));
#40615=CARTESIAN_POINT('Ctrl Pts',(12.5557450093985,-0.959533788525683,
26.7525515777318));
#40616=CARTESIAN_POINT('Ctrl Pts',(12.545159473898,-0.91755989038677,26.9124388003046));
#40617=CARTESIAN_POINT('Ctrl Pts',(12.5345739383974,-0.835416712401015,
27.0630572532426));
#40618=CARTESIAN_POINT('Ctrl Pts',(12.5239884028969,-0.722001864471279,
27.1825932310416));
#40619=CARTESIAN_POINT('Ctrl Pts',(12.5028173318958,-0.495172168611806,
27.4216651866396));
#40620=CARTESIAN_POINT('Ctrl Pts',(12.4816462608948,-0.143255792976409,
27.5364072416815));
#40621=CARTESIAN_POINT('Ctrl Pts',(12.4604751898937,0.180898312867456,27.4769831174414));
#40622=CARTESIAN_POINT('Ctrl Pts',(12.4498896543932,0.342975365789387,27.4472710553214));
#40623=CARTESIAN_POINT('Ctrl Pts',(12.4393041188926,0.498111851263434,27.3740174483809));
#40624=CARTESIAN_POINT('Ctrl Pts',(12.4287185833921,0.626262354207043,27.2695991517929));
#40625=CARTESIAN_POINT('Ctrl Pts',(12.4181330478916,0.754412857150651,27.1651808552049));
#40626=CARTESIAN_POINT('Ctrl Pts',(12.407547512391,0.855577377563819,27.0295978689694));
#40627=CARTESIAN_POINT('Ctrl Pts',(12.3969619768905,0.918141159608453,26.8772138612182));
#40628=CARTESIAN_POINT('Ctrl Pts',(12.38637644139,0.980704941653088,26.724829853467));
#40629=CARTESIAN_POINT('Ctrl Pts',(12.3757909058894,1.00466798532919,26.5556448242001));
#40630=CARTESIAN_POINT('Ctrl Pts',(12.3652053703889,0.986710013514384,26.3915093479651));
#40631=CARTESIAN_POINT('Ctrl Pts',(12.3546198348884,0.96875204169958,26.2273738717301));
#40632=CARTESIAN_POINT('Ctrl Pts',(12.3440342993879,0.908873054393874,26.0682879485269));
#40633=CARTESIAN_POINT('Ctrl Pts',(12.3334487638873,0.814577187513826,25.932954333274));
#40634=CARTESIAN_POINT('Ctrl Pts',(12.3228632283868,0.720281320633778,25.7976207180211));
#40635=CARTESIAN_POINT('Ctrl Pts',(12.3122776928863,0.591568574179388,25.6860394107184));
#40636=CARTESIAN_POINT('Ctrl Pts',(12.3016921573857,0.444028354131184,25.6122068850723));
#40637=CARTESIAN_POINT('Ctrl Pts',(12.2911066218852,0.296488134082977,25.5383743594262));
#40638=CARTESIAN_POINT('Ctrl Pts',(12.2805210863847,0.130120440440954,25.5022906154369));
#40639=CARTESIAN_POINT('Ctrl Pts',(12.2699355508841,-0.0347793480614057,
25.5080723953903));
#40640=CARTESIAN_POINT('Ctrl Pts',(12.2593500153836,-0.199679136563763,
25.5138541753437));
#40641=CARTESIAN_POINT('Ctrl Pts',(12.2487644798831,-0.363111019926459,
25.5615014792399));
#40642=CARTESIAN_POINT('Ctrl Pts',(12.2381789443825,-0.505117790383664,
25.6454862130876));
#40643=CARTESIAN_POINT('Ctrl Pts',(12.227593408882,-0.647124560840869,25.7294709469352));
#40644=CARTESIAN_POINT('Ctrl Pts',(12.2170078733815,-0.767706218392585,
25.8497931107343));
#40645=CARTESIAN_POINT('Ctrl Pts',(12.2064223378809,-0.852291934685505,
25.9913987410154));
#40646=CARTESIAN_POINT('Ctrl Pts',(12.1958368023804,-0.936877650978427,
26.1330043712965));
#40647=CARTESIAN_POINT('Ctrl Pts',(12.1852512668799,-0.985467426012552,
26.2958934680595));
#40648=CARTESIAN_POINT('Ctrl Pts',(12.1746657313793,-0.991885467981796,
26.4608836254868));
#40649=CARTESIAN_POINT('Ctrl Pts',(12.1738327467983,-0.992390509035276,
26.473866838018));
#40650=CARTESIAN_POINT('Ctrl Pts',(12.1729997622173,-0.992634412308672,
26.4868630608355));
#40651=CARTESIAN_POINT('Ctrl Pts',(12.1721667776362,-0.992619537425882,
26.499861786204));
#40652=CARTESIAN_POINT('Ctrl Pts',(12.0278332223638,-0.992474254593845,
26.5000252858765));
#40653=CARTESIAN_POINT('Ctrl Pts',(12.0354641047429,-0.992360081274713,
26.3810522772844));
#40654=CARTESIAN_POINT('Ctrl Pts',(12.0430949871219,-0.970951506468747,
26.2620392883616));
#40655=CARTESIAN_POINT('Ctrl Pts',(12.0507258695009,-0.929098865159217,
26.15071209629));
#40656=CARTESIAN_POINT('Ctrl Pts',(12.0613350723992,-0.870911208551999,
25.9959340889619));
#40657=CARTESIAN_POINT('Ctrl Pts',(12.0719442752975,-0.773206614762282,
25.8560121843233));
#40658=CARTESIAN_POINT('Ctrl Pts',(12.0825534781957,-0.647943343047954,
25.748071702143));
#40659=CARTESIAN_POINT('Ctrl Pts',(12.093162681094,-0.522680071333622,25.6401312199627));
#40660=CARTESIAN_POINT('Ctrl Pts',(12.1037718839923,-0.369858121694682,
25.5641721602407));
#40661=CARTESIAN_POINT('Ctrl Pts',(12.1143810868906,-0.208181676024677,
25.5294913031375));
#40662=CARTESIAN_POINT('Ctrl Pts',(12.1249902897888,-0.0465052303546761,
25.4948104460343));
#40663=CARTESIAN_POINT('Ctrl Pts',(12.1355994926871,0.124025711346386,25.5014077915499));
#40664=CARTESIAN_POINT('Ctrl Pts',(12.1462086955854,0.28253952847956,25.5484758774656));
#40665=CARTESIAN_POINT('Ctrl Pts',(12.1568178984836,0.441053345612737,25.5955439633813));
#40666=CARTESIAN_POINT('Ctrl Pts',(12.1674271013819,0.587550038178023,25.6830827896971));
#40667=CARTESIAN_POINT('Ctrl Pts',(12.1780363042802,0.704099585055956,25.8003783056235));
#40668=CARTESIAN_POINT('Ctrl Pts',(12.1886455071785,0.820649131933889,25.9176738215499));
#40669=CARTESIAN_POINT('Ctrl Pts',(12.1992547100767,0.907251533124466,26.064726027087));
#40670=CARTESIAN_POINT('Ctrl Pts',(12.209863912975,0.953307348768988,26.2235369107796));
#40671=CARTESIAN_POINT('Ctrl Pts',(12.2204731158733,0.999363164413512,26.3823477944721));
#40672=CARTESIAN_POINT('Ctrl Pts',(12.2310823187716,1.00487239451198,26.5529173563202));
#40673=CARTESIAN_POINT('Ctrl Pts',(12.2416915216698,0.969160753452287,26.7143692489282));
#40674=CARTESIAN_POINT('Ctrl Pts',(12.2523007245681,0.933449112392596,26.8758211415363));
#40675=CARTESIAN_POINT('Ctrl Pts',(12.2629099274664,0.856516600174747,27.0281553649044));
#40676=CARTESIAN_POINT('Ctrl Pts',(12.2735191303646,0.747779139743386,27.1527274309257));
#40677=CARTESIAN_POINT('Ctrl Pts',(12.2841283332629,0.639041679312023,27.2772994969471));
#40678=CARTESIAN_POINT('Ctrl Pts',(12.2947375361612,0.498499270667149,27.3741094056218));
#40679=CARTESIAN_POINT('Ctrl Pts',(12.3053467390595,0.343353178295059,27.4313083999798));
#40680=CARTESIAN_POINT('Ctrl Pts',(12.3159559419577,0.188207085922968,27.4885073943378));
#40681=CARTESIAN_POINT('Ctrl Pts',(12.326565144856,0.0184573098236633,27.5060954743792));
#40682=CARTESIAN_POINT('Ctrl Pts',(12.3371743477543,-0.145120137813161,
27.4819200000608));
#40683=CARTESIAN_POINT('Ctrl Pts',(12.3477835506525,-0.308697585449984,
27.4577445257424));
#40684=CARTESIAN_POINT('Ctrl Pts',(12.3583927535508,-0.46610270462433,27.3918054970643));
#40685=CARTESIAN_POINT('Ctrl Pts',(12.3690019564491,-0.598070370221847,
27.2921733226895));
#40686=CARTESIAN_POINT('Ctrl Pts',(12.3796111593474,-0.730038035819365,
27.1925411483148));
#40687=CARTESIAN_POINT('Ctrl Pts',(12.3902203622456,-0.836568247840052,
27.0592158282434));
#40688=CARTESIAN_POINT('Ctrl Pts',(12.4008295651439,-0.904622562084627,
26.9085153131594));
#40689=CARTESIAN_POINT('Ctrl Pts',(12.4098307842172,-0.962362224269649,
26.7806557214693));
#40690=CARTESIAN_POINT('Ctrl Pts',(12.4188320032905,-0.992405321125612,
26.6402887354989));
#40691=CARTESIAN_POINT('Ctrl Pts',(12.4278332223638,-0.992540878678463,
26.4999779426563));
#40692=CARTESIAN_POINT('Origin',(18.,0.,26.5));
#40693=CARTESIAN_POINT('',(12.9721667776362,-0.993584665131883,26.5006674583246));
#40694=CARTESIAN_POINT('',(12.8278332223638,-0.992423719932019,26.5000125385131));
#40695=CARTESIAN_POINT('',(18.,-0.9925,26.5));
#40696=CARTESIAN_POINT('Ctrl Pts',(12.9721667776362,-0.993584665131883,
26.5006674583246));
#40697=CARTESIAN_POINT('Ctrl Pts',(12.9709714830639,-0.993603791415993,
26.519301517892));
#40698=CARTESIAN_POINT('Ctrl Pts',(12.9697761884916,-0.993073070228261,
26.537921851123));
#40699=CARTESIAN_POINT('Ctrl Pts',(12.9685808939192,-0.991982052232969,
26.5564961893539));
#40700=CARTESIAN_POINT('Ctrl Pts',(12.9474098229182,-0.972657929145171,
26.8854850784429));
#40701=CARTESIAN_POINT('Ctrl Pts',(12.9262387519171,-0.777560099683024,
27.2000446301572));
#40702=CARTESIAN_POINT('Ctrl Pts',(12.9050676809161,-0.491426019562643,
27.3635512021071));
#40703=CARTESIAN_POINT('Ctrl Pts',(12.8944821454155,-0.348358979502456,
27.445304488082));
#40704=CARTESIAN_POINT('Ctrl Pts',(12.883896609915,-0.182532876777712,27.4892945291159));
#40705=CARTESIAN_POINT('Ctrl Pts',(12.8733110744145,-0.0172511009544274,
27.4920634003193));
#40706=CARTESIAN_POINT('Ctrl Pts',(12.8627255389139,0.148030674868862,27.4948322715228));
#40707=CARTESIAN_POINT('Ctrl Pts',(12.8521400034134,0.312768123790687,27.4563799728959));
#40708=CARTESIAN_POINT('Ctrl Pts',(12.8415544679129,0.458822861540175,27.3802017199428));
#40709=CARTESIAN_POINT('Ctrl Pts',(12.8309689324123,0.604877599289659,27.3040234669898));
#40710=CARTESIAN_POINT('Ctrl Pts',(12.8203833969118,0.732249625866807,27.1901192597107));
#40711=CARTESIAN_POINT('Ctrl Pts',(12.8097978614113,0.824316265337188,27.0530547595393));
#40712=CARTESIAN_POINT('Ctrl Pts',(12.7992123259107,0.916382904807572,26.9159902593679));
#40713=CARTESIAN_POINT('Ctrl Pts',(12.7886267904102,0.973144157171193,26.7557654663044));
#40714=CARTESIAN_POINT('Ctrl Pts',(12.7780412549097,0.988282106757489,26.5915164467931));
#40715=CARTESIAN_POINT('Ctrl Pts',(12.7674557194091,1.00342005634378,26.4272674272819));
#40716=CARTESIAN_POINT('Ctrl Pts',(12.7568701839086,0.976934703152756,26.2589941813229));
#40717=CARTESIAN_POINT('Ctrl Pts',(12.7462846484081,0.91172322008537,26.1074461003344));
#40718=CARTESIAN_POINT('Ctrl Pts',(12.7356991129075,0.846511737017982,25.9558980193459));
#40719=CARTESIAN_POINT('Ctrl Pts',(12.725113577407,0.742574124074235,25.8210751033278));
#40720=CARTESIAN_POINT('Ctrl Pts',(12.7145280419065,0.612773646105535,25.7192065353265));
#40721=CARTESIAN_POINT('Ctrl Pts',(12.7039425064059,0.482973168136835,25.6173379673251));
#40722=CARTESIAN_POINT('Ctrl Pts',(12.6933569709054,0.327309825143181,25.5484237473404));
#40723=CARTESIAN_POINT('Ctrl Pts',(12.6827714354049,0.164605080401317,25.5211011483858));
#40724=CARTESIAN_POINT('Ctrl Pts',(12.6721858999044,0.00190033565945694,
25.4937785494312));
#40725=CARTESIAN_POINT('Ctrl Pts',(12.6616003644038,-0.167845810830615,
25.5080475715067));
#40726=CARTESIAN_POINT('Ctrl Pts',(12.6510148289033,-0.323789974945903,
25.5617906232108));
#40727=CARTESIAN_POINT('Ctrl Pts',(12.6404292934027,-0.479734139061194,
25.6155336749149));
#40728=CARTESIAN_POINT('Ctrl Pts',(12.6298437579022,-0.621876320801701,
25.7087507562476));
#40729=CARTESIAN_POINT('Ctrl Pts',(12.6192582224017,-0.73313048178971,25.8307567191078));
#40730=CARTESIAN_POINT('Ctrl Pts',(12.6086726869012,-0.844384642777722,
25.9527626819681));
#40731=CARTESIAN_POINT('Ctrl Pts',(12.5980871514006,-0.924750783013234,
26.1035575263558));
#40732=CARTESIAN_POINT('Ctrl Pts',(12.5875016159001,-0.964031543984952,
26.2635329446535));
#40733=CARTESIAN_POINT('Ctrl Pts',(12.5823900031455,-0.982999695268774,
26.3407829230373));
#40734=CARTESIAN_POINT('Ctrl Pts',(12.5772783903908,-0.992387581500161,
26.4201736223531));
#40735=CARTESIAN_POINT('Ctrl Pts',(12.5721667776362,-0.992298354748071,
26.4996276611265));
#40736=CARTESIAN_POINT('Ctrl Pts',(12.4278332223638,-0.992540878678463,
26.4999779426563));
#40737=CARTESIAN_POINT('Ctrl Pts',(12.4294412061888,-0.992565094770813,
26.47491272832));
#40738=CARTESIAN_POINT('Ctrl Pts',(12.4310491900138,-0.991634886822353,
26.4498493072463));
#40739=CARTESIAN_POINT('Ctrl Pts',(12.4326571738387,-0.98973765036095,26.4248593027964));
#40740=CARTESIAN_POINT('Ctrl Pts',(12.443266376737,-0.977220007924238,26.2599795176142));
#40741=CARTESIAN_POINT('Ctrl Pts',(12.4538755796353,-0.922606306582356,
26.0982956573466));
#40742=CARTESIAN_POINT('Ctrl Pts',(12.4644847825335,-0.832580825695646,
25.9595965307271));
#40743=CARTESIAN_POINT('Ctrl Pts',(12.4750939854318,-0.742555344808936,
25.8208974041076));
#40744=CARTESIAN_POINT('Ctrl Pts',(12.4857031883301,-0.617118084377399,
25.7051830111362));
#40745=CARTESIAN_POINT('Ctrl Pts',(12.4963123912284,-0.47162155980136,25.6266158661569));
#40746=CARTESIAN_POINT('Ctrl Pts',(12.5069215941266,-0.326125035225322,
25.5480487211777));
#40747=CARTESIAN_POINT('Ctrl Pts',(12.5175307970249,-0.160569246504779,
25.5066288241905));
#40748=CARTESIAN_POINT('Ctrl Pts',(12.5281399999232,0.00478310461436772,
25.5074256386403));
#40749=CARTESIAN_POINT('Ctrl Pts',(12.5387492028215,0.170135455733517,25.5082224530901));
#40750=CARTESIAN_POINT('Ctrl Pts',(12.5493584057197,0.335284369251272,25.5512359789769));
#40751=CARTESIAN_POINT('Ctrl Pts',(12.559967608618,0.480016941685798,25.6312017054501));
#40752=CARTESIAN_POINT('Ctrl Pts',(12.5705768115163,0.624749514120321,25.7111674319232));
#40753=CARTESIAN_POINT('Ctrl Pts',(12.5811860144145,0.749065745471615,25.8280853589828));
#40754=CARTESIAN_POINT('Ctrl Pts',(12.5917952173128,0.837750325314641,25.9676456693578));
#40755=CARTESIAN_POINT('Ctrl Pts',(12.6024044202111,0.92643490515767,26.1072059797328));
#40756=CARTESIAN_POINT('Ctrl Pts',(12.6130136231094,0.979487833492432,26.2694086734232));
#40757=CARTESIAN_POINT('Ctrl Pts',(12.6236228260076,0.990415857066348,26.4344014406425));
#40758=CARTESIAN_POINT('Ctrl Pts',(12.6342320289059,1.00134388064026,26.5993942078617));
#40759=CARTESIAN_POINT('Ctrl Pts',(12.6448412318042,0.970146999453333,26.7671770486098));
#40760=CARTESIAN_POINT('Ctrl Pts',(12.6554504347025,0.900643461745485,26.9172146878207));
#40761=CARTESIAN_POINT('Ctrl Pts',(12.6660596376007,0.831139924037638,27.0672523270317));
#40762=CARTESIAN_POINT('Ctrl Pts',(12.676668840499,0.723329729808879,27.1995447647054));
#40763=CARTESIAN_POINT('Ctrl Pts',(12.6872780433973,0.590407982822753,27.2979004666858));
#40764=CARTESIAN_POINT('Ctrl Pts',(12.6978872462955,0.457486235836628,27.3962561686662));
#40765=CARTESIAN_POINT('Ctrl Pts',(12.7084964491938,0.299452936093136,27.4606751349532));
#40766=CARTESIAN_POINT('Ctrl Pts',(12.7191056520921,0.135650092973945,27.4832730003384));
#40767=CARTESIAN_POINT('Ctrl Pts',(12.7297148549904,-0.0281527501452476,
27.5058708657235));
#40768=CARTESIAN_POINT('Ctrl Pts',(12.7403240578886,-0.19772513664014,27.4866476302068));
#40769=CARTESIAN_POINT('Ctrl Pts',(12.7509332607869,-0.352312765386994,
27.4279560637571));
#40770=CARTESIAN_POINT('Ctrl Pts',(12.7615424636852,-0.506900394133848,
27.3692644973074));
#40771=CARTESIAN_POINT('Ctrl Pts',(12.7721516665834,-0.646503265132669,
27.2711045999246));
#40772=CARTESIAN_POINT('Ctrl Pts',(12.7827608694817,-0.754035105775395,
27.1454903563777));
#40773=CARTESIAN_POINT('Ctrl Pts',(12.79337007238,-0.861566946418121,27.0198761128307));
#40774=CARTESIAN_POINT('Ctrl Pts',(12.8039792752783,-0.937027756704759,
26.8668075231194));
#40775=CARTESIAN_POINT('Ctrl Pts',(12.8145884781765,-0.971181738212568,
26.7050189559057));
#40776=CARTESIAN_POINT('Ctrl Pts',(12.8190033929056,-0.985394579409199,
26.6376922457618));
#40777=CARTESIAN_POINT('Ctrl Pts',(12.8234183076347,-0.992454210461741,
26.5688554746092));
#40778=CARTESIAN_POINT('Ctrl Pts',(12.8278332223638,-0.992423719932019,
26.5000125385131));
#40779=CARTESIAN_POINT('Origin',(18.,0.,26.5));
#40780=CARTESIAN_POINT('',(13.3721667776362,-0.990996827870586,26.5001850440327));
#40781=CARTESIAN_POINT('',(13.2278332223638,-0.992585204636762,26.4999971408611));
#40782=CARTESIAN_POINT('',(18.,-0.9925,26.5));
#40783=CARTESIAN_POINT('Ctrl Pts',(13.3721667776362,-0.990996827870586,
26.5001850440327));
#40784=CARTESIAN_POINT('Ctrl Pts',(13.3646645757369,-0.991718635376042,
26.6170275101808));
#40785=CARTESIAN_POINT('Ctrl Pts',(13.3571623738377,-0.972510103653976,
26.7338149156839));
#40786=CARTESIAN_POINT('Ctrl Pts',(13.3496601719384,-0.932335445090473,
26.843468818369));
#40787=CARTESIAN_POINT('Ctrl Pts',(13.3390746364379,-0.875649384097233,
26.9981894317609));
#40788=CARTESIAN_POINT('Ctrl Pts',(13.3284891009373,-0.777221983820787,
27.1387079961211));
#40789=CARTESIAN_POINT('Ctrl Pts',(13.3179035654368,-0.652640928626889,
27.247360160176));
#40790=CARTESIAN_POINT('Ctrl Pts',(13.3073180299363,-0.528059873432998,
27.3560123242309));
#40791=CARTESIAN_POINT('Ctrl Pts',(13.2967324944357,-0.377325163321658,
27.4327980879805));
#40792=CARTESIAN_POINT('Ctrl Pts',(13.2861469589352,-0.216557357470861,
27.4686983002914));
#40793=CARTESIAN_POINT('Ctrl Pts',(13.2755614234347,-0.0557895516200603,
27.5045985126023));
#40794=CARTESIAN_POINT('Ctrl Pts',(13.2649758879341,0.115011349970196,27.4996131734745));
#40795=CARTESIAN_POINT('Ctrl Pts',(13.2543903524336,0.273747971638755,27.4541639902932));
#40796=CARTESIAN_POINT('Ctrl Pts',(13.2438048169331,0.432484593307314,27.4087148071119));
#40797=CARTESIAN_POINT('Ctrl Pts',(13.2332192814326,0.579156935054173,27.3228017798771));
#40798=CARTESIAN_POINT('Ctrl Pts',(13.222633745932,0.696600166892606,27.2069830196376));
#40799=CARTESIAN_POINT('Ctrl Pts',(13.2120482104315,0.814043398731035,27.091164259398));
#40800=CARTESIAN_POINT('Ctrl Pts',(13.201462674931,0.902257520661038,26.9454397661536));
#40801=CARTESIAN_POINT('Ctrl Pts',(13.1908771394304,0.95008317966956,26.7875408595217));
#40802=CARTESIAN_POINT('Ctrl Pts',(13.1802916039299,0.997908838678084,26.6296419528898));
#40803=CARTESIAN_POINT('Ctrl Pts',(13.1697060684293,1.00534603476512,26.4595686328704));
#40804=CARTESIAN_POINT('Ctrl Pts',(13.1591205329288,0.971768544810025,26.2980201219027));
#40805=CARTESIAN_POINT('Ctrl Pts',(13.1485349974283,0.938191054854925,26.1364716109351));
#40806=CARTESIAN_POINT('Ctrl Pts',(13.1379494619278,0.863598878857685,25.9834479090192));
#40807=CARTESIAN_POINT('Ctrl Pts',(13.1273639264272,0.756814616848371,25.8576843222292));
#40808=CARTESIAN_POINT('Ctrl Pts',(13.1167783909267,0.65003035483906,25.7319207354392));
#40809=CARTESIAN_POINT('Ctrl Pts',(13.1061928554262,0.511054006817676,25.6334172637753));
#40810=CARTESIAN_POINT('Ctrl Pts',(13.0956073199256,0.357186261541762,25.5739898720119));
#40811=CARTESIAN_POINT('Ctrl Pts',(13.0850217844251,0.203318516265847,25.5145624802486));
#40812=CARTESIAN_POINT('Ctrl Pts',(13.0744362489246,0.034559373735403,25.4942111683859));
#40813=CARTESIAN_POINT('Ctrl Pts',(13.063850713424,-0.129140779817654,25.5157797343396));
#40814=CARTESIAN_POINT('Ctrl Pts',(13.0532651779235,-0.292840933370716,
25.5373483002933));
#40815=CARTESIAN_POINT('Ctrl Pts',(13.042679642423,-0.451482097946389,25.6008367440633));
#40816=CARTESIAN_POINT('Ctrl Pts',(13.0320941069224,-0.584629033760132,
25.6978264658149));
#40817=CARTESIAN_POINT('Ctrl Pts',(13.0215085714219,-0.717775969573874,
25.7948161875666));
#40818=CARTESIAN_POINT('Ctrl Pts',(13.0109230359214,-0.825428676625686,
25.9253071872998));
#40819=CARTESIAN_POINT('Ctrl Pts',(13.0003375004208,-0.896395712676435,
26.0746035766105));
#40820=CARTESIAN_POINT('Ctrl Pts',(12.9909472594926,-0.959349312562228,
26.2070417574913));
#40821=CARTESIAN_POINT('Ctrl Pts',(12.9815570185644,-0.993434408935617,
26.3542781808535));
#40822=CARTESIAN_POINT('Ctrl Pts',(12.9721667776362,-0.993584665131883,
26.5006674583246));
#40823=CARTESIAN_POINT('Ctrl Pts',(12.8278332223638,-0.992423719932019,
26.5000125385131));
#40824=CARTESIAN_POINT('Ctrl Pts',(12.834027510533,-0.99238094059445,26.4034233605202));
#40825=CARTESIAN_POINT('Ctrl Pts',(12.8402217987022,-0.97838116847057,26.306822046759));
#40826=CARTESIAN_POINT('Ctrl Pts',(12.8464160868713,-0.950598647581288,
26.2143622011447));
#40827=CARTESIAN_POINT('Ctrl Pts',(12.8570252897696,-0.903014422713221,
26.0560025583136));
#40828=CARTESIAN_POINT('Ctrl Pts',(12.8676344926679,-0.814998820248106,
25.9097918173675));
#40829=CARTESIAN_POINT('Ctrl Pts',(12.8782436955662,-0.697324244555001,
25.7936250012394));
#40830=CARTESIAN_POINT('Ctrl Pts',(12.8888528984644,-0.579649668861895,
25.6774581851113));
#40831=CARTESIAN_POINT('Ctrl Pts',(12.8994621013627,-0.432316119940802,
25.5913352938011));
#40832=CARTESIAN_POINT('Ctrl Pts',(12.910071304261,-0.273356043422418,25.5457970790012));
#40833=CARTESIAN_POINT('Ctrl Pts',(12.9206805071593,-0.114395966904035,
25.5002588642012));
#40834=CARTESIAN_POINT('Ctrl Pts',(12.9312897100575,0.0561906372116295,
25.4953053259114));
#40835=CARTESIAN_POINT('Ctrl Pts',(12.9418989129558,0.217525335692179,25.53154273752));
#40836=CARTESIAN_POINT('Ctrl Pts',(12.9525081158541,0.378860034172724,25.5677801491285));
#40837=CARTESIAN_POINT('Ctrl Pts',(12.9631173187524,0.530942827018157,25.6452085106354));
#40838=CARTESIAN_POINT('Ctrl Pts',(12.9737265216506,0.655159999202703,25.7543512111168));
#40839=CARTESIAN_POINT('Ctrl Pts',(12.9843357245489,0.779377171387251,25.8634939115982));
#40840=CARTESIAN_POINT('Ctrl Pts',(12.9949449274472,0.875728722910919,26.0043509510541));
#40841=CARTESIAN_POINT('Ctrl Pts',(13.0055541303454,0.932421996045665,26.1596825567085));
#40842=CARTESIAN_POINT('Ctrl Pts',(13.0161633332437,0.989115269180413,26.3150141623629));
#40843=CARTESIAN_POINT('Ctrl Pts',(13.026772536142,1.00615026392623,26.4848203342157));
#40844=CARTESIAN_POINT('Ctrl Pts',(13.0373817390403,0.981442033447716,26.648318157689));
#40845=CARTESIAN_POINT('Ctrl Pts',(13.0479909419385,0.956733802969197,26.8118159811624));
#40846=CARTESIAN_POINT('Ctrl Pts',(13.0586001448368,0.890282347266338,26.9690054562562));
#40847=CARTESIAN_POINT('Ctrl Pts',(13.0692093477351,0.790220791963399,27.1006478509634));
#40848=CARTESIAN_POINT('Ctrl Pts',(13.0798185506333,0.69015923666046,27.2322902456707));
#40849=CARTESIAN_POINT('Ctrl Pts',(13.0904277535316,0.556487581757443,27.3383855599913));
#40850=CARTESIAN_POINT('Ctrl Pts',(13.1010369564299,0.405566166546082,27.4059485777192));
#40851=CARTESIAN_POINT('Ctrl Pts',(13.1116461593282,0.254644751334718,27.473511595447));
#40852=CARTESIAN_POINT('Ctrl Pts',(13.1222553622264,0.0864735758150087,
27.5025423165822));
#40853=CARTESIAN_POINT('Ctrl Pts',(13.1328645651247,-0.0783645558831055,
27.4894876135149));
#40854=CARTESIAN_POINT('Ctrl Pts',(13.143473768023,-0.243202687581215,27.4764329104477));
#40855=CARTESIAN_POINT('Ctrl Pts',(13.1540829709213,-0.404707775457734,
27.4212927831782));
#40856=CARTESIAN_POINT('Ctrl Pts',(13.1646921738195,-0.543112891087042,
27.3308159413813));
#40857=CARTESIAN_POINT('Ctrl Pts',(13.1753013767178,-0.681518006716351,
27.2403390995845));
#40858=CARTESIAN_POINT('Ctrl Pts',(13.1859105796161,-0.796823150098447,
27.1145255432603));
#40859=CARTESIAN_POINT('Ctrl Pts',(13.1965197825143,-0.874915895759271,
26.9687738434107));
#40860=CARTESIAN_POINT('Ctrl Pts',(13.2069575957975,-0.951747068260401,
26.8253767340029));
#40861=CARTESIAN_POINT('Ctrl Pts',(13.2173954090807,-0.992558449567449,
26.6626804713408));
#40862=CARTESIAN_POINT('Ctrl Pts',(13.2278332223638,-0.992585204636762,
26.4999971408611));
#40863=CARTESIAN_POINT('Origin',(18.,0.,26.5));
#40864=CARTESIAN_POINT('',(13.7721667776362,-0.992441988512883,26.5000464541839));
#40865=CARTESIAN_POINT('',(13.6278332223638,-0.992417767911371,26.4999920932966));
#40866=CARTESIAN_POINT('',(18.,-0.9925,26.5));
#40867=CARTESIAN_POINT('Ctrl Pts',(13.7721667776362,-0.992441988512883,
26.5000464541839));
#40868=CARTESIAN_POINT('Ctrl Pts',(13.7689432039105,-0.992296790322603,
26.5505240435116));
#40869=CARTESIAN_POINT('Ctrl Pts',(13.7657196301848,-0.988377443742599,
26.6009707314814));
#40870=CARTESIAN_POINT('Ctrl Pts',(13.7624960564592,-0.980698963259128,
26.6507213793718));
#40871=CARTESIAN_POINT('Ctrl Pts',(13.7519105209586,-0.955484454560221,
26.8140920028575));
#40872=CARTESIAN_POINT('Ctrl Pts',(13.7413249854581,-0.889734192649526,
26.969957038724));
#40873=CARTESIAN_POINT('Ctrl Pts',(13.7307394499576,-0.789959661753805,
27.1010301314111));
#40874=CARTESIAN_POINT('Ctrl Pts',(13.720153914457,-0.690185130858087,27.2321032240983));
#40875=CARTESIAN_POINT('Ctrl Pts',(13.7095683789565,-0.556386330977346,
27.3383843736063));
#40876=CARTESIAN_POINT('Ctrl Pts',(13.698982843456,-0.405729575639403,27.4059527492093));
#40877=CARTESIAN_POINT('Ctrl Pts',(13.6883973079554,-0.255072820301461,
27.4735211248124));
#40878=CARTESIAN_POINT('Ctrl Pts',(13.6778117724549,-0.0875581095063172,
27.5023767265106));
#40879=CARTESIAN_POINT('Ctrl Pts',(13.6672262369544,0.0768858145131292,
27.4895278440233));
#40880=CARTESIAN_POINT('Ctrl Pts',(13.6566407014538,0.24132973853258,27.476678961536));
#40881=CARTESIAN_POINT('Ctrl Pts',(13.6460551659533,0.402702875776333,27.4221255948632));
#40882=CARTESIAN_POINT('Ctrl Pts',(13.6354696304528,0.541044341020947,27.3322312270245));
#40883=CARTESIAN_POINT('Ctrl Pts',(13.6248840949522,0.679385806265562,27.2423368591858));
#40884=CARTESIAN_POINT('Ctrl Pts',(13.6142985594517,0.794695599511036,27.1171014901811));
#40885=CARTESIAN_POINT('Ctrl Pts',(13.6037130239512,0.873152901183207,26.9719470171468));
#40886=CARTESIAN_POINT('Ctrl Pts',(13.5931274884506,0.951610202855376,26.8267925441124));
#40887=CARTESIAN_POINT('Ctrl Pts',(13.5825419529501,0.993215012954245,26.6617189670485));
#40888=CARTESIAN_POINT('Ctrl Pts',(13.5719564174496,0.992636462924212,26.4967370781788));
#40889=CARTESIAN_POINT('Ctrl Pts',(13.561370881949,0.992057912894179,26.3317551893091));
#40890=CARTESIAN_POINT('Ctrl Pts',(13.5507853464485,0.949296002735245,26.1668649886337));
#40891=CARTESIAN_POINT('Ctrl Pts',(13.540199810948,0.869961747212413,26.0222518017221));
#40892=CARTESIAN_POINT('Ctrl Pts',(13.5296142754474,0.790627491689576,25.8776386148105));
#40893=CARTESIAN_POINT('Ctrl Pts',(13.5190287399469,0.674720890802834,25.7533024416627));
#40894=CARTESIAN_POINT('Ctrl Pts',(13.5084432044464,0.535661944560877,25.6642768679175));
#40895=CARTESIAN_POINT('Ctrl Pts',(13.4978576689459,0.396602998318923,25.5752512941722));
#40896=CARTESIAN_POINT('Ctrl Pts',(13.4872721334453,0.234391706721755,25.5215363198295));
#40897=CARTESIAN_POINT('Ctrl Pts',(13.4766865979448,0.0700781368495305,
25.5098674125159));
#40898=CARTESIAN_POINT('Ctrl Pts',(13.4661010624443,-0.0942354330226944,
25.4981985052023));
#40899=CARTESIAN_POINT('Ctrl Pts',(13.4555155269437,-0.260651281169975,
25.5285756649179));
#40900=CARTESIAN_POINT('Ctrl Pts',(13.4449299914432,-0.411140528373641,
25.596976823849));
#40901=CARTESIAN_POINT('Ctrl Pts',(13.4343444559427,-0.561629775577303,
25.66537798278));
#40902=CARTESIAN_POINT('Ctrl Pts',(13.4237589204421,-0.69619242183735,25.7718031409266));
#40903=CARTESIAN_POINT('Ctrl Pts',(13.4131733849416,-0.794833058535104,
25.9037948168427));
#40904=CARTESIAN_POINT('Ctrl Pts',(13.3995045158398,-0.922205542531897,
26.0742327640333));
#40905=CARTESIAN_POINT('Ctrl Pts',(13.385835646738,-0.989681708330851,26.287300294095));
#40906=CARTESIAN_POINT('Ctrl Pts',(13.3721667776362,-0.990996827870586,
26.5001850440327));
#40907=CARTESIAN_POINT('Ctrl Pts',(13.2278332223638,-0.992585204636762,
26.4999971408611));
#40908=CARTESIAN_POINT('Ctrl Pts',(13.2280046119789,-0.992585643956848,
26.497325869337));
#40909=CARTESIAN_POINT('Ctrl Pts',(13.228176001594,-0.992575086980314,26.4946546012997));
#40910=CARTESIAN_POINT('Ctrl Pts',(13.2283473912092,-0.992553512612486,
26.4919834222468));
#40911=CARTESIAN_POINT('Ctrl Pts',(13.2389565941074,-0.991218035865332,
26.3266345443076));
#40912=CARTESIAN_POINT('Ctrl Pts',(13.2495657970057,-0.947666734431473,
26.1616266318042));
#40913=CARTESIAN_POINT('Ctrl Pts',(13.260174999904,-0.867229938578543,26.0171553308244));
#40914=CARTESIAN_POINT('Ctrl Pts',(13.2707842028023,-0.786793142725617,
25.8726840298445));
#40915=CARTESIAN_POINT('Ctrl Pts',(13.2813934057005,-0.669470852453621,
25.7487493403882));
#40916=CARTESIAN_POINT('Ctrl Pts',(13.2920026085988,-0.529622375850176,
25.6605198752102));
#40917=CARTESIAN_POINT('Ctrl Pts',(13.3026118114971,-0.389773899246729,
25.5722904100322));
#40918=CARTESIAN_POINT('Ctrl Pts',(13.3132210143953,-0.227399236311832,
25.5197661691326));
#40919=CARTESIAN_POINT('Ctrl Pts',(13.3238302172936,-0.0623717444893147,
25.5093756986589));
#40920=CARTESIAN_POINT('Ctrl Pts',(13.3344394201919,0.102655747333203,25.4989852281851));
#40921=CARTESIAN_POINT('Ctrl Pts',(13.3450486230902,0.270336068043336,25.5307285281372));
#40922=CARTESIAN_POINT('Ctrl Pts',(13.3556578259884,0.420146490206049,25.6007204729975));
#40923=CARTESIAN_POINT('Ctrl Pts',(13.3662670288867,0.56995691236876,25.6707124178578));
#40924=CARTESIAN_POINT('Ctrl Pts',(13.376876231785,0.701897435984052,25.7789530076263));
#40925=CARTESIAN_POINT('Ctrl Pts',(13.3874854346832,0.799819598356204,25.9121944615746));
#40926=CARTESIAN_POINT('Ctrl Pts',(13.3980946375815,0.897741760728361,26.0454359155229));
#40927=CARTESIAN_POINT('Ctrl Pts',(13.4087038404798,0.961645561857379,26.2036782336511));
#40928=CARTESIAN_POINT('Ctrl Pts',(13.4193130433781,0.983709688621481,26.3675538244022));
#40929=CARTESIAN_POINT('Ctrl Pts',(13.4299222462763,1.00577381538558,26.5314294151533));
#40930=CARTESIAN_POINT('Ctrl Pts',(13.4405314491746,0.985998267784771,26.7009382785275));
#40931=CARTESIAN_POINT('Ctrl Pts',(13.4511406520729,0.926803414360631,26.8553338881218));
#40932=CARTESIAN_POINT('Ctrl Pts',(13.4617498549712,0.867608560936492,27.0097294977161));
#40933=CARTESIAN_POINT('Ctrl Pts',(13.4723590578694,0.768994401689023,27.1490118535305));
#40934=CARTESIAN_POINT('Ctrl Pts',(13.4829682607677,0.643030519398727,27.256133911447));
#40935=CARTESIAN_POINT('Ctrl Pts',(13.493577463666,0.517066637108437,27.3632559693634));
#40936=CARTESIAN_POINT('Ctrl Pts',(13.5041866665642,0.363753031775324,27.4382177293818));
#40937=CARTESIAN_POINT('Ctrl Pts',(13.5147958694625,0.201854060009683,27.4718444728329));
#40938=CARTESIAN_POINT('Ctrl Pts',(13.5254050723608,0.0399550882440378,
27.505471216284));
#40939=CARTESIAN_POINT('Ctrl Pts',(13.5360142752591,-0.13052924995413,27.4977629431677));
#40940=CARTESIAN_POINT('Ctrl Pts',(13.5466234781573,-0.288733037881145,
27.4496630843379));
#40941=CARTESIAN_POINT('Ctrl Pts',(13.5572326810556,-0.446936825808157,
27.4015632255082));
#40942=CARTESIAN_POINT('Ctrl Pts',(13.5678418839539,-0.592860063464017,
27.313071780965));
#40943=CARTESIAN_POINT('Ctrl Pts',(13.5784510868521,-0.708642916014393,
27.1950193943343));
#40944=CARTESIAN_POINT('Ctrl Pts',(13.5890602897504,-0.824425768564771,
27.0769670077037));
#40945=CARTESIAN_POINT('Ctrl Pts',(13.5996694926487,-0.910068236009666,
26.9293536789855));
#40946=CARTESIAN_POINT('Ctrl Pts',(13.610278695547,-0.955088366687774,26.7702460966155));
#40947=CARTESIAN_POINT('Ctrl Pts',(13.6161302044859,-0.979919232834984,
26.6824902633621));
#40948=CARTESIAN_POINT('Ctrl Pts',(13.6219817134249,-0.992392470420054,
26.5912377893801));
#40949=CARTESIAN_POINT('Ctrl Pts',(13.6278332223638,-0.992417767911371,
26.4999920932966));
#40950=CARTESIAN_POINT('Origin',(18.,0.,26.5));
#40951=CARTESIAN_POINT('',(14.1721667776362,-0.992571522832967,26.4995949047598));
#40952=CARTESIAN_POINT('',(14.0278332223638,-0.992555916844723,26.5000186768892));
#40953=CARTESIAN_POINT('',(18.,-0.9925,26.5));
#40954=CARTESIAN_POINT('Ctrl Pts',(14.1721667776362,-0.992571522832967,
26.4995949047598));
#40955=CARTESIAN_POINT('Ctrl Pts',(14.1626362965836,-0.992457550700201,
26.64806001));
#40956=CARTESIAN_POINT('Ctrl Pts',(14.1531058155309,-0.958639467274736,
26.7971838773033));
#40957=CARTESIAN_POINT('Ctrl Pts',(14.1435753344783,-0.894147088982726,
26.9311239446055));
#40958=CARTESIAN_POINT('Ctrl Pts',(14.1329897989778,-0.822515200082955,
27.0798916017197));
#40959=CARTESIAN_POINT('Ctrl Pts',(14.1224042634772,-0.713041613705988,
27.2099275889229));
#40960=CARTESIAN_POINT('Ctrl Pts',(14.1118187279767,-0.579034442518051,
27.3060991855525));
#40961=CARTESIAN_POINT('Ctrl Pts',(14.1012331924762,-0.445027271330115,
27.4022707821822));
#40962=CARTESIAN_POINT('Ctrl Pts',(14.0906476569756,-0.286486515331208,
27.4645779882383));
#40963=CARTESIAN_POINT('Ctrl Pts',(14.0800621214751,-0.122774913851459,
27.4850198549848));
#40964=CARTESIAN_POINT('Ctrl Pts',(14.0694765859746,0.0409366876282946,
27.5054617217313));
#40965=CARTESIAN_POINT('Ctrl Pts',(14.0588910504741,0.209819134588893,27.4840382491683));
#40966=CARTESIAN_POINT('Ctrl Pts',(14.0483055149735,0.363365302276931,27.4236317626303));
#40967=CARTESIAN_POINT('Ctrl Pts',(14.037719979473,0.516911469964969,27.3632252760923));
#40968=CARTESIAN_POINT('Ctrl Pts',(14.0271344439725,0.655121358380448,27.2638357755792));
#40969=CARTESIAN_POINT('Ctrl Pts',(14.0165489084719,0.761020962357605,27.1373263599113));
#40970=CARTESIAN_POINT('Ctrl Pts',(14.0059633729714,0.866920566334765,27.0108169442434));
#40971=CARTESIAN_POINT('Ctrl Pts',(13.9953778374708,0.940509885873604,26.8571876134207));
#40972=CARTESIAN_POINT('Ctrl Pts',(13.9847923019703,0.973068007556158,26.6954876856514));
#40973=CARTESIAN_POINT('Ctrl Pts',(13.9742067664698,1.00562612923871,26.5337877578821));
#40974=CARTESIAN_POINT('Ctrl Pts',(13.9636212309693,0.997153053064983,26.3640172331663));
#40975=CARTESIAN_POINT('Ctrl Pts',(13.9530356954687,0.948218849432393,26.2063200961427));
#40976=CARTESIAN_POINT('Ctrl Pts',(13.9424501599682,0.899284645799801,26.0486229591191));
#40977=CARTESIAN_POINT('Ctrl Pts',(13.9318646244677,0.809889314708351,25.9029992097878));
#40978=CARTESIAN_POINT('Ctrl Pts',(13.9212790889671,0.691785171387141,25.7881666187154));
#40979=CARTESIAN_POINT('Ctrl Pts',(13.9106935534666,0.573681028065935,25.6733340276429));
#40980=CARTESIAN_POINT('Ctrl Pts',(13.9001080179661,0.426868072514974,25.5892925948294));
#40981=CARTESIAN_POINT('Ctrl Pts',(13.8895224824655,0.267722733869405,25.544588084381));
#40982=CARTESIAN_POINT('Ctrl Pts',(13.878936946965,0.108577395223831,25.4998835739326));
#40983=CARTESIAN_POINT('Ctrl Pts',(13.8683514114645,-0.0629003265163543,
25.4945159858495));
#40984=CARTESIAN_POINT('Ctrl Pts',(13.8577658759639,-0.223393305045033,
25.5318493698681));
#40985=CARTESIAN_POINT('Ctrl Pts',(13.8365948049629,-0.544379262102385,
25.6065161379052));
#40986=CARTESIAN_POINT('Ctrl Pts',(13.8154237339618,-0.821426246313716,
25.851986794349));
#40987=CARTESIAN_POINT('Ctrl Pts',(13.7942526629607,-0.934203567068004,
26.161645294637));
#40988=CARTESIAN_POINT('Ctrl Pts',(13.7868907011859,-0.973420398584022,
26.2693249695227));
#40989=CARTESIAN_POINT('Ctrl Pts',(13.7795287394111,-0.992773590522822,
26.3847662978295));
#40990=CARTESIAN_POINT('Ctrl Pts',(13.7721667776362,-0.992441988512883,
26.5000464541839));
#40991=CARTESIAN_POINT('Ctrl Pts',(13.6278332223638,-0.992417767911371,
26.4999920932966));
#40992=CARTESIAN_POINT('Ctrl Pts',(13.6325909163231,-0.992438336575435,
26.4258028368843));
#40993=CARTESIAN_POINT('Ctrl Pts',(13.6373486102825,-0.984229759594754,
26.3516180612386));
#40994=CARTESIAN_POINT('Ctrl Pts',(13.6421063042418,-0.967743493691695,
26.2793208860457));
#40995=CARTESIAN_POINT('Ctrl Pts',(13.6527155071401,-0.930980696106187,
26.1181050938677));
#40996=CARTESIAN_POINT('Ctrl Pts',(13.6633247100383,-0.853057307023846,
25.9662753455335));
#40997=CARTESIAN_POINT('Ctrl Pts',(13.6739339129366,-0.74351052477647,25.8424143854487));
#40998=CARTESIAN_POINT('Ctrl Pts',(13.6845431158349,-0.633963742529094,
25.7185534253638));
#40999=CARTESIAN_POINT('Ctrl Pts',(13.6951523187332,-0.492793567116679,
25.6226612535283));
#41000=CARTESIAN_POINT('Ctrl Pts',(13.7057615216314,-0.337278096646842,
25.5664743032779));
#41001=CARTESIAN_POINT('Ctrl Pts',(13.7163707245297,-0.181762626177006,
25.5102873530275));
#41002=CARTESIAN_POINT('Ctrl Pts',(13.726979927428,-0.011901860649759,25.4938056243621));
#41003=CARTESIAN_POINT('Ctrl Pts',(13.7375891303262,0.151514603528741,25.5190463487831));
#41004=CARTESIAN_POINT('Ctrl Pts',(13.7481983332245,0.314931067707251,25.544287073204));
#41005=CARTESIAN_POINT('Ctrl Pts',(13.7588075361228,0.471903230537002,25.6112502507112));
#41006=CARTESIAN_POINT('Ctrl Pts',(13.7694167390211,0.603218957290428,25.7117401250326));
#41007=CARTESIAN_POINT('Ctrl Pts',(13.7800259419193,0.734534684043851,25.8122299993539));
#41008=CARTESIAN_POINT('Ctrl Pts',(13.7906351448176,0.840193974720952,25.9462465704894));
#41009=CARTESIAN_POINT('Ctrl Pts',(13.8012443477159,0.907264978915181,26.0973872841647));
#41010=CARTESIAN_POINT('Ctrl Pts',(13.8118535506141,0.974335983109407,26.2485279978399));
#41011=CARTESIAN_POINT('Ctrl Pts',(13.8224627535124,1.00281870082077,26.416792854055));
#41012=CARTESIAN_POINT('Ctrl Pts',(13.8330719564107,0.989227075666942,26.5815875829136));
#41013=CARTESIAN_POINT('Ctrl Pts',(13.843681159309,0.975635450513119,26.7463823117722));
#41014=CARTESIAN_POINT('Ctrl Pts',(13.8542903622072,0.919969482494115,26.9077069132743));
#41015=CARTESIAN_POINT('Ctrl Pts',(13.8648995651055,0.829042239978501,27.0458165490801));
#41016=CARTESIAN_POINT('Ctrl Pts',(13.8755087680038,0.738114997462886,27.1839261848858));
#41017=CARTESIAN_POINT('Ctrl Pts',(13.8861179709021,0.611926480450659,27.2988208549953));
#41018=CARTESIAN_POINT('Ctrl Pts',(13.8967271738003,0.465921152126924,27.3764383725733));
#41019=CARTESIAN_POINT('Ctrl Pts',(13.9073363766986,0.319915823803185,27.4540558901513));
#41020=CARTESIAN_POINT('Ctrl Pts',(13.9179455795969,0.154093684167947,27.4943962551979));
#41021=CARTESIAN_POINT('Ctrl Pts',(13.9285547824951,-0.0112499658155442,
27.4925221303263));
#41022=CARTESIAN_POINT('Ctrl Pts',(13.9391639853934,-0.176593615799031,
27.4906480054546));
#41023=CARTESIAN_POINT('Ctrl Pts',(13.9497731882917,-0.341458776130763,
27.4465593906646));
#41024=CARTESIAN_POINT('Ctrl Pts',(13.96038239119,-0.485667272444817,27.3656523790727));
#41025=CARTESIAN_POINT('Ctrl Pts',(13.9709915940882,-0.62987576875887,27.2847453674808));
#41026=CARTESIAN_POINT('Ctrl Pts',(13.9816007969865,-0.75342760105525,27.1670199590869));
#41027=CARTESIAN_POINT('Ctrl Pts',(13.9922099998848,-0.84120101522721,27.0268848004061));
#41028=CARTESIAN_POINT('Ctrl Pts',(14.002819202783,-0.92897442939917,26.8867496417253));
#41029=CARTESIAN_POINT('Ctrl Pts',(14.0134284056813,-0.980969425446714,
26.7242047327576));
#41030=CARTESIAN_POINT('Ctrl Pts',(14.0240376085796,-0.990822232550754,
26.5591442676968));
#41031=CARTESIAN_POINT('Ctrl Pts',(14.0253028131743,-0.991997232872517,
26.5394599180989));
#41032=CARTESIAN_POINT('Ctrl Pts',(14.0265680177691,-0.992572893419552,
26.5197397926465));
#41033=CARTESIAN_POINT('Ctrl Pts',(14.0278332223638,-0.992555916844723,
26.5000186768892));
#41034=CARTESIAN_POINT('Origin',(18.,0.,26.5));
#41035=CARTESIAN_POINT('',(14.5721667776362,-0.992492707894564,26.5000909218272));
#41036=CARTESIAN_POINT('',(14.4278332223638,-0.992459136234123,26.4999764698814));
#41037=CARTESIAN_POINT('',(18.,-0.9925,26.5));
#41038=CARTESIAN_POINT('Ctrl Pts',(14.5721667776362,-0.992492707894564,
26.5000909218272));
#41039=CARTESIAN_POINT('Ctrl Pts',(14.5669149247572,-0.99244755231627,26.5819256581969));
#41040=CARTESIAN_POINT('Ctrl Pts',(14.5616630718781,-0.982361046646003,
26.6637403493712));
#41041=CARTESIAN_POINT('Ctrl Pts',(14.5564112189991,-0.962284559437845,
26.7430744931871));
#41042=CARTESIAN_POINT('Ctrl Pts',(14.5458256834985,-0.921818770893843,
26.9029788955205));
#41043=CARTESIAN_POINT('Ctrl Pts',(14.535240147998,-0.840768010570442,27.0528059074049));
#41044=CARTESIAN_POINT('Ctrl Pts',(14.5246546124975,-0.728778863616166,
27.1739578340904));
#41045=CARTESIAN_POINT('Ctrl Pts',(14.5140690769969,-0.616789716661883,
27.2951097607759));
#41046=CARTESIAN_POINT('Ctrl Pts',(14.5034835414964,-0.473862183076721,
27.3875866022624));
#41047=CARTESIAN_POINT('Ctrl Pts',(14.4928980059959,-0.317532787833618,
27.4403738110395));
#41048=CARTESIAN_POINT('Ctrl Pts',(14.4823124704953,-0.161203392590524,
27.4931610198166));
#41049=CARTESIAN_POINT('Ctrl Pts',(14.4717269349948,0.00852786431050967,
27.5062585958844));
#41050=CARTESIAN_POINT('Ctrl Pts',(14.4611413994943,0.171036982825635,27.4777955536263));
#41051=CARTESIAN_POINT('Ctrl Pts',(14.4505558639937,0.333546101340761,27.4493325113683));
#41052=CARTESIAN_POINT('Ctrl Pts',(14.4399703284932,0.488833081469978,27.3793088507844));
#41053=CARTESIAN_POINT('Ctrl Pts',(14.4293847929927,0.617951802230289,27.2766674659666));
#41054=CARTESIAN_POINT('Ctrl Pts',(14.4187992574921,0.7470705229906,27.1740260811488));
#41055=CARTESIAN_POINT('Ctrl Pts',(14.4082137219916,0.850020984382004,27.0387669720972));
#41056=CARTESIAN_POINT('Ctrl Pts',(14.3976281864911,0.914254878263044,26.8866586219403));
#41057=CARTESIAN_POINT('Ctrl Pts',(14.3870426509905,0.978488772144085,26.7345502717833));
#41058=CARTESIAN_POINT('Ctrl Pts',(14.37645711549,1.00400609851476,26.565592680521));
#41059=CARTESIAN_POINT('Ctrl Pts',(14.3658715799895,0.987727198252969,26.4016716323048));
#41060=CARTESIAN_POINT('Ctrl Pts',(14.355286044489,0.971448297991179,26.2377505840885));
#41061=CARTESIAN_POINT('Ctrl Pts',(14.3447005089884,0.913373171096924,26.0788660789183));
#41062=CARTESIAN_POINT('Ctrl Pts',(14.3341149734879,0.820514056354027,25.9421074708667));
#41063=CARTESIAN_POINT('Ctrl Pts',(14.3235294379874,0.72765494161113,25.8053488628151));
#41064=CARTESIAN_POINT('Ctrl Pts',(14.3129439024868,0.600011839019592,25.6907161518822));
#41065=CARTESIAN_POINT('Ctrl Pts',(14.3023583669863,0.453243444191403,25.6158107715758));
#41066=CARTESIAN_POINT('Ctrl Pts',(14.2811872959852,0.159706654535029,25.4660000109631));
#41067=CARTESIAN_POINT('Ctrl Pts',(14.2600162249842,-0.210331304067943,
25.4750985728568));
#41068=CARTESIAN_POINT('Ctrl Pts',(14.2388451539831,-0.496150677754313,
25.6391546501678));
#41069=CARTESIAN_POINT('Ctrl Pts',(14.2282596184826,-0.639060364597492,
25.7211826888233));
#41070=CARTESIAN_POINT('Ctrl Pts',(14.217674082982,-0.760915405211523,25.841950106333));
#41071=CARTESIAN_POINT('Ctrl Pts',(14.2070885474815,-0.84694107800222,25.9831071666876));
#41072=CARTESIAN_POINT('Ctrl Pts',(14.196503011981,-0.932966750792924,26.1242642270422));
#41073=CARTESIAN_POINT('Ctrl Pts',(14.1859174764804,-0.983163055760287,
26.2858109302416));
#41074=CARTESIAN_POINT('Ctrl Pts',(14.1753319409799,-0.991366112532681,
26.4503339453539));
#41075=CARTESIAN_POINT('Ctrl Pts',(14.174276886532,-0.992183706648124,26.4667318629526));
#41076=CARTESIAN_POINT('Ctrl Pts',(14.1732218320841,-0.992584139909162,
26.4831593472286));
#41077=CARTESIAN_POINT('Ctrl Pts',(14.1721667776362,-0.992571522832967,
26.4995949047598));
#41078=CARTESIAN_POINT('Ctrl Pts',(14.0278332223638,-0.992555916844723,
26.5000186768892));
#41079=CARTESIAN_POINT('Ctrl Pts',(14.0371772206673,-0.992430538635496,
26.3543710299033));
#41080=CARTESIAN_POINT('Ctrl Pts',(14.0465212189709,-0.959980584759993,
26.208669368106));
#41081=CARTESIAN_POINT('Ctrl Pts',(14.0558652172744,-0.89790604859668,26.0769261662407));
#41082=CARTESIAN_POINT('Ctrl Pts',(14.0664744201727,-0.827426439378023,
25.9273445509992));
#41083=CARTESIAN_POINT('Ctrl Pts',(14.077083623071,-0.718756602780171,25.7957573416698));
#41084=CARTESIAN_POINT('Ctrl Pts',(14.0876928259692,-0.585196855903322,
25.6982697581112));
#41085=CARTESIAN_POINT('Ctrl Pts',(14.0983020288675,-0.451637109026474,
25.6007821745526));
#41086=CARTESIAN_POINT('Ctrl Pts',(14.1089112317658,-0.29318745187063,25.5373942167648));
#41087=CARTESIAN_POINT('Ctrl Pts',(14.119520434664,-0.129240852627964,25.5158640627788));
#41088=CARTESIAN_POINT('Ctrl Pts',(14.1301296375623,0.0347057466146934,
25.4943339087927));
#41089=CARTESIAN_POINT('Ctrl Pts',(14.1407388404606,0.20414928794417,25.5146615586084));
#41090=CARTESIAN_POINT('Ctrl Pts',(14.1513480433589,0.358351239852387,25.5743590707977));
#41091=CARTESIAN_POINT('Ctrl Pts',(14.1619572462571,0.512553191760612,25.634056582987));
#41092=CARTESIAN_POINT('Ctrl Pts',(14.1725664491554,0.651513554247573,25.73312395755));
#41093=CARTESIAN_POINT('Ctrl Pts',(14.1831756520537,0.7582246925979,25.8594361417836));
#41094=CARTESIAN_POINT('Ctrl Pts',(14.193784854952,0.864935830948223,25.9857483260173));
#41095=CARTESIAN_POINT('Ctrl Pts',(14.2043940578502,0.939397745161913,26.1393053199216));
#41096=CARTESIAN_POINT('Ctrl Pts',(14.2150032607485,0.972496893690223,26.3013129780758));
#41097=CARTESIAN_POINT('Ctrl Pts',(14.2256124636468,1.00559604221853,26.4633206362299));
#41098=CARTESIAN_POINT('Ctrl Pts',(14.236221666545,0.997332425061462,26.6337789586339));
#41099=CARTESIAN_POINT('Ctrl Pts',(14.2468308694433,0.948717442732942,26.7918252127088));
#41100=CARTESIAN_POINT('Ctrl Pts',(14.2574400723416,0.900102460404423,26.9498714667836));
#41101=CARTESIAN_POINT('Ctrl Pts',(14.2680492752399,0.811136112904449,27.0955056525294));
#41102=CARTESIAN_POINT('Ctrl Pts',(14.2786584781381,0.692707168174913,27.2109033127489));
#41103=CARTESIAN_POINT('Ctrl Pts',(14.2892676810364,0.574278223445373,27.3263009729684));
#41104=CARTESIAN_POINT('Ctrl Pts',(14.2998768839347,0.426386681486266,27.4114621076618));
#41105=CARTESIAN_POINT('Ctrl Pts',(14.3104860868329,0.267133281804292,27.455963676439));
#41106=CARTESIAN_POINT('Ctrl Pts',(14.3210952897312,0.107879882122317,27.5004652452162));
#41107=CARTESIAN_POINT('Ctrl Pts',(14.3317044926295,-0.0627353752825216,
27.5043072480772));
#41108=CARTESIAN_POINT('Ctrl Pts',(14.3423136955278,-0.22383055024486,27.4670194546623));
#41109=CARTESIAN_POINT('Ctrl Pts',(14.352922898426,-0.384925725207203,27.4297316612474));
#41110=CARTESIAN_POINT('Ctrl Pts',(14.3635321013243,-0.536500817727043,
27.3513140715566));
#41111=CARTESIAN_POINT('Ctrl Pts',(14.3741413042226,-0.660004251229673,
27.2413643701157));
#41112=CARTESIAN_POINT('Ctrl Pts',(14.3847505071209,-0.783507684732299,
27.1314146686747));
#41113=CARTESIAN_POINT('Ctrl Pts',(14.3953597100191,-0.878939459217715,
26.9899328554835));
#41114=CARTESIAN_POINT('Ctrl Pts',(14.4059689129174,-0.934619490296102,
26.8342351706163));
#41115=CARTESIAN_POINT('Ctrl Pts',(14.4132570160662,-0.972869471347363,
26.727277013795));
#41116=CARTESIAN_POINT('Ctrl Pts',(14.420545119215,-0.992360020119326,26.6136101780797));
#41117=CARTESIAN_POINT('Ctrl Pts',(14.4278332223638,-0.992459136234123,
26.4999764698814));
#41118=CARTESIAN_POINT('Origin',(18.,0.,26.5));
#41119=CARTESIAN_POINT('',(14.9721667776363,-0.992543902023409,26.5000135256884));
#41120=CARTESIAN_POINT('',(14.8278332223638,-0.992487339104761,26.5000259875884));
#41121=CARTESIAN_POINT('',(18.,-0.9925,26.5));
#41122=CARTESIAN_POINT('Ctrl Pts',(14.9721667776362,-0.992609386691394,
26.5000337007337));
#41123=CARTESIAN_POINT('Ctrl Pts',(14.9711935529308,-0.992625808208597,
26.5152038908542));
#41124=CARTESIAN_POINT('Ctrl Pts',(14.9702203282253,-0.992289639355945,
26.530373213192));
#41125=CARTESIAN_POINT('Ctrl Pts',(14.9692471035198,-0.99159729580047,26.5455257855143));
#41126=CARTESIAN_POINT('Ctrl Pts',(14.9586615680193,-0.98406683829784,26.7103367395949));
#41127=CARTESIAN_POINT('Ctrl Pts',(14.9480760325187,-0.934399490014543,
26.873166099916));
#41128=CARTESIAN_POINT('Ctrl Pts',(14.9374904970182,-0.848903141093112,
27.0142892502091));
#41129=CARTESIAN_POINT('Ctrl Pts',(14.9269049615177,-0.763406792171678,
27.1554124005022));
#41130=CARTESIAN_POINT('Ctrl Pts',(14.9163194260172,-0.642081442612108,
27.2748293407674));
#41131=CARTESIAN_POINT('Ctrl Pts',(14.9057338905166,-0.499489145232929,
27.3578160571941));
#41132=CARTESIAN_POINT('Ctrl Pts',(14.8951483550161,-0.356896847853745,
27.4408027736207));
#41133=CARTESIAN_POINT('Ctrl Pts',(14.8845628195156,-0.193037602654965,
27.4873592662088));
#41134=CARTESIAN_POINT('Ctrl Pts',(14.873977284015,-0.0281609175057919,
27.4921107525352));
#41135=CARTESIAN_POINT('Ctrl Pts',(14.8633917485145,0.136715767643367,27.4968622388615));
#41136=CARTESIAN_POINT('Ctrl Pts',(14.852806213014,0.302609892742916,27.4598087189262));
#41137=CARTESIAN_POINT('Ctrl Pts',(14.8422206775134,0.449763830553274,27.384917718816));
#41138=CARTESIAN_POINT('Ctrl Pts',(14.8316351420129,0.596917768363644,27.3100267187059));
#41139=CARTESIAN_POINT('Ctrl Pts',(14.8210496065124,0.725331518884833,27.197298238421));
#41140=CARTESIAN_POINT('Ctrl Pts',(14.8104640710118,0.818543675128617,27.0614799533102));
#41141=CARTESIAN_POINT('Ctrl Pts',(14.7998785355113,0.911755831372396,26.9256616681994));
#41142=CARTESIAN_POINT('Ctrl Pts',(14.7892930000108,0.969766393338773,26.7667535782628));
#41143=CARTESIAN_POINT('Ctrl Pts',(14.7787074645102,0.986921312052431,26.6023411674448));
#41144=CARTESIAN_POINT('Ctrl Pts',(14.7681219290097,1.00407623076609,26.4379287566269));
#41145=CARTESIAN_POINT('Ctrl Pts',(14.7575363935092,0.980375506227025,26.2680120249276));
#41146=CARTESIAN_POINT('Ctrl Pts',(14.7469508580086,0.916445647298258,26.1161411888312));
#41147=CARTESIAN_POINT('Ctrl Pts',(14.7257797870076,0.788585929440723,25.8123995166384));
#41148=CARTESIAN_POINT('Ctrl Pts',(14.7046087160065,0.49980967402437,25.5808414268568));
#41149=CARTESIAN_POINT('Ctrl Pts',(14.6834376450054,0.175541983023264,25.5220402750828));
#41150=CARTESIAN_POINT('Ctrl Pts',(14.6728521095049,0.013408137522709,25.4926396991958));
#41151=CARTESIAN_POINT('Ctrl Pts',(14.6622665740044,-0.157598566874034,
25.5064283578108));
#41152=CARTESIAN_POINT('Ctrl Pts',(14.6516810385039,-0.31435451270915,25.5589003075781));
#41153=CARTESIAN_POINT('Ctrl Pts',(14.6410955030033,-0.47111045854426,25.6113722573453));
#41154=CARTESIAN_POINT('Ctrl Pts',(14.6305099675028,-0.613615645817744,
25.702527498265));
#41155=CARTESIAN_POINT('Ctrl Pts',(14.6199244320022,-0.725933430857789,
25.8230257464088));
#41156=CARTESIAN_POINT('Ctrl Pts',(14.6093388965017,-0.838251215897837,
25.9435239945527));
#41157=CARTESIAN_POINT('Ctrl Pts',(14.5987533610012,-0.920381598704446,
26.0933652499209));
#41158=CARTESIAN_POINT('Ctrl Pts',(14.5881678255007,-0.961506381725449,
26.2532767739961));
#41159=CARTESIAN_POINT('Ctrl Pts',(14.5828341428792,-0.982227727424042,
26.3338506209113));
#41160=CARTESIAN_POINT('Ctrl Pts',(14.5775004602577,-0.992538567047276,
26.4169811087267));
#41161=CARTESIAN_POINT('Ctrl Pts',(14.5721667776362,-0.992492707894564,
26.5000909218272));
#41162=CARTESIAN_POINT('Ctrl Pts',(14.4278332223638,-0.992459136234123,
26.4999764698814));
#41163=CARTESIAN_POINT('Ctrl Pts',(14.4311543221133,-0.992504302239228,
26.4481949744602));
#41164=CARTESIAN_POINT('Ctrl Pts',(14.4344754218628,-0.988522810522003,
26.3964203580136));
#41165=CARTESIAN_POINT('Ctrl Pts',(14.4377965216122,-0.980454858551326,
26.3452905585901));
#41166=CARTESIAN_POINT('Ctrl Pts',(14.4484057245105,-0.954681908056806,
26.1819571879744));
#41167=CARTESIAN_POINT('Ctrl Pts',(14.4590149274088,-0.887207719396409,
26.0252040032861));
#41168=CARTESIAN_POINT('Ctrl Pts',(14.469624130307,-0.786290592512034,25.8942163380832));
#41169=CARTESIAN_POINT('Ctrl Pts',(14.4802333332053,-0.685373465627659,
25.7632286728803));
#41170=CARTESIAN_POINT('Ctrl Pts',(14.4908425361036,-0.551013400519304,
25.6580065271629));
#41171=CARTESIAN_POINT('Ctrl Pts',(14.5014517390018,-0.399654992370801,
25.5914282482977));
#41172=CARTESIAN_POINT('Ctrl Pts',(14.5120609419001,-0.248296584222298,
25.5248499694325));
#41173=CARTESIAN_POINT('Ctrl Pts',(14.5226701447984,-0.0799398330336454,
25.4969155574197));
#41174=CARTESIAN_POINT('Ctrl Pts',(14.5332793476967,0.0848097440905795,
25.5110439604181));
#41175=CARTESIAN_POINT('Ctrl Pts',(14.5438885505949,0.249559321214804,25.5251723634165));
#41176=CARTESIAN_POINT('Ctrl Pts',(14.5544977534932,0.410701724274602,25.5813635814262));
#41177=CARTESIAN_POINT('Ctrl Pts',(14.5651069563915,0.548514414559299,25.6727402596893));
#41178=CARTESIAN_POINT('Ctrl Pts',(14.5757161592898,0.686327104843997,25.7641169379523));
#41179=CARTESIAN_POINT('Ctrl Pts',(14.586325362188,0.800810082353595,25.8906790764687));
#41180=CARTESIAN_POINT('Ctrl Pts',(14.5969345650863,0.877951548127839,26.0369364837755));
#41181=CARTESIAN_POINT('Ctrl Pts',(14.6075437679846,0.955093013902084,26.1831938910823));
#41182=CARTESIAN_POINT('Ctrl Pts',(14.6181529708829,0.994892967940975,26.3491465671794));
#41183=CARTESIAN_POINT('Ctrl Pts',(14.6287621737811,0.992480214834056,26.5144832344869));
#41184=CARTESIAN_POINT('Ctrl Pts',(14.6393713766794,0.990067461727136,26.6798199017944));
#41185=CARTESIAN_POINT('Ctrl Pts',(14.6499805795777,0.945442001474406,26.8445405603122));
#41186=CARTESIAN_POINT('Ctrl Pts',(14.6605897824759,0.864065632774431,26.9884847215383));
#41187=CARTESIAN_POINT('Ctrl Pts',(14.6711989853742,0.782689264074457,27.1324288827645));
#41188=CARTESIAN_POINT('Ctrl Pts',(14.6818081882725,0.664561986927239,27.255596546699));
#41189=CARTESIAN_POINT('Ctrl Pts',(14.6924173911708,0.524141633362612,27.3429129783639));
#41190=CARTESIAN_POINT('Ctrl Pts',(14.703026594069,0.38372127979798,27.4302294100287));
#41191=CARTESIAN_POINT('Ctrl Pts',(14.7136357969673,0.221007849815937,27.4816946094239));
#41192=CARTESIAN_POINT('Ctrl Pts',(14.7242449998656,0.0559161632319498,
27.4910096485946));
#41193=CARTESIAN_POINT('Ctrl Pts',(14.7348542027638,-0.109175523352037,
27.5003246877654));
#41194=CARTESIAN_POINT('Ctrl Pts',(14.7454634056621,-0.276645466537967,
27.4674895667118));
#41195=CARTESIAN_POINT('Ctrl Pts',(14.7560726085604,-0.425996687413761,
27.3965230411042));
#41196=CARTESIAN_POINT('Ctrl Pts',(14.7666818114587,-0.57534790828955,27.3255565154967));
#41197=CARTESIAN_POINT('Ctrl Pts',(14.7772910143569,-0.706580406855203,
27.2164585853352));
#41198=CARTESIAN_POINT('Ctrl Pts',(14.7879002172552,-0.803632377006842,
27.0825819629414));
#41199=CARTESIAN_POINT('Ctrl Pts',(14.7985094201535,-0.900684347158478,
26.9487053405475));
#41200=CARTESIAN_POINT('Ctrl Pts',(14.8091186230517,-0.963555788896102,
26.7900500259213));
#41201=CARTESIAN_POINT('Ctrl Pts',(14.81972782595,-0.984551741613934,26.6260341580811));
#41202=CARTESIAN_POINT('Ctrl Pts',(14.8224296247546,-0.989898688080915,
26.5842649620431));
#41203=CARTESIAN_POINT('Ctrl Pts',(14.8251314235592,-0.992529818241405,
26.5421481096989));
#41204=CARTESIAN_POINT('Ctrl Pts',(14.8278332223638,-0.992487339104761,
26.5000259875884));
#41205=CARTESIAN_POINT('Origin',(18.,0.,26.5));
#41206=CARTESIAN_POINT('',(15.3721667776362,-0.9925,26.4999999999999));
#41207=CARTESIAN_POINT('',(15.2278332223638,-0.992527725525489,26.4999759343258));
#41208=CARTESIAN_POINT('',(18.,-0.9925,26.5));
#41209=CARTESIAN_POINT('Ctrl Pts',(15.3721667776362,-0.9925,26.4999999999999));
#41210=CARTESIAN_POINT('Ctrl Pts',(15.3554259338597,-0.992500000000016,
26.7609923249228));
#41211=CARTESIAN_POINT('Ctrl Pts',(15.3386850900832,-0.884539443097445,
27.0203491301746));
#41212=CARTESIAN_POINT('Ctrl Pts',(15.3219442463066,-0.699346033936964,
27.2042523516586));
#41213=CARTESIAN_POINT('Ctrl Pts',(15.3052034025301,-0.514152624776482,
27.3881555731425));
#41214=CARTESIAN_POINT('Ctrl Pts',(15.2884625587536,-0.254047408344541,
27.4943003359056));
#41215=CARTESIAN_POINT('Ctrl Pts',(15.271721714977,0.00693853867338895,
27.4924757461425));
#41216=CARTESIAN_POINT('Ctrl Pts',(15.2549808712005,0.267924485691319,27.4906511563793));
#41217=CARTESIAN_POINT('Ctrl Pts',(15.238240027424,0.526520203887957,27.3808800818309));
#41218=CARTESIAN_POINT('Ctrl Pts',(15.2214991836474,0.709124249559236,27.1944055361869));
#41219=CARTESIAN_POINT('Ctrl Pts',(15.2047583398709,0.891728295230515,27.0079309905429));
#41220=CARTESIAN_POINT('Ctrl Pts',(15.1880174960944,0.996052076106157,26.747090075384));
#41221=CARTESIAN_POINT('Ctrl Pts',(15.1712766523178,0.99240298575532,26.4861232617692));
#41222=CARTESIAN_POINT('Ctrl Pts',(15.1545358085413,0.988753895404483,26.2251564481544));
#41223=CARTESIAN_POINT('Ctrl Pts',(15.1377949647648,0.877177668191593,25.9673344556904));
#41224=CARTESIAN_POINT('Ctrl Pts',(15.1210541209882,0.68943109987178,25.7860385104716));
#41225=CARTESIAN_POINT('Ctrl Pts',(15.1043132772117,0.501684531551967,25.6047425652528));
#41226=CARTESIAN_POINT('Ctrl Pts',(15.0875724334352,0.240120666075862,25.5022448650135));
#41227=CARTESIAN_POINT('Ctrl Pts',(15.0708315896586,-0.0208142595727541,
25.5077182776054));
#41228=CARTESIAN_POINT('Ctrl Pts',(15.0540907458821,-0.28174918522137,25.5131916901973));
#41229=CARTESIAN_POINT('Ctrl Pts',(15.0373499021056,-0.538784851090443,
25.6265676168677));
#41230=CARTESIAN_POINT('Ctrl Pts',(15.020609058329,-0.718763835149441,25.8155770318865));
#41231=CARTESIAN_POINT('Ctrl Pts',(15.0044616314314,-0.892363059118749,
25.9978865828694));
#41232=CARTESIAN_POINT('Ctrl Pts',(14.9883142045338,-0.992499999999987,
26.2482591353349));
#41233=CARTESIAN_POINT('Ctrl Pts',(14.9721667776362,-0.9925,26.4999999999999));
#41234=CARTESIAN_POINT('Ctrl Pts',(14.8278332223638,-0.992487339104761,
26.5000259875884));
#41235=CARTESIAN_POINT('Ctrl Pts',(14.8357406264575,-0.992363014636773,
26.3767464005799));
#41236=CARTESIAN_POINT('Ctrl Pts',(14.8436480305512,-0.969337407946782,
26.2534216744387));
#41237=CARTESIAN_POINT('Ctrl Pts',(14.8515554346448,-0.92446862061909,26.1386352114429));
#41238=CARTESIAN_POINT('Ctrl Pts',(14.8621646375431,-0.864269083208378,
25.9846285536991));
#41239=CARTESIAN_POINT('Ctrl Pts',(14.8727738404414,-0.764749544688916,
25.8459916592655));
#41240=CARTESIAN_POINT('Ctrl Pts',(14.8833830433397,-0.638090399008227,
25.7396925729603));
#41241=CARTESIAN_POINT('Ctrl Pts',(14.8939922462379,-0.511431253327537,
25.633393486655));
#41242=CARTESIAN_POINT('Ctrl Pts',(14.9046014491362,-0.35763250048562,25.559432208478));
#41243=CARTESIAN_POINT('Ctrl Pts',(14.9152106520345,-0.195517875259795,
25.5268610061393));
#41244=CARTESIAN_POINT('Ctrl Pts',(14.9258198549328,-0.0334032500339701,
25.4942898038006));
#41245=CARTESIAN_POINT('Ctrl Pts',(14.936429057831,0.137027247575762,25.5031086773003));
#41246=CARTESIAN_POINT('Ctrl Pts',(14.9470382607293,0.294914290522258,25.5522382671979));
#41247=CARTESIAN_POINT('Ctrl Pts',(14.9576474636276,0.452801333468754,25.6013678570955));
#41248=CARTESIAN_POINT('Ctrl Pts',(14.9682566665258,0.598144921752012,25.6908081633911));
#41249=CARTESIAN_POINT('Ctrl Pts',(14.9788658694241,0.713156164975501,25.8096124093846));
#41250=CARTESIAN_POINT('Ctrl Pts',(14.9894750723224,0.82816740819899,25.9284166553781));
#41251=CARTESIAN_POINT('Ctrl Pts',(15.0000842752207,0.91284630636271,26.0765848410695));
#41252=CARTESIAN_POINT('Ctrl Pts',(15.0106934781189,0.956828840963156,26.2359823679764));
#41253=CARTESIAN_POINT('Ctrl Pts',(15.0213026810172,1.0008113755636,26.3953798948832));
#41254=CARTESIAN_POINT('Ctrl Pts',(15.0319118839155,1.00409754660077,26.5660067630055));
#41255=CARTESIAN_POINT('Ctrl Pts',(15.0425210868137,0.966285153075671,26.7269796111191));
#41256=CARTESIAN_POINT('Ctrl Pts',(15.053130289712,0.928472759550572,26.8879524592327));
#41257=CARTESIAN_POINT('Ctrl Pts',(15.0637394926103,0.849561801463207,27.0392712873376));
#41258=CARTESIAN_POINT('Ctrl Pts',(15.0743486955086,0.739210347677032,27.1624158835697));
#41259=CARTESIAN_POINT('Ctrl Pts',(15.0849578984068,0.628858893890858,27.2855604798019));
#41260=CARTESIAN_POINT('Ctrl Pts',(15.0955671013051,0.487066944405874,27.3805308441612));
#41261=CARTESIAN_POINT('Ctrl Pts',(15.1061763042034,0.331188697493168,27.4357033651596));
#41262=CARTESIAN_POINT('Ctrl Pts',(15.1167855071017,0.175310450580462,27.490875886158));
#41263=CARTESIAN_POINT('Ctrl Pts',(15.1273947099999,0.00534590624003523,
27.5062505637954));
#41264=CARTESIAN_POINT('Ctrl Pts',(15.1380039128982,-0.1579026374269,27.4799456607445));
#41265=CARTESIAN_POINT('Ctrl Pts',(15.1486131157965,-0.321151181093836,
27.4536407576935));
#41266=CARTESIAN_POINT('Ctrl Pts',(15.1592223186947,-0.47768372408728,27.3856562739541));
#41267=CARTESIAN_POINT('Ctrl Pts',(15.169831521593,-0.608341937624443,27.2843129654963));
#41268=CARTESIAN_POINT('Ctrl Pts',(15.1804407244913,-0.739000151161607,
27.1829696570385));
#41269=CARTESIAN_POINT('Ctrl Pts',(15.1910499273896,-0.84378403524249,27.0482675238623));
#41270=CARTESIAN_POINT('Ctrl Pts',(15.2016591302878,-0.909868882212257,
26.8966930275415));
#41271=CARTESIAN_POINT('Ctrl Pts',(15.2103838276465,-0.964215122484324,
26.7720426065467));
#41272=CARTESIAN_POINT('Ctrl Pts',(15.2191085250052,-0.992389454393167,
26.6359815155442));
#41273=CARTESIAN_POINT('Ctrl Pts',(15.2278332223638,-0.992527725525489,
26.4999759343258));
#41274=CARTESIAN_POINT('Origin',(18.,0.,26.5));
#41275=CARTESIAN_POINT('',(15.7721667776362,-0.99246122082366,26.5000241305601));
#41276=CARTESIAN_POINT('',(15.6278332223638,-0.992430455435604,26.5000159512924));
#41277=CARTESIAN_POINT('',(18.,-0.9925,26.5));
#41278=CARTESIAN_POINT('Ctrl Pts',(15.7721667776362,-0.9925,26.4999999999999));
#41279=CARTESIAN_POINT('Ctrl Pts',(15.7554259338597,-0.992500000000018,
26.7609923249228));
#41280=CARTESIAN_POINT('Ctrl Pts',(15.7386850900832,-0.884539443097449,
27.0203491301746));
#41281=CARTESIAN_POINT('Ctrl Pts',(15.7219442463066,-0.699346033936969,
27.2042523516586));
#41282=CARTESIAN_POINT('Ctrl Pts',(15.7052034025301,-0.514152624776489,
27.3881555731425));
#41283=CARTESIAN_POINT('Ctrl Pts',(15.6884625587536,-0.254047408344548,
27.4943003359056));
#41284=CARTESIAN_POINT('Ctrl Pts',(15.671721714977,0.00693853867338218,
27.4924757461425));
#41285=CARTESIAN_POINT('Ctrl Pts',(15.6549808712005,0.267924485691312,27.4906511563793));
#41286=CARTESIAN_POINT('Ctrl Pts',(15.638240027424,0.526520203887951,27.3808800818309));
#41287=CARTESIAN_POINT('Ctrl Pts',(15.6214991836474,0.709124249559231,27.1944055361869));
#41288=CARTESIAN_POINT('Ctrl Pts',(15.6047583398709,0.891728295230511,27.0079309905429));
#41289=CARTESIAN_POINT('Ctrl Pts',(15.5880174960944,0.996052076106155,26.747090075384));
#41290=CARTESIAN_POINT('Ctrl Pts',(15.5712766523178,0.99240298575532,26.4861232617692));
#41291=CARTESIAN_POINT('Ctrl Pts',(15.5545358085413,0.988753895404485,26.2251564481544));
#41292=CARTESIAN_POINT('Ctrl Pts',(15.5377949647648,0.877177668191597,25.9673344556904));
#41293=CARTESIAN_POINT('Ctrl Pts',(15.5210541209882,0.689431099871785,25.7860385104716));
#41294=CARTESIAN_POINT('Ctrl Pts',(15.5043132772117,0.501684531551973,25.6047425652528));
#41295=CARTESIAN_POINT('Ctrl Pts',(15.4875724334352,0.240120666075869,25.5022448650135));
#41296=CARTESIAN_POINT('Ctrl Pts',(15.4708315896586,-0.0208142595727472,
25.5077182776054));
#41297=CARTESIAN_POINT('Ctrl Pts',(15.4540907458821,-0.281749185221363,
25.5131916901973));
#41298=CARTESIAN_POINT('Ctrl Pts',(15.4373499021056,-0.538784851090437,
25.6265676168677));
#41299=CARTESIAN_POINT('Ctrl Pts',(15.420609058329,-0.718763835149436,25.8155770318865));
#41300=CARTESIAN_POINT('Ctrl Pts',(15.4044616314314,-0.892363059118746,
25.9978865828694));
#41301=CARTESIAN_POINT('Ctrl Pts',(15.3883142045338,-0.992499999999985,
26.2482591353348));
#41302=CARTESIAN_POINT('Ctrl Pts',(15.3721667776362,-0.9925,26.4999999999999));
#41303=CARTESIAN_POINT('Ctrl Pts',(15.2278332223638,-0.992527725525489,
26.4999759343258));
#41304=CARTESIAN_POINT('Ctrl Pts',(15.2297177279034,-0.992557591629048,
26.4705991822521));
#41305=CARTESIAN_POINT('Ctrl Pts',(15.231602233443,-0.991279447663092,26.4412250199629));
#41306=CARTESIAN_POINT('Ctrl Pts',(15.2334867389827,-0.988674508136253,
26.4119689947814));
#41307=CARTESIAN_POINT('Ctrl Pts',(15.2440959418809,-0.974009477231833,
26.2472663178072));
#41308=CARTESIAN_POINT('Ctrl Pts',(15.2547051447792,-0.917293605564346,
26.086307823324));
#41309=CARTESIAN_POINT('Ctrl Pts',(15.2653143476775,-0.825468461294819,
25.9487935411066));
#41310=CARTESIAN_POINT('Ctrl Pts',(15.2759235505757,-0.733643317025287,
25.8112792588891));
#41311=CARTESIAN_POINT('Ctrl Pts',(15.286532753474,-0.606708900153712,25.6972091889375));
#41312=CARTESIAN_POINT('Ctrl Pts',(15.2971419563723,-0.460200966030206,
25.6205445936359));
#41313=CARTESIAN_POINT('Ctrl Pts',(15.3077511592706,-0.313693031906705,
25.5438799983342));
#41314=CARTESIAN_POINT('Ctrl Pts',(15.3183603621688,-0.147611580531275,
25.5046208776827));
#41315=CARTESIAN_POINT('Ctrl Pts',(15.3289695650671,0.0177163494539894,
25.5075722334193));
#41316=CARTESIAN_POINT('Ctrl Pts',(15.3395787679654,0.183044279439254,25.510523589156));
#41317=CARTESIAN_POINT('Ctrl Pts',(15.3501879708637,0.347618688034365,25.5556854212809));
#41318=CARTESIAN_POINT('Ctrl Pts',(15.3607971737619,0.491296986555805,25.6375302834769));
#41319=CARTESIAN_POINT('Ctrl Pts',(15.3714063766602,0.634975285077253,25.7193751456729));
#41320=CARTESIAN_POINT('Ctrl Pts',(15.3820155795585,0.757757473525031,25.83790303794));
#41321=CARTESIAN_POINT('Ctrl Pts',(15.3926247824567,0.844615996031423,25.9786070961682));
#41322=CARTESIAN_POINT('Ctrl Pts',(15.403233985355,0.931474518537809,26.1193111543965));
#41323=CARTESIAN_POINT('Ctrl Pts',(15.4138431882533,0.9824093751028,26.282191378586));
#41324=CARTESIAN_POINT('Ctrl Pts',(15.4244523911516,0.991186547483833,26.4473125346469));
#41325=CARTESIAN_POINT('Ctrl Pts',(15.4350615940498,0.999963719864865,26.6124336907078));
#41326=CARTESIAN_POINT('Ctrl Pts',(15.4456707969481,0.966583208061936,26.7797957786401));
#41327=CARTESIAN_POINT('Ctrl Pts',(15.4562799998464,0.895130519202377,26.9289150201505));
#41328=CARTESIAN_POINT('Ctrl Pts',(15.4668892027446,0.823677830342816,27.0780342616609));
#41329=CARTESIAN_POINT('Ctrl Pts',(15.4774984056429,0.714152964426622,27.2089106567494));
#41330=CARTESIAN_POINT('Ctrl Pts',(15.4881076085412,0.579960887290202,27.3055259835237));
#41331=CARTESIAN_POINT('Ctrl Pts',(15.4987168114395,0.445768810153782,27.402141310298));
#41332=CARTESIAN_POINT('Ctrl Pts',(15.5093260143377,0.286909521797139,27.4644955687583));
#41333=CARTESIAN_POINT('Ctrl Pts',(15.519935217236,0.122826125988562,27.4849570973869));
#41334=CARTESIAN_POINT('Ctrl Pts',(15.5305444201343,-0.0412572698200145,
27.5054186260156));
#41335=CARTESIAN_POINT('Ctrl Pts',(15.5411536230325,-0.210564773080522,
27.4839874248128));
#41336=CARTESIAN_POINT('Ctrl Pts',(15.5517628259308,-0.364374502254287,
27.4232865010522));
#41337=CARTESIAN_POINT('Ctrl Pts',(15.5623720288291,-0.518184231428048,
27.3625855772916));
#41338=CARTESIAN_POINT('Ctrl Pts',(15.5729812317274,-0.656496186515066,
27.2626149309732));
#41339=CARTESIAN_POINT('Ctrl Pts',(15.5835904346256,-0.762382092669272,
27.135610168024));
#41340=CARTESIAN_POINT('Ctrl Pts',(15.5941996375239,-0.868267998823484,
27.0086054050747));
#41341=CARTESIAN_POINT('Ctrl Pts',(15.6048088404222,-0.941727856044881,
26.8545665254945));
#41342=CARTESIAN_POINT('Ctrl Pts',(15.6154180433205,-0.973770766529909,
26.6923466536491));
#41343=CARTESIAN_POINT('Ctrl Pts',(15.6195564363349,-0.986269929585368,
26.6290686118502));
#41344=CARTESIAN_POINT('Ctrl Pts',(15.6236948293494,-0.992467126962446,
26.5645457575642));
#41345=CARTESIAN_POINT('Ctrl Pts',(15.6278332223638,-0.992430455435604,
26.5000159512924));
#41346=CARTESIAN_POINT('Origin',(18.,0.,26.5));
#41347=CARTESIAN_POINT('',(16.1721667776362,-0.992590313145785,26.499881711609));
#41348=CARTESIAN_POINT('',(16.0278332223638,-0.992581467290118,26.4999926332401));
#41349=CARTESIAN_POINT('',(18.,-0.9925,26.5));
#41350=CARTESIAN_POINT('Ctrl Pts',(16.1721667776362,-0.992590313145785,
26.499881711609));
#41351=CARTESIAN_POINT('Ctrl Pts',(16.1628583664504,-0.992388437590192,
26.645171964642));
#41352=CARTESIAN_POINT('Ctrl Pts',(16.1535499552646,-0.960027564764405,
26.7907481822402));
#41353=CARTESIAN_POINT('Ctrl Pts',(16.1442415440789,-0.898492852461372,
26.9218815949269));
#41354=CARTESIAN_POINT('Ctrl Pts',(16.1336560085783,-0.828515509540174,
27.0710066569378));
#41355=CARTESIAN_POINT('Ctrl Pts',(16.1230704730778,-0.720809788480869,
27.2014539029726));
#41356=CARTESIAN_POINT('Ctrl Pts',(16.1124849375773,-0.587682335814658,
27.2994478487736));
#41357=CARTESIAN_POINT('Ctrl Pts',(16.1018994020768,-0.454554883148454,
27.3974417945746));
#41358=CARTESIAN_POINT('Ctrl Pts',(16.0913138665762,-0.296005698875348,
27.4629824401418));
#41359=CARTESIAN_POINT('Ctrl Pts',(16.0807283310757,-0.132664255717563,
27.4846930519805));
#41360=CARTESIAN_POINT('Ctrl Pts',(16.0595572600746,0.194018630598016,27.5281142756581));
#41361=CARTESIAN_POINT('Ctrl Pts',(16.0383861890736,0.539870552452309,27.3962153644219));
#41362=CARTESIAN_POINT('Ctrl Pts',(16.0172151180725,0.754676553619223,27.1462843884709));
#41363=CARTESIAN_POINT('Ctrl Pts',(16.006629582572,0.862079554202677,27.0213189004954));
#41364=CARTESIAN_POINT('Ctrl Pts',(15.9960440470714,0.936721074614288,26.8668453963413));
#41365=CARTESIAN_POINT('Ctrl Pts',(15.9854585115709,0.970786327779025,26.7050885090262));
#41366=CARTESIAN_POINT('Ctrl Pts',(15.9748729760704,1.00485158094376,26.5433316217111));
#41367=CARTESIAN_POINT('Ctrl Pts',(15.9642874405698,0.998340566861622,26.3742913512351));
#41368=CARTESIAN_POINT('Ctrl Pts',(15.9537019050693,0.951245016724583,26.2164397696804));
#41369=CARTESIAN_POINT('Ctrl Pts',(15.9431163695688,0.904149466587543,26.0585881881256));
#41370=CARTESIAN_POINT('Ctrl Pts',(15.9325308340682,0.816469380395605,25.9119252954921));
#41371=CARTESIAN_POINT('Ctrl Pts',(15.9219452985677,0.699353476675405,25.7955345380996));
#41372=CARTESIAN_POINT('Ctrl Pts',(15.9113597630672,0.582237572955209,25.6791437807071));
#41373=CARTESIAN_POINT('Ctrl Pts',(15.9007742275666,0.435685851706754,25.5930251585557));
#41374=CARTESIAN_POINT('Ctrl Pts',(15.8901886920661,0.277288843390337,25.5470111858464));
#41375=CARTESIAN_POINT('Ctrl Pts',(15.8796031565656,0.118891835073919,25.5009972131371));
#41376=CARTESIAN_POINT('Ctrl Pts',(15.869017621065,-0.0513504603104619,
25.4950878898698));
#41377=CARTESIAN_POINT('Ctrl Pts',(15.8584320855645,-0.212515773811046,
25.5303738658292));
#41378=CARTESIAN_POINT('Ctrl Pts',(15.847846550064,-0.373681087311639,25.5656598417886));
#41379=CARTESIAN_POINT('Ctrl Pts',(15.8372610145634,-0.525769418928423,
25.6421411169746));
#41380=CARTESIAN_POINT('Ctrl Pts',(15.8266754790629,-0.650406542850507,
25.7502658438782));
#41381=CARTESIAN_POINT('Ctrl Pts',(15.8160899435624,-0.775043666772584,
25.8583905707819));
#41382=CARTESIAN_POINT('Ctrl Pts',(15.8055044080619,-0.872229582999959,
25.9981587494031));
#41383=CARTESIAN_POINT('Ctrl Pts',(15.7949188725613,-0.929914181101119,
26.1527286220079));
#41384=CARTESIAN_POINT('Ctrl Pts',(15.7873348409196,-0.971242446186617,
26.263470568377));
#41385=CARTESIAN_POINT('Ctrl Pts',(15.7797508092779,-0.992294528632976,
26.38181028274));
#41386=CARTESIAN_POINT('Ctrl Pts',(15.7721667776362,-0.992381283892664,
26.5000738717641));
#41387=CARTESIAN_POINT('Ctrl Pts',(15.6278332223638,-0.992430455435604,
26.5000159512924));
#41388=CARTESIAN_POINT('Ctrl Pts',(15.6343040322476,-0.992373115671711,
26.3991168567002));
#41389=CARTESIAN_POINT('Ctrl Pts',(15.6407748421315,-0.977074845476574,
26.2982007654828));
#41390=CARTESIAN_POINT('Ctrl Pts',(15.6472456520153,-0.946795964687865,
26.2019997614615));
#41391=CARTESIAN_POINT('Ctrl Pts',(15.6578548549136,-0.897152288612132,
26.0442736052299));
#41392=CARTESIAN_POINT('Ctrl Pts',(15.6684640578118,-0.807238972712001,
25.8992221568774));
#41393=CARTESIAN_POINT('Ctrl Pts',(15.6790732607101,-0.688060686272364,
25.7845985512143));
#41394=CARTESIAN_POINT('Ctrl Pts',(15.6896824636084,-0.568882399832727,
25.6699749455512));
#41395=CARTESIAN_POINT('Ctrl Pts',(15.7002916665066,-0.42043914285358,25.5857791825775));
#41396=CARTESIAN_POINT('Ctrl Pts',(15.7109008694049,-0.260899180338543,
25.5423161489213));
#41397=CARTESIAN_POINT('Ctrl Pts',(15.7215100723032,-0.101359217823505,
25.4988531152651));
#41398=CARTESIAN_POINT('Ctrl Pts',(15.7321192752015,0.0692774502274137,
25.4961228109265));
#41399=CARTESIAN_POINT('Ctrl Pts',(15.7427284780997,0.230126263157377,25.5344594032753));
#41400=CARTESIAN_POINT('Ctrl Pts',(15.753337680998,0.390975076087336,25.5727959956241));
#41401=CARTESIAN_POINT('Ctrl Pts',(15.7639468838963,0.542036033896329,25.6521994846604));
#41402=CARTESIAN_POINT('Ctrl Pts',(15.7745560867945,0.664820485977887,25.7629515196797));
#41403=CARTESIAN_POINT('Ctrl Pts',(15.7851652896928,0.787604938059444,25.8737035546991));
#41404=CARTESIAN_POINT('Ctrl Pts',(15.7957744925911,0.882112884413569,26.0158041357016));
#41405=CARTESIAN_POINT('Ctrl Pts',(15.8063836954894,0.936777309809986,26.1718612903917));
#41406=CARTESIAN_POINT('Ctrl Pts',(15.8169928983876,0.991441735206403,26.3279184450818));
#41407=CARTESIAN_POINT('Ctrl Pts',(15.8276021012859,1.00626263964511,26.4979321734596));
#41408=CARTESIAN_POINT('Ctrl Pts',(15.8382113041842,0.979426063200181,26.6610941576918));
#41409=CARTESIAN_POINT('Ctrl Pts',(15.8488205070824,0.952589486755249,26.8242561419241));
#41410=CARTESIAN_POINT('Ctrl Pts',(15.8594297099807,0.884095429426674,26.9805663820109));
#41411=CARTESIAN_POINT('Ctrl Pts',(15.870038912879,0.782327014907929,27.1108937572635));
#41412=CARTESIAN_POINT('Ctrl Pts',(15.8806481157773,0.680558600389184,27.2412211325161));
#41413=CARTESIAN_POINT('Ctrl Pts',(15.8912573186755,0.545515828680267,27.3455656429346));
#41414=CARTESIAN_POINT('Ctrl Pts',(15.9018665215738,0.393726852781588,27.4111563566792));
#41415=CARTESIAN_POINT('Ctrl Pts',(15.9124757244721,0.241937876882906,27.4767470704238));
#41416=CARTESIAN_POINT('Ctrl Pts',(15.9230849273704,0.0734026967944721,
27.5035839874945));
#41417=CARTESIAN_POINT('Ctrl Pts',(15.9336941302686,-0.0912513321117865,
27.4883824843177));
#41418=CARTESIAN_POINT('Ctrl Pts',(15.9443033331669,-0.25590536101804,27.4731809811409));
#41419=CARTESIAN_POINT('Ctrl Pts',(15.9549125360652,-0.416678238742111,
27.4159410577166));
#41420=CARTESIAN_POINT('Ctrl Pts',(15.9655217389634,-0.553892653512971,
27.3236684219409));
#41421=CARTESIAN_POINT('Ctrl Pts',(15.9761309418617,-0.691107068283828,
27.2313957861652));
#41422=CARTESIAN_POINT('Ctrl Pts',(15.98674014476,-0.804763020101481,27.1040904380383));
#41423=CARTESIAN_POINT('Ctrl Pts',(15.9973493476583,-0.880949931322436,
26.9573335319231));
#41424=CARTESIAN_POINT('Ctrl Pts',(16.0075106392268,-0.953920297338052,
26.8167725748909));
#41425=CARTESIAN_POINT('Ctrl Pts',(16.0176719307953,-0.992518656563027,
26.6583678441027));
#41426=CARTESIAN_POINT('Ctrl Pts',(16.0278332223638,-0.992581467290118,
26.4999926332401));
#41427=CARTESIAN_POINT('Origin',(18.,0.,26.5));
#41428=CARTESIAN_POINT('',(16.5721667776362,-0.992268890272332,26.499572269901));
#41429=CARTESIAN_POINT('',(16.4278332223638,-0.992414999655005,26.4999960454856));
#41430=CARTESIAN_POINT('',(18.,-0.9925,26.5));
#41431=CARTESIAN_POINT('Ctrl Pts',(16.5721667776362,-0.992268890272332,
26.499572269901));
#41432=CARTESIAN_POINT('Ctrl Pts',(16.567136994624,-0.992197798349475,26.5777683735014));
#41433=CARTESIAN_POINT('Ctrl Pts',(16.5621072116118,-0.982958907028698,
26.6560429188629));
#41434=CARTESIAN_POINT('Ctrl Pts',(16.5570774285996,-0.964609050907775,
26.7324150805005));
#41435=CARTESIAN_POINT('Ctrl Pts',(16.5464918930991,-0.925990475727351,
26.8931457176487));
#41436=CARTESIAN_POINT('Ctrl Pts',(16.5359063575986,-0.847017441008614,
27.0454502804246));
#41437=CARTESIAN_POINT('Ctrl Pts',(16.525320822098,-0.736129089314115,27.1673336311242));
#41438=CARTESIAN_POINT('Ctrl Pts',(16.504149751097,-0.514352385925116,27.4111003325234));
#41439=CARTESIAN_POINT('Ctrl Pts',(16.4829786800959,-0.164914414633087,
27.5331821856175));
#41440=CARTESIAN_POINT('Ctrl Pts',(16.4618076090948,0.160412328171246,27.4805549940388));
#41441=CARTESIAN_POINT('Ctrl Pts',(16.4512220735943,0.323075699573415,27.4542413982495));
#41442=CARTESIAN_POINT('Ctrl Pts',(16.4406365380938,0.479711263853668,27.384250541292));
#41443=CARTESIAN_POINT('Ctrl Pts',(16.4300510025932,0.610018972578666,27.2825370558838));
#41444=CARTESIAN_POINT('Ctrl Pts',(16.4194654670927,0.74032668130366,27.1808235704756));
#41445=CARTESIAN_POINT('Ctrl Pts',(16.4088799315922,0.844306534473414,27.0473874566168));
#41446=CARTESIAN_POINT('Ctrl Pts',(16.3982943960917,0.910045716302035,26.896346162215));
#41447=CARTESIAN_POINT('Ctrl Pts',(16.3877088605911,0.97578489813066,26.7453048678133));
#41448=CARTESIAN_POINT('Ctrl Pts',(16.3771233250906,1.00328340861815,26.5766583928687));
#41449=CARTESIAN_POINT('Ctrl Pts',(16.3665377895901,0.98876440761581,26.4121830393336));
#41450=CARTESIAN_POINT('Ctrl Pts',(16.3559522540895,0.974245406613472,26.2477076857986));
#41451=CARTESIAN_POINT('Ctrl Pts',(16.345366718589,0.917708894121311,26.087403453673));
#41452=CARTESIAN_POINT('Ctrl Pts',(16.3347811830884,0.826265950081132,25.9501260487101));
#41453=CARTESIAN_POINT('Ctrl Pts',(16.3241956475879,0.734823006040954,25.8128486437472));
#41454=CARTESIAN_POINT('Ctrl Pts',(16.3136101120874,0.608473630452758,25.6985980659469));
#41455=CARTESIAN_POINT('Ctrl Pts',(16.3030245765869,0.462510895873329,25.6216939796495));
#41456=CARTESIAN_POINT('Ctrl Pts',(16.2924390410863,0.316548161293896,25.544789893352));
#41457=CARTESIAN_POINT('Ctrl Pts',(16.2818535055858,0.150972067723229,25.5052322985575));
#41458=CARTESIAN_POINT('Ctrl Pts',(16.2712679700853,-0.0140126065616156,
25.5075617789023));
#41459=CARTESIAN_POINT('Ctrl Pts',(16.2606824345847,-0.178997280846465,
25.509891259247));
#41460=CARTESIAN_POINT('Ctrl Pts',(16.2500968990842,-0.343390535845491,
25.5541078147311));
#41461=CARTESIAN_POINT('Ctrl Pts',(16.2395113635837,-0.487123842434778,
25.6351022278228));
#41462=CARTESIAN_POINT('Ctrl Pts',(16.2289258280831,-0.630857149024054,
25.7160966409144));
#41463=CARTESIAN_POINT('Ctrl Pts',(16.2183402925826,-0.753930507203593,
25.8338689116136));
#41464=CARTESIAN_POINT('Ctrl Pts',(16.2077547570821,-0.841461229554299,
25.9736733127347));
#41465=CARTESIAN_POINT('Ctrl Pts',(16.1971692215815,-0.928991951905009,
26.1134777138559));
#41466=CARTESIAN_POINT('Ctrl Pts',(16.186583686081,-0.980980038426882,26.2753142453991));
#41467=CARTESIAN_POINT('Ctrl Pts',(16.1759981505805,-0.99084959929627,26.4401339501642));
#41468=CARTESIAN_POINT('Ctrl Pts',(16.1747210262657,-0.992040342661269,
26.4600191276779));
#41469=CARTESIAN_POINT('Ctrl Pts',(16.173443901951,-0.992618010695394,26.4799477281244));
#41470=CARTESIAN_POINT('Ctrl Pts',(16.1721667776362,-0.992590313145785,
26.499881711609));
#41471=CARTESIAN_POINT('Ctrl Pts',(16.0278332223638,-0.992581467290118,
26.4999926332401));
#41472=CARTESIAN_POINT('Ctrl Pts',(16.0282811336936,-0.992584235996843,
26.4930114290478));
#41473=CARTESIAN_POINT('Ctrl Pts',(16.0287290450233,-0.992512127810711,
26.4860302822144));
#41474=CARTESIAN_POINT('Ctrl Pts',(16.0291769563531,-0.992364786122702,
26.4790507235948));
#41475=CARTESIAN_POINT('Ctrl Pts',(16.0397861592514,-0.988874859077747,
26.3137332854852));
#41476=CARTESIAN_POINT('Ctrl Pts',(16.0503953621496,-0.943177134363577,
26.1493068733695));
#41477=CARTESIAN_POINT('Ctrl Pts',(16.0610045650479,-0.860864647255521,
26.0058959623481));
#41478=CARTESIAN_POINT('Ctrl Pts',(16.0716137679462,-0.778552160147466,
25.8624850513267));
#41479=CARTESIAN_POINT('Ctrl Pts',(16.0822229708444,-0.659624910645523,
25.7400896413997));
#41480=CARTESIAN_POINT('Ctrl Pts',(16.0928321737427,-0.518638640984628,
25.6536899498435));
#41481=CARTESIAN_POINT('Ctrl Pts',(16.103441376641,-0.377652371323737,25.5672902582873));
#41482=CARTESIAN_POINT('Ctrl Pts',(16.1140505795393,-0.214607081503895,
25.516886285102));
#41483=CARTESIAN_POINT('Ctrl Pts',(16.1246597824375,-0.049458208325129,
25.508647072659));
#41484=CARTESIAN_POINT('Ctrl Pts',(16.1352689853358,0.115690664853637,25.500407860216));
#41485=CARTESIAN_POINT('Ctrl Pts',(16.1458781882341,0.282943121391326,25.5343334085154));
#41486=CARTESIAN_POINT('Ctrl Pts',(16.1564873911323,0.431828800998626,25.6062715023306));
#41487=CARTESIAN_POINT('Ctrl Pts',(16.1670965940306,0.580714480605926,25.6782095961459));
#41488=CARTESIAN_POINT('Ctrl Pts',(16.1777057969289,0.711233383282836,25.788160235477));
#41489=CARTESIAN_POINT('Ctrl Pts',(16.1883149998272,0.807411041343378,25.9226663432338));
#41490=CARTESIAN_POINT('Ctrl Pts',(16.1989242027255,0.90358869940392,26.0571724509906));
#41491=CARTESIAN_POINT('Ctrl Pts',(16.2095334056237,0.965425112848094,26.2162340271731));
#41492=CARTESIAN_POINT('Ctrl Pts',(16.220142608522,0.985352000238336,26.3803832096043));
#41493=CARTESIAN_POINT('Ctrl Pts',(16.2307518114202,1.00527888762858,26.5445323920355));
#41494=CARTESIAN_POINT('Ctrl Pts',(16.2413610143185,0.983296248964886,26.7137691807154));
#41495=CARTESIAN_POINT('Ctrl Pts',(16.2519702172168,0.922094583046927,26.8673803490033));
#41496=CARTESIAN_POINT('Ctrl Pts',(16.2625794201151,0.860892917128968,27.0209915172911));
#41497=CARTESIAN_POINT('Ctrl Pts',(16.2731886230133,0.760472223956742,27.158977065187));
#41498=CARTESIAN_POINT('Ctrl Pts',(16.2837978259116,0.633123191585252,27.264448667469));
#41499=CARTESIAN_POINT('Ctrl Pts',(16.2944070288099,0.505774159213761,27.369920269751));
#41500=CARTESIAN_POINT('Ctrl Pts',(16.3050162317082,0.351496787643007,27.4428779264193));
#41501=CARTESIAN_POINT('Ctrl Pts',(16.3156254346064,0.189173390746985,27.4743922049932));
#41502=CARTESIAN_POINT('Ctrl Pts',(16.3262346375047,0.0268499938509623,
27.5059064835671));
#41503=CARTESIAN_POINT('Ctrl Pts',(16.336843840403,-0.143519428370328,27.4959773840466));
#41504=CARTESIAN_POINT('Ctrl Pts',(16.3474530433012,-0.301083024007819,
27.4458201486396));
#41505=CARTESIAN_POINT('Ctrl Pts',(16.3580622461995,-0.458646619645319,
27.3956629132325));
#41506=CARTESIAN_POINT('Ctrl Pts',(16.3686714490978,-0.603404388699017,
27.3052775419388));
#41507=CARTESIAN_POINT('Ctrl Pts',(16.3792806519961,-0.717639140351219,
27.1857264798403));
#41508=CARTESIAN_POINT('Ctrl Pts',(16.3898898548944,-0.831873892003415,
27.0661754177419));
#41509=CARTESIAN_POINT('Ctrl Pts',(16.4004990577926,-0.915585626254117,
26.9174586648388));
#41510=CARTESIAN_POINT('Ctrl Pts',(16.4111082606909,-0.95852869771175,26.7577779598439));
#41511=CARTESIAN_POINT('Ctrl Pts',(16.4166832479152,-0.981094679062509,
26.6738679904662));
#41512=CARTESIAN_POINT('Ctrl Pts',(16.4222582351395,-0.992402985346778,
26.5869304847006));
#41513=CARTESIAN_POINT('Ctrl Pts',(16.4278332223638,-0.992414999655005,
26.4999960454856));
#41514=CARTESIAN_POINT('Origin',(18.,0.,26.5));
#41515=CARTESIAN_POINT('',(16.9721667776362,-0.993608664717065,26.5006377171609));
#41516=CARTESIAN_POINT('',(16.8278332223638,-0.992566518425997,26.500015300021));
#41517=CARTESIAN_POINT('',(18.,-0.9925,26.5));
#41518=CARTESIAN_POINT('Ctrl Pts',(16.9721667776362,-0.993608664717065,
26.5006377171609));
#41519=CARTESIAN_POINT('Ctrl Pts',(16.9714156227976,-0.99360792305922,26.5123412234469));
#41520=CARTESIAN_POINT('Ctrl Pts',(16.970664467959,-0.993388337675886,26.5240391525227));
#41521=CARTESIAN_POINT('Ctrl Pts',(16.9699133131204,-0.992947148238254,
26.5357235520371));
#41522=CARTESIAN_POINT('Ctrl Pts',(16.9487422421193,-0.98051235792753,26.8650448038074));
#41523=CARTESIAN_POINT('Ctrl Pts',(16.9275711711183,-0.792040380383265,
27.1836184818102));
#41524=CARTESIAN_POINT('Ctrl Pts',(16.9064001001172,-0.509390844161436,
27.3530774755247));
#41525=CARTESIAN_POINT('Ctrl Pts',(16.8958145646167,-0.36806607605052,27.4378069723819));
#41526=CARTESIAN_POINT('Ctrl Pts',(16.8852290291161,-0.203196918270212,
27.4852577981671));
#41527=CARTESIAN_POINT('Ctrl Pts',(16.8746434936156,-0.0380092888994282,
27.4914850905056));
#41528=CARTESIAN_POINT('Ctrl Pts',(16.8640579581151,0.127178340471351,27.4977123828441));
#41529=CARTESIAN_POINT('Ctrl Pts',(16.8534724226145,0.292684441432607,27.462716141736));
#41530=CARTESIAN_POINT('Ctrl Pts',(16.842886887114,0.44030145421419,27.3896112159135));
#41531=CARTESIAN_POINT('Ctrl Pts',(16.8323013516135,0.587918466995774,27.316506290091));
#41532=CARTESIAN_POINT('Ctrl Pts',(16.8217158161129,0.717646391597684,27.205292679554));
#41533=CARTESIAN_POINT('Ctrl Pts',(16.8111302806124,0.812561361623588,27.0701849752009));
#41534=CARTESIAN_POINT('Ctrl Pts',(16.8005447451119,0.907476331649495,26.9350772708479));
#41535=CARTESIAN_POINT('Ctrl Pts',(16.7899592096113,0.967578347099393,26.7760754726787));
#41536=CARTESIAN_POINT('Ctrl Pts',(16.7793736741108,0.986150395205684,26.6121792342922));
#41537=CARTESIAN_POINT('Ctrl Pts',(16.7687881386103,1.00472244331198,26.4482829959057));
#41538=CARTESIAN_POINT('Ctrl Pts',(16.7582026031097,0.981764524074659,26.279492317302));
#41539=CARTESIAN_POINT('Ctrl Pts',(16.7476170676092,0.919738931278878,26.1266126776718));
#41540=CARTESIAN_POINT('Ctrl Pts',(16.7370315321087,0.857713338483099,25.9737330380415));
#41541=CARTESIAN_POINT('Ctrl Pts',(16.7264459966081,0.756620072128858,25.8367644373847));
#41542=CARTESIAN_POINT('Ctrl Pts',(16.7158604611076,0.628979934428365,25.7322017075267));
#41543=CARTESIAN_POINT('Ctrl Pts',(16.7052749256071,0.501339796727873,25.6276389776688));
#41544=CARTESIAN_POINT('Ctrl Pts',(16.6946893901066,0.347152787681117,25.5554821186096));
#41545=CARTESIAN_POINT('Ctrl Pts',(16.684103854606,0.185055486963601,25.5247604084482));
#41546=CARTESIAN_POINT('Ctrl Pts',(16.6735183191055,0.0229581862460808,
25.4940386982867));
#41547=CARTESIAN_POINT('Ctrl Pts',(16.662932783605,-0.14704940614221,25.504752137023));
#41548=CARTESIAN_POINT('Ctrl Pts',(16.6523472481044,-0.304084154022982,
25.5552198087159));
#41549=CARTESIAN_POINT('Ctrl Pts',(16.6417617126039,-0.461118901903754,
25.6056874804089));
#41550=CARTESIAN_POINT('Ctrl Pts',(16.6311761771033,-0.605180805276994,
25.6959093850586));
#41551=CARTESIAN_POINT('Ctrl Pts',(16.6205906416028,-0.718963948417315,
25.8155602924839));
#41552=CARTESIAN_POINT('Ctrl Pts',(16.6100051061023,-0.832747091557636,
25.9352111999092));
#41553=CARTESIAN_POINT('Ctrl Pts',(16.5994195706018,-0.916251474465024,
26.0842911101102));
#41554=CARTESIAN_POINT('Ctrl Pts',(16.5888340351012,-0.958871608097665,
26.243409420971));
#41555=CARTESIAN_POINT('Ctrl Pts',(16.5832782826129,-0.98124052022978,26.3269216770548));
#41556=CARTESIAN_POINT('Ctrl Pts',(16.5777225301246,-0.992347416349173,
26.4131991209793));
#41557=CARTESIAN_POINT('Ctrl Pts',(16.5721667776362,-0.992268890272332,
26.499572269901));
#41558=CARTESIAN_POINT('Ctrl Pts',(16.4278332223638,-0.992414999655005,
26.4999960454856));
#41559=CARTESIAN_POINT('Ctrl Pts',(16.4328674380378,-0.992425848580097,
26.4214942124059));
#41560=CARTESIAN_POINT('Ctrl Pts',(16.4379016537117,-0.983225591272503,
26.3429948798214));
#41561=CARTESIAN_POINT('Ctrl Pts',(16.4429358693857,-0.964785793511,26.2667295270344));
#41562=CARTESIAN_POINT('Ctrl Pts',(16.453545072284,-0.925925409188051,26.1060064563066));
#41563=CARTESIAN_POINT('Ctrl Pts',(16.4641542751823,-0.846030231877589,
25.9552049719378));
#41564=CARTESIAN_POINT('Ctrl Pts',(16.4747634780805,-0.734878790988267,
25.8327819670648));
#41565=CARTESIAN_POINT('Ctrl Pts',(16.4853726809788,-0.62372735009895,25.7103589621919));
#41566=CARTESIAN_POINT('Ctrl Pts',(16.4959818838771,-0.481319645630766,
25.6163144368148));
#41567=CARTESIAN_POINT('Ctrl Pts',(16.5065910867753,-0.325085239329991,
25.5621586871501));
#41568=CARTESIAN_POINT('Ctrl Pts',(16.5172002896736,-0.168850833029208,
25.5080029374855));
#41569=CARTESIAN_POINT('Ctrl Pts',(16.5278094925719,0.00121027510417573,
25.4937359635333));
#41570=CARTESIAN_POINT('Ctrl Pts',(16.5384186954702,0.164283968334559,25.5211039285672));
#41571=CARTESIAN_POINT('Ctrl Pts',(16.5490278983684,0.327357661564934,25.5484718936012));
#41572=CARTESIAN_POINT('Ctrl Pts',(16.5596371012667,0.483443939892306,25.6174747976213));
#41573=CARTESIAN_POINT('Ctrl Pts',(16.570246304165,0.613439093752594,25.719667238177));
#41574=CARTESIAN_POINT('Ctrl Pts',(16.5808555070633,0.743434247612885,25.8218596787328));
#41575=CARTESIAN_POINT('Ctrl Pts',(16.5914647099615,0.847338277006087,25.9572416558241));
#41576=CARTESIAN_POINT('Ctrl Pts',(16.6020739128598,0.912434161439791,26.1092435004303));
#41577=CARTESIAN_POINT('Ctrl Pts',(16.6126831157581,0.977530045873495,26.2612453450365));
#41578=CARTESIAN_POINT('Ctrl Pts',(16.6232923186563,1.0038177853477,26.4298670571576));
#41579=CARTESIAN_POINT('Ctrl Pts',(16.6339015215546,0.988079971225441,26.5944706905942));
#41580=CARTESIAN_POINT('Ctrl Pts',(16.6445107244529,0.972342157103183,26.7590743240309));
#41581=CARTESIAN_POINT('Ctrl Pts',(16.6551199273512,0.914578789384463,26.9196598787832));
#41582=CARTESIAN_POINT('Ctrl Pts',(16.6657291302494,0.821859641352038,27.0565729699105));
#41583=CARTESIAN_POINT('Ctrl Pts',(16.6763383331477,0.729140493319612,27.1934860610379));
#41584=CARTESIAN_POINT('Ctrl Pts',(16.686947536046,0.601465564973483,27.3067266885402));
#41585=CARTESIAN_POINT('Ctrl Pts',(16.6975567389442,0.454461244333888,27.382435107142));
#41586=CARTESIAN_POINT('Ctrl Pts',(16.7081659418425,0.307456923694284,27.4581435257437));
#41587=CARTESIAN_POINT('Ctrl Pts',(16.7187751447408,0.141123210761213,27.4963197354449));
#41588=CARTESIAN_POINT('Ctrl Pts',(16.7293843476391,-0.0241819810306813,
27.4922912741286));
#41589=CARTESIAN_POINT('Ctrl Pts',(16.7399935505373,-0.189487172822562,
27.4882628128124));
#41590=CARTESIAN_POINT('Ctrl Pts',(16.7506027534356,-0.353763843473277,
27.4420296804787));
#41591=CARTESIAN_POINT('Ctrl Pts',(16.7612119563339,-0.496905845036753,
27.3592504420054));
#41592=CARTESIAN_POINT('Ctrl Pts',(16.7718211592322,-0.640047846600237,
27.2764712035321));
#41593=CARTESIAN_POINT('Ctrl Pts',(16.7824303621304,-0.762055179076489,
27.1571458589192));
#41594=CARTESIAN_POINT('Ctrl Pts',(16.7930395650287,-0.847995122760424,
27.0158788740514));
#41595=CARTESIAN_POINT('Ctrl Pts',(16.803648767927,-0.933935066444353,26.8746118891835));
#41596=CARTESIAN_POINT('Ctrl Pts',(16.8142579708253,-0.983807621335963,
26.7114032640608));
#41597=CARTESIAN_POINT('Ctrl Pts',(16.8248671737235,-0.99150878640109,26.546228426418));
#41598=CARTESIAN_POINT('Ctrl Pts',(16.8258558566036,-0.992226466148543,
26.5308356079597));
#41599=CARTESIAN_POINT('Ctrl Pts',(16.8268445394837,-0.992577905342496,
26.5154257137833));
#41600=CARTESIAN_POINT('Ctrl Pts',(16.8278332223638,-0.992566518425997,
26.500015300021));
#41601=CARTESIAN_POINT('Origin',(18.,0.,26.5));
#41602=CARTESIAN_POINT('',(17.3721667776362,-0.991136349068622,26.5001921337659));
#41603=CARTESIAN_POINT('',(17.2278332223638,-0.99244811917863,26.4999785467739));
#41604=CARTESIAN_POINT('',(18.,-0.9925,26.5));
#41605=CARTESIAN_POINT('Ctrl Pts',(17.3721667776362,-0.991136349068622,
26.5001921337659));
#41606=CARTESIAN_POINT('Ctrl Pts',(17.3651087154707,-0.991892155534025,
26.6100961603842));
#41607=CARTESIAN_POINT('Ctrl Pts',(17.3580506533051,-0.974948391853953,
26.7199509551589));
#41608=CARTESIAN_POINT('Ctrl Pts',(17.3509925911395,-0.939319387565507,
26.8238816182409));
#41609=CARTESIAN_POINT('Ctrl Pts',(17.340407055639,-0.885883744623132,26.9797546748733));
#41610=CARTESIAN_POINT('Ctrl Pts',(17.3298215201385,-0.790418681165517,
27.1223023573604));
#41611=CARTESIAN_POINT('Ctrl Pts',(17.319235984638,-0.668138790300684,27.2335379649631));
#41612=CARTESIAN_POINT('Ctrl Pts',(17.3086504491374,-0.545858899435857,
27.3447735725658));
#41613=CARTESIAN_POINT('Ctrl Pts',(17.2980649136369,-0.396764181163814,
27.4246971052841));
#41614=CARTESIAN_POINT('Ctrl Pts',(17.2874793781363,-0.236782908219976,
27.4639540139289));
#41615=CARTESIAN_POINT('Ctrl Pts',(17.2768938426358,-0.0768016352761392,
27.5032109225737));
#41616=CARTESIAN_POINT('Ctrl Pts',(17.2663083071353,0.0940661923394922,
27.5018012071451));
#41617=CARTESIAN_POINT('Ctrl Pts',(17.2557227716348,0.253719211720844,27.4596840281348));
#41618=CARTESIAN_POINT('Ctrl Pts',(17.2451372361342,0.413372231102205,27.4175668491245));
#41619=CARTESIAN_POINT('Ctrl Pts',(17.2345517006337,0.561810442249285,27.3347422065326));
#41620=CARTESIAN_POINT('Ctrl Pts',(17.2239661651331,0.68165181448249,27.2214066719458));
#41621=CARTESIAN_POINT('Ctrl Pts',(17.2133806296326,0.801493186715687,27.1080711373589));
#41622=CARTESIAN_POINT('Ctrl Pts',(17.2027950941321,0.892737720035012,26.9642247107773));
#41623=CARTESIAN_POINT('Ctrl Pts',(17.1922095586316,0.943857422910035,26.807361284942));
#41624=CARTESIAN_POINT('Ctrl Pts',(17.181624023131,0.994977125785058,26.6504978591067));
#41625=CARTESIAN_POINT('Ctrl Pts',(17.1710384876305,1.00597199821578,26.4806174340177));
#41626=CARTESIAN_POINT('Ctrl Pts',(17.16045295213,0.975782759799013,26.3184015929024));
#41627=CARTESIAN_POINT('Ctrl Pts',(17.1498674166294,0.945593521382245,26.156185751787));
#41628=CARTESIAN_POINT('Ctrl Pts',(17.1392818811289,0.874220172117985,26.0016344946453));
#41629=CARTESIAN_POINT('Ctrl Pts',(17.1286963456284,0.770091285950915,25.8736636642194));
#41630=CARTESIAN_POINT('Ctrl Pts',(17.1181108101278,0.66596239978385,25.7456928337934));
#41631=CARTESIAN_POINT('Ctrl Pts',(17.1075252746273,0.529077976713979,25.6443024300833));
#41632=CARTESIAN_POINT('Ctrl Pts',(17.0969397391268,0.376487631167103,25.5816678998663));
#41633=CARTESIAN_POINT('Ctrl Pts',(17.0863542036262,0.223897285620227,25.5190333696494));
#41634=CARTESIAN_POINT('Ctrl Pts',(17.0757686681257,0.0556010175963462,
25.4951547129257));
#41635=CARTESIAN_POINT('Ctrl Pts',(17.0651831326252,-0.108514671340715,
25.5132926277484));
#41636=CARTESIAN_POINT('Ctrl Pts',(17.0545975971246,-0.272630360277776,
25.5314305425711));
#41637=CARTESIAN_POINT('Ctrl Pts',(17.0440120616241,-0.432565470128018,
25.5915850289401));
#41638=CARTESIAN_POINT('Ctrl Pts',(17.0334265261236,-0.567713051738021,
25.6857670008228));
#41639=CARTESIAN_POINT('Ctrl Pts',(17.022840990623,-0.702860633348025,25.7799489727055));
#41640=CARTESIAN_POINT('Ctrl Pts',(17.0122554551225,-0.813220686717791,
25.9081584301017));
#41641=CARTESIAN_POINT('Ctrl Pts',(17.001669919622,-0.887296664229188,26.0559369184634));
#41642=CARTESIAN_POINT('Ctrl Pts',(16.9918355389601,-0.956116173711191,
26.1932289721453));
#41643=CARTESIAN_POINT('Ctrl Pts',(16.9820011582981,-0.993618374759788,
26.347411338285));
#41644=CARTESIAN_POINT('Ctrl Pts',(16.9721667776362,-0.993608664717065,
26.5006377171609));
#41645=CARTESIAN_POINT('Ctrl Pts',(16.8278332223638,-0.992566518425997,
26.500015300021));
#41646=CARTESIAN_POINT('Ctrl Pts',(16.837453742382,-0.992455716408151,26.3500620672179));
#41647=CARTESIAN_POINT('Ctrl Pts',(16.8470742624002,-0.957990575121126,
26.2000596372117));
#41648=CARTESIAN_POINT('Ctrl Pts',(16.8566947824183,-0.892316991382856,
26.065262000966));
#41649=CARTESIAN_POINT('Ctrl Pts',(16.8673039853166,-0.819894256060864,
25.9166114633197));
#41650=CARTESIAN_POINT('Ctrl Pts',(16.8779131882149,-0.709519010178247,
25.7864514381899));
#41651=CARTESIAN_POINT('Ctrl Pts',(16.8885223911132,-0.57470029925367,25.690712469537));
#41652=CARTESIAN_POINT('Ctrl Pts',(16.8991315940114,-0.439881588329094,
25.594973500884));
#41653=CARTESIAN_POINT('Ctrl Pts',(16.9097407969097,-0.280619412362559,
25.5336555887078));
#41654=CARTESIAN_POINT('Ctrl Pts',(16.920349999808,-0.11640618535689,25.5142635540274));
#41655=CARTESIAN_POINT('Ctrl Pts',(16.9309592027062,0.0478070416487797,
25.4948715193471));
#41656=CARTESIAN_POINT('Ctrl Pts',(16.9415684056045,0.216971319693583,25.5174053621625));
#41657=CARTESIAN_POINT('Ctrl Pts',(16.9521776085028,0.370382296894979,25.5791071207387));
#41658=CARTESIAN_POINT('Ctrl Pts',(16.9627868114011,0.523793274096375,25.6408088793148));
#41659=CARTESIAN_POINT('Ctrl Pts',(16.9733960142993,0.661450950454363,25.7416785536516));
#41660=CARTESIAN_POINT('Ctrl Pts',(16.9840052171976,0.766507129524873,25.8693705039312));
#41661=CARTESIAN_POINT('Ctrl Pts',(16.9946144200959,0.871563308595388,25.9970624542109));
#41662=CARTESIAN_POINT('Ctrl Pts',(17.0052236229942,0.944017990378417,26.1515766804334));
#41663=CARTESIAN_POINT('Ctrl Pts',(17.0158328258924,0.975003302622344,26.314001879739));
#41664=CARTESIAN_POINT('Ctrl Pts',(17.0264420287907,1.00598861486627,26.4764270790447));
#41665=CARTESIAN_POINT('Ctrl Pts',(17.037051231689,0.995504557571091,26.6467632514335));
#41666=CARTESIAN_POINT('Ctrl Pts',(17.0476604345872,0.94483429507576,26.8041626142725));
#41667=CARTESIAN_POINT('Ctrl Pts',(17.0582696374855,0.894164032580429,26.9615619771116));
#41668=CARTESIAN_POINT('Ctrl Pts',(17.0688788403838,0.803307564884947,27.106024530401));
#41669=CARTESIAN_POINT('Ctrl Pts',(17.0794880432821,0.683384995972857,27.2198692158136));
#41670=CARTESIAN_POINT('Ctrl Pts',(17.0900972461803,0.563462427060767,27.3337139012263));
#41671=CARTESIAN_POINT('Ctrl Pts',(17.1007064490786,0.414473756932069,27.4169407187623));
#41672=CARTESIAN_POINT('Ctrl Pts',(17.1113156519769,0.254654003887244,27.4593633721055));
#41673=CARTESIAN_POINT('Ctrl Pts',(17.1219248548751,0.0948342508424191,
27.5017860254488));
#41674=CARTESIAN_POINT('Ctrl Pts',(17.1325340577734,-0.0758165851185327,
27.5034045145994));
#41675=CARTESIAN_POINT('Ctrl Pts',(17.1431432606717,-0.236412207597704,
27.4640207510499));
#41676=CARTESIAN_POINT('Ctrl Pts',(17.15375246357,-0.397007830076871,27.4246369875004));
#41677=CARTESIAN_POINT('Ctrl Pts',(17.1643616664682,-0.547548239074259,
27.3442509712509));
#41678=CARTESIAN_POINT('Ctrl Pts',(17.1749708693665,-0.669608498200657,
27.232701303453));
#41679=CARTESIAN_POINT('Ctrl Pts',(17.1855800722648,-0.791668757327062,
27.1211516356551));
#41680=CARTESIAN_POINT('Ctrl Pts',(17.196189275163,-0.885248866582474,26.978438316309));
#41681=CARTESIAN_POINT('Ctrl Pts',(17.2067984780613,-0.938895364492047,
26.8220283176548));
#41682=CARTESIAN_POINT('Ctrl Pts',(17.2138100594955,-0.974350128846863,
26.7186575504825));
#41683=CARTESIAN_POINT('Ctrl Pts',(17.2208216409296,-0.992362541423131,
26.6093042966119));
#41684=CARTESIAN_POINT('Ctrl Pts',(17.2278332223638,-0.99244811917863,26.4999785467739));
#41685=CARTESIAN_POINT('Origin',(18.,0.,26.5));
#41686=CARTESIAN_POINT('',(17.7721667776362,-0.992388106880432,26.5001388685385));
#41687=CARTESIAN_POINT('',(17.6278332223638,-0.992500513774779,26.5000263957801));
#41688=CARTESIAN_POINT('',(18.,-0.9925,26.5));
#41689=CARTESIAN_POINT('Ctrl Pts',(17.7721667776362,-0.992388106880432,
26.5001388685385));
#41690=CARTESIAN_POINT('Ctrl Pts',(17.7693873436442,-0.992277927963132,
26.5436557685285));
#41691=CARTESIAN_POINT('Ctrl Pts',(17.7666079096523,-0.989362052989495,
26.5871401972748));
#41692=CARTESIAN_POINT('Ctrl Pts',(17.7638284756603,-0.983640977958964,
26.6301655848495));
#41693=CARTESIAN_POINT('Ctrl Pts',(17.7532429401598,-0.961852137852761,
26.7940287199015));
#41694=CARTESIAN_POINT('Ctrl Pts',(17.7426574046592,-0.899374320287603,
26.9512335362917));
#41695=CARTESIAN_POINT('Ctrl Pts',(17.7320718691587,-0.802363869957874,
27.0843655363258));
#41696=CARTESIAN_POINT('Ctrl Pts',(17.7214863336582,-0.705353419628139,
27.2174975363598));
#41697=CARTESIAN_POINT('Ctrl Pts',(17.7109007981576,-0.573810336533829,
27.3265567200377));
#41698=CARTESIAN_POINT('Ctrl Pts',(17.7003152626571,-0.424601154204597,
27.3972635217341));
#41699=CARTESIAN_POINT('Ctrl Pts',(17.6897297271566,-0.275391971875373,
27.4679703234305));
#41700=CARTESIAN_POINT('Ctrl Pts',(17.679144191656,-0.108516690311227,27.5003247431453));
#41701=CARTESIAN_POINT('Ctrl Pts',(17.6685586561555,0.0561603902068333,
27.4909200220565));
#41702=CARTESIAN_POINT('Ctrl Pts',(17.657973120655,0.220837470724894,27.4815153009676));
#41703=CARTESIAN_POINT('Ctrl Pts',(17.6473875851544,0.383316350196873,27.4303514390751));
#41704=CARTESIAN_POINT('Ctrl Pts',(17.6368020496539,0.523508687926737,27.3433720559961));
#41705=CARTESIAN_POINT('Ctrl Pts',(17.6262165141534,0.663701025656609,27.2563926729171));
#41706=CARTESIAN_POINT('Ctrl Pts',(17.6156309786528,0.781606821644367,27.1335977686517));
#41707=CARTESIAN_POINT('Ctrl Pts',(17.6050454431523,0.863084818137216,26.9901170051206));
#41708=CARTESIAN_POINT('Ctrl Pts',(17.5944599076518,0.944562814630061,26.8466362415895));
#41709=CARTESIAN_POINT('Ctrl Pts',(17.5838743721513,0.989613011628003,26.6824696187928));
#41710=CARTESIAN_POINT('Ctrl Pts',(17.5732888366507,0.992487299462635,26.5175117774126));
#41711=CARTESIAN_POINT('Ctrl Pts',(17.5627033011502,0.995361587297268,26.3525539360324));
#41712=CARTESIAN_POINT('Ctrl Pts',(17.5521177656496,0.956059965968592,26.1868048760686));
#41713=CARTESIAN_POINT('Ctrl Pts',(17.5415322301491,0.879769581345556,26.0405630378266));
#41714=CARTESIAN_POINT('Ctrl Pts',(17.5309466946486,0.803479196722518,25.8943211995846));
#41715=CARTESIAN_POINT('Ctrl Pts',(17.5203611591481,0.690200048805118,25.7675865830643));
#41716=CARTESIAN_POINT('Ctrl Pts',(17.5097756236475,0.553034680142503,25.6756702789943));
#41717=CARTESIAN_POINT('Ctrl Pts',(17.499190088147,0.415869311479896,25.5837539749243));
#41718=CARTESIAN_POINT('Ctrl Pts',(17.4886045526465,0.254817722072074,25.5266559833047));
#41719=CARTESIAN_POINT('Ctrl Pts',(17.4780190171459,0.0907843533403148,
25.5115508634293));
#41720=CARTESIAN_POINT('Ctrl Pts',(17.4674334816454,-0.0732490153914441,
25.4964457435539));
#41721=CARTESIAN_POINT('Ctrl Pts',(17.4568479461449,-0.240264163447142,
25.5233334954228));
#41722=CARTESIAN_POINT('Ctrl Pts',(17.4462624106443,-0.392151958435379,
25.5885702267216));
#41723=CARTESIAN_POINT('Ctrl Pts',(17.4356768751438,-0.544039753423623,
25.6538069580204));
#41724=CARTESIAN_POINT('Ctrl Pts',(17.4250913396433,-0.680800195344407,
25.7573926687492));
#41725=CARTESIAN_POINT('Ctrl Pts',(17.4145058041427,-0.782181555987627,
25.8872910775428));
#41726=CARTESIAN_POINT('Ctrl Pts',(17.4003927953072,-0.917346757449673,
26.0604762121946));
#41727=CARTESIAN_POINT('Ctrl Pts',(17.3862797864717,-0.989625069757963,
26.2804325932095));
#41728=CARTESIAN_POINT('Ctrl Pts',(17.3721667776362,-0.991136349068622,
26.5001921337659));
#41729=CARTESIAN_POINT('Ctrl Pts',(17.2278332223638,-0.99244811917863,26.4999785467739));
#41730=CARTESIAN_POINT('Ctrl Pts',(17.2314308438279,-0.992492028869037,
26.443883831496));
#41731=CARTESIAN_POINT('Ctrl Pts',(17.235028465292,-0.987816366912872,26.3877963571647));
#41732=CARTESIAN_POINT('Ctrl Pts',(17.2386260867561,-0.978355688226005,
26.3325279671566));
#41733=CARTESIAN_POINT('Ctrl Pts',(17.2492352896544,-0.95045662748666,26.1695442932747));
#41734=CARTESIAN_POINT('Ctrl Pts',(17.2598444925527,-0.880945619444235,
26.0136836234732));
#41735=CARTESIAN_POINT('Ctrl Pts',(17.270453695451,-0.778330232769517,25.8840220748992));
#41736=CARTESIAN_POINT('Ctrl Pts',(17.2810628983492,-0.675714846094799,
25.7543605263252));
#41737=CARTESIAN_POINT('Ctrl Pts',(17.2916721012475,-0.539995080787785,
25.6508980989787));
#41738=CARTESIAN_POINT('Ctrl Pts',(17.3022813041458,-0.387781989300544,
25.5862977265485));
#41739=CARTESIAN_POINT('Ctrl Pts',(17.312890507044,-0.235568897813299,25.5216973541183));
#41740=CARTESIAN_POINT('Ctrl Pts',(17.3234997099423,-0.0668624801458348,
25.4959590366045));
#41741=CARTESIAN_POINT('Ctrl Pts',(17.3341089128406,0.0976890273760728,
25.5122330100268));
#41742=CARTESIAN_POINT('Ctrl Pts',(17.3447181157389,0.262240534897985,25.5285069834492));
#41743=CARTESIAN_POINT('Ctrl Pts',(17.3553273186371,0.42263713227433,25.5867932478078));
#41744=CARTESIAN_POINT('Ctrl Pts',(17.3659365215354,0.559247415751573,25.6799578950811));
#41745=CARTESIAN_POINT('Ctrl Pts',(17.3765457244337,0.695857699228807,25.7731225423545));
#41746=CARTESIAN_POINT('Ctrl Pts',(17.387154927332,0.808681668806945,25.9011655725426));
#41747=CARTESIAN_POINT('Ctrl Pts',(17.3977641302302,0.883910849877243,26.0484158024241));
#41748=CARTESIAN_POINT('Ctrl Pts',(17.4083733331285,0.959140030947542,26.1956660323055));
#41749=CARTESIAN_POINT('Ctrl Pts',(17.4189825360268,0.996774423510004,26.3621234618803));
#41750=CARTESIAN_POINT('Ctrl Pts',(17.429591738925,0.992207360123716,26.5274145495491));
#41751=CARTESIAN_POINT('Ctrl Pts',(17.4402009418233,0.987640296737429,26.6927056372179));
#41752=CARTESIAN_POINT('Ctrl Pts',(17.4508101447216,0.940871777402391,26.8568303829806));
#41753=CARTESIAN_POINT('Ctrl Pts',(17.4614193476199,0.857626874806772,26.9997021513987));
#41754=CARTESIAN_POINT('Ctrl Pts',(17.4720285505181,0.774381972211152,27.1425739198167));
#41755=CARTESIAN_POINT('Ctrl Pts',(17.4826377534164,0.654660686354949,27.2641927108899));
#41756=CARTESIAN_POINT('Ctrl Pts',(17.4932469563147,0.513114091336382,27.3496716256727));
#41757=CARTESIAN_POINT('Ctrl Pts',(17.503856159213,0.371567496317814,27.4351505404554));
#41758=CARTESIAN_POINT('Ctrl Pts',(17.5144653621112,0.20819559213688,27.4844895789476));
#41759=CARTESIAN_POINT('Ctrl Pts',(17.5250745650095,0.0429972871920246,
27.4916533116257));
#41760=CARTESIAN_POINT('Ctrl Pts',(17.5356837679078,-0.122201017752836,
27.4988170443038));
#41761=CARTESIAN_POINT('Ctrl Pts',(17.546292970806,-0.289225723461607,27.4638054711678));
#41762=CARTESIAN_POINT('Ctrl Pts',(17.5569021737043,-0.437640946846334,
27.3908975473816));
#41763=CARTESIAN_POINT('Ctrl Pts',(17.5675113766026,-0.586056170231056,
27.3179896235954));
#41764=CARTESIAN_POINT('Ctrl Pts',(17.5781205795009,-0.715861911291723,
27.2071853491589));
#41765=CARTESIAN_POINT('Ctrl Pts',(17.5887297823991,-0.811158521085179,
27.0720579498581));
#41766=CARTESIAN_POINT('Ctrl Pts',(17.5993389852974,-0.906455130878635,
26.9369305505572));
#41767=CARTESIAN_POINT('Ctrl Pts',(17.6099481881957,-0.967242609404881,
26.7774800263921));
#41768=CARTESIAN_POINT('Ctrl Pts',(17.6205573910939,-0.986104595712793,
26.6131998072346));
#41769=CARTESIAN_POINT('Ctrl Pts',(17.6229826681839,-0.990416469441883,
26.5756451430741));
#41770=CARTESIAN_POINT('Ctrl Pts',(17.6254079452739,-0.992537378432218,
26.5378380861361));
#41771=CARTESIAN_POINT('Ctrl Pts',(17.6278332223638,-0.992500513774779,
26.5000263957801));
#41772=CARTESIAN_POINT('Origin',(18.,0.,26.5));
#41773=CARTESIAN_POINT('',(18.1721667776362,-0.993299106214555,26.5003419800918));
#41774=CARTESIAN_POINT('',(18.0278332223638,-0.992167930500117,26.4998747777436));
#41775=CARTESIAN_POINT('',(18.,-0.9925,26.5));
#41776=CARTESIAN_POINT('Ctrl Pts',(18.1721667776362,-0.993299106214555,
26.5003419800918));
#41777=CARTESIAN_POINT('Ctrl Pts',(18.1524949008168,-0.991326401614957,
26.8062082540558));
#41778=CARTESIAN_POINT('Ctrl Pts',(18.1328230239973,-0.841330030363234,
27.1099769695095));
#41779=CARTESIAN_POINT('Ctrl Pts',(18.1131511471779,-0.596827584575755,
27.2943640520012));
#41780=CARTESIAN_POINT('Ctrl Pts',(18.1025656116773,-0.465259593193731,
27.3935836651306));
#41781=CARTESIAN_POINT('Ctrl Pts',(18.0919800761768,-0.306326706074318,
27.4582354903689));
#41782=CARTESIAN_POINT('Ctrl Pts',(18.0813945406763,-0.142734068023168,
27.4819016698871));
#41783=CARTESIAN_POINT('Ctrl Pts',(18.0708090051757,0.020858570027974,27.5055678494052));
#41784=CARTESIAN_POINT('Ctrl Pts',(18.0602234696752,0.189110959010848,27.4882483832032));
#41785=CARTESIAN_POINT('Ctrl Pts',(18.0496379341747,0.343650673209678,27.4311978245028));
#41786=CARTESIAN_POINT('Ctrl Pts',(18.0390523986741,0.498190387408508,27.3741472658025));
#41787=CARTESIAN_POINT('Ctrl Pts',(18.0284668631736,0.639017426823289,27.2773656146038));
#41788=CARTESIAN_POINT('Ctrl Pts',(18.0178813276731,0.747674083450534,27.153028467699));
#41789=CARTESIAN_POINT('Ctrl Pts',(18.0072957921725,0.856330740077779,27.0286913207943));
#41790=CARTESIAN_POINT('Ctrl Pts',(17.996710256672,0.932817013917483,26.8767986781835));
#41791=CARTESIAN_POINT('Ctrl Pts',(17.9861247211715,0.968680791357801,26.7158540046014));
#41792=CARTESIAN_POINT('Ctrl Pts',(17.9755391856709,1.00454456879812,26.5549093310193));
#41793=CARTESIAN_POINT('Ctrl Pts',(17.9649536501704,0.999785849839044,26.3849126264658));
#41794=CARTESIAN_POINT('Ctrl Pts',(17.9543681146699,0.954200819239477,26.2262053483874));
#41795=CARTESIAN_POINT('Ctrl Pts',(17.9437825791693,0.908615788639911,26.067498070309));
#41796=CARTESIAN_POINT('Ctrl Pts',(17.9331970436688,0.822204446399863,25.9200802187056));
#41797=CARTESIAN_POINT('Ctrl Pts',(17.9226115081683,0.706508638419301,25.8028122796583));
#41798=CARTESIAN_POINT('Ctrl Pts',(17.9120259726677,0.590812830438738,25.685544340611));
#41799=CARTESIAN_POINT('Ctrl Pts',(17.9014404371672,0.445832556717666,25.5984263141198));
#41800=CARTESIAN_POINT('Ctrl Pts',(17.8908549016667,0.287669343599446,25.5503946860645));
#41801=CARTESIAN_POINT('Ctrl Pts',(17.8802693661661,0.129506130481227,25.5023630580093));
#41802=CARTESIAN_POINT('Ctrl Pts',(17.8696838306656,-0.0418400220341332,
25.49341782839));
#41803=CARTESIAN_POINT('Ctrl Pts',(17.8590982951651,-0.203087213622878,
25.5273885686025));
#41804=CARTESIAN_POINT('Ctrl Pts',(17.837927224164,-0.525581596800377,25.5953300490274));
#41805=CARTESIAN_POINT('Ctrl Pts',(17.816756153163,-0.807680136271397,25.8349354087794));
#41806=CARTESIAN_POINT('Ctrl Pts',(17.7955850821619,-0.926913165898742,
26.1421658003154));
#41807=CARTESIAN_POINT('Ctrl Pts',(17.7877789806533,-0.970876229099324,
26.2554464001832));
#41808=CARTESIAN_POINT('Ctrl Pts',(17.7799728791448,-0.992697546793389,
26.3779206976304));
#41809=CARTESIAN_POINT('Ctrl Pts',(17.7721667776362,-0.992388106880432,
26.5001388685385));
#41810=CARTESIAN_POINT('Ctrl Pts',(17.6278332223638,-0.992500513774779,
26.5000263957801));
#41811=CARTESIAN_POINT('Ctrl Pts',(17.6360171481721,-0.992376116598608,
26.372433524086));
#41812=CARTESIAN_POINT('Ctrl Pts',(17.6442010739804,-0.96768164208166,26.2447878927147));
#41813=CARTESIAN_POINT('Ctrl Pts',(17.6523849997888,-0.91969241995934,26.1266093718736));
#41814=CARTESIAN_POINT('Ctrl Pts',(17.662994202687,-0.857481763808406,25.9734090698196));
#41815=CARTESIAN_POINT('Ctrl Pts',(17.6736034055853,-0.756123957416963,
25.8361183798614));
#41816=CARTESIAN_POINT('Ctrl Pts',(17.6842126084836,-0.628108302777589,
25.7314620191992));
#41817=CARTESIAN_POINT('Ctrl Pts',(17.6948218113819,-0.500092648138214,
25.6268056585371));
#41818=CARTESIAN_POINT('Ctrl Pts',(17.7054310142801,-0.345419145250907,
25.5547836271711));
#41819=CARTESIAN_POINT('Ctrl Pts',(17.7160402171784,-0.182860175475946,
25.5243591626045));
#41820=CARTESIAN_POINT('Ctrl Pts',(17.7266494200767,-0.0203012057009853,
25.493934698038));
#41821=CARTESIAN_POINT('Ctrl Pts',(17.7372586229749,0.150143230961628,25.5051078002709));
#41822=CARTESIAN_POINT('Ctrl Pts',(17.7478678258732,0.307313306622748,25.5562311193872));
#41823=CARTESIAN_POINT('Ctrl Pts',(17.7584770287715,0.464483382283867,25.6073544385036));
#41824=CARTESIAN_POINT('Ctrl Pts',(17.7690862316698,0.608379096943491,25.6984279745035));
#41825=CARTESIAN_POINT('Ctrl Pts',(17.779695434568,0.721950285213137,25.8188318149112));
#41826=CARTESIAN_POINT('Ctrl Pts',(17.7903046374663,0.835521473482784,25.9392356553189));
#41827=CARTESIAN_POINT('Ctrl Pts',(17.8009138403646,0.918768135362452,26.0889698001345));
#41828=CARTESIAN_POINT('Ctrl Pts',(17.8115230432629,0.960463045171784,26.2487268741978));
#41829=CARTESIAN_POINT('Ctrl Pts',(17.8221322461611,1.00215795498112,26.4084839482611));
#41830=CARTESIAN_POINT('Ctrl Pts',(17.8327414490594,1.00230111272011,26.5782639515722));
#41831=CARTESIAN_POINT('Ctrl Pts',(17.8433506519577,0.962664065091785,26.7390341250452));
#41832=CARTESIAN_POINT('Ctrl Pts',(17.8539598548559,0.923027017463459,26.8998042985182));
#41833=CARTESIAN_POINT('Ctrl Pts',(17.8645690577542,0.843609764467811,27.0515646421531));
#41834=CARTESIAN_POINT('Ctrl Pts',(17.8751782606525,0.73155870107366,27.1728217499988));
#41835=CARTESIAN_POINT('Ctrl Pts',(17.896396666449,0.507456574285351,27.4153359656903));
#41836=CARTESIAN_POINT('Ctrl Pts',(17.9176150722456,0.152819205903019,27.5358372382248));
#41837=CARTESIAN_POINT('Ctrl Pts',(17.9388334780421,-0.170925105187162,
27.4793334710585));
#41838=CARTESIAN_POINT('Ctrl Pts',(17.9600518838387,-0.494669416277325,
27.4228297038923));
#41839=CARTESIAN_POINT('Ctrl Pts',(17.9812702896352,-0.787520670075341,
27.1893208970252));
#41840=CARTESIAN_POINT('Ctrl Pts',(18.0024886954318,-0.916222847840073,
26.8852310131387));
#41841=CARTESIAN_POINT('Ctrl Pts',(18.0109368710758,-0.967466028593146,
26.7641566602738));
#41842=CARTESIAN_POINT('Ctrl Pts',(18.0193850467198,-0.992687320953884,
26.6318933750482));
#41843=CARTESIAN_POINT('Ctrl Pts',(18.0278332223638,-0.992167930500117,
26.4998747777436));
#41844=CARTESIAN_POINT('Origin',(18.,0.,26.5));
#41845=CARTESIAN_POINT('',(18.5721667776362,-0.992013826433795,26.5001094462548));
#41846=CARTESIAN_POINT('',(18.4278332223638,-0.992438477235227,26.500018847878));
#41847=CARTESIAN_POINT('',(18.,-0.9925,26.5));
#41848=CARTESIAN_POINT('Ctrl Pts',(18.5721667776362,-0.992013826433795,
26.5001094462548));
#41849=CARTESIAN_POINT('Ctrl Pts',(18.5673590644909,-0.992691797507188,
26.5748924995848));
#41850=CARTESIAN_POINT('Ctrl Pts',(18.5625513513455,-0.984964120408148,
26.6496733034542));
#41851=CARTESIAN_POINT('Ctrl Pts',(18.5577436382002,-0.968324488518865,
26.7226384852639));
#41852=CARTESIAN_POINT('Ctrl Pts',(18.5471581026997,-0.931687649182769,
26.8832918976037));
#41853=CARTESIAN_POINT('Ctrl Pts',(18.5365725671991,-0.851847049743327,
27.0351434587505));
#41854=CARTESIAN_POINT('Ctrl Pts',(18.5259870316986,-0.742027972960165,
27.1586971060113));
#41855=CARTESIAN_POINT('Ctrl Pts',(18.5154014961981,-0.632208896177009,
27.2822507532721));
#41856=CARTESIAN_POINT('Ctrl Pts',(18.5048159606975,-0.492411342050135,
27.3775064866468));
#41857=CARTESIAN_POINT('Ctrl Pts',(18.494230425197,-0.337483980317443,27.4334763293345));
#41858=CARTESIAN_POINT('Ctrl Pts',(18.4836448896965,-0.182556618584751,
27.4894461720223));
#41859=CARTESIAN_POINT('Ctrl Pts',(18.473059354196,-0.0124994492462404,
27.5061301240229));
#41860=CARTESIAN_POINT('Ctrl Pts',(18.4624738186954,0.150714681188409,27.4811482717958));
#41861=CARTESIAN_POINT('Ctrl Pts',(18.4518882831949,0.313928811623069,27.4561664195688));
#41862=CARTESIAN_POINT('Ctrl Pts',(18.4413027476943,0.470299903153866,27.3895187631141));
#41863=CARTESIAN_POINT('Ctrl Pts',(18.4307172121938,0.601464224911203,27.2895046704257));
#41864=CARTESIAN_POINT('Ctrl Pts',(18.4201316766933,0.732628546668532,27.1894905777374));
#41865=CARTESIAN_POINT('Ctrl Pts',(18.4095461411927,0.838586098652403,27.0561100488154));
#41866=CARTESIAN_POINT('Ctrl Pts',(18.3989606056922,0.906022115696002,26.9055386884288));
#41867=CARTESIAN_POINT('Ctrl Pts',(18.3883750701917,0.973458132739602,26.7549673280422));
#41868=CARTESIAN_POINT('Ctrl Pts',(18.3777895346912,1.00237261484293,26.5872051361909));
#41869=CARTESIAN_POINT('Ctrl Pts',(18.3672039991906,0.989522901577106,26.4227050502185));
#41870=CARTESIAN_POINT('Ctrl Pts',(18.3566184636901,0.976673188311281,26.2582049642461));
#41871=CARTESIAN_POINT('Ctrl Pts',(18.3460329281896,0.922059279676299,26.0969669841524));
#41872=CARTESIAN_POINT('Ctrl Pts',(18.335447392689,0.832060708684393,25.9586934803334));
#41873=CARTESIAN_POINT('Ctrl Pts',(18.3248618571885,0.742062137692492,25.8204199765144));
#41874=CARTESIAN_POINT('Ctrl Pts',(18.314276321688,0.616678904343671,25.7051109489701));
#41875=CARTESIAN_POINT('Ctrl Pts',(18.3036907861874,0.47157520535541,25.6266768609303));
#41876=CARTESIAN_POINT('Ctrl Pts',(18.2931052506869,0.326471506367148,25.5482427728905));
#41877=CARTESIAN_POINT('Ctrl Pts',(18.2825197151864,0.161647341739446,25.5066836243552));
#41878=CARTESIAN_POINT('Ctrl Pts',(18.2719341796858,-0.00346591980345378,
25.5073490266028));
#41879=CARTESIAN_POINT('Ctrl Pts',(18.2613486441853,-0.168579181346363,
25.5080144288503));
#41880=CARTESIAN_POINT('Ctrl Pts',(18.2507631086848,-0.333981539804471,
25.5509043818806));
#41881=CARTESIAN_POINT('Ctrl Pts',(18.2401775731842,-0.478339357414782,
25.6302515771747));
#41882=CARTESIAN_POINT('Ctrl Pts',(18.2295920376837,-0.622697175025086,
25.7095987724687));
#41883=CARTESIAN_POINT('Ctrl Pts',(18.2190065021832,-0.746010451787596,
25.8254032100265));
#41884=CARTESIAN_POINT('Ctrl Pts',(18.2084209666827,-0.835311394982777,
25.9645118802334));
#41885=CARTESIAN_POINT('Ctrl Pts',(18.1978354311821,-0.924612338177959,
26.1036205504403));
#41886=CARTESIAN_POINT('Ctrl Pts',(18.1872498956816,-0.97990094780581,26.2660334532962));
#41887=CARTESIAN_POINT('Ctrl Pts',(18.176664360181,-0.991147287588631,26.4304271181706));
#41888=CARTESIAN_POINT('Ctrl Pts',(18.1751651659994,-0.992740069282665,
26.4537096460938));
#41889=CARTESIAN_POINT('Ctrl Pts',(18.1736659718178,-0.993449446077136,
26.4770319043688));
#41890=CARTESIAN_POINT('Ctrl Pts',(18.1721667776362,-0.993299106214555,
26.5003419800918));
#41891=CARTESIAN_POINT('Ctrl Pts',(18.0278332223638,-0.992167930500117,
26.4998747777436));
#41892=CARTESIAN_POINT('Ctrl Pts',(18.0299942496181,-0.992035071410358,
26.4661046717627));
#41893=CARTESIAN_POINT('Ctrl Pts',(18.0321552768723,-0.990217930806179,
26.432350576365));
#41894=CARTESIAN_POINT('Ctrl Pts',(18.0343163041266,-0.986721215380445,
26.3988038623597));
#41895=CARTESIAN_POINT('Ctrl Pts',(18.0449255070248,-0.969554674164404,
26.2341118647219));
#41896=CARTESIAN_POINT('Ctrl Pts',(18.0555347099231,-0.911907771858281,
26.0744180806445));
#41897=CARTESIAN_POINT('Ctrl Pts',(18.0661439128214,-0.81856096012734,25.9382301187795));
#41898=CARTESIAN_POINT('Ctrl Pts',(18.0767531157197,-0.725214148396399,
25.8020421569145));
#41899=CARTESIAN_POINT('Ctrl Pts',(18.0873623186179,-0.59616742724064,25.6893600172619));
#41900=CARTESIAN_POINT('Ctrl Pts',(18.0979715215162,-0.448524532865736,
25.6145464133485));
#41901=CARTESIAN_POINT('Ctrl Pts',(18.1085807244145,-0.300881638490831,
25.5397328094351));
#41902=CARTESIAN_POINT('Ctrl Pts',(18.1191899273128,-0.134642570896782,
25.502787741261));
#41903=CARTESIAN_POINT('Ctrl Pts',(18.129799130211,0.0305530962615577,25.5079275849267));
#41904=CARTESIAN_POINT('Ctrl Pts',(18.1404083331093,0.195748763419897,25.5130674285925));
#41905=CARTESIAN_POINT('Ctrl Pts',(18.1510175360076,0.359901030142527,25.5602921840981));
#41906=CARTESIAN_POINT('Ctrl Pts',(18.1616267389058,0.502543046533664,25.6439840108097));
#41907=CARTESIAN_POINT('Ctrl Pts',(18.1722359418041,0.645185062924801,25.7276758375213));
#41908=CARTESIAN_POINT('Ctrl Pts',(18.1828451447024,0.766316828984445,25.847834735439));
#41909=CARTESIAN_POINT('Ctrl Pts',(18.1934543476007,0.851312079351126,25.9896683318641));
#41910=CARTESIAN_POINT('Ctrl Pts',(18.2040635504989,0.936307329717812,26.1315019282893));
#41911=CARTESIAN_POINT('Ctrl Pts',(18.2146727533972,0.985166064391531,26.295010223222));
#41912=CARTESIAN_POINT('Ctrl Pts',(18.2252819562955,0.991802795610055,26.4602266028182));
#41913=CARTESIAN_POINT('Ctrl Pts',(18.2358911591938,0.998439526828578,26.6254429824145));
#41914=CARTESIAN_POINT('Ctrl Pts',(18.246500362092,0.962854254591912,26.7923674466743));
#41915=CARTESIAN_POINT('Ctrl Pts',(18.2571095649903,0.889458244410594,26.9405456860461));
#41916=CARTESIAN_POINT('Ctrl Pts',(18.2677187678886,0.816062234229276,27.088723925418));
#41917=CARTESIAN_POINT('Ctrl Pts',(18.2783279707868,0.704855486103307,27.218155939902));
#41918=CARTESIAN_POINT('Ctrl Pts',(18.2889371736851,0.569419202462848,27.3130130479835));
#41919=CARTESIAN_POINT('Ctrl Pts',(18.2995463765834,0.433982918822389,27.4078701560651));
#41920=CARTESIAN_POINT('Ctrl Pts',(18.3101555794817,0.27431709966744,27.4681523577442));
#41921=CARTESIAN_POINT('Ctrl Pts',(18.3207647823799,0.109979244513689,27.4864748370148));
#41922=CARTESIAN_POINT('Ctrl Pts',(18.3313739852782,-0.0543586106400621,
27.5047973162853));
#41923=CARTESIAN_POINT('Ctrl Pts',(18.3419831881765,-0.223368501792614,
27.4811600731473));
#41924=CARTESIAN_POINT('Ctrl Pts',(18.3525923910747,-0.376373278442671,
27.4184596955982));
#41925=CARTESIAN_POINT('Ctrl Pts',(18.363201593973,-0.529378055092728,27.3557593180491));
#41926=CARTESIAN_POINT('Ctrl Pts',(18.3738107968713,-0.666377717240289,
27.2539958060888));
#41927=CARTESIAN_POINT('Ctrl Pts',(18.3844199997696,-0.770600205445519,
27.1256223026464));
#41928=CARTESIAN_POINT('Ctrl Pts',(18.3950292026678,-0.874822693650748,
26.9972487992039));
#41929=CARTESIAN_POINT('Ctrl Pts',(18.4056384055661,-0.946268007913646,
26.8422653042792));
#41930=CARTESIAN_POINT('Ctrl Pts',(18.4162476084644,-0.976194143930204,
26.6796415593889));
#41931=CARTESIAN_POINT('Ctrl Pts',(18.4201094797642,-0.98708760000836,26.6204446546749));
#41932=CARTESIAN_POINT('Ctrl Pts',(18.423971351064,-0.992479585039877,26.5602353837305));
#41933=CARTESIAN_POINT('Ctrl Pts',(18.4278332223638,-0.992438477235227,
26.500018847878));
#41934=CARTESIAN_POINT('Origin',(18.,0.,26.5));
#41935=CARTESIAN_POINT('',(18.9721667776362,-0.992230389713068,26.5005256112294));
#41936=CARTESIAN_POINT('',(18.8278332223638,-0.992574927394752,26.4999883895028));
#41937=CARTESIAN_POINT('',(18.,-0.9925,26.5));
#41938=CARTESIAN_POINT('Ctrl Pts',(18.9721667776362,-0.992230389713068,
26.5005256112294));
#41939=CARTESIAN_POINT('Ctrl Pts',(18.9716376926645,-0.9922196485029,26.5087936640491));
#41940=CARTESIAN_POINT('Ctrl Pts',(18.9711086076927,-0.992106388713782,
26.5170588667457));
#41941=CARTESIAN_POINT('Ctrl Pts',(18.970579522721,-0.991890303783251,26.5253182937189));
#41942=CARTESIAN_POINT('Ctrl Pts',(18.9599939872204,-0.987567038475448,
26.6905667171419));
#41943=CARTESIAN_POINT('Ctrl Pts',(18.9494084517199,-0.942083890356008,
26.8535031758697));
#41944=CARTESIAN_POINT('Ctrl Pts',(18.9388229162194,-0.859710884972681,
26.9961559032424));
#41945=CARTESIAN_POINT('Ctrl Pts',(18.9282373807188,-0.777337879589353,
27.138808630615));
#41946=CARTESIAN_POINT('Ctrl Pts',(18.9176518452183,-0.658075016942137,
27.2611776266325));
#41947=CARTESIAN_POINT('Ctrl Pts',(18.9070663097178,-0.517187564913484,
27.3472802930853));
#41948=CARTESIAN_POINT('Ctrl Pts',(18.8964807742172,-0.376300112884831,
27.433382959538));
#41949=CARTESIAN_POINT('Ctrl Pts',(18.8858952387167,-0.213788071474739,
27.4832192964261));
#41950=CARTESIAN_POINT('Ctrl Pts',(18.8753097032162,-0.0490408952192969,
27.4912980243871));
#41951=CARTESIAN_POINT('Ctrl Pts',(18.8647241677156,0.115706281036145,27.4993767523481));
#41952=CARTESIAN_POINT('Ctrl Pts',(18.8541386322151,0.282688592136938,27.4656978713822));
#41953=CARTESIAN_POINT('Ctrl Pts',(18.8435530967146,0.43130001490854,27.3940459112129));
#41954=CARTESIAN_POINT('Ctrl Pts',(18.832967561214,0.57991143768015,27.3223939510436));
#41955=CARTESIAN_POINT('Ctrl Pts',(18.8223820257135,0.710151972122568,27.212768911671));
#41956=CARTESIAN_POINT('Ctrl Pts',(18.811796490213,0.806359128334629,27.0787183528563));
#41957=CARTESIAN_POINT('Ctrl Pts',(18.8012109547124,0.902566284546691,26.9446677940417));
#41958=CARTESIAN_POINT('Ctrl Pts',(18.7906254192119,0.964740062528397,26.7861917157849));
#41959=CARTESIAN_POINT('Ctrl Pts',(18.7800398837114,0.985058465493209,26.6224647452279));
#41960=CARTESIAN_POINT('Ctrl Pts',(18.7694543482108,1.00537686845802,26.4587377746709));
#41961=CARTESIAN_POINT('Ctrl Pts',(18.7588688127103,0.98383989640594,26.2897599118136));
#41962=CARTESIAN_POINT('Ctrl Pts',(18.7482832772098,0.923457247109937,26.1362645256848));
#41963=CARTESIAN_POINT('Ctrl Pts',(18.7376977417093,0.863074597813934,25.9827691395561));
#41964=CARTESIAN_POINT('Ctrl Pts',(18.7271122062087,0.763846271274007,25.8447562301559));
#41965=CARTESIAN_POINT('Ctrl Pts',(18.7165266707082,0.637180468464792,25.7388377815076));
#41966=CARTESIAN_POINT('Ctrl Pts',(18.7059411352077,0.510514665655577,25.6329193328593));
#41967=CARTESIAN_POINT('Ctrl Pts',(18.6953555997071,0.356411386577074,25.5590953449629));
#41968=CARTESIAN_POINT('Ctrl Pts',(18.6847700642066,0.194898297897354,25.5267127145229));
#41969=CARTESIAN_POINT('Ctrl Pts',(18.6741845287061,0.0333852092176347,
25.4943300840828));
#41970=CARTESIAN_POINT('Ctrl Pts',(18.6635989932055,-0.135537689063301,
25.5033888110992));
#41971=CARTESIAN_POINT('Ctrl Pts',(18.653013457705,-0.293477330358148,25.5521822718937));
#41972=CARTESIAN_POINT('Ctrl Pts',(18.6424279222045,-0.451416971653003,
25.6009757326883));
#41973=CARTESIAN_POINT('Ctrl Pts',(18.6318423867039,-0.598373355961768,
25.689503927261));
#41974=CARTESIAN_POINT('Ctrl Pts',(18.6212568512034,-0.712934505791141,
25.8079417618848));
#41975=CARTESIAN_POINT('Ctrl Pts',(18.6048934933477,-0.890025696966787,
25.9910256192399));
#41976=CARTESIAN_POINT('Ctrl Pts',(18.5885301354919,-0.989706308710838,
26.2455805618997));
#41977=CARTESIAN_POINT('Ctrl Pts',(18.5721667776362,-0.992013826433795,
26.5001094462548));
#41978=CARTESIAN_POINT('Ctrl Pts',(18.4278332223638,-0.992438477235227,
26.500018847878));
#41979=CARTESIAN_POINT('Ctrl Pts',(18.4345805539623,-0.992366655062056,
26.394810542483));
#41980=CARTESIAN_POINT('Ctrl Pts',(18.4413278855608,-0.975709826569298,
26.2895800603005));
#41981=CARTESIAN_POINT('Ctrl Pts',(18.4480752171592,-0.942832678942907,
26.1896879916471));
#41982=CARTESIAN_POINT('Ctrl Pts',(18.4586844200575,-0.891138120168834,
26.0326221636518));
#41983=CARTESIAN_POINT('Ctrl Pts',(18.4692936229557,-0.799342044850471,
25.8887545025172));
#41984=CARTESIAN_POINT('Ctrl Pts',(18.479902825854,-0.678680210339956,25.7756935385323));
#41985=CARTESIAN_POINT('Ctrl Pts',(18.4905120287523,-0.558018375829447,
25.6626325745473));
#41986=CARTESIAN_POINT('Ctrl Pts',(18.5011212316506,-0.408490782126793,
25.580378307712));
#41987=CARTESIAN_POINT('Ctrl Pts',(18.5117304345488,-0.248398062315547,
25.5389978519782));
#41988=CARTESIAN_POINT('Ctrl Pts',(18.5223396374471,-0.0883053425042835,
25.4976173962445));
#41989=CARTESIAN_POINT('Ctrl Pts',(18.5329488403454,0.0823525034155692,
25.4971107516123));
#41990=CARTESIAN_POINT('Ctrl Pts',(18.5435580432436,0.242688139518946,25.5375400062926));
#41991=CARTESIAN_POINT('Ctrl Pts',(18.5541672461419,0.403023775622313,25.577969260973));
#41992=CARTESIAN_POINT('Ctrl Pts',(18.5647764490402,0.553037201909199,25.659334414966));
#41993=CARTESIAN_POINT('Ctrl Pts',(18.5753856519385,0.674368074295156,25.7716769836757));
#41994=CARTESIAN_POINT('Ctrl Pts',(18.5859948548367,0.795698946681113,25.8840195523854));
#41995=CARTESIAN_POINT('Ctrl Pts',(18.596604057735,0.888347265166135,26.0273395358117));
#41996=CARTESIAN_POINT('Ctrl Pts',(18.6072132606333,0.940973566665014,26.1840957387243));
#41997=CARTESIAN_POINT('Ctrl Pts',(18.6178224635316,0.993599868163893,26.3408519416368));
#41998=CARTESIAN_POINT('Ctrl Pts',(18.6284316664298,1.00620415267662,26.5110443640355));
#41999=CARTESIAN_POINT('Ctrl Pts',(18.6390408693281,0.977243784014913,26.6738428056409));
#42000=CARTESIAN_POINT('Ctrl Pts',(18.6496500722264,0.948283415353202,26.8366412472463));
#42001=CARTESIAN_POINT('Ctrl Pts',(18.6602592751246,0.877758393517053,26.9920457080584));
#42002=CARTESIAN_POINT('Ctrl Pts',(18.6708684780229,0.774300401561698,27.121035933725));
#42003=CARTESIAN_POINT('Ctrl Pts',(18.6814776809212,0.670842409606337,27.2500261593916));
#42004=CARTESIAN_POINT('Ctrl Pts',(18.6920868838195,0.53445144753177,27.3526021499128));
#42005=CARTESIAN_POINT('Ctrl Pts',(18.7026960867178,0.381820683670061,27.416209422821));
#42006=CARTESIAN_POINT('Ctrl Pts',(18.713305289616,0.229189919808361,27.4798166957291));
#42007=CARTESIAN_POINT('Ctrl Pts',(18.7239144925143,0.0603193541595261,
27.5044552510242));
#42008=CARTESIAN_POINT('Ctrl Pts',(18.7345236954126,-0.104122613443559,
27.4871095287382));
#42009=CARTESIAN_POINT('Ctrl Pts',(18.7451328983108,-0.268564581046635,
27.4697638064523));
#42010=CARTESIAN_POINT('Ctrl Pts',(18.7557421012091,-0.428577950603957,
27.4104338065854));
#42011=CARTESIAN_POINT('Ctrl Pts',(18.7663513041074,-0.564578365915668,
27.3163810447172));
#42012=CARTESIAN_POINT('Ctrl Pts',(18.7769605070056,-0.700578781227387,
27.222328282849));
#42013=CARTESIAN_POINT('Ctrl Pts',(18.7875697099039,-0.812566242293489,
27.0935527589795));
#42014=CARTESIAN_POINT('Ctrl Pts',(18.7981789128022,-0.886834382501103,
26.9458155656893));
#42015=CARTESIAN_POINT('Ctrl Pts',(18.8080636826561,-0.956031237388956,
26.8081663786076));
#42016=CARTESIAN_POINT('Ctrl Pts',(18.8179484525099,-0.992484111373763,
26.6540566475057));
#42017=CARTESIAN_POINT('Ctrl Pts',(18.8278332223638,-0.992574927394752,
26.4999883895028));
#42018=CARTESIAN_POINT('Origin',(18.,0.,26.5));
#42019=CARTESIAN_POINT('',(19.3721667776362,-0.992405353361108,26.4996434684176));
#42020=CARTESIAN_POINT('',(19.2278332223638,-0.992414099467528,26.5000000900757));
#42021=CARTESIAN_POINT('',(18.,-0.9925,26.5));
#42022=CARTESIAN_POINT('Ctrl Pts',(19.3721667776362,-0.992405353361108,
26.4996434684176));
#42023=CARTESIAN_POINT('Ctrl Pts',(19.3653307853375,-0.992340977052407,
26.6063601754747));
#42024=CARTESIAN_POINT('Ctrl Pts',(19.3584947930388,-0.975264170858423,
26.7132672752177));
#42025=CARTESIAN_POINT('Ctrl Pts',(19.3516588007401,-0.941543675704311,
26.8144238844136));
#42026=CARTESIAN_POINT('Ctrl Pts',(19.3410732652396,-0.889327481924047,
26.9710649148549));
#42027=CARTESIAN_POINT('Ctrl Pts',(19.3304877297391,-0.797202170370003,
27.1139171148842));
#42028=CARTESIAN_POINT('Ctrl Pts',(19.3199021942385,-0.676452402081721,
27.2262843315731));
#42029=CARTESIAN_POINT('Ctrl Pts',(19.309316658738,-0.555702633793439,27.338651548262));
#42030=CARTESIAN_POINT('Ctrl Pts',(19.2987311232374,-0.406328408770916,
27.4205337816104));
#42031=CARTESIAN_POINT('Ctrl Pts',(19.2881455877369,-0.246523395998278,
27.4615425156544));
#42032=CARTESIAN_POINT('Ctrl Pts',(19.2775600522364,-0.0867183832256306,
27.5025512496983));
#42033=CARTESIAN_POINT('Ctrl Pts',(19.2669745167358,0.0835174172971379,
27.5026864844377));
#42034=CARTESIAN_POINT('Ctrl Pts',(19.2563889812353,0.243476972870307,27.462210444508));
#42035=CARTESIAN_POINT('Ctrl Pts',(19.2458034457348,0.403436528443476,27.4217344045784));
#42036=CARTESIAN_POINT('Ctrl Pts',(19.2352179102343,0.553119839067051,27.3406470899797));
#42037=CARTESIAN_POINT('Ctrl Pts',(19.2246323747337,0.674187278220771,27.2285666119654));
#42038=CARTESIAN_POINT('Ctrl Pts',(19.2140468392332,0.795254717374478,27.1164861339511));
#42039=CARTESIAN_POINT('Ctrl Pts',(19.2034613037327,0.887706285058342,26.9734124925212));
#42040=CARTESIAN_POINT('Ctrl Pts',(19.1928757682321,0.94047898641325,26.817137286811));
#42041=CARTESIAN_POINT('Ctrl Pts',(19.1822902327316,0.993251687768168,26.6608620811007));
#42042=CARTESIAN_POINT('Ctrl Pts',(19.1717046972311,1.00634552279412,26.49138531111));
#42043=CARTESIAN_POINT('Ctrl Pts',(19.1611191617305,0.977775061776517,26.3287609830781));
#42044=CARTESIAN_POINT('Ctrl Pts',(19.15053362623,0.949204600758917,26.1661366550462));
#42045=CARTESIAN_POINT('Ctrl Pts',(19.1399480907295,0.878969843697767,26.0103647689731));
#42046=CARTESIAN_POINT('Ctrl Pts',(19.1293625552289,0.776358190350592,25.8815006496868));
#42047=CARTESIAN_POINT('Ctrl Pts',(19.1187770197284,0.673746537003416,25.7526365304005));
#42048=CARTESIAN_POINT('Ctrl Pts',(19.1081914842279,0.538757987370212,25.6506801779009));
#42049=CARTESIAN_POINT('Ctrl Pts',(19.0976059487273,0.386554949372809,25.586182369478));
#42050=CARTESIAN_POINT('Ctrl Pts',(19.0870204132268,0.234351911375407,25.521684561055));
#42051=CARTESIAN_POINT('Ctrl Pts',(19.0764348777263,0.0649343850138017,
25.4946452967086));
#42052=CARTESIAN_POINT('Ctrl Pts',(19.0658493422258,-0.0989942199664423,
25.5113542819714));
#42053=CARTESIAN_POINT('Ctrl Pts',(19.0446782712247,-0.42685142992694,25.5447722524971));
#42054=CARTESIAN_POINT('Ctrl Pts',(19.0235072002236,-0.732752954362004,
25.7531832214598));
#42055=CARTESIAN_POINT('Ctrl Pts',(19.0023361292225,-0.883835619178809,
26.0460673952717));
#42056=CARTESIAN_POINT('Ctrl Pts',(18.9922796786938,-0.955601253728412,
26.1851900312712));
#42057=CARTESIAN_POINT('Ctrl Pts',(18.982223228165,-0.992434550584083,26.3433726611575));
#42058=CARTESIAN_POINT('Ctrl Pts',(18.9721667776362,-0.992230389713068,
26.5005256112294));
#42059=CARTESIAN_POINT('Ctrl Pts',(18.8278332223638,-0.992574927394752,
26.4999883895028));
#42060=CARTESIAN_POINT('Ctrl Pts',(18.8285576554082,-0.992581583101212,
26.4886970656946));
#42061=CARTESIAN_POINT('Ctrl Pts',(18.8292820884526,-0.992392934494438,
26.4774059646426));
#42062=CARTESIAN_POINT('Ctrl Pts',(18.830006521497,-0.992007557368196,26.4661215821387));
#42063=CARTESIAN_POINT('Ctrl Pts',(18.8406157243953,-0.986363772678551,
26.3008636545894));
#42064=CARTESIAN_POINT('Ctrl Pts',(18.8512249272935,-0.938527383950129,
26.1370466622021));
#42065=CARTESIAN_POINT('Ctrl Pts',(18.8618341301918,-0.854353182112096,
25.9947204921234));
#42066=CARTESIAN_POINT('Ctrl Pts',(18.8724433330901,-0.770178980274068,
25.8523943220447));
#42067=CARTESIAN_POINT('Ctrl Pts',(18.8830525359884,-0.649666965326431,
25.7315589742747));
#42068=CARTESIAN_POINT('Ctrl Pts',(18.8936617388866,-0.507566841925601,
25.6470037269119));
#42069=CARTESIAN_POINT('Ctrl Pts',(18.9042709417849,-0.365466718524772,
25.5624484795491));
#42070=CARTESIAN_POINT('Ctrl Pts',(18.9148801446832,-0.201778486670748,
25.5141733325935));
#42071=CARTESIAN_POINT('Ctrl Pts',(18.9254893475815,-0.0365362742051188,
25.5080867771853));
#42072=CARTESIAN_POINT('Ctrl Pts',(18.9360985504797,0.128705938260501,25.5020002217771));
#42073=CARTESIAN_POINT('Ctrl Pts',(18.946707753378,0.295502131337727,25.5381022579163));
#42074=CARTESIAN_POINT('Ctrl Pts',(18.9573169562763,0.443437787775487,25.6119742856872));
#42075=CARTESIAN_POINT('Ctrl Pts',(18.9679261591746,0.591373444213265,25.6858463134581));
#42076=CARTESIAN_POINT('Ctrl Pts',(18.9785353620728,0.720448564011572,25.7974883328607));
#42077=CARTESIAN_POINT('Ctrl Pts',(18.9891445649711,0.814865386913012,25.93323625545));
#42078=CARTESIAN_POINT('Ctrl Pts',(18.9997537678693,0.909282209814446,26.0689841780393));
#42079=CARTESIAN_POINT('Ctrl Pts',(19.0103629707676,0.969040735819015,26.2288380038151));
#42080=CARTESIAN_POINT('Ctrl Pts',(19.0209721736659,0.986827000272459,26.3932329055939));
#42081=CARTESIAN_POINT('Ctrl Pts',(19.0315813765642,1.0046132647259,26.5576278073727));
#42082=CARTESIAN_POINT('Ctrl Pts',(19.0421905794624,0.980427267628221,26.7265637851543));
#42083=CARTESIAN_POINT('Ctrl Pts',(19.0527997823607,0.917229181186273,26.8793644291443));
#42084=CARTESIAN_POINT('Ctrl Pts',(19.063408985259,0.854031094744325,27.0321650731344));
#42085=CARTESIAN_POINT('Ctrl Pts',(19.0740181881573,0.751820918958111,27.1688303833328));
#42086=CARTESIAN_POINT('Ctrl Pts',(19.0846273910556,0.623108360217072,27.2726336210298));
#42087=CARTESIAN_POINT('Ctrl Pts',(19.0952365939538,0.494395801476034,27.3764368587268));
#42088=CARTESIAN_POINT('Ctrl Pts',(19.1058457968521,0.339180859780171,27.4473780239223));
#42089=CARTESIAN_POINT('Ctrl Pts',(19.1164549997504,0.176460600070971,27.4767744865324));
#42090=CARTESIAN_POINT('Ctrl Pts',(19.1270642026486,0.0137403403617714,
27.5061709491426));
#42091=CARTESIAN_POINT('Ctrl Pts',(19.1376734055469,-0.156485237360765,
27.4940227091673));
#42092=CARTESIAN_POINT('Ctrl Pts',(19.1482826084452,-0.313381886600382,
27.441816613821));
#42093=CARTESIAN_POINT('Ctrl Pts',(19.1588918113435,-0.470278535839999,
27.3896105184747));
#42094=CARTESIAN_POINT('Ctrl Pts',(19.1695010142417,-0.613846256596695,
27.2973465677573));
#42095=CARTESIAN_POINT('Ctrl Pts',(19.18011021714,-0.726513510427623,27.1763171298173));
#42096=CARTESIAN_POINT('Ctrl Pts',(19.1907194200383,-0.839180764258558,
27.0552876918772));
#42097=CARTESIAN_POINT('Ctrl Pts',(19.2013286229365,-0.92094755116372,26.9054927667144));
#42098=CARTESIAN_POINT('Ctrl Pts',(19.2119378258348,-0.961806271719183,
26.7452660526856));
#42099=CARTESIAN_POINT('Ctrl Pts',(19.2172362913445,-0.982212000943896,
26.6652453644069));
#42100=CARTESIAN_POINT('Ctrl Pts',(19.2225347568541,-0.992414359490076,
26.5826227587524));
#42101=CARTESIAN_POINT('Ctrl Pts',(19.2278332223638,-0.992414099682224,
26.5000000900755));
#42102=CARTESIAN_POINT('Origin',(18.,0.,26.5));
#42103=CARTESIAN_POINT('',(19.7721667776362,-0.992492903155771,26.500016853248));
#42104=CARTESIAN_POINT('',(19.6278332223638,-0.992575270015615,26.5000114296632));
#42105=CARTESIAN_POINT('',(18.,-0.9925,26.5));
#42106=CARTESIAN_POINT('Ctrl Pts',(19.7721667776362,-0.992492903155771,
26.500016853248));
#42107=CARTESIAN_POINT('Ctrl Pts',(19.7696094135111,-0.992505792531705,
26.5398596057124));
#42108=CARTESIAN_POINT('Ctrl Pts',(19.767052049386,-0.990124581390803,26.5797014438245));
#42109=CARTESIAN_POINT('Ctrl Pts',(19.7644946852609,-0.985319177046528,
26.6192598084646));
#42110=CARTESIAN_POINT('Ctrl Pts',(19.7539091497603,-0.965428470916284,
26.783001244081));
#42111=CARTESIAN_POINT('Ctrl Pts',(19.7433236142598,-0.904003382287043,
26.9418858491443));
#42112=CARTESIAN_POINT('Ctrl Pts',(19.7327380787593,-0.80825773862658,27.0762440647293));
#42113=CARTESIAN_POINT('Ctrl Pts',(19.7221525432587,-0.712512094966116,
27.2106022803143));
#42114=CARTESIAN_POINT('Ctrl Pts',(19.7115670077582,-0.582445896274432,
27.3204341064211));
#42115=CARTESIAN_POINT('Ctrl Pts',(19.7009814722577,-0.434059675387492,
27.3925929498046));
#42116=CARTESIAN_POINT('Ctrl Pts',(19.6903959367571,-0.285673454500552,
27.4647517931881));
#42117=CARTESIAN_POINT('Ctrl Pts',(19.6798104012566,-0.118967211418359,
27.4992376538483));
#42118=CARTESIAN_POINT('Ctrl Pts',(19.6692248657561,0.0458380169416741,
27.4915829115048));
#42119=CARTESIAN_POINT('Ctrl Pts',(19.6586393302555,0.210643245301707,27.4839281691613));
#42120=CARTESIAN_POINT('Ctrl Pts',(19.648053794755,0.373547458939575,27.4341328238141));
#42121=CARTESIAN_POINT('Ctrl Pts',(19.6374682592545,0.51462458881678,27.3486685543578));
#42122=CARTESIAN_POINT('Ctrl Pts',(19.6268827237539,0.655701718694,27.2632042849015));
#42123=CARTESIAN_POINT('Ctrl Pts',(19.6162971882534,0.774951764810546,27.1420710913361));
#42124=CARTESIAN_POINT('Ctrl Pts',(19.6057116527529,0.857930614775059,26.9993214721802));
#42125=CARTESIAN_POINT('Ctrl Pts',(19.5951261172524,0.940909464739562,26.8565718530243));
#42126=CARTESIAN_POINT('Ctrl Pts',(19.5845405817518,0.987617118552037,26.6922058082778));
#42127=CARTESIAN_POINT('Ctrl Pts',(19.5739550462513,0.992227228213515,26.5275429419996));
#42128=CARTESIAN_POINT('Ctrl Pts',(19.5633695107507,0.996837337874994,26.3628800757214));
#42129=CARTESIAN_POINT('Ctrl Pts',(19.5527839752502,0.959349903385473,26.1979203879114));
#42130=CARTESIAN_POINT('Ctrl Pts',(19.5421984397497,0.884556620605071,26.0505036421938));
#42131=CARTESIAN_POINT('Ctrl Pts',(19.5316129042492,0.809763337824661,25.9030868964762));
#42132=CARTESIAN_POINT('Ctrl Pts',(19.5210273687486,0.697664206753381,25.773213092851));
#42133=CARTESIAN_POINT('Ctrl Pts',(19.5104418332481,0.561562925403105,25.680324886204));
#42134=CARTESIAN_POINT('Ctrl Pts',(19.489270762247,0.289360362702577,25.4945484729099));
#42135=CARTESIAN_POINT('Ctrl Pts',(19.468099691246,-0.0788508011138748,
25.456714447529));
#42136=CARTESIAN_POINT('Ctrl Pts',(19.4469286202449,-0.383144249725361,
25.5832553816541));
#42137=CARTESIAN_POINT('Ctrl Pts',(19.4363430847444,-0.535290974031126,
25.6465258487166));
#42138=CARTESIAN_POINT('Ctrl Pts',(19.4257575492438,-0.671458269535649,
25.7508900556557));
#42139=CARTESIAN_POINT('Ctrl Pts',(19.4151720137433,-0.774666660030811,
25.8800169707371));
#42140=CARTESIAN_POINT('Ctrl Pts',(19.4045864782428,-0.877875050525961,
26.0091438858185));
#42141=CARTESIAN_POINT('Ctrl Pts',(19.3940009427422,-0.948124536011754,
26.1630335090423));
#42142=CARTESIAN_POINT('Ctrl Pts',(19.3834154072417,-0.977095740751408,
26.3251932510807));
#42143=CARTESIAN_POINT('Ctrl Pts',(19.3796658640399,-0.987357742496616,
26.3826324763651));
#42144=CARTESIAN_POINT('Ctrl Pts',(19.375916320838,-0.99244066377986,26.4411093323356));
#42145=CARTESIAN_POINT('Ctrl Pts',(19.3721667776362,-0.992405353361108,
26.4996434684176));
#42146=CARTESIAN_POINT('Ctrl Pts',(19.2278332223638,-0.992414099682224,
26.5000000900755));
#42147=CARTESIAN_POINT('Ctrl Pts',(19.2331439597524,-0.992413839272626,
26.4171860574298));
#42148=CARTESIAN_POINT('Ctrl Pts',(19.238454697141,-0.98216364481267,26.3343719614693));
#42149=CARTESIAN_POINT('Ctrl Pts',(19.2437654345296,-0.961664273866392,
26.254177777068));
#42150=CARTESIAN_POINT('Ctrl Pts',(19.2543746374279,-0.920712901252369,
26.0939747183739));
#42151=CARTESIAN_POINT('Ctrl Pts',(19.2649838403262,-0.838859501818548,
25.9442271038806));
#42152=CARTESIAN_POINT('Ctrl Pts',(19.2755930432245,-0.726122275667864,
25.8232628414981));
#42153=CARTESIAN_POINT('Ctrl Pts',(19.2862022461227,-0.613385049517181,
25.7022985791156));
#42154=CARTESIAN_POINT('Ctrl Pts',(19.296811449021,-0.469763996649633,25.6101176688438));
#42155=CARTESIAN_POINT('Ctrl Pts',(19.3074206519193,-0.312837182931623,
25.5580023153459));
#42156=CARTESIAN_POINT('Ctrl Pts',(19.3180298548175,-0.15591036921363,25.505886961848));
#42157=CARTESIAN_POINT('Ctrl Pts',(19.3286390577158,0.0143222053548266,
25.4938371651239));
#42158=CARTESIAN_POINT('Ctrl Pts',(19.3392482606141,0.177025437920684,25.5233277237234));
#42159=CARTESIAN_POINT('Ctrl Pts',(19.3498574635124,0.33972867048655,25.552818282323));
#42160=CARTESIAN_POINT('Ctrl Pts',(19.3604666664106,0.494902561049821,25.6238491962462));
#42161=CARTESIAN_POINT('Ctrl Pts',(19.3710758693089,0.623555068996665,25.7277268508832));
#42162=CARTESIAN_POINT('Ctrl Pts',(19.3816850722072,0.752207576943509,25.8316045055202));
#42163=CARTESIAN_POINT('Ctrl Pts',(19.3922942751055,0.854338702273929,25.968328900871));
#42164=CARTESIAN_POINT('Ctrl Pts',(19.4029034780037,0.917448413744468,26.1211660666783));
#42165=CARTESIAN_POINT('Ctrl Pts',(19.413512680902,0.98055812521501,26.2740032324856));
#42166=CARTESIAN_POINT('Ctrl Pts',(19.4241218838003,1.00464642282567,26.4429531687493));
#42167=CARTESIAN_POINT('Ctrl Pts',(19.4347310866985,0.986765091996794,26.6073377572656));
#42168=CARTESIAN_POINT('Ctrl Pts',(19.4453402895968,0.968883761167923,26.7717223457819));
#42169=CARTESIAN_POINT('Ctrl Pts',(19.4559494924951,0.909032801899521,26.9315415865509));
#42170=CARTESIAN_POINT('Ctrl Pts',(19.4665586953933,0.814537491949821,27.0672348853221));
#42171=CARTESIAN_POINT('Ctrl Pts',(19.4771678982916,0.720042182000127,27.2029281840933));
#42172=CARTESIAN_POINT('Ctrl Pts',(19.4877771011899,0.590902521369115,27.3144955408667));
#42173=CARTESIAN_POINT('Ctrl Pts',(19.4983863040882,0.442924169569878,27.388282005294));
#42174=CARTESIAN_POINT('Ctrl Pts',(19.5089955069864,0.294945817770624,27.4620684697212));
#42175=CARTESIAN_POINT('Ctrl Pts',(19.5196047098847,0.128128774803148,27.4980740418023));
#42176=CARTESIAN_POINT('Ctrl Pts',(19.530213912783,-0.0371098901747996,
27.4918919280695));
#42177=CARTESIAN_POINT('Ctrl Pts',(19.5408231156813,-0.202348555152747,
27.4857098143367));
#42178=CARTESIAN_POINT('Ctrl Pts',(19.5514323185795,-0.366008842141143,
27.4373400147901));
#42179=CARTESIAN_POINT('Ctrl Pts',(19.5620415214778,-0.508060043615217,
27.3527026052499));
#42180=CARTESIAN_POINT('Ctrl Pts',(19.5726507243761,-0.650111245089282,
27.2680651957097));
#42181=CARTESIAN_POINT('Ctrl Pts',(19.5832599272743,-0.770553361049032,
27.147160176176));
#42182=CARTESIAN_POINT('Ctrl Pts',(19.5938691301726,-0.854645241745505,
27.0047853520854));
#42183=CARTESIAN_POINT('Ctrl Pts',(19.6044783330709,-0.938737122441978,
26.8624105279949));
#42184=CARTESIAN_POINT('Ctrl Pts',(19.6150875359692,-0.986478767875177,
26.6985658993474));
#42185=CARTESIAN_POINT('Ctrl Pts',(19.6256967388675,-0.992026983254105,
26.5333047356095));
#42186=CARTESIAN_POINT('Ctrl Pts',(19.6264089000329,-0.992399416844861,
26.5222112930482));
#42187=CARTESIAN_POINT('Ctrl Pts',(19.6271210611984,-0.992581726893453,
26.5111114675817));
#42188=CARTESIAN_POINT('Ctrl Pts',(19.6278332223638,-0.992575270015615,
26.5000114296632));
#42189=CARTESIAN_POINT('Origin',(18.,0.,26.5));
#42190=CARTESIAN_POINT('',(20.1721667776362,-0.9925,26.5000000000001));
#42191=CARTESIAN_POINT('',(20.0278332223638,-0.992438391306935,26.4999811413391));
#42192=CARTESIAN_POINT('',(18.,-0.9925,26.5));
#42193=CARTESIAN_POINT('Ctrl Pts',(20.1721667776362,-0.992597511301432,
26.4999846070725));
#42194=CARTESIAN_POINT('Ctrl Pts',(20.1633025061841,-0.992451437885555,
26.6381508584163));
#42195=CARTESIAN_POINT('Ctrl Pts',(20.1544382347321,-0.963248274446475,
26.7763584278731));
#42196=CARTESIAN_POINT('Ctrl Pts',(20.14557396328,-0.907195507711203,26.9026490862115));
#42197=CARTESIAN_POINT('Ctrl Pts',(20.1349884277795,-0.840258415882739,
27.0534628619918));
#42198=CARTESIAN_POINT('Ctrl Pts',(20.124402892279,-0.735032022423416,27.1872823381065));
#42199=CARTESIAN_POINT('Ctrl Pts',(20.1138173567784,-0.60409658984389,27.2876579868982));
#42200=CARTESIAN_POINT('Ctrl Pts',(20.1032318212779,-0.473161157264348,
27.3880336356899));
#42201=CARTESIAN_POINT('Ctrl Pts',(20.0926462857774,-0.316516685564598,
27.4549654571587));
#42202=CARTESIAN_POINT('Ctrl Pts',(20.0820607502768,-0.153569034970045,
27.4805576648362));
#42203=CARTESIAN_POINT('Ctrl Pts',(20.0714752147763,0.00937861562448072,
27.5061498725137));
#42204=CARTESIAN_POINT('Ctrl Pts',(20.0608896792758,0.178629445113807,27.4904024663998));
#42205=CARTESIAN_POINT('Ctrl Pts',(20.0503041437752,0.334082461328613,27.4347490472748));
#42206=CARTESIAN_POINT('Ctrl Pts',(20.0397186082747,0.489535477543428,27.3790956281497));
#42207=CARTESIAN_POINT('Ctrl Pts',(20.0291330727742,0.63119068048372,27.2835361960135));
#42208=CARTESIAN_POINT('Ctrl Pts',(20.0185475372736,0.740851630053171,27.1606151287322));
#42209=CARTESIAN_POINT('Ctrl Pts',(20.0079620017731,0.850512579622629,27.0376940614509));
#42210=CARTESIAN_POINT('Ctrl Pts',(19.9973764662726,0.928179275821242,26.8874113590246));
#42211=CARTESIAN_POINT('Ctrl Pts',(19.986790930772,0.966016269521608,26.726494939804));
#42212=CARTESIAN_POINT('Ctrl Pts',(19.9762053952715,1.00385326322197,26.5655785205835));
#42213=CARTESIAN_POINT('Ctrl Pts',(19.965619859771,1.00186055442409,26.3940283845687));
#42214=CARTESIAN_POINT('Ctrl Pts',(19.9550343242704,0.957677353194437,26.2352844950851));
#42215=CARTESIAN_POINT('Ctrl Pts',(19.9338632532694,0.869310950735119,25.9177967161179));
#42216=CARTESIAN_POINT('Ctrl Pts',(19.9126921822683,0.612182578548673,25.6515339232753));
#42217=CARTESIAN_POINT('Ctrl Pts',(19.8915211112673,0.297971613651096,25.5521428753119));
#42218=CARTESIAN_POINT('Ctrl Pts',(19.8809355757667,0.14086613120232,25.5024473513302));
#42219=CARTESIAN_POINT('Ctrl Pts',(19.8703500402662,-0.0305099994242361,
25.4944697635683));
#42220=CARTESIAN_POINT('Ctrl Pts',(19.8597645047656,-0.192648711794436,
25.5266686768725));
#42221=CARTESIAN_POINT('Ctrl Pts',(19.8491789692651,-0.354787424164644,
25.5588675901767));
#42222=CARTESIAN_POINT('Ctrl Pts',(19.8385934337646,-0.507688718278495,
25.631243004547));
#42223=CARTESIAN_POINT('Ctrl Pts',(19.8280078982641,-0.63436145167657,25.7365479486641));
#42224=CARTESIAN_POINT('Ctrl Pts',(19.8174223627635,-0.761034185074659,
25.8418528927812));
#42225=CARTESIAN_POINT('Ctrl Pts',(19.806836827263,-0.861478357756966,25.9800873666451));
#42226=CARTESIAN_POINT('Ctrl Pts',(19.7962512917625,-0.922522282282495,
26.1335037366619));
#42227=CARTESIAN_POINT('Ctrl Pts',(19.788223120387,-0.968818578534504,26.249856179127));
#42228=CARTESIAN_POINT('Ctrl Pts',(19.7801949490116,-0.992452440353502,
26.37494102157));
#42229=CARTESIAN_POINT('Ctrl Pts',(19.7721667776362,-0.992492903155771,
26.500016853248));
#42230=CARTESIAN_POINT('Ctrl Pts',(19.6278332223638,-0.992575270015615,
26.5000114296632));
#42231=CARTESIAN_POINT('Ctrl Pts',(19.6377302640966,-0.992485537532951,
26.3457520515285));
#42232=CARTESIAN_POINT('Ctrl Pts',(19.6476273058294,-0.955938871864007,
26.1914516421247));
#42233=CARTESIAN_POINT('Ctrl Pts',(19.6575243475622,-0.886576419823079,
26.0536716536764));
#42234=CARTESIAN_POINT('Ctrl Pts',(19.6681335504605,-0.812222855688468,
25.9059774343096));
#42235=CARTESIAN_POINT('Ctrl Pts',(19.6787427533588,-0.700160942094587,
25.7772666944042));
#42236=CARTESIAN_POINT('Ctrl Pts',(19.6893519562571,-0.564106159181243,
25.683292597014));
#42237=CARTESIAN_POINT('Ctrl Pts',(19.6999611591554,-0.428051376267899,
25.5893184996239));
#42238=CARTESIAN_POINT('Ctrl Pts',(19.7105703620536,-0.268003724035092,
25.5300810447489));
#42239=CARTESIAN_POINT('Ctrl Pts',(19.7211795649519,-0.103551752465798,
25.5128304221262));
#42240=CARTESIAN_POINT('Ctrl Pts',(19.7317887678502,0.060900219103496,25.4955797995036));
#42241=CARTESIAN_POINT('Ctrl Pts',(19.7423979707484,0.229756510009277,25.5203160091333));
#42242=CARTESIAN_POINT('Ctrl Pts',(19.7530071736467,0.382350463488992,25.5840115371971));
#42243=CARTESIAN_POINT('Ctrl Pts',(19.763616376545,0.534944416968706,25.6477070652609));
#42244=CARTESIAN_POINT('Ctrl Pts',(19.7742255794432,0.671276033022354,25.7503619117588));
#42245=CARTESIAN_POINT('Ctrl Pts',(19.7848347823415,0.774659414430762,25.8794119461736));
#42246=CARTESIAN_POINT('Ctrl Pts',(19.7954439852398,0.87804279583917,26.0084619805884));
#42247=CARTESIAN_POINT('Ctrl Pts',(19.8060531881381,0.948477942602338,26.1639072029201));
#42248=CARTESIAN_POINT('Ctrl Pts',(19.8166623910364,0.977344157236233,26.3267223637209));
#42249=CARTESIAN_POINT('Ctrl Pts',(19.8272715939346,1.00621037187013,26.4895375245218));
#42250=CARTESIAN_POINT('Ctrl Pts',(19.8378807968329,0.993507654374749,26.6597226237918));
#42251=CARTESIAN_POINT('Ctrl Pts',(19.8484899997312,0.940790715569691,26.8164483692739));
#42252=CARTESIAN_POINT('Ctrl Pts',(19.8590992026294,0.888073776764639,26.973174114756));
#42253=CARTESIAN_POINT('Ctrl Pts',(19.8697084055277,0.795342616649919,27.1164405064502));
#42254=CARTESIAN_POINT('Ctrl Pts',(19.880317608426,0.67394678605958,27.2287128861755));
#42255=CARTESIAN_POINT('Ctrl Pts',(19.8909268113243,0.552550955469226,27.3409852659008));
#42256=CARTESIAN_POINT('Ctrl Pts',(19.9015360142225,0.402490454403247,27.4222636336571));
#42257=CARTESIAN_POINT('Ctrl Pts',(19.9121452171208,0.242131485580603,27.4626001686104));
#42258=CARTESIAN_POINT('Ctrl Pts',(19.9227544200191,0.08177251675796,27.5029367035637));
#42259=CARTESIAN_POINT('Ctrl Pts',(19.9333636229173,-0.0888849198213473,
27.5023314057139));
#42260=CARTESIAN_POINT('Ctrl Pts',(19.9439728258156,-0.248953721599025,
27.460858358667));
#42261=CARTESIAN_POINT('Ctrl Pts',(19.9545820287139,-0.409022523376694,
27.4193853116201));
#42262=CARTESIAN_POINT('Ctrl Pts',(19.9651912316122,-0.558502690352734,
27.3370445153759));
#42263=CARTESIAN_POINT('Ctrl Pts',(19.9758004345104,-0.679099048049894,
27.2239138235011));
#42264=CARTESIAN_POINT('Ctrl Pts',(19.9864096374087,-0.799695405747047,
27.1107831316263));
#42265=CARTESIAN_POINT('Ctrl Pts',(19.997018840307,-0.891407954165323,26.9668625441208));
#42266=CARTESIAN_POINT('Ctrl Pts',(20.0076280432052,-0.943011812378983,
26.8097667874901));
#42267=CARTESIAN_POINT('Ctrl Pts',(20.0143631029248,-0.975771584263756,
26.7100374003971));
#42268=CARTESIAN_POINT('Ctrl Pts',(20.0210981626443,-0.992367094517968,
26.6049982692141));
#42269=CARTESIAN_POINT('Ctrl Pts',(20.0278332223638,-0.992438391306935,
26.4999811413391));
#42270=CARTESIAN_POINT('Origin',(18.,0.,26.5));
#42271=CARTESIAN_POINT('',(20.5721667776362,-0.9925,26.5));
#42272=CARTESIAN_POINT('',(20.4278332223638,-0.992514693241506,26.5000253500233));
#42273=CARTESIAN_POINT('',(18.,-0.9925,26.5));
#42274=CARTESIAN_POINT('Ctrl Pts',(20.5721667776362,-0.9925,26.5000000000001));
#42275=CARTESIAN_POINT('Ctrl Pts',(20.5554259338597,-0.99249999999998,26.760992324923));
#42276=CARTESIAN_POINT('Ctrl Pts',(20.5386850900831,-0.884539443097369,
27.0203491301748));
#42277=CARTESIAN_POINT('Ctrl Pts',(20.5219442463066,-0.699346033936857,
27.2042523516587));
#42278=CARTESIAN_POINT('Ctrl Pts',(20.5052034025301,-0.514152624776344,
27.3881555731426));
#42279=CARTESIAN_POINT('Ctrl Pts',(20.4884625587535,-0.25404740834438,27.4943003359057));
#42280=CARTESIAN_POINT('Ctrl Pts',(20.471721714977,0.00693853867355432,
27.4924757461425));
#42281=CARTESIAN_POINT('Ctrl Pts',(20.4549808712005,0.267924485691489,27.4906511563793));
#42282=CARTESIAN_POINT('Ctrl Pts',(20.4382400274239,0.526520203888113,27.3808800818308));
#42283=CARTESIAN_POINT('Ctrl Pts',(20.4214991836474,0.709124249559362,27.1944055361868));
#42284=CARTESIAN_POINT('Ctrl Pts',(20.4047583398709,0.89172829523061,27.0079309905428));
#42285=CARTESIAN_POINT('Ctrl Pts',(20.3880174960943,0.996052076106205,26.7470900753838));
#42286=CARTESIAN_POINT('Ctrl Pts',(20.3712766523178,0.992402985755317,26.486123261769));
#42287=CARTESIAN_POINT('Ctrl Pts',(20.3545358085413,0.98875389540443,26.2251564481542));
#42288=CARTESIAN_POINT('Ctrl Pts',(20.3377949647647,0.877177668191485,25.9673344556902));
#42289=CARTESIAN_POINT('Ctrl Pts',(20.3210541209882,0.689431099871631,25.7860385104715));
#42290=CARTESIAN_POINT('Ctrl Pts',(20.3043132772117,0.501684531551776,25.6047425652527));
#42291=CARTESIAN_POINT('Ctrl Pts',(20.2875724334351,0.240120666075644,25.5022448650134));
#42292=CARTESIAN_POINT('Ctrl Pts',(20.2708315896586,-0.0208142595729757,
25.5077182776054));
#42293=CARTESIAN_POINT('Ctrl Pts',(20.2540907458821,-0.281749185221595,
25.5131916901973));
#42294=CARTESIAN_POINT('Ctrl Pts',(20.2373499021055,-0.538784851090647,
25.6265676168679));
#42295=CARTESIAN_POINT('Ctrl Pts',(20.220609058329,-0.718763835149603,25.8155770318867));
#42296=CARTESIAN_POINT('Ctrl Pts',(20.2044616314314,-0.892363059118839,
25.9978865828696));
#42297=CARTESIAN_POINT('Ctrl Pts',(20.1883142045338,-0.992500000000014,
26.248259135335));
#42298=CARTESIAN_POINT('Ctrl Pts',(20.1721667776362,-0.9925,26.5000000000001));
#42299=CARTESIAN_POINT('Ctrl Pts',(20.0278332223638,-0.992438391306935,
26.4999811413391));
#42300=CARTESIAN_POINT('Ctrl Pts',(20.0317073655426,-0.992479402668399,
26.4395731558791));
#42301=CARTESIAN_POINT('Ctrl Pts',(20.0355815087213,-0.987052908523862,
26.3791724508387));
#42302=CARTESIAN_POINT('Ctrl Pts',(20.0394556519001,-0.97609039996612,26.3197938069537));
#42303=CARTESIAN_POINT('Ctrl Pts',(20.0500648547983,-0.946069961330555,
26.1571875088038));
#42304=CARTESIAN_POINT('Ctrl Pts',(20.0606740576966,-0.874533916050388,
26.0022458382598));
#42305=CARTESIAN_POINT('Ctrl Pts',(20.0712832605949,-0.77023770276533,25.8739324140662));
#42306=CARTESIAN_POINT('Ctrl Pts',(20.0818924634931,-0.66594148948026,25.7456189898725));
#42307=CARTESIAN_POINT('Ctrl Pts',(20.0925016663914,-0.528885108190297,
25.6439338120293));
#42308=CARTESIAN_POINT('Ctrl Pts',(20.1031108692897,-0.375843161571139,
25.5813223313814));
#42309=CARTESIAN_POINT('Ctrl Pts',(20.113720072188,-0.222801214951989,25.5187108507335));
#42310=CARTESIAN_POINT('Ctrl Pts',(20.1243292750862,-0.0537737030036256,
25.495173067281));
#42311=CARTESIAN_POINT('Ctrl Pts',(20.1349384779845,0.110551761427937,25.5135898170825));
#42312=CARTESIAN_POINT('Ctrl Pts',(20.1455476808828,0.27487722585949,25.5320065668839));
#42313=CARTESIAN_POINT('Ctrl Pts',(20.1561568837811,0.434500642774264,25.5923778499392));
#42314=CARTESIAN_POINT('Ctrl Pts',(20.1667660866793,0.569885385192319,25.6873147050288));
#42315=CARTESIAN_POINT('Ctrl Pts',(20.1773752895776,0.705270127610389,25.7822515601183));
#42316=CARTESIAN_POINT('Ctrl Pts',(20.1879844924759,0.816416195531731,25.911753987242));
#42317=CARTESIAN_POINT('Ctrl Pts',(20.1985936953741,0.889720200987109,26.0599719271754));
#42318=CARTESIAN_POINT('Ctrl Pts',(20.2092028982724,0.963024206442483,26.2081898671088));
#42319=CARTESIAN_POINT('Ctrl Pts',(20.2198121011707,0.998486149431895,26.3751233198519));
#42320=CARTESIAN_POINT('Ctrl Pts',(20.230421304069,0.991765772331754,26.5403409686232));
#42321=CARTESIAN_POINT('Ctrl Pts',(20.2410305069672,0.985045395231612,26.7055586173945));
#42322=CARTESIAN_POINT('Ctrl Pts',(20.2516397098655,0.936142698041916,26.8690604621941));
#42323=CARTESIAN_POINT('Ctrl Pts',(20.2622489127638,0.851042978983781,27.0108351875514));
#42324=CARTESIAN_POINT('Ctrl Pts',(20.272858115662,0.765943259925651,27.1526099129086));
#42325=CARTESIAN_POINT('Ctrl Pts',(20.2834673185603,0.644646518999089,27.2726575188235));
#42326=CARTESIAN_POINT('Ctrl Pts',(20.2940765214586,0.501998505199868,27.3562851404149));
#42327=CARTESIAN_POINT('Ctrl Pts',(20.3046857243569,0.359350491400631,27.4399127620063));
#42328=CARTESIAN_POINT('Ctrl Pts',(20.3152949272551,0.195351204728735,27.4871203992742));
#42329=CARTESIAN_POINT('Ctrl Pts',(20.3259041301534,0.0300728435533973,
27.4921302157474));
#42330=CARTESIAN_POINT('Ctrl Pts',(20.3365133330517,-0.135205517621921,
27.4971400322205));
#42331=CARTESIAN_POINT('Ctrl Pts',(20.34712253595,-0.301762953300702,27.459952027899));
#42332=CARTESIAN_POINT('Ctrl Pts',(20.3577317388482,-0.449214168176698,
27.3851177164804));
#42333=CARTESIAN_POINT('Ctrl Pts',(20.3683409417465,-0.596665383052711,
27.3102834050619));
#42334=CARTESIAN_POINT('Ctrl Pts',(20.3789501446448,-0.725010377125957,
27.1978027865463));
#42335=CARTESIAN_POINT('Ctrl Pts',(20.3895593475431,-0.818540751701458,
27.0614425872004));
#42336=CARTESIAN_POINT('Ctrl Pts',(20.4001685504413,-0.912071126276949,
26.9250823878545));
#42337=CARTESIAN_POINT('Ctrl Pts',(20.4107777533396,-0.9707868813547,26.7648426076782));
#42338=CARTESIAN_POINT('Ctrl Pts',(20.4213869562379,-0.987501679071689,
26.600335311575));
#42339=CARTESIAN_POINT('Ctrl Pts',(20.4235357116132,-0.99088704287197,26.5670165090062));
#42340=CARTESIAN_POINT('Ctrl Pts',(20.4256844669885,-0.99254947667873,26.5335226477804));
#42341=CARTESIAN_POINT('Ctrl Pts',(20.4278332223638,-0.992514693241506,
26.5000253500233));
#42342=CARTESIAN_POINT('Origin',(18.,0.,26.5));
#42343=CARTESIAN_POINT('',(20.9721667776362,-0.9925,26.5000000000001));
#42344=CARTESIAN_POINT('',(20.8278332223638,-0.992500311415872,26.4999739716271));
#42345=CARTESIAN_POINT('',(18.,-0.9925,26.5));
#42346=CARTESIAN_POINT('Ctrl Pts',(20.9721667776362,-0.9925,26.5000000000001));
#42347=CARTESIAN_POINT('Ctrl Pts',(20.9554259338597,-0.992499999999982,
26.760992324923));
#42348=CARTESIAN_POINT('Ctrl Pts',(20.9386850900831,-0.884539443097373,
27.0203491301748));
#42349=CARTESIAN_POINT('Ctrl Pts',(20.9219442463066,-0.699346033936861,
27.2042523516587));
#42350=CARTESIAN_POINT('Ctrl Pts',(20.9052034025301,-0.51415262477635,27.3881555731426));
#42351=CARTESIAN_POINT('Ctrl Pts',(20.8884625587535,-0.254047408344387,
27.4943003359057));
#42352=CARTESIAN_POINT('Ctrl Pts',(20.871721714977,0.00693853867354749,
27.4924757461425));
#42353=CARTESIAN_POINT('Ctrl Pts',(20.8549808712005,0.267924485691482,27.4906511563793));
#42354=CARTESIAN_POINT('Ctrl Pts',(20.8382400274239,0.526520203888107,27.3808800818308));
#42355=CARTESIAN_POINT('Ctrl Pts',(20.8214991836474,0.709124249559357,27.1944055361868));
#42356=CARTESIAN_POINT('Ctrl Pts',(20.8047583398709,0.891728295230606,27.0079309905428));
#42357=CARTESIAN_POINT('Ctrl Pts',(20.7880174960943,0.996052076106204,26.7470900753838));
#42358=CARTESIAN_POINT('Ctrl Pts',(20.7712766523178,0.992402985755318,26.486123261769));
#42359=CARTESIAN_POINT('Ctrl Pts',(20.7545358085413,0.988753895404431,26.2251564481542));
#42360=CARTESIAN_POINT('Ctrl Pts',(20.7377949647647,0.877177668191489,25.9673344556903));
#42361=CARTESIAN_POINT('Ctrl Pts',(20.7210541209882,0.689431099871636,25.7860385104715));
#42362=CARTESIAN_POINT('Ctrl Pts',(20.7043132772117,0.501684531551782,25.6047425652527));
#42363=CARTESIAN_POINT('Ctrl Pts',(20.6875724334351,0.240120666075651,25.5022448650134));
#42364=CARTESIAN_POINT('Ctrl Pts',(20.6708315896586,-0.020814259572969,
25.5077182776054));
#42365=CARTESIAN_POINT('Ctrl Pts',(20.6540907458821,-0.281749185221589,
25.5131916901973));
#42366=CARTESIAN_POINT('Ctrl Pts',(20.6373499021055,-0.538784851090641,
25.6265676168679));
#42367=CARTESIAN_POINT('Ctrl Pts',(20.620609058329,-0.718763835149599,25.8155770318867));
#42368=CARTESIAN_POINT('Ctrl Pts',(20.6044616314314,-0.892363059118843,
25.9978865828696));
#42369=CARTESIAN_POINT('Ctrl Pts',(20.5883142045338,-0.99250000000002,26.248259135335));
#42370=CARTESIAN_POINT('Ctrl Pts',(20.5721667776362,-0.9925,26.5000000000001));
#42371=CARTESIAN_POINT('Ctrl Pts',(20.4278332223638,-0.992514693241506,
26.5000253500233));
#42372=CARTESIAN_POINT('Ctrl Pts',(20.4362936698868,-0.992377737937666,
26.368134054676));
#42373=CARTESIAN_POINT('Ctrl Pts',(20.4447541174097,-0.965929007104012,
26.2361894831557));
#42374=CARTESIAN_POINT('Ctrl Pts',(20.4532145649327,-0.914738023432971,
26.114667559886));
#42375=CARTESIAN_POINT('Ctrl Pts',(20.463823767831,-0.850545729721046,25.9622819163303));
#42376=CARTESIAN_POINT('Ctrl Pts',(20.4744329707292,-0.747447301940976,
25.8262854412488));
#42377=CARTESIAN_POINT('Ctrl Pts',(20.4850421736275,-0.618061161403927,
25.7233230132917));
#42378=CARTESIAN_POINT('Ctrl Pts',(20.4956513765258,-0.488675020866886,
25.6203605853346));
#42379=CARTESIAN_POINT('Ctrl Pts',(20.5062605794241,-0.333001167572864,
25.5504322045018));
#42380=CARTESIAN_POINT('Ctrl Pts',(20.5168697823223,-0.170092833567137,
25.5220965441889));
#42381=CARTESIAN_POINT('Ctrl Pts',(20.5274789852206,-0.00718449956139197,
25.4937608838759));
#42382=CARTESIAN_POINT('Ctrl Pts',(20.5380881881189,0.16295831515607,25.5070179440828));
#42383=CARTESIAN_POINT('Ctrl Pts',(20.5486973910171,0.319511493618563,25.5602451668845));
#42384=CARTESIAN_POINT('Ctrl Pts',(20.5593065939154,0.476064672081055,25.6134723896863));
#42385=CARTESIAN_POINT('Ctrl Pts',(20.5699157968137,0.619028214288567,25.706669775083));
#42386=CARTESIAN_POINT('Ctrl Pts',(20.580524999712,0.730904528410161,25.8284307100025));
#42387=CARTESIAN_POINT('Ctrl Pts',(20.5911342026102,0.842780842531747,25.9501916449219));
#42388=CARTESIAN_POINT('Ctrl Pts',(20.6017434055085,0.9235699285674,26.1005161293642));
#42389=CARTESIAN_POINT('Ctrl Pts',(20.6123526084068,0.96338384984444,26.2610056511606));
#42390=CARTESIAN_POINT('Ctrl Pts',(20.622961811305,1.00319777112148,26.421495172957));
#42391=CARTESIAN_POINT('Ctrl Pts',(20.6335710142033,1.00203652763991,26.5921497321076));
#42392=CARTESIAN_POINT('Ctrl Pts',(20.6441802171016,0.960042246295454,26.7520825782283));
#42393=CARTESIAN_POINT('Ctrl Pts',(20.6547894199999,0.918047964951002,26.912015424349));
#42394=CARTESIAN_POINT('Ctrl Pts',(20.6653986228981,0.835220645743676,27.0612265574397));
#42395=CARTESIAN_POINT('Ctrl Pts',(20.6760078257964,0.721697688751602,27.1814537306148));
#42396=CARTESIAN_POINT('Ctrl Pts',(20.6866170286947,0.608174731759521,27.3016809037899));
#42397=CARTESIAN_POINT('Ctrl Pts',(20.697226231593,0.463956136982686,27.3929241170493));
#42398=CARTESIAN_POINT('Ctrl Pts',(20.7078354344912,0.306693104628343,27.4440159323294));
#42399=CARTESIAN_POINT('Ctrl Pts',(20.7184446373895,0.149430072273992,27.4951077476095));
#42400=CARTESIAN_POINT('Ctrl Pts',(20.7290538402878,-0.0208773976578456,
27.5060481649102));
#42401=CARTESIAN_POINT('Ctrl Pts',(20.739663043186,-0.183385035721877,27.4754981648325));
#42402=CARTESIAN_POINT('Ctrl Pts',(20.7502722460843,-0.3458926737859,27.4449481647547));
#42403=CARTESIAN_POINT('Ctrl Pts',(20.7608814489826,-0.500600479982099,
27.3729077472986));
#42404=CARTESIAN_POINT('Ctrl Pts',(20.7714906518809,-0.628573458687896,
27.2681940822158));
#42405=CARTESIAN_POINT('Ctrl Pts',(20.7820998547791,-0.756546437393693,
27.1634804171331));
#42406=CARTESIAN_POINT('Ctrl Pts',(20.7927090576774,-0.857784588609095,
27.0260935044238));
#42407=CARTESIAN_POINT('Ctrl Pts',(20.8033182605757,-0.919897173965862,
26.8728484011604));
#42408=CARTESIAN_POINT('Ctrl Pts',(20.811489914505,-0.967738897520507,26.7548125824239));
#42409=CARTESIAN_POINT('Ctrl Pts',(20.8196615684344,-0.992368487932995,
26.6273685309256));
#42410=CARTESIAN_POINT('Ctrl Pts',(20.8278332223638,-0.992500311415872,
26.4999739716271));
#42411=CARTESIAN_POINT('Origin',(18.,0.,26.5));
#42412=CARTESIAN_POINT('',(21.3721667776362,-0.992404881561636,26.5000957579287));
#42413=CARTESIAN_POINT('',(21.2278332223638,-0.992448585256559,26.5000215597106));
#42414=CARTESIAN_POINT('',(18.,-0.9925,26.5));
#42415=CARTESIAN_POINT('Ctrl Pts',(21.3721667776362,-0.992404881561636,
26.5000957579287));
#42416=CARTESIAN_POINT('Ctrl Pts',(21.3655528552044,-0.99229338944025,26.6034157298074));
#42417=CARTESIAN_POINT('Ctrl Pts',(21.3589389327725,-0.976255401996959,
26.706744520868));
#42418=CARTESIAN_POINT('Ctrl Pts',(21.3523250103407,-0.944684059200136,
26.8047056191727));
#42419=CARTESIAN_POINT('Ctrl Pts',(21.3417394748401,-0.894154351085294,
26.9614916556679));
#42420=CARTESIAN_POINT('Ctrl Pts',(21.3311539393396,-0.803834751993709,
27.1045279320697));
#42421=CARTESIAN_POINT('Ctrl Pts',(21.3205684038391,-0.684188391208178,
27.2185914249928));
#42422=CARTESIAN_POINT('Ctrl Pts',(21.3099828683386,-0.564542030422647,
27.3326549179159));
#42423=CARTESIAN_POINT('Ctrl Pts',(21.299397332838,-0.415568907943175,27.4177456273603));
#42424=CARTESIAN_POINT('Ctrl Pts',(21.2888117973375,-0.256291739646409,
27.4599660179157));
#42425=CARTESIAN_POINT('Ctrl Pts',(21.2676407263364,0.0622625969471221,
27.5444067990263));
#42426=CARTESIAN_POINT('Ctrl Pts',(21.2464696553354,0.422033116809841,27.4573663045809));
#42427=CARTESIAN_POINT('Ctrl Pts',(21.2252985843343,0.666759555135708,27.2366491071053));
#42428=CARTESIAN_POINT('Ctrl Pts',(21.2147130488338,0.789122774298649,27.1262905083675));
#42429=CARTESIAN_POINT('Ctrl Pts',(21.2041275133332,0.882724973077366,26.9825127338723));
#42430=CARTESIAN_POINT('Ctrl Pts',(21.1935419778327,0.936999885799728,26.826371881063));
#42431=CARTESIAN_POINT('Ctrl Pts',(21.1829564423322,0.991274798522085,26.6702310282536));
#42432=CARTESIAN_POINT('Ctrl Pts',(21.1723709068316,1.00622242518808,26.5017270971303));
#42433=CARTESIAN_POINT('Ctrl Pts',(21.1617853713311,0.979495373543125,26.3391824037305));
#42434=CARTESIAN_POINT('Ctrl Pts',(21.1511998358306,0.952768321898173,26.1766377103308));
#42435=CARTESIAN_POINT('Ctrl Pts',(21.14061430033,0.884366591942281,26.0200522546547));
#42436=CARTESIAN_POINT('Ctrl Pts',(21.1300287648295,0.782932539033663,25.8897676576329));
#42437=CARTESIAN_POINT('Ctrl Pts',(21.119443229329,0.681498486125039,25.7594830606111));
#42438=CARTESIAN_POINT('Ctrl Pts',(21.1088576938284,0.54703211026369,25.6554993222437));
#42439=CARTESIAN_POINT('Ctrl Pts',(21.0982721583279,0.395737200458154,25.5897973573186));
#42440=CARTESIAN_POINT('Ctrl Pts',(21.0876866228274,0.244442290652617,25.5240953923935));
#42441=CARTESIAN_POINT('Ctrl Pts',(21.0771010873268,0.0763188469028976,
25.4966752009106));
#42442=CARTESIAN_POINT('Ctrl Pts',(21.0665155518263,-0.0880174092237496,
25.5112681203385));
#42443=CARTESIAN_POINT('Ctrl Pts',(21.0559300163258,-0.252353665350397,
25.5258610397663));
#42444=CARTESIAN_POINT('Ctrl Pts',(21.0453444808252,-0.412902733853967,
25.5824670701049));
#42445=CARTESIAN_POINT('Ctrl Pts',(21.0347589453247,-0.550228722711753,
25.673938060106));
#42446=CARTESIAN_POINT('Ctrl Pts',(21.0241734098242,-0.687554711569525,
25.7654090501072));
#42447=CARTESIAN_POINT('Ctrl Pts',(21.0135878743236,-0.801657620781514,
25.8917449997708));
#42448=CARTESIAN_POINT('Ctrl Pts',(21.0030023388231,-0.878451612019513,
26.0377656876369));
#42449=CARTESIAN_POINT('Ctrl Pts',(20.9927238184275,-0.953018326680525,
26.1795512986096));
#42450=CARTESIAN_POINT('Ctrl Pts',(20.9824452980318,-0.992408900464791,
26.3398963629713));
#42451=CARTESIAN_POINT('Ctrl Pts',(20.9721667776362,-0.992502482922401,
26.5000686713788));
#42452=CARTESIAN_POINT('Ctrl Pts',(20.8278332223638,-0.992500311415872,
26.4999739716271));
#42453=CARTESIAN_POINT('Ctrl Pts',(20.8302707713327,-0.992539633467141,
26.4619730382366));
#42454=CARTESIAN_POINT('Ctrl Pts',(20.8327083203016,-0.990399172499557,
26.4239765086048));
#42455=CARTESIAN_POINT('Ctrl Pts',(20.8351458692705,-0.986044805495746,
26.3862354076476));
#42456=CARTESIAN_POINT('Ctrl Pts',(20.8457550721688,-0.96709283217073,26.2219708112155));
#42457=CARTESIAN_POINT('Ctrl Pts',(20.856364275067,-0.906201866022573,26.0625449121689));
#42458=CARTESIAN_POINT('Ctrl Pts',(20.8669734779653,-0.810824473316787,
25.9274701628834));
#42459=CARTESIAN_POINT('Ctrl Pts',(20.8775826808636,-0.71544708061099,25.7923954135978));
#42460=CARTESIAN_POINT('Ctrl Pts',(20.8881918837618,-0.585583261347557,
25.6816718140735));
#42461=CARTESIAN_POINT('Ctrl Pts',(20.8988010866601,-0.437127306252613,
25.6088510455336));
#42462=CARTESIAN_POINT('Ctrl Pts',(20.9094102895584,-0.288671351157678,
25.5360302769936));
#42463=CARTESIAN_POINT('Ctrl Pts',(20.9200194924567,-0.121623260231236,
25.5011123394381));
#42464=CARTESIAN_POINT('Ctrl Pts',(20.930628695355,0.0435716189503967,25.5083709085851));
#42465=CARTESIAN_POINT('Ctrl Pts',(20.9412378982532,0.208766498132029,25.5156294777322));
#42466=CARTESIAN_POINT('Ctrl Pts',(20.9518471011515,0.372108165568853,25.5650645535818));
#42467=CARTESIAN_POINT('Ctrl Pts',(20.9624563040498,0.513604910215741,25.6506256790316));
#42468=CARTESIAN_POINT('Ctrl Pts',(20.973065506948,0.655101654862629,25.7361868044813));
#42469=CARTESIAN_POINT('Ctrl Pts',(20.9836747098463,0.774753476719582,25.8578739795312));
#42470=CARTESIAN_POINT('Ctrl Pts',(20.9942839127446,0.857915951702268,26.0007936691777));
#42471=CARTESIAN_POINT('Ctrl Pts',(21.0048931156429,0.941078426684954,26.1437133588242));
#42472=CARTESIAN_POINT('Ctrl Pts',(21.0155023185411,0.987751554793373,26.3078655630673));
#42473=CARTESIAN_POINT('Ctrl Pts',(21.0261115214394,0.992222919193793,26.4731593676527));
#42474=CARTESIAN_POINT('Ctrl Pts',(21.0367207243377,0.996694283594215,26.638453172238));
#42475=CARTESIAN_POINT('Ctrl Pts',(21.047329927236,0.958963884286633,26.8048885771656));
#42476=CARTESIAN_POINT('Ctrl Pts',(21.0579391301342,0.883649619768174,26.9520952227151));
#42477=CARTESIAN_POINT('Ctrl Pts',(21.0685483330325,0.808335355249724,27.0993018682646));
#42478=CARTESIAN_POINT('Ctrl Pts',(21.0791575359308,0.695437225520406,27.2272797544361));
#42479=CARTESIAN_POINT('Ctrl Pts',(21.089766738829,0.558773056873417,27.3203654135997));
#42480=CARTESIAN_POINT('Ctrl Pts',(21.1003759417273,0.422108888226428,27.4134510727633));
#42481=CARTESIAN_POINT('Ctrl Pts',(21.1109851446256,0.261678680661741,27.471644504919));
#42482=CARTESIAN_POINT('Ctrl Pts',(21.1215943475238,0.0971178058691354,
27.4878233003434));
#42483=CARTESIAN_POINT('Ctrl Pts',(21.1322035504221,-0.0674430689234892,
27.5040020957679));
#42484=CARTESIAN_POINT('Ctrl Pts',(21.1428127533204,-0.236134610944028,
27.4781662544611));
#42485=CARTESIAN_POINT('Ctrl Pts',(21.1534219562187,-0.38831032737321,27.413477876346));
#42486=CARTESIAN_POINT('Ctrl Pts',(21.1640311591169,-0.5404860438024,27.3487894982309));
#42487=CARTESIAN_POINT('Ctrl Pts',(21.1746403620152,-0.676145934640202,
27.2452485833074));
#42488=CARTESIAN_POINT('Ctrl Pts',(21.1852495649135,-0.778686316450531,
27.1155277097669));
#42489=CARTESIAN_POINT('Ctrl Pts',(21.1958587678118,-0.881226698260843,
26.9858068362265));
#42490=CARTESIAN_POINT('Ctrl Pts',(21.20646797071,-0.950647571043694,26.8299060040692));
#42491=CARTESIAN_POINT('Ctrl Pts',(21.2170771736083,-0.978452376321672,
26.6669062257339));
#42492=CARTESIAN_POINT('Ctrl Pts',(21.2206625231935,-0.987848930240464,
26.6118209197745));
#42493=CARTESIAN_POINT('Ctrl Pts',(21.2242478727786,-0.992492585617876,
26.5559248555442));
#42494=CARTESIAN_POINT('Ctrl Pts',(21.2278332223638,-0.992448585256559,
26.5000215597106));
#42495=CARTESIAN_POINT('Origin',(18.,0.,26.5));
#42496=CARTESIAN_POINT('',(21.7721667776362,-0.992176529618623,26.499357490987));
#42497=CARTESIAN_POINT('',(21.6278332223638,-0.992566083749324,26.4999845389628));
#42498=CARTESIAN_POINT('',(18.,-0.9925,26.5));
#42499=CARTESIAN_POINT('Ctrl Pts',(21.7721667776362,-0.992176529618623,
26.499357490987));
#42500=CARTESIAN_POINT('Ctrl Pts',(21.7698314833779,-0.992196569891483,
26.5357287700307));
#42501=CARTESIAN_POINT('Ctrl Pts',(21.7674961891197,-0.990235918585997,
26.5721393492544));
#42502=CARTESIAN_POINT('Ctrl Pts',(21.7651608948614,-0.986275112555324,
26.6083918497455));
#42503=CARTESIAN_POINT('Ctrl Pts',(21.7545753593609,-0.968321378159688,
26.772718948814));
#42504=CARTESIAN_POINT('Ctrl Pts',(21.7439898238604,-0.909271030322288,
26.9337980488715));
#42505=CARTESIAN_POINT('Ctrl Pts',(21.7334042883598,-0.814709943053242,
27.0687424021946));
#42506=CARTESIAN_POINT('Ctrl Pts',(21.7122332173588,-0.62558776851514,27.3386311088407));
#42507=CARTESIAN_POINT('Ctrl Pts',(21.6910621463577,-0.294422636250437,
27.5039808285492));
#42508=CARTESIAN_POINT('Ctrl Pts',(21.6698910753566,0.0349494571674246,
27.4929746959553));
#42509=CARTESIAN_POINT('Ctrl Pts',(21.6593055398561,0.199635503876346,27.4874716296583));
#42510=CARTESIAN_POINT('Ctrl Pts',(21.6487200043556,0.363873290873557,27.4378796002858));
#42511=CARTESIAN_POINT('Ctrl Pts',(21.6381344688551,0.506012333303722,27.353486326359));
#42512=CARTESIAN_POINT('Ctrl Pts',(21.6275489333545,0.648151375733887,27.2690930524323));
#42513=CARTESIAN_POINT('Ctrl Pts',(21.616963397854,0.768191673597007,27.1498985339513));
#42514=CARTESIAN_POINT('Ctrl Pts',(21.6063778623534,0.85252856782575,27.0083980006877));
#42515=CARTESIAN_POINT('Ctrl Pts',(21.5957923268529,0.936865462054492,26.866897467424));
#42516=CARTESIAN_POINT('Ctrl Pts',(21.5852067913524,0.985498952648858,26.7030909193777));
#42517=CARTESIAN_POINT('Ctrl Pts',(21.5746212558519,0.9919249873757,26.5381010730589));
#42518=CARTESIAN_POINT('Ctrl Pts',(21.5640357203513,0.998351022102542,26.3731112267402));
#42519=CARTESIAN_POINT('Ctrl Pts',(21.5534501848508,0.962569600961857,26.2069380821491));
#42520=CARTESIAN_POINT('Ctrl Pts',(21.5428646493503,0.889246785300691,26.0591860512608));
#42521=CARTESIAN_POINT('Ctrl Pts',(21.5322791138497,0.815923969639525,25.9114340203725));
#42522=CARTESIAN_POINT('Ctrl Pts',(21.5216935783492,0.705059759457878,25.7821031031871));
#42523=CARTESIAN_POINT('Ctrl Pts',(21.5111080428487,0.570010756288525,25.6873343049563));
#42524=CARTESIAN_POINT('Ctrl Pts',(21.5005225073481,0.434961753119187,25.5925655067255));
#42525=CARTESIAN_POINT('Ctrl Pts',(21.4899369718476,0.275727956962149,25.5323588274492));
#42526=CARTESIAN_POINT('Ctrl Pts',(21.4793514363471,0.111776496367536,25.5137769062234));
#42527=CARTESIAN_POINT('Ctrl Pts',(21.4687659008465,-0.0521749642271047,
25.4951949849977));
#42528=CARTESIAN_POINT('Ctrl Pts',(21.458180365346,-0.220844089259322,25.5182378218223));
#42529=CARTESIAN_POINT('Ctrl Pts',(21.4475948298455,-0.373676910774448,
25.580378686339));
#42530=CARTESIAN_POINT('Ctrl Pts',(21.4370092943449,-0.526509732289548,
25.6425195508557));
#42531=CARTESIAN_POINT('Ctrl Pts',(21.4264237588444,-0.663506250287563,
25.7437584430643));
#42532=CARTESIAN_POINT('Ctrl Pts',(21.4158382233439,-0.768036281504167,
25.8713529982065));
#42533=CARTESIAN_POINT('Ctrl Pts',(21.4052526878434,-0.872566312720771,
25.9989475533487));
#42534=CARTESIAN_POINT('Ctrl Pts',(21.3946671523428,-0.944629857155963,
26.1528977714245));
#42535=CARTESIAN_POINT('Ctrl Pts',(21.3840816168423,-0.975291720804518,
26.3151407787567));
#42536=CARTESIAN_POINT('Ctrl Pts',(21.3801100037736,-0.98679582075023,26.376013131241));
#42537=CARTESIAN_POINT('Ctrl Pts',(21.3761383907049,-0.992471831782313,
26.4380528545232));
#42538=CARTESIAN_POINT('Ctrl Pts',(21.3721667776362,-0.992404881561636,
26.5000957579287));
#42539=CARTESIAN_POINT('Ctrl Pts',(21.2278332223638,-0.992448585256559,
26.5000215597106));
#42540=CARTESIAN_POINT('Ctrl Pts',(21.2348570756769,-0.992362386665246,
26.3905046101561));
#42541=CARTESIAN_POINT('Ctrl Pts',(21.24188092899,-0.974285674510598,26.2809599068025));
#42542=CARTESIAN_POINT('Ctrl Pts',(21.2489047823031,-0.938708977451642,
26.1774287728734));
#42543=CARTESIAN_POINT('Ctrl Pts',(21.2595139852014,-0.884972035530529,
26.0210498228614));
#42544=CARTESIAN_POINT('Ctrl Pts',(21.2701231880997,-0.791309413915201,
25.8783906473505));
#42545=CARTESIAN_POINT('Ctrl Pts',(21.2807323909979,-0.669184666862485,
25.7669115861273));
#42546=CARTESIAN_POINT('Ctrl Pts',(21.2913415938962,-0.547059919809769,
25.6554325249041));
#42547=CARTESIAN_POINT('Ctrl Pts',(21.3019507967945,-0.396473047319665,
25.5751335779686));
#42548=CARTESIAN_POINT('Ctrl Pts',(21.3125599996928,-0.235854675755011,
25.5358426928956));
#42549=CARTESIAN_POINT('Ctrl Pts',(21.323169202591,-0.075236304190348,25.4965518078227));
#42550=CARTESIAN_POINT('Ctrl Pts',(21.3337784054893,0.0954135664488655,
25.4982689846123));
#42551=CARTESIAN_POINT('Ctrl Pts',(21.3443876083876,0.255208759614769,25.5407840545872));
#42552=CARTESIAN_POINT('Ctrl Pts',(21.3549968112858,0.415003952780655,25.5832991245621));
#42553=CARTESIAN_POINT('Ctrl Pts',(21.3656060141841,0.563944468473233,25.6666120877223));
#42554=CARTESIAN_POINT('Ctrl Pts',(21.3762152170824,0.683801181207488,25.7805261050618));
#42555=CARTESIAN_POINT('Ctrl Pts',(21.3868244199807,0.803657893941749,25.8944401224014));
#42556=CARTESIAN_POINT('Ctrl Pts',(21.3974336228789,0.894430803717683,26.0389551939203));
#42557=CARTESIAN_POINT('Ctrl Pts',(21.4080428257772,0.945010033848943,26.1963838330341));
#42558=CARTESIAN_POINT('Ctrl Pts',(21.4186520286755,0.995589263980203,26.3538124721479));
#42559=CARTESIAN_POINT('Ctrl Pts',(21.4292612315738,1.00597481446679,26.5241546788566));
#42560=CARTESIAN_POINT('Ctrl Pts',(21.439870434472,0.974895577160786,26.6865619322118));
#42561=CARTESIAN_POINT('Ctrl Pts',(21.4504796373703,0.943816339854783,26.848969185567));
#42562=CARTESIAN_POINT('Ctrl Pts',(21.4610888402686,0.871272314756188,27.0034414855686));
#42563=CARTESIAN_POINT('Ctrl Pts',(21.4716980431668,0.766142309156365,27.131072660665));
#42564=CARTESIAN_POINT('Ctrl Pts',(21.4823072460651,0.661012303556554,27.2587038357614));
#42565=CARTESIAN_POINT('Ctrl Pts',(21.4929164489634,0.523296317455523,27.3594938859524));
#42566=CARTESIAN_POINT('Ctrl Pts',(21.5035256518616,0.369849683871657,27.4211069168442));
#42567=CARTESIAN_POINT('Ctrl Pts',(21.5141348547599,0.216403050287774,27.482719947736));
#42568=CARTESIAN_POINT('Ctrl Pts',(21.5247440576582,0.047225769221051,27.5051559593285));
#42569=CARTESIAN_POINT('Ctrl Pts',(21.5353532605565,-0.116976215942728,
27.485668963609));
#42570=CARTESIAN_POINT('Ctrl Pts',(21.5459624634548,-0.281178201106498,
27.4661819678894));
#42571=CARTESIAN_POINT('Ctrl Pts',(21.556571666353,-0.440404890367325,27.4047719648578));
#42572=CARTESIAN_POINT('Ctrl Pts',(21.5671808692513,-0.575168213030661,
27.3089550467346));
#42573=CARTESIAN_POINT('Ctrl Pts',(21.5777900721496,-0.709931535694004,
27.2131381286113));
#42574=CARTESIAN_POINT('Ctrl Pts',(21.5883992750478,-0.820231491759853,
27.0829142953965));
#42575=CARTESIAN_POINT('Ctrl Pts',(21.5990084779461,-0.89256825056919,26.9342219006385));
#42576=CARTESIAN_POINT('Ctrl Pts',(21.6086167260854,-0.958080196649587,
26.7995583034814));
#42577=CARTESIAN_POINT('Ctrl Pts',(21.6182249742246,-0.992454502819291,
26.649746682434));
#42578=CARTESIAN_POINT('Ctrl Pts',(21.6278332223638,-0.992566083749324,
26.4999845389628));
#42579=CARTESIAN_POINT('Origin',(18.,0.,26.5));
#42580=CARTESIAN_POINT('',(22.1721667776362,-0.993165579585467,26.5002657239842));
#42581=CARTESIAN_POINT('',(22.0278332223638,-0.99241508312295,26.500004132563));
#42582=CARTESIAN_POINT('',(18.,-0.9925,26.5));
#42583=CARTESIAN_POINT('Ctrl Pts',(22.1721667776362,-0.993165579585467,
26.5002657239842));
#42584=CARTESIAN_POINT('Ctrl Pts',(22.1529390405505,-0.990983883449612,
26.7991898919088));
#42585=CARTESIAN_POINT('Ctrl Pts',(22.1337113034647,-0.848467038466999,
27.0965311454012));
#42586=CARTESIAN_POINT('Ctrl Pts',(22.114483566379,-0.613318510459232,27.2817036625806));
#42587=CARTESIAN_POINT('Ctrl Pts',(22.1038980308785,-0.483861097970969,
27.3836475494553));
#42588=CARTESIAN_POINT('Ctrl Pts',(22.0933124953779,-0.326328096839694,
27.4515943934557));
#42589=CARTESIAN_POINT('Ctrl Pts',(22.0827269598774,-0.163258892301617,
27.4786899022784));
#42590=CARTESIAN_POINT('Ctrl Pts',(22.0721414243769,-0.000189687763549218,
27.5057854111011));
#42591=CARTESIAN_POINT('Ctrl Pts',(22.0615558888763,0.168415720181321,27.4920295847462));
#42592=CARTESIAN_POINT('Ctrl Pts',(22.0509703533758,0.32410190589134,27.4382065021411));
#42593=CARTESIAN_POINT('Ctrl Pts',(22.0403848178753,0.47978809160136,27.3843834195361));
#42594=CARTESIAN_POINT('Ctrl Pts',(22.0297992823747,0.622555055076529,27.2904930806809));
#42595=CARTESIAN_POINT('Ctrl Pts',(22.0192137468742,0.7338151263775,27.1684925075482));
#42596=CARTESIAN_POINT('Ctrl Pts',(22.0086282113737,0.845075197678483,27.0464919344155));
#42597=CARTESIAN_POINT('Ctrl Pts',(21.9980426758731,0.924828376805261,26.8963811270054));
#42598=CARTESIAN_POINT('Ctrl Pts',(21.9874571403726,0.964005726421413,26.736156181366));
#42599=CARTESIAN_POINT('Ctrl Pts',(21.9768716048721,1.00318307603756,26.5759312357267));
#42600=CARTESIAN_POINT('Ctrl Pts',(21.9662860693715,1.00178459614309,26.4055921518581));
#42601=CARTESIAN_POINT('Ctrl Pts',(21.955700533871,0.959618079499461,26.2460887247811));
#42602=CARTESIAN_POINT('Ctrl Pts',(21.9451149983705,0.917451562855824,26.0865852977042));
#42603=CARTESIAN_POINT('Ctrl Pts',(21.93452946287,0.83451700946301,25.9379175274189));
#42604=CARTESIAN_POINT('Ctrl Pts',(21.9239439273694,0.721145618717982,25.818033012205));
#42605=CARTESIAN_POINT('Ctrl Pts',(21.9133583918689,0.607774227972941,25.698148496991));
#42606=CARTESIAN_POINT('Ctrl Pts',(21.9027728563683,0.463965999875679,25.6070472368483));
#42607=CARTESIAN_POINT('Ctrl Pts',(21.8921873208678,0.307064068355902,25.5560458421564));
#42608=CARTESIAN_POINT('Ctrl Pts',(21.8816017853673,0.150162136836144,25.5050444474645));
#42609=CARTESIAN_POINT('Ctrl Pts',(21.8710162498668,-0.0198334981061266,
25.4941429182234));
#42610=CARTESIAN_POINT('Ctrl Pts',(21.8604307143662,-0.181994958540001,
25.5243183830589));
#42611=CARTESIAN_POINT('Ctrl Pts',(21.8498451788657,-0.344156418973875,
25.5544938478944));
#42612=CARTESIAN_POINT('Ctrl Pts',(21.8392596433651,-0.498483704899352,
25.6257463068065));
#42613=CARTESIAN_POINT('Ctrl Pts',(21.8286741078646,-0.626502697534403,
25.7300251677291));
#42614=CARTESIAN_POINT('Ctrl Pts',(21.8180885723641,-0.754521690169455,
25.8343040286516));
#42615=CARTESIAN_POINT('Ctrl Pts',(21.8075030368636,-0.856232389514079,
25.9716092915846));
#42616=CARTESIAN_POINT('Ctrl Pts',(21.7969175013631,-0.918659178709456,
26.1240494720909));
#42617=CARTESIAN_POINT('Ctrl Pts',(21.7886672601208,-0.967313880289416,
26.2428595468509));
#42618=CARTESIAN_POINT('Ctrl Pts',(21.7804170188785,-0.992105730367064,
26.3708632657564));
#42619=CARTESIAN_POINT('Ctrl Pts',(21.7721667776362,-0.992176529618623,
26.499357490987));
#42620=CARTESIAN_POINT('Ctrl Pts',(21.6278332223638,-0.992566083749324,
26.4999845389628));
#42621=CARTESIAN_POINT('Ctrl Pts',(21.6288341771228,-0.992577707872818,
26.4843828259284));
#42622=CARTESIAN_POINT('Ctrl Pts',(21.6298351318819,-0.992217486624713,
26.4687816498625));
#42623=CARTESIAN_POINT('Ctrl Pts',(21.6308360866409,-0.991481886769432,
26.453198193129));
#42624=CARTESIAN_POINT('Ctrl Pts',(21.6414452895392,-0.983685202607518,
26.2880278366786));
#42625=CARTESIAN_POINT('Ctrl Pts',(21.6520544924375,-0.93371827273086,26.1248480800787));
#42626=CARTESIAN_POINT('Ctrl Pts',(21.6626636953357,-0.847696648912507,
25.9836308177856));
#42627=CARTESIAN_POINT('Ctrl Pts',(21.673272898234,-0.761675025094154,25.8424135554925));
#42628=CARTESIAN_POINT('Ctrl Pts',(21.6838821011323,-0.639598707334108,
25.7231587875063));
#42629=CARTESIAN_POINT('Ctrl Pts',(21.6944913040306,-0.496408858584897,
25.6404623416995));
#42630=CARTESIAN_POINT('Ctrl Pts',(21.7051005069288,-0.353219009835685,
25.5577658958927));
#42631=CARTESIAN_POINT('Ctrl Pts',(21.7157097098271,-0.188915630097313,
25.5116277722654));
#42632=CARTESIAN_POINT('Ctrl Pts',(21.7263189127254,-0.0236081362932755,
25.5076949073904));
#42633=CARTESIAN_POINT('Ctrl Pts',(21.7369281156237,0.141699357510753,25.5037620425154));
#42634=CARTESIAN_POINT('Ctrl Pts',(21.7475373185219,0.30801096538044,25.5420344363926));
#42635=CARTESIAN_POINT('Ctrl Pts',(21.7581465214202,0.454971479363318,25.6178278547334));
#42636=CARTESIAN_POINT('Ctrl Pts',(21.7687557243185,0.601931993346212,25.6936212730742));
#42637=CARTESIAN_POINT('Ctrl Pts',(21.7793649272167,0.729541413442286,25.8069357158786));
#42638=CARTESIAN_POINT('Ctrl Pts',(21.789974130115,0.822181369316348,25.9439024034692));
#42639=CARTESIAN_POINT('Ctrl Pts',(21.8005833330133,0.91482132519041,26.0808690910598));
#42640=CARTESIAN_POINT('Ctrl Pts',(21.8111925359116,0.972491816842456,26.2414880234368));
#42641=CARTESIAN_POINT('Ctrl Pts',(21.8218017388098,0.988134438275843,26.4061007305058));
#42642=CARTESIAN_POINT('Ctrl Pts',(21.8324109417081,1.00377705970923,26.5707134375748));
#42643=CARTESIAN_POINT('Ctrl Pts',(21.8430201446064,0.977391810923953,26.7393199193359));
#42644=CARTESIAN_POINT('Ctrl Pts',(21.8536293475047,0.912208034915269,26.8912840936638));
#42645=CARTESIAN_POINT('Ctrl Pts',(21.8642385504029,0.847024258906589,27.0432482679916));
#42646=CARTESIAN_POINT('Ctrl Pts',(21.8748477533012,0.743041955674507,27.1785701348863));
#42647=CARTESIAN_POINT('Ctrl Pts',(21.8854569561995,0.612987725801971,27.2806873823333));
#42648=CARTESIAN_POINT('Ctrl Pts',(21.8960661590977,0.48293349592942,27.3828046297803));
#42649=CARTESIAN_POINT('Ctrl Pts',(21.906675361996,0.326807339416416,27.4517172577797));
#42650=CARTESIAN_POINT('Ctrl Pts',(21.9172845648943,0.163717846597389,27.4789909129424));
#42651=CARTESIAN_POINT('Ctrl Pts',(21.9278937677926,0.000628353778372309,
27.5062645681051));
#42652=CARTESIAN_POINT('Ctrl Pts',(21.9385029706908,-0.169424475346632,
27.491899250431));
#42653=CARTESIAN_POINT('Ctrl Pts',(21.9491121735891,-0.325627537326366,
27.4376531596774));
#42654=CARTESIAN_POINT('Ctrl Pts',(21.9597213764874,-0.481830599306091,
27.3834070689238));
#42655=CARTESIAN_POINT('Ctrl Pts',(21.9703305793856,-0.624183894140539,
27.2892802050905));
#42656=CARTESIAN_POINT('Ctrl Pts',(21.9809397822839,-0.735264519386526,
27.1667929419614));
#42657=CARTESIAN_POINT('Ctrl Pts',(21.9915489851822,-0.84634514463252,27.0443056788323));
#42658=CARTESIAN_POINT('Ctrl Pts',(22.0021581880805,-0.926153100290073,
26.8934580164074));
#42659=CARTESIAN_POINT('Ctrl Pts',(22.0127673909787,-0.964920532181839,
26.7327124996475));
#42660=CARTESIAN_POINT('Ctrl Pts',(22.0177893347738,-0.983271379639895,
26.6566224334841));
#42661=CARTESIAN_POINT('Ctrl Pts',(22.0228112785688,-0.992426394010815,
26.5783145833347));
#42662=CARTESIAN_POINT('Ctrl Pts',(22.0278332223638,-0.99241508312295,26.500004132563));
#42663=CARTESIAN_POINT('Origin',(18.,0.,26.5));
#42664=CARTESIAN_POINT('',(22.5721667776362,-0.992204861021737,26.5000685690985));
#42665=CARTESIAN_POINT('',(22.4278332223638,-0.992581696356067,26.5000071712556));
#42666=CARTESIAN_POINT('',(18.,-0.9925,26.5));
#42667=CARTESIAN_POINT('Ctrl Pts',(22.5721667776362,-0.992204861021737,
26.5000685690985));
#42668=CARTESIAN_POINT('Ctrl Pts',(22.5678032042246,-0.992827066651901,
26.5679305324631));
#42669=CARTESIAN_POINT('Ctrl Pts',(22.563439630813,-0.986484995098284,26.6357983943371));
#42670=CARTESIAN_POINT('Ctrl Pts',(22.5590760574013,-0.972771803344622,
26.7023245659368));
#42671=CARTESIAN_POINT('Ctrl Pts',(22.5484905219008,-0.93950515135077,26.8637095329703));
#42672=CARTESIAN_POINT('Ctrl Pts',(22.5379049864003,-0.862859993839026,
27.0171987504581));
#42673=CARTESIAN_POINT('Ctrl Pts',(22.5273194508997,-0.755650710103984,
27.1430236349129));
#42674=CARTESIAN_POINT('Ctrl Pts',(22.5167339153992,-0.648441426368947,
27.2688485193677));
#42675=CARTESIAN_POINT('Ctrl Pts',(22.5061483798987,-0.510668016410612,
27.3670090707894));
#42676=CARTESIAN_POINT('Ctrl Pts',(22.4955628443982,-0.356945922593113,
27.4262089906746));
#42677=CARTESIAN_POINT('Ctrl Pts',(22.4849773088976,-0.203223828775614,
27.4854089105597));
#42678=CARTESIAN_POINT('Ctrl Pts',(22.4743917733971,-0.033553051098976,
27.5056481989083));
#42679=CARTESIAN_POINT('Ctrl Pts',(22.4638062378966,0.130148147127243,27.4840875632523));
#42680=CARTESIAN_POINT('Ctrl Pts',(22.453220702396,0.293849345353462,27.4625269275963));
#42681=CARTESIAN_POINT('Ctrl Pts',(22.4426351668955,0.451580964129261,27.3991663679356));
#42682=CARTESIAN_POINT('Ctrl Pts',(22.4320496313949,0.584809674211439,27.301919215083));
#42683=CARTESIAN_POINT('Ctrl Pts',(22.4214640958944,0.718038384293619,27.2046720622305));
#42684=CARTESIAN_POINT('Ctrl Pts',(22.4108785603939,0.826764185682209,27.0735383161861));
#42685=CARTESIAN_POINT('Ctrl Pts',(22.4002930248934,0.89733657369241,26.9244112011946));
#42686=CARTESIAN_POINT('Ctrl Pts',(22.3897074893929,0.967908961702614,26.7752840862031));
#42687=CARTESIAN_POINT('Ctrl Pts',(22.3791219538923,1.00032793633442,26.6081636022645));
#42688=CARTESIAN_POINT('Ctrl Pts',(22.3685364183917,0.990923755700695,26.4434306953693));
#42689=CARTESIAN_POINT('Ctrl Pts',(22.3579508828912,0.981519575066965,26.278697788474));
#42690=CARTESIAN_POINT('Ctrl Pts',(22.3473653473907,0.930292239167682,26.1163524586221));
#42691=CARTESIAN_POINT('Ctrl Pts',(22.3367798118902,0.843207081642137,25.9762256099674));
#42692=CARTESIAN_POINT('Ctrl Pts',(22.3261942763896,0.756121924116602,25.8360987613127));
#42693=CARTESIAN_POINT('Ctrl Pts',(22.3156087408891,0.633178944964809,25.7181903938551));
#42694=CARTESIAN_POINT('Ctrl Pts',(22.3050232053886,0.489748677103296,25.6367369949742));
#42695=CARTESIAN_POINT('Ctrl Pts',(22.294437669888,0.346318409241783,25.5552835960932));
#42696=CARTESIAN_POINT('Ctrl Pts',(22.2838521343875,0.182400852670543,25.5102851657888));
#42697=CARTESIAN_POINT('Ctrl Pts',(22.273266598887,0.0173094984056945,25.5074944566334));
#42698=CARTESIAN_POINT('Ctrl Pts',(22.2626810633864,-0.147781855859145,
25.5047037474779));
#42699=CARTESIAN_POINT('Ctrl Pts',(22.2520955278859,-0.314047007817625,
25.5441207594714));
#42700=CARTESIAN_POINT('Ctrl Pts',(22.2415099923854,-0.460033215139826,
25.6204302602804));
#42701=CARTESIAN_POINT('Ctrl Pts',(22.2309244568849,-0.606019422462045,
25.6967397610894));
#42702=CARTESIAN_POINT('Ctrl Pts',(22.2203389213843,-0.73172668514799,25.809941750714));
#42703=CARTESIAN_POINT('Ctrl Pts',(22.2097533858838,-0.823920078142038,
25.9471500243541));
#42704=CARTESIAN_POINT('Ctrl Pts',(22.1991678503832,-0.916113471136081,
26.0843582979942));
#42705=CARTESIAN_POINT('Ctrl Pts',(22.1885823148827,-0.97479299443821,26.2455728556497));
#42706=CARTESIAN_POINT('Ctrl Pts',(22.1779967793822,-0.98947726490555,26.4096952182945));
#42707=CARTESIAN_POINT('Ctrl Pts',(22.1760534454669,-0.992173060580657,
26.4398254420867));
#42708=CARTESIAN_POINT('Ctrl Pts',(22.1741101115516,-0.993386082085311,
26.4700536677735));
#42709=CARTESIAN_POINT('Ctrl Pts',(22.1721667776362,-0.993165579585467,
26.5002657239842));
#42710=CARTESIAN_POINT('Ctrl Pts',(22.0278332223638,-0.99241508312295,26.500004132563));
#42711=CARTESIAN_POINT('Ctrl Pts',(22.0334204814671,-0.992402498979485,
26.4128783508313));
#42712=CARTESIAN_POINT('Ctrl Pts',(22.0390077405703,-0.981043747310354,
26.3257493500237));
#42713=CARTESIAN_POINT('Ctrl Pts',(22.0445949996735,-0.958379464788188,
26.2416677674185));
#42714=CARTESIAN_POINT('Ctrl Pts',(22.0552042025718,-0.915344057376794,
26.0820119230443));
#42715=CARTESIAN_POINT('Ctrl Pts',(22.0658134054701,-0.831546334428029,
25.9333436053908));
#42716=CARTESIAN_POINT('Ctrl Pts',(22.0764226083684,-0.717242465660984,
25.8138586250846));
#42717=CARTESIAN_POINT('Ctrl Pts',(22.0870318112667,-0.602938596893939,
25.6943736447783));
#42718=CARTESIAN_POINT('Ctrl Pts',(22.0976410141649,-0.458128582308614,
25.6040720018193));
#42719=CARTESIAN_POINT('Ctrl Pts',(22.1082502170632,-0.300536007157066,
25.5540058936123));
#42720=CARTESIAN_POINT('Ctrl Pts',(22.1188594199615,-0.14294343200551,25.5039397854052));
#42721=CARTESIAN_POINT('Ctrl Pts',(22.1294686228597,0.0274317037122691,
25.4941092119501));
#42722=CARTESIAN_POINT('Ctrl Pts',(22.140077825758,0.189736848801019,25.525717356654));
#42723=CARTESIAN_POINT('Ctrl Pts',(22.1506870286563,0.35204199388976,25.5573255013578));
#42724=CARTESIAN_POINT('Ctrl Pts',(22.1612962315546,0.506277148349473,25.6303723642206));
#42725=CARTESIAN_POINT('Ctrl Pts',(22.1719054344528,0.633565165342219,25.7359175946384));
#42726=CARTESIAN_POINT('Ctrl Pts',(22.1825146373511,0.760853182334965,25.8414628250562));
#42727=CARTESIAN_POINT('Ctrl Pts',(22.1931238402494,0.861194061860744,25.9795064230291));
#42728=CARTESIAN_POINT('Ctrl Pts',(22.2037330431476,0.922306884415235,26.1331529584711));
#42729=CARTESIAN_POINT('Ctrl Pts',(22.2143422460459,0.983419706969726,26.2867994939131));
#42730=CARTESIAN_POINT('Ctrl Pts',(22.2249514489442,1.00530447255293,26.4560489668241));
#42731=CARTESIAN_POINT('Ctrl Pts',(22.2355606518425,0.985282661245862,26.6201865981153));
#42732=CARTESIAN_POINT('Ctrl Pts',(22.2461698547407,0.965260849938794,26.7843242294065));
#42733=CARTESIAN_POINT('Ctrl Pts',(22.256779057639,0.903332461741456,26.9433500190778));
#42734=CARTESIAN_POINT('Ctrl Pts',(22.2673882605373,0.807077035064093,27.0778004849344));
#42735=CARTESIAN_POINT('Ctrl Pts',(22.2779974634355,0.710821608386725,27.212250950791));
#42736=CARTESIAN_POINT('Ctrl Pts',(22.2886066663338,0.58023914322933,27.3221260928329));
#42737=CARTESIAN_POINT('Ctrl Pts',(22.2992158692321,0.431311886816099,27.393978074233));
#42738=CARTESIAN_POINT('Ctrl Pts',(22.3098250721304,0.282384630402886,27.4658300556332));
#42739=CARTESIAN_POINT('Ctrl Pts',(22.3204342750286,0.115112582733842,27.4996588763916));
#42740=CARTESIAN_POINT('Ctrl Pts',(22.3310434779269,-0.0500314981042523,
27.4913241599576));
#42741=CARTESIAN_POINT('Ctrl Pts',(22.3416526808252,-0.215175578942356,
27.4829894435237));
#42742=CARTESIAN_POINT('Ctrl Pts',(22.3522618837235,-0.37819169294951,27.4324911898973));
#42743=CARTESIAN_POINT('Ctrl Pts',(22.3628710866217,-0.519127974211338,
27.3460099806205));
#42744=CARTESIAN_POINT('Ctrl Pts',(22.37348028952,-0.660064255473166,27.2595287713437));
#42745=CARTESIAN_POINT('Ctrl Pts',(22.3840894924183,-0.778920703989667,
27.1370646064163));
#42746=CARTESIAN_POINT('Ctrl Pts',(22.3946986953166,-0.861150242999118,
26.993606118176));
#42747=CARTESIAN_POINT('Ctrl Pts',(22.4053078982148,-0.943379782008568,
26.8501476299357));
#42748=CARTESIAN_POINT('Ctrl Pts',(22.4159171011131,-0.988982411510966,
26.6856948183825));
#42749=CARTESIAN_POINT('Ctrl Pts',(22.4265263040114,-0.992376735122795,
26.5203753896963));
#42750=CARTESIAN_POINT('Ctrl Pts',(22.4269619434622,-0.992516114234338,
26.5135869753534));
#42751=CARTESIAN_POINT('Ctrl Pts',(22.427397582913,-0.992584325009407,26.5067970997886));
#42752=CARTESIAN_POINT('Ctrl Pts',(22.4278332223638,-0.992581696356067,
26.5000071712556));
#42753=CARTESIAN_POINT('Origin',(18.,0.,26.5));
#42754=CARTESIAN_POINT('',(22.9721667776362,-0.992215768961308,26.5005746468071));
#42755=CARTESIAN_POINT('',(22.8278332223638,-0.99243012155925,26.4999841927042));
#42756=CARTESIAN_POINT('',(18.,-0.9925,26.5));
#42757=CARTESIAN_POINT('Ctrl Pts',(22.9721667776362,-0.992215768961308,
26.5005746468071));
#42758=CARTESIAN_POINT('Ctrl Pts',(22.9720818323982,-0.992214140284424,
26.5019013181872));
#42759=CARTESIAN_POINT('Ctrl Pts',(22.9719968871601,-0.992209860101849,
26.5032279082689));
#42760=CARTESIAN_POINT('Ctrl Pts',(22.9719119419221,-0.992202926891772,
26.5045544049738));
#42761=CARTESIAN_POINT('Ctrl Pts',(22.9613264064216,-0.9913389380079,26.669857113936));
#42762=CARTESIAN_POINT('Ctrl Pts',(22.950740870921,-0.949275696035103,26.8337097612191));
#42763=CARTESIAN_POINT('Ctrl Pts',(22.9401553354205,-0.869906177042421,
26.9780551528911));
#42764=CARTESIAN_POINT('Ctrl Pts',(22.92956979992,-0.790536658049743,27.122400544563));
#42765=CARTESIAN_POINT('Ctrl Pts',(22.9189842644194,-0.673860862037187,
27.2472386806237));
#42766=CARTESIAN_POINT('Ctrl Pts',(22.9083987289189,-0.534806228703558,
27.3362709908208));
#42767=CARTESIAN_POINT('Ctrl Pts',(22.8978131934184,-0.395751595369929,
27.425303301018));
#42768=CARTESIAN_POINT('Ctrl Pts',(22.8872276579178,-0.234318124715232,
27.4785297853516));
#42769=CARTESIAN_POINT('Ctrl Pts',(22.8766421224173,-0.06977610285199,27.4900545833647));
#42770=CARTESIAN_POINT('Ctrl Pts',(22.8660565869168,0.0947659190112521,
27.5015793813778));
#42771=CARTESIAN_POINT('Ctrl Pts',(22.8554710514162,0.262416492083034,27.4714024930703));
#42772=CARTESIAN_POINT('Ctrl Pts',(22.8448855159157,0.412494903395397,27.4028763751801));
#42773=CARTESIAN_POINT('Ctrl Pts',(22.8342999804152,0.56257331470776,27.3343502572899));
#42774=CARTESIAN_POINT('Ctrl Pts',(22.8237144449146,0.695079564260698,27.2274749098169));
#42775=CARTESIAN_POINT('Ctrl Pts',(22.8131289094141,0.794071068217059,27.0954671396971));
#42776=CARTESIAN_POINT('Ctrl Pts',(22.8025433739136,0.89306257217342,26.9634593695772));
#42777=CARTESIAN_POINT('Ctrl Pts',(22.791957838413,0.958539330533199,26.8063191768106));
#42778=CARTESIAN_POINT('Ctrl Pts',(22.7813723029125,0.982279771970663,26.6430532899404));
#42779=CARTESIAN_POINT('Ctrl Pts',(22.770786767412,1.00602021340813,26.4797874030702));
#42780=CARTESIAN_POINT('Ctrl Pts',(22.7602012319115,0.988024337923265,26.3103958220965));
#42781=CARTESIAN_POINT('Ctrl Pts',(22.7496156964109,0.930867274580648,26.1556703618835));
#42782=CARTESIAN_POINT('Ctrl Pts',(22.7390301609104,0.87371021123803,26.0009449016704));
#42783=CARTESIAN_POINT('Ctrl Pts',(22.7284446254099,0.777391960037676,25.8608855622181));
#42784=CARTESIAN_POINT('Ctrl Pts',(22.7178590899093,0.652970567212468,25.7523394415226));
#42785=CARTESIAN_POINT('Ctrl Pts',(22.7072735544088,0.528549174387274,25.6437933208272));
#42786=CARTESIAN_POINT('Ctrl Pts',(22.6966880189083,0.376024639937221,25.5667604188887));
#42787=CARTESIAN_POINT('Ctrl Pts',(22.6861024834077,0.21522463077963,25.5310047242798));
#42788=CARTESIAN_POINT('Ctrl Pts',(22.6755169479072,0.0544246216220219,
25.4952490296709));
#42789=CARTESIAN_POINT('Ctrl Pts',(22.6649314124067,-0.114650862243145,
25.5007705423917));
#42790=CARTESIAN_POINT('Ctrl Pts',(22.6543458769061,-0.273577064688015,
25.54624794605));
#42791=CARTESIAN_POINT('Ctrl Pts',(22.6437603414056,-0.432503267132867,
25.5917253497082));
#42792=CARTESIAN_POINT('Ctrl Pts',(22.6331748059051,-0.581280188157419,
25.6771586443039));
#42793=CARTESIAN_POINT('Ctrl Pts',(22.6225892704045,-0.698294921854431,
25.793172996076));
#42794=CARTESIAN_POINT('Ctrl Pts',(22.6057817728151,-0.884088531865305,
25.9773782200491));
#42795=CARTESIAN_POINT('Ctrl Pts',(22.5889742752257,-0.989808265698904,
26.2386796389553));
#42796=CARTESIAN_POINT('Ctrl Pts',(22.5721667776362,-0.992204861021737,
26.5000685690985));
#42797=CARTESIAN_POINT('Ctrl Pts',(22.4278332223638,-0.992581696356067,
26.5000071712556));
#42798=CARTESIAN_POINT('Ctrl Pts',(22.4380067858113,-0.992520308959953,
26.3414407957685));
#42799=CARTESIAN_POINT('Ctrl Pts',(22.4481803492587,-0.953825173771418,
26.1828455329487));
#42800=CARTESIAN_POINT('Ctrl Pts',(22.4583539127062,-0.88068530865534,26.042157092403));
#42801=CARTESIAN_POINT('Ctrl Pts',(22.4689631156045,-0.804413540854797,
25.8954442696148));
#42802=CARTESIAN_POINT('Ctrl Pts',(22.4795723185027,-0.69068398753245,25.7682046698575));
#42803=CARTESIAN_POINT('Ctrl Pts',(22.490181521401,-0.553416234566112,25.6760114004205));
#42804=CARTESIAN_POINT('Ctrl Pts',(22.5007907242993,-0.416148481599767,
25.5838181309836));
#42805=CARTESIAN_POINT('Ctrl Pts',(22.5113999271975,-0.255342528989424,
25.5266711918671));
#42806=CARTESIAN_POINT('Ctrl Pts',(22.5220091300958,-0.0906797366071229,
25.5115649104331));
#42807=CARTESIAN_POINT('Ctrl Pts',(22.5326183329941,0.073983055775169,25.4964586289991));
#42808=CARTESIAN_POINT('Ctrl Pts',(22.5432275358924,0.242502687929425,25.5233930052477));
#42809=CARTESIAN_POINT('Ctrl Pts',(22.5538367387906,0.394253707426228,25.5890714873828));
#42810=CARTESIAN_POINT('Ctrl Pts',(22.5644459416889,0.54600472692304,25.654749969518));
#42811=CARTESIAN_POINT('Ctrl Pts',(22.5750551445872,0.680987133762404,25.7591725575397));
#42812=CARTESIAN_POINT('Ctrl Pts',(22.5856643474855,0.782680163120166,25.8895587635354));
#42813=CARTESIAN_POINT('Ctrl Pts',(22.5962735503837,0.884373192477921,26.019944969531));
#42814=CARTESIAN_POINT('Ctrl Pts',(22.606882753282,0.952776844354082,26.1762947935006));
#42815=CARTESIAN_POINT('Ctrl Pts',(22.6174919561803,0.979519059958022,26.3394722700054));
#42816=CARTESIAN_POINT('Ctrl Pts',(22.6281011590785,1.00626127556196,26.5026497465103));
#42817=CARTESIAN_POINT('Ctrl Pts',(22.6387103619768,0.991342054893685,26.6726548755504));
#42818=CARTESIAN_POINT('Ctrl Pts',(22.6493195648751,0.936587390997702,26.8286803917826));
#42819=CARTESIAN_POINT('Ctrl Pts',(22.6599287677734,0.881832727101723,26.9847059080148));
#42820=CARTESIAN_POINT('Ctrl Pts',(22.6705379706716,0.787242619978021,27.1267518114392));
#42821=CARTESIAN_POINT('Ctrl Pts',(22.6811471735699,0.664394140676646,27.2374328218576));
#42822=CARTESIAN_POINT('Ctrl Pts',(22.6917563764682,0.541545661375256,27.3481138322759));
#42823=CARTESIAN_POINT('Ctrl Pts',(22.7023655793664,0.390438809896197,27.4274299496884));
#42824=CARTESIAN_POINT('Ctrl Pts',(22.7129747822647,0.229567853863308,27.465673516977));
#42825=CARTESIAN_POINT('Ctrl Pts',(22.723583985163,0.0686968978304285,27.5039170842657));
#42826=CARTESIAN_POINT('Ctrl Pts',(22.7341931880613,-0.101938162756261,
27.5010881014307));
#42827=CARTESIAN_POINT('Ctrl Pts',(22.7448023909595,-0.261452963980634,
27.4575328132989));
#42828=CARTESIAN_POINT('Ctrl Pts',(22.7554115938578,-0.420967765205008,
27.4139775251671));
#42829=CARTESIAN_POINT('Ctrl Pts',(22.7660207967561,-0.56936230706707,27.3296959317385));
#42830=CARTESIAN_POINT('Ctrl Pts',(22.7766299996544,-0.688474286903125,
27.2150034246012));
#42831=CARTESIAN_POINT('Ctrl Pts',(22.7872392025526,-0.807586266739185,
27.1003109174639));
#42832=CARTESIAN_POINT('Ctrl Pts',(22.7978484054509,-0.897415684549238,
26.955207496618));
#42833=CARTESIAN_POINT('Ctrl Pts',(22.8084576083492,-0.946968139502241,
26.7974526578902));
#42834=CARTESIAN_POINT('Ctrl Pts',(22.814916146354,-0.977134063994168,26.7014166379228));
#42835=CARTESIAN_POINT('Ctrl Pts',(22.8213746843589,-0.992373431511741,
26.6006920293325));
#42836=CARTESIAN_POINT('Ctrl Pts',(22.8278332223638,-0.99243012155925,26.4999841927042));
#42837=CARTESIAN_POINT('Origin',(18.,0.,26.5));
#42838=CARTESIAN_POINT('',(23.3721667776362,-0.992388032386622,26.499675821275));
#42839=CARTESIAN_POINT('',(23.2278332223638,-0.992528322420212,26.5000239907786));
#42840=CARTESIAN_POINT('',(18.,-0.9925,26.5));
#42841=CARTESIAN_POINT('Ctrl Pts',(23.3721667776362,-0.992388032386622,
26.499675821275));
#42842=CARTESIAN_POINT('Ctrl Pts',(23.3657749250712,-0.992351027245097,
26.5994813785654));
#42843=CARTESIAN_POINT('Ctrl Pts',(23.3593830725062,-0.977461020605066,
26.6994268097226));
#42844=CARTESIAN_POINT('Ctrl Pts',(23.3529912199413,-0.947917745793742,
26.7946503343929));
#42845=CARTESIAN_POINT('Ctrl Pts',(23.3424056844407,-0.898991181681411,
26.9523498417946));
#42846=CARTESIAN_POINT('Ctrl Pts',(23.3318201489402,-0.809875667003528,
27.0970987593237));
#42847=CARTESIAN_POINT('Ctrl Pts',(23.3212346134396,-0.691503973124327,
27.2119684246678));
#42848=CARTESIAN_POINT('Ctrl Pts',(23.3106490779391,-0.573132279245139,
27.3268380900118));
#42849=CARTESIAN_POINT('Ctrl Pts',(23.3000635424386,-0.425504406164642,
27.4118285031709));
#42850=CARTESIAN_POINT('Ctrl Pts',(23.2894780069381,-0.266592626638276,
27.4561726651644));
#42851=CARTESIAN_POINT('Ctrl Pts',(23.2788924714375,-0.107680847111892,
27.500516827158));
#42852=CARTESIAN_POINT('Ctrl Pts',(23.268306935937,0.0625148388603637,27.5042147379859));
#42853=CARTESIAN_POINT('Ctrl Pts',(23.2577214004365,0.223286445894541,27.4670952067496));
#42854=CARTESIAN_POINT('Ctrl Pts',(23.2471358649359,0.384058052928701,27.4299756755133));
#42855=CARTESIAN_POINT('Ctrl Pts',(23.2365503294354,0.535405581024785,27.3520387022128));
#42856=CARTESIAN_POINT('Ctrl Pts',(23.2259647939349,0.658792131885872,27.2425164787066));
#42857=CARTESIAN_POINT('Ctrl Pts',(23.2153792584343,0.782178682746974,27.1329942552003));
#42858=CARTESIAN_POINT('Ctrl Pts',(23.2047937229338,0.877604256373074,26.9918867814884));
#42859=CARTESIAN_POINT('Ctrl Pts',(23.1942081874333,0.933635937153906,26.8367502329998));
#42860=CARTESIAN_POINT('Ctrl Pts',(23.1836226519327,0.989667617934738,26.6816136845112));
#42861=CARTESIAN_POINT('Ctrl Pts',(23.1730371164322,1.0063054058703,26.5124480612458));
#42862=CARTESIAN_POINT('Ctrl Pts',(23.1624515809317,0.981144614563025,26.3492614260964));
#42863=CARTESIAN_POINT('Ctrl Pts',(23.1518660454311,0.955983823255751,26.186074790947));
#42864=CARTESIAN_POINT('Ctrl Pts',(23.1412805099306,0.889024452705641,26.0288671439135));
#42865=CARTESIAN_POINT('Ctrl Pts',(23.1306949744301,0.789132149463115,25.8978837846844));
#42866=CARTESIAN_POINT('Ctrl Pts',(23.1201094389296,0.68923984622059,25.7669004254553));
#42867=CARTESIAN_POINT('Ctrl Pts',(23.109523903429,0.55641461028565,25.6621413540304));
#42868=CARTESIAN_POINT('Ctrl Pts',(23.0989383679285,0.405594721429978,25.5944723567525));
#42869=CARTESIAN_POINT('Ctrl Pts',(23.0883528324279,0.254774832574307,25.5268033594745));
#42870=CARTESIAN_POINT('Ctrl Pts',(23.0777672969274,0.0859602907979053,
25.4962244363435));
#42871=CARTESIAN_POINT('Ctrl Pts',(23.0671817614269,-0.0782820979201608,
25.5094990537566));
#42872=CARTESIAN_POINT('Ctrl Pts',(23.0460106904258,-0.406766875356302,
25.5360482885829));
#42873=CARTESIAN_POINT('Ctrl Pts',(23.0248396194247,-0.7169630405591,25.7380116855861));
#42874=CARTESIAN_POINT('Ctrl Pts',(23.0036685484237,-0.874142114566764,
26.0276698454422));
#42875=CARTESIAN_POINT('Ctrl Pts',(22.9931679581612,-0.952100997889672,
26.1713367224124));
#42876=CARTESIAN_POINT('Ctrl Pts',(22.9826673678987,-0.992417099477605,
26.3365768418982));
#42877=CARTESIAN_POINT('Ctrl Pts',(22.9721667776362,-0.992215768961308,
26.5005746468071));
#42878=CARTESIAN_POINT('Ctrl Pts',(22.8278332223638,-0.99243012155925,26.4999841927042));
#42879=CARTESIAN_POINT('Ctrl Pts',(22.8319838872572,-0.992466554168273,
26.43526296916));
#42880=CARTESIAN_POINT('Ctrl Pts',(22.8361345521506,-0.986232297652164,
26.3705486727048));
#42881=CARTESIAN_POINT('Ctrl Pts',(22.840285217044,-0.973659369893009,26.3070902482045));
#42882=CARTESIAN_POINT('Ctrl Pts',(22.8508944199423,-0.941522653234819,
26.1448889338561));
#42883=CARTESIAN_POINT('Ctrl Pts',(22.8615036228405,-0.867973727822483,
25.990892561769));
#42884=CARTESIAN_POINT('Ctrl Pts',(22.8721128257388,-0.762014392692314,
25.8639490537323));
#42885=CARTESIAN_POINT('Ctrl Pts',(22.8827220286371,-0.65605505756214,25.7370055456956));
#42886=CARTESIAN_POINT('Ctrl Pts',(22.8933312315354,-0.517685312714129,
25.6371149017093));
#42887=CARTESIAN_POINT('Ctrl Pts',(22.9039404344336,-0.363840505997963,
25.5765029360559));
#42888=CARTESIAN_POINT('Ctrl Pts',(22.9145496373319,-0.209995699281814,
25.5158909704025));
#42889=CARTESIAN_POINT('Ctrl Pts',(22.9251588402302,-0.0406758306975135,
25.4945576830821));
#42890=CARTESIAN_POINT('Ctrl Pts',(22.9357680431284,0.123395704799732,25.5151140974939));
#42891=CARTESIAN_POINT('Ctrl Pts',(22.9463772460267,0.287467240296987,25.5356705119057));
#42892=CARTESIAN_POINT('Ctrl Pts',(22.956986448925,0.446290442707186,25.5981166280497));
#42893=CARTESIAN_POINT('Ctrl Pts',(22.9675956518233,0.580426624892681,25.6948095417642));
#42894=CARTESIAN_POINT('Ctrl Pts',(22.9782048547215,0.714562807078176,25.7915024554787));
#42895=CARTESIAN_POINT('Ctrl Pts',(22.9888140576198,0.824011969038968,25.9224421667636));
#42896=CARTESIAN_POINT('Ctrl Pts',(22.9994232605181,0.895378410496085,26.0716027043319));
#42897=CARTESIAN_POINT('Ctrl Pts',(23.0100324634163,0.966744851953198,26.2207632419001));
#42898=CARTESIAN_POINT('Ctrl Pts',(23.0206416663146,1.00002857290664,26.3881446057516));
#42899=CARTESIAN_POINT('Ctrl Pts',(23.0312508692129,0.991155912653363,26.553260658375));
#42900=CARTESIAN_POINT('Ctrl Pts',(23.0418600721112,0.982283252400084,26.7183767109984));
#42901=CARTESIAN_POINT('Ctrl Pts',(23.0524692750094,0.931254210940078,26.8812274523936));
#42902=CARTESIAN_POINT('Ctrl Pts',(23.0630784779077,0.844314333992244,27.0218812569287));
#42903=CARTESIAN_POINT('Ctrl Pts',(23.073687680806,0.75737445704441,27.1625350614638));
#42904=CARTESIAN_POINT('Ctrl Pts',(23.0842968837043,0.634523744608749,27.2809919291387));
#42905=CARTESIAN_POINT('Ctrl Pts',(23.0949060866025,0.490798139339951,27.3627536886845));
#42906=CARTESIAN_POINT('Ctrl Pts',(23.1055152895008,0.347072534071171,27.4445154482302));
#42907=CARTESIAN_POINT('Ctrl Pts',(23.1161244923991,0.182472035969259,27.4895820996468));
#42908=CARTESIAN_POINT('Ctrl Pts',(23.1267336952973,0.0171424268642523,
27.492437845973));
#42909=CARTESIAN_POINT('Ctrl Pts',(23.1373428981956,-0.148187182240773,
27.4952935922991));
#42910=CARTESIAN_POINT('Ctrl Pts',(23.1479521010939,-0.314245902348893,
27.4559384335349));
#42911=CARTESIAN_POINT('Ctrl Pts',(23.1585613039922,-0.460709476942957,
27.3791891257137));
#42912=CARTESIAN_POINT('Ctrl Pts',(23.1691705068904,-0.607173051537012,
27.3024398178925));
#42913=CARTESIAN_POINT('Ctrl Pts',(23.1797797097887,-0.734041480617014,
27.1882963610144));
#42914=CARTESIAN_POINT('Ctrl Pts',(23.190388912687,-0.825787085209699,27.0507289994354));
#42915=CARTESIAN_POINT('Ctrl Pts',(23.2009981155852,-0.917532689802385,
26.9131616378564));
#42916=CARTESIAN_POINT('Ctrl Pts',(23.2116073184835,-0.974155469907755,
26.7521703715764));
#42917=CARTESIAN_POINT('Ctrl Pts',(23.2222165213818,-0.988725251025931,
26.5874592413754));
#42918=CARTESIAN_POINT('Ctrl Pts',(23.2240887550425,-0.991296418237979,
26.558392239339));
#42919=CARTESIAN_POINT('Ctrl Pts',(23.2259609887031,-0.99255794656802,26.5292093911432));
#42920=CARTESIAN_POINT('Ctrl Pts',(23.2278332223638,-0.992528322420212,
26.5000239907786));
#42921=CARTESIAN_POINT('Origin',(18.,0.,26.5));
#42922=CARTESIAN_POINT('',(23.7721667776362,-0.992500262637294,26.5000027623734));
#42923=CARTESIAN_POINT('',(23.6278332223638,-0.992486745736932,26.499974029444));
#42924=CARTESIAN_POINT('',(18.,-0.9925,26.5));
#42925=CARTESIAN_POINT('Ctrl Pts',(23.7721667776362,-0.992500262637294,
26.5000027623734));
#42926=CARTESIAN_POINT('Ctrl Pts',(23.7700535532448,-0.992512026843979,
26.5329256477546));
#42927=CARTESIAN_POINT('Ctrl Pts',(23.7679403288534,-0.990885127798118,
26.5658486953477));
#42928=CARTESIAN_POINT('Ctrl Pts',(23.765827104462,-0.987599253356915,26.5986128659939));
#42929=CARTESIAN_POINT('Ctrl Pts',(23.7552415689615,-0.971139694831468,
26.7627347135987));
#42930=CARTESIAN_POINT('Ctrl Pts',(23.7446560334609,-0.913053206437673,
26.9228700285835));
#42931=CARTESIAN_POINT('Ctrl Pts',(23.7340704979604,-0.820140389914714,
27.0592025885277));
#42932=CARTESIAN_POINT('Ctrl Pts',(23.7234849624599,-0.727227573391749,
27.1955351484718));
#42933=CARTESIAN_POINT('Ctrl Pts',(23.7128994269593,-0.599488428739612,
27.3080649533752));
#42934=CARTESIAN_POINT('Ctrl Pts',(23.7023138914588,-0.452644851679794,
27.3833134291327));
#42935=CARTESIAN_POINT('Ctrl Pts',(23.6917283559583,-0.305801274619976,
27.4585619048902));
#42936=CARTESIAN_POINT('Ctrl Pts',(23.6811428204577,-0.13985326515247,27.4965290515018));
#42937=CARTESIAN_POINT('Ctrl Pts',(23.6705572849572,0.0250760671767568,
27.4923250400148));
#42938=CARTESIAN_POINT('Ctrl Pts',(23.6599717494567,0.190005399506003,27.4881210285279));
#42939=CARTESIAN_POINT('Ctrl Pts',(23.6493862139561,0.353916054696976,27.4417458589422));
#42940=CARTESIAN_POINT('Ctrl Pts',(23.6388006784556,0.49675088812807,27.3592527787064));
#42941=CARTESIAN_POINT('Ctrl Pts',(23.6282151429551,0.63958572155914,27.2767596984705));
#42942=CARTESIAN_POINT('Ctrl Pts',(23.6176296074546,0.761344733230343,27.1581487075844));
#42943=CARTESIAN_POINT('Ctrl Pts',(23.607044071954,0.847292882654172,27.017166939539));
#42944=CARTESIAN_POINT('Ctrl Pts',(23.5964585364535,0.933241032078011,26.8761851714936));
#42945=CARTESIAN_POINT('Ctrl Pts',(23.5858730009529,0.983378319254465,26.7128326262889));
#42946=CARTESIAN_POINT('Ctrl Pts',(23.5752874654524,0.991433494211962,26.5483023044681));
#42947=CARTESIAN_POINT('Ctrl Pts',(23.5647019299519,0.999488669169459,26.3837719826473));
#42948=CARTESIAN_POINT('Ctrl Pts',(23.5541163944514,0.965461731907988,26.2180638842104));
#42949=CARTESIAN_POINT('Ctrl Pts',(23.5435308589508,0.893769977117369,26.0691141465064));
#42950=CARTESIAN_POINT('Ctrl Pts',(23.5329453234503,0.822078222326754,25.9201644088025));
#42951=CARTESIAN_POINT('Ctrl Pts',(23.5223597879498,0.712721650006991,25.7879730318314));
#42952=CARTESIAN_POINT('Ctrl Pts',(23.5117742524492,0.578594147325075,25.6922568328701));
#42953=CARTESIAN_POINT('Ctrl Pts',(23.4906031814482,0.310339141961234,25.5008244349476));
#42954=CARTESIAN_POINT('Ctrl Pts',(23.4694321104471,-0.0569995848512428,
25.4552927490642));
#42955=CARTESIAN_POINT('Ctrl Pts',(23.448261039446,-0.363874645107573,25.5754376959817));
#42956=CARTESIAN_POINT('Ctrl Pts',(23.4376755039455,-0.517312175235725,
25.6355101694404));
#42957=CARTESIAN_POINT('Ctrl Pts',(23.427089968445,-0.655633788724846,25.7370018010994));
#42958=CARTESIAN_POINT('Ctrl Pts',(23.4165044329445,-0.761521951267013,
25.8639404835428));
#42959=CARTESIAN_POINT('Ctrl Pts',(23.4059188974439,-0.867410113809191,
25.9908791659863));
#42960=CARTESIAN_POINT('Ctrl Pts',(23.3953333619434,-0.94086482540441,26.1432648992143));
#42961=CARTESIAN_POINT('Ctrl Pts',(23.3847478264428,-0.97322337442863,26.3047828144655));
#42962=CARTESIAN_POINT('Ctrl Pts',(23.3805541435073,-0.986042895449097,
26.3687715399239));
#42963=CARTESIAN_POINT('Ctrl Pts',(23.3763604605718,-0.992412311393211,
26.4341935752085));
#42964=CARTESIAN_POINT('Ctrl Pts',(23.3721667776362,-0.992388032386622,
26.499675821275));
#42965=CARTESIAN_POINT('Ctrl Pts',(23.2278332223638,-0.992528322420212,
26.5000239907786));
#42966=CARTESIAN_POINT('Ctrl Pts',(23.2365701916014,-0.992390078314509,
26.3638273447456));
#42967=CARTESIAN_POINT('Ctrl Pts',(23.245307160839,-0.964134182439229,26.2275751196904));
#42968=CARTESIAN_POINT('Ctrl Pts',(23.2540441300766,-0.909639323030658,
26.1027808628545));
#42969=CARTESIAN_POINT('Ctrl Pts',(23.2646533329749,-0.843466831786224,
25.9512446086564));
#42970=CARTESIAN_POINT('Ctrl Pts',(23.2752625358732,-0.738605067166374,
25.816603094382));
#42971=CARTESIAN_POINT('Ctrl Pts',(23.2858717387714,-0.607888268779764,
25.7153353623374));
#42972=CARTESIAN_POINT('Ctrl Pts',(23.2964809416697,-0.477171470393162,
25.6140676302928));
#42973=CARTESIAN_POINT('Ctrl Pts',(23.307090144568,-0.32059963823978,25.5461736804781));
#42974=CARTESIAN_POINT('Ctrl Pts',(23.3176993474663,-0.157335909780756,
25.5199631882364));
#42975=CARTESIAN_POINT('Ctrl Pts',(23.3283085503645,0.00592781867827763,
25.4937526959947));
#42976=CARTESIAN_POINT('Ctrl Pts',(23.3389177532628,0.175883443442949,25.509225661326));
#42977=CARTESIAN_POINT('Ctrl Pts',(23.3495269561611,0.331729758096689,25.5644883172769));
#42978=CARTESIAN_POINT('Ctrl Pts',(23.3601361590593,0.487576072750439,25.6197509732278));
#42979=CARTESIAN_POINT('Ctrl Pts',(23.3707453619576,0.6293130772932,25.7148033197982));
#42980=CARTESIAN_POINT('Ctrl Pts',(23.3813545648559,0.739593298274526,25.8380117115344));
#42981=CARTESIAN_POINT('Ctrl Pts',(23.3919637677542,0.849873519255846,25.9612201032705));
#42982=CARTESIAN_POINT('Ctrl Pts',(23.4025729706524,0.928696956675713,26.1125845401724));
#42983=CARTESIAN_POINT('Ctrl Pts',(23.4131821735507,0.966416253498947,26.2735792282247));
#42984=CARTESIAN_POINT('Ctrl Pts',(23.423791376449,1.00413555032218,26.434573916277));
#42985=CARTESIAN_POINT('Ctrl Pts',(23.4344005793472,1.00075070654879,26.6051988554798));
#42986=CARTESIAN_POINT('Ctrl Pts',(23.4450097822455,0.956675999929901,26.7645709206931));
#42987=CARTESIAN_POINT('Ctrl Pts',(23.4556189851438,0.912601293311011,26.9239429859064));
#42988=CARTESIAN_POINT('Ctrl Pts',(23.4662281880421,0.827836723846627,27.0720621771303));
#42989=CARTESIAN_POINT('Ctrl Pts',(23.4768373909403,0.712756795520865,27.1907998924125));
#42990=CARTESIAN_POINT('Ctrl Pts',(23.4874465938386,0.597676867195097,27.3095376076947));
#42991=CARTESIAN_POINT('Ctrl Pts',(23.4980557967369,0.452281580007953,27.3988938470351));
#42992=CARTESIAN_POINT('Ctrl Pts',(23.5086649996351,0.294366151887474,27.4479321228554));
#42993=CARTESIAN_POINT('Ctrl Pts',(23.5192742025334,0.136450723767013,27.4969703986757));
#42994=CARTESIAN_POINT('Ctrl Pts',(23.5298834054317,-0.0339848452867753,
27.5056907109758));
#42995=CARTESIAN_POINT('Ctrl Pts',(23.54049260833,-0.196080607522645,27.4730257634163));
#42996=CARTESIAN_POINT('Ctrl Pts',(23.5511018112282,-0.358176369758524,
27.4403608158567));
#42997=CARTESIAN_POINT('Ctrl Pts',(23.5617110141265,-0.511932325176479,
27.3663106084376));
#42998=CARTESIAN_POINT('Ctrl Pts',(23.5723202170248,-0.638529977060899,
27.2599382930955));
#42999=CARTESIAN_POINT('Ctrl Pts',(23.582929419923,-0.765127628945325,27.1535659777533));
#43000=CARTESIAN_POINT('Ctrl Pts',(23.5935386228213,-0.86456697729621,27.0148715544882));
#43001=CARTESIAN_POINT('Ctrl Pts',(23.6041478257196,-0.924677442800011,
26.8608301091859));
#43002=CARTESIAN_POINT('Ctrl Pts',(23.6120429579343,-0.9694103107819,26.7461959006717));
#43003=CARTESIAN_POINT('Ctrl Pts',(23.6199380901491,-0.992362825760545,
26.6230625044533));
#43004=CARTESIAN_POINT('Ctrl Pts',(23.6278332223638,-0.992486745736932,
26.499974029444));
#43005=CARTESIAN_POINT('Origin',(18.,0.,26.5));
#43006=CARTESIAN_POINT('',(24.1721667776362,-0.9925,26.5000000000003));
#43007=CARTESIAN_POINT('',(24.0278332223638,-0.992459651580774,26.5000236090481));
#43008=CARTESIAN_POINT('',(18.,-0.9925,26.5));
#43009=CARTESIAN_POINT('Ctrl Pts',(24.1721667776362,-0.99257394234428,26.4999790041826));
#43010=CARTESIAN_POINT('Ctrl Pts',(24.1637466459179,-0.992421357292391,
26.6312298628555));
#43011=CARTESIAN_POINT('Ctrl Pts',(24.1553265141995,-0.966145501910799,
26.7625240981299));
#43012=CARTESIAN_POINT('Ctrl Pts',(24.1469063824812,-0.915423483254653,
26.8835750541215));
#43013=CARTESIAN_POINT('Ctrl Pts',(24.1363208469806,-0.851657292047284,
27.0357566630184));
#43014=CARTESIAN_POINT('Ctrl Pts',(24.1257353114801,-0.749254527386481,
27.171749015222));
#43015=CARTESIAN_POINT('Ctrl Pts',(24.1151497759796,-0.620448439739691,
27.274842905246));
#43016=CARTESIAN_POINT('Ctrl Pts',(24.104564240479,-0.4916423520929,27.37793679527));
#43017=CARTESIAN_POINT('Ctrl Pts',(24.0939787049785,-0.336432941460122,
27.4481322231143));
#43018=CARTESIAN_POINT('Ctrl Pts',(24.083393169478,-0.174056574351007,27.4771290045311));
#43019=CARTESIAN_POINT('Ctrl Pts',(24.0728076339774,-0.0116802072418913,
27.5061257859478));
#43020=CARTESIAN_POINT('Ctrl Pts',(24.0622220984769,0.157863116343561,27.493923920937));
#43021=CARTESIAN_POINT('Ctrl Pts',(24.0516365629764,0.314446804184475,27.4415360214494));
#43022=CARTESIAN_POINT('Ctrl Pts',(24.0410510274758,0.471030492025389,27.3891481219617));
#43023=CARTESIAN_POINT('Ctrl Pts',(24.0304654919753,0.614654544121765,27.2965741879971));
#43024=CARTESIAN_POINT('Ctrl Pts',(24.0198799564748,0.726863976145958,27.1759750337428));
#43025=CARTESIAN_POINT('Ctrl Pts',(24.0092944209742,0.839073408170171,27.0553758794885));
#43026=CARTESIAN_POINT('Ctrl Pts',(23.9987088854737,0.91986822012219,26.9067515049444));
#43027=CARTESIAN_POINT('Ctrl Pts',(23.9881233499732,0.961064596018904,26.7466621840013));
#43028=CARTESIAN_POINT('Ctrl Pts',(23.9775378144726,1.00226097191561,26.5865728630582));
#43029=CARTESIAN_POINT('Ctrl Pts',(23.9669522789721,1.00385891175703,26.4150185957161));
#43030=CARTESIAN_POINT('Ctrl Pts',(23.9563667434716,0.963007589610471,26.2553848048128));
#43031=CARTESIAN_POINT('Ctrl Pts',(23.9351956724705,0.881304945317355,25.9361172230061));
#43032=CARTESIAN_POINT('Ctrl Pts',(23.9140246014695,0.629805253072327,25.6645315469549));
#43033=CARTESIAN_POINT('Ctrl Pts',(23.8928535304684,0.31774316757647,25.5585864400688));
#43034=CARTESIAN_POINT('Ctrl Pts',(23.8822679949679,0.161712124828541,25.5056138866258));
#43035=CARTESIAN_POINT('Ctrl Pts',(23.8716824594673,-0.00945951623209451,
25.494051475474));
#43036=CARTESIAN_POINT('Ctrl Pts',(23.8610969239668,-0.172236578558568,
25.5228500873746));
#43037=CARTESIAN_POINT('Ctrl Pts',(23.8505113884663,-0.335013640885051,
25.5516486992753));
#43038=CARTESIAN_POINT('Ctrl Pts',(23.8399258529657,-0.489396124477372,
25.6208083342283));
#43039=CARTESIAN_POINT('Ctrl Pts',(23.8293403174652,-0.618244943128008,
25.7234391998311));
#43040=CARTESIAN_POINT('Ctrl Pts',(23.8187547819647,-0.747093761778644,
25.826070065434));
#43041=CARTESIAN_POINT('Ctrl Pts',(23.8081692464641,-0.850408915487596,
25.9621721616866));
#43042=CARTESIAN_POINT('Ctrl Pts',(23.7975837109636,-0.914650178013526,
26.1142773999254));
#43043=CARTESIAN_POINT('Ctrl Pts',(23.7891113998545,-0.966066751330558,
26.2360173817735));
#43044=CARTESIAN_POINT('Ctrl Pts',(23.7806390887453,-0.992453097736398,
26.3680087684108));
#43045=CARTESIAN_POINT('Ctrl Pts',(23.7721667776362,-0.992500262637294,
26.5000027623734));
#43046=CARTESIAN_POINT('Ctrl Pts',(23.6278332223638,-0.992486745736932,
26.499974029444));
#43047=CARTESIAN_POINT('Ctrl Pts',(23.6305472930473,-0.992529345096369,
26.457660511137));
#43048=CARTESIAN_POINT('Ctrl Pts',(23.6332613637309,-0.989874188395367,
26.415352301368));
#43049=CARTESIAN_POINT('Ctrl Pts',(23.6359754344144,-0.984478691600277,
26.3733964980608));
#43050=CARTESIAN_POINT('Ctrl Pts',(23.6465846373127,-0.96338789224003,26.2093927995774));
#43051=CARTESIAN_POINT('Ctrl Pts',(23.657193840211,-0.900424710862815,26.0507738699499));
#43052=CARTESIAN_POINT('Ctrl Pts',(23.6678030431092,-0.803295336271083,
25.9169533949645));
#43053=CARTESIAN_POINT('Ctrl Pts',(23.6784122460075,-0.706165961679351,
25.7831329199791));
#43054=CARTESIAN_POINT('Ctrl Pts',(23.6890214489058,-0.574870393873098,
25.6741108996358));
#43055=CARTESIAN_POINT('Ctrl Pts',(23.699630651804,-0.425478158125808,25.6032307555028));
#43056=CARTESIAN_POINT('Ctrl Pts',(23.7102398547023,-0.276085922378518,
25.5323506113697));
#43057=CARTESIAN_POINT('Ctrl Pts',(23.7208490576006,-0.108597018690186,
25.4996123434469));
#43058=CARTESIAN_POINT('Ctrl Pts',(23.7314582604989,0.0564892534135627,
25.5090228533578));
#43059=CARTESIAN_POINT('Ctrl Pts',(23.7420674633972,0.221575525517311,25.5184333632687));
#43060=CARTESIAN_POINT('Ctrl Pts',(23.7526766662954,0.384259166036481,25.5699926510134));
#43061=CARTESIAN_POINT('Ctrl Pts',(23.7632858691937,0.524629001147119,25.6573902729771));
#43062=CARTESIAN_POINT('Ctrl Pts',(23.773895072092,0.664998836257765,25.7447878949408));
#43063=CARTESIAN_POINT('Ctrl Pts',(23.7845042749902,0.783054865959882,25.8680238511235));
#43064=CARTESIAN_POINT('Ctrl Pts',(23.7951134778885,0.864347978339919,26.0120150481234));
#43065=CARTESIAN_POINT('Ctrl Pts',(23.8057226807868,0.945641090719952,26.1560062451233));
#43066=CARTESIAN_POINT('Ctrl Pts',(23.816331883685,0.990171285777908,26.3207526829404));
#43067=CARTESIAN_POINT('Ctrl Pts',(23.8269410865833,0.992488424511603,26.486090717893));
#43068=CARTESIAN_POINT('Ctrl Pts',(23.8375502894816,0.994805563245297,26.6514287528456));
#43069=CARTESIAN_POINT('Ctrl Pts',(23.8481594923799,0.954909645654713,26.8173583849337));
#43070=CARTESIAN_POINT('Ctrl Pts',(23.8587686952781,0.87768361231997,26.9635711569794));
#43071=CARTESIAN_POINT('Ctrl Pts',(23.8693778981764,0.800457578985232,27.1097839290251));
#43072=CARTESIAN_POINT('Ctrl Pts',(23.8799871010747,0.685901429906335,27.2362798410283));
#43073=CARTESIAN_POINT('Ctrl Pts',(23.890596303973,0.54803591965721,27.3275768071205));
#43074=CARTESIAN_POINT('Ctrl Pts',(23.9012055068712,0.410170409408084,27.4188737732127));
#43075=CARTESIAN_POINT('Ctrl Pts',(23.9118147097695,0.248995537988726,27.474971793394));
#43076=CARTESIAN_POINT('Ctrl Pts',(23.9224239126678,0.0842378179768146,
27.4890049195736));
#43077=CARTESIAN_POINT('Ctrl Pts',(23.933033115566,-0.0805199020350873,
27.5030380457532));
#43078=CARTESIAN_POINT('Ctrl Pts',(23.9436423184643,-0.248860470639547,
27.4750062779312));
#43079=CARTESIAN_POINT('Ctrl Pts',(23.9542515213626,-0.400180351350601,
27.4083404798374));
#43080=CARTESIAN_POINT('Ctrl Pts',(23.9648607242609,-0.551500232061663,
27.3416746817435));
#43081=CARTESIAN_POINT('Ctrl Pts',(23.9754699271591,-0.685799424879341,
27.2363748533779));
#43082=CARTESIAN_POINT('Ctrl Pts',(23.9860791300574,-0.786640784900299,
27.1053288498409));
#43083=CARTESIAN_POINT('Ctrl Pts',(23.9966883329557,-0.887482144921262,
26.9742828463039));
#43084=CARTESIAN_POINT('Ctrl Pts',(24.007297535854,-0.954865672145517,26.8174906675955));
#43085=CARTESIAN_POINT('Ctrl Pts',(24.0179067387522,-0.980544162864392,
26.6541424198293));
#43086=CARTESIAN_POINT('Ctrl Pts',(24.0212155666228,-0.988552842364468,
26.6031969114822));
#43087=CARTESIAN_POINT('Ctrl Pts',(24.0245243944933,-0.992504836310417,
26.551613688536));
#43088=CARTESIAN_POINT('Ctrl Pts',(24.0278332223638,-0.992459651580774,
26.5000236090481));
#43089=CARTESIAN_POINT('Origin',(18.,0.,26.5));
#43090=CARTESIAN_POINT('',(24.5721667776362,-0.9925,26.5000000000003));
#43091=CARTESIAN_POINT('',(24.4278332223638,-0.992555410679472,26.4999811860602));
#43092=CARTESIAN_POINT('',(18.,-0.9925,26.5));
#43093=CARTESIAN_POINT('Ctrl Pts',(24.5721667776362,-0.9925,26.5000000000003));
#43094=CARTESIAN_POINT('Ctrl Pts',(24.5554259338597,-0.992499999999917,
26.7609923249232));
#43095=CARTESIAN_POINT('Ctrl Pts',(24.5386850900831,-0.884539443097234,
27.020349130175));
#43096=CARTESIAN_POINT('Ctrl Pts',(24.5219442463066,-0.699346033936665,
27.2042523516589));
#43097=CARTESIAN_POINT('Ctrl Pts',(24.5052034025301,-0.514152624776095,
27.3881555731427));
#43098=CARTESIAN_POINT('Ctrl Pts',(24.4884625587535,-0.254047408344091,
27.4943003359058));
#43099=CARTESIAN_POINT('Ctrl Pts',(24.471721714977,0.00693853867385297,
27.4924757461425));
#43100=CARTESIAN_POINT('Ctrl Pts',(24.4549808712005,0.267924485691796,27.4906511563792));
#43101=CARTESIAN_POINT('Ctrl Pts',(24.4382400274239,0.526520203888397,27.3808800818307));
#43102=CARTESIAN_POINT('Ctrl Pts',(24.4214991836474,0.70912424955959,27.1944055361866));
#43103=CARTESIAN_POINT('Ctrl Pts',(24.4047583398709,0.891728295230784,27.0079309905425));
#43104=CARTESIAN_POINT('Ctrl Pts',(24.3880174960943,0.996052076106294,26.7470900753835));
#43105=CARTESIAN_POINT('Ctrl Pts',(24.3712766523178,0.992402985755312,26.4861232617686));
#43106=CARTESIAN_POINT('Ctrl Pts',(24.3545358085413,0.988753895404331,26.2251564481538));
#43107=CARTESIAN_POINT('Ctrl Pts',(24.3377949647647,0.877177668191286,25.9673344556899));
#43108=CARTESIAN_POINT('Ctrl Pts',(24.3210541209882,0.689431099871355,25.7860385104712));
#43109=CARTESIAN_POINT('Ctrl Pts',(24.3043132772117,0.501684531551424,25.6047425652525));
#43110=CARTESIAN_POINT('Ctrl Pts',(24.2875724334351,0.240120666075239,25.5022448650133));
#43111=CARTESIAN_POINT('Ctrl Pts',(24.2708315896586,-0.0208142595733872,
25.5077182776054));
#43112=CARTESIAN_POINT('Ctrl Pts',(24.2540907458821,-0.281749185222014,
25.5131916901974));
#43113=CARTESIAN_POINT('Ctrl Pts',(24.2373499021055,-0.538784851091028,
25.6265676168681));
#43114=CARTESIAN_POINT('Ctrl Pts',(24.220609058329,-0.718763835149907,25.815577031887));
#43115=CARTESIAN_POINT('Ctrl Pts',(24.2044616314314,-0.89236305911901,25.9978865828699));
#43116=CARTESIAN_POINT('Ctrl Pts',(24.1883142045338,-0.992500000000069,
26.2482591353353));
#43117=CARTESIAN_POINT('Ctrl Pts',(24.1721667776362,-0.9925,26.5000000000003));
#43118=CARTESIAN_POINT('Ctrl Pts',(24.0278332223638,-0.992459651580774,
26.5000236090481));
#43119=CARTESIAN_POINT('Ctrl Pts',(24.0351335973915,-0.992359959035612,
26.3861987312633));
#43120=CARTESIAN_POINT('Ctrl Pts',(24.0424339724193,-0.972802385036297,
26.2723404764931));
#43121=CARTESIAN_POINT('Ctrl Pts',(24.049734347447,-0.934426046269535,26.1652243960929));
#43122=CARTESIAN_POINT('Ctrl Pts',(24.0603435503453,-0.878655984742315,
26.0095589369469));
#43123=CARTESIAN_POINT('Ctrl Pts',(24.0709527532436,-0.783142407474387,
25.8681323354789));
#43124=CARTESIAN_POINT('Ctrl Pts',(24.0815619561419,-0.659575410860569,
25.7582540742907));
#43125=CARTESIAN_POINT('Ctrl Pts',(24.0921711590401,-0.536008414246758,
25.6483758131025));
#43126=CARTESIAN_POINT('Ctrl Pts',(24.1027803619384,-0.384387998287034,
25.5700458921941));
#43127=CARTESIAN_POINT('Ctrl Pts',(24.1133895648367,-0.223271286781966,
25.5328512661348));
#43128=CARTESIAN_POINT('Ctrl Pts',(24.123998767735,-0.0621545752768985,
25.4956566400755));
#43129=CARTESIAN_POINT('Ctrl Pts',(24.1346079706332,0.108458431773511,25.4995973088654));
#43130=CARTESIAN_POINT('Ctrl Pts',(24.1452171735315,0.267686069629295,25.5441909662256));
#43131=CARTESIAN_POINT('Ctrl Pts',(24.1558263764298,0.426913707485089,25.5887846235859));
#43132=CARTESIAN_POINT('Ctrl Pts',(24.166435579328,0.574755976146227,25.6740312695166));
#43133=CARTESIAN_POINT('Ctrl Pts',(24.1770447822263,0.693118166762793,25.7894973977376));
#43134=CARTESIAN_POINT('Ctrl Pts',(24.1876539851246,0.811480357379345,25.9049635259586));
#43135=CARTESIAN_POINT('Ctrl Pts',(24.1982631880229,0.900362469951331,26.0506491364699));
#43136=CARTESIAN_POINT('Ctrl Pts',(24.2088723909211,0.948886046216982,26.2087234780952));
#43137=CARTESIAN_POINT('Ctrl Pts',(24.2194815938194,0.997409622482638,26.3667978197206));
#43138=CARTESIAN_POINT('Ctrl Pts',(24.2300907967177,1.00557466244195,26.53726089246));
#43139=CARTESIAN_POINT('Ctrl Pts',(24.2406999996159,0.972381830639979,26.6992493823315));
#43140=CARTESIAN_POINT('Ctrl Pts',(24.2513092025142,0.939188998838011,26.8612378722031));
#43141=CARTESIAN_POINT('Ctrl Pts',(24.2619184054125,0.86463829527477,27.0147517792067));
#43142=CARTESIAN_POINT('Ctrl Pts',(24.2725276083108,0.757854128603812,27.141002231413));
#43143=CARTESIAN_POINT('Ctrl Pts',(24.283136811209,0.651069961932841,27.2672526836192));
#43144=CARTESIAN_POINT('Ctrl Pts',(24.2937460141073,0.512052332154146,27.3662396810281));
#43145=CARTESIAN_POINT('Ctrl Pts',(24.3043552170056,0.357815883040657,27.4258480084561));
#43146=CARTESIAN_POINT('Ctrl Pts',(24.3149644199038,0.203579433927185,27.4854563358841));
#43147=CARTESIAN_POINT('Ctrl Pts',(24.3255736228021,0.0341241654789235,
27.5056859933312));
#43148=CARTESIAN_POINT('Ctrl Pts',(24.3361828257004,-0.129809955490691,
27.48406103285));
#43149=CARTESIAN_POINT('Ctrl Pts',(24.3467920285987,-0.293744076460323,
27.4624360723688));
#43150=CARTESIAN_POINT('Ctrl Pts',(24.357401231497,-0.452157049951307,27.3989564939593));
#43151=CARTESIAN_POINT('Ctrl Pts',(24.3680104343952,-0.585660397558057,
27.3013916892821));
#43152=CARTESIAN_POINT('Ctrl Pts',(24.3786196372935,-0.719163745164792,
27.203826884605));
#43153=CARTESIAN_POINT('Ctrl Pts',(24.3892288401918,-0.827757466887299,
27.0721768536602));
#43154=CARTESIAN_POINT('Ctrl Pts',(24.39983804309,-0.898150561476123,26.9225545051687));
#43155=CARTESIAN_POINT('Ctrl Pts',(24.4091697695146,-0.960067475233129,
26.7909484989009));
#43156=CARTESIAN_POINT('Ctrl Pts',(24.4185014959392,-0.992429524077198,
26.6454377623415));
#43157=CARTESIAN_POINT('Ctrl Pts',(24.4278332223638,-0.992555410679472,
26.4999811860602));
#43158=CARTESIAN_POINT('Origin',(18.,0.,26.5));
#43159=CARTESIAN_POINT('',(24.9721667776362,-0.99251277648446,26.5000582001704));
#43160=CARTESIAN_POINT('',(24.8278332223638,-0.992417933442169,26.5000080784797));
#43161=CARTESIAN_POINT('',(18.,-0.9925,26.5));
#43162=CARTESIAN_POINT('Ctrl Pts',(24.9721667776362,-0.99251277648446,26.5000582001704));
#43163=CARTESIAN_POINT('Ctrl Pts',(24.9617183667645,-0.99255659087909,26.6628621040987));
#43164=CARTESIAN_POINT('Ctrl Pts',(24.9512699558928,-0.951915057130168,
26.8255137793979));
#43165=CARTESIAN_POINT('Ctrl Pts',(24.9408215450211,-0.874820116044522,
26.9691019472486));
#43166=CARTESIAN_POINT('Ctrl Pts',(24.9302360095206,-0.796713383279699,
27.1145745618789));
#43167=CARTESIAN_POINT('Ctrl Pts',(24.91965047402,-0.681190137660315,27.240480007797));
#43168=CARTESIAN_POINT('Ctrl Pts',(24.9090649385195,-0.543356244838065,
27.3306849446437));
#43169=CARTESIAN_POINT('Ctrl Pts',(24.8984794030189,-0.40552235201583,27.4208898814904));
#43170=CARTESIAN_POINT('Ctrl Pts',(24.8878938675184,-0.24537781199073,27.4753943092657));
#43171=CARTESIAN_POINT('Ctrl Pts',(24.8773083320179,-0.0806281138645919,
27.4889319986692));
#43172=CARTESIAN_POINT('Ctrl Pts',(24.8667227965174,0.0841215842615465,
27.5024696880728));
#43173=CARTESIAN_POINT('Ctrl Pts',(24.8561372610168,0.253476440488729,27.4750406391045));
#43174=CARTESIAN_POINT('Ctrl Pts',(24.8455517255163,0.403905693619946,27.4077887430593));
#43175=CARTESIAN_POINT('Ctrl Pts',(24.8243806545152,0.704764199882382,27.273284950969));
#43176=CARTESIAN_POINT('Ctrl Pts',(24.8032095835142,0.929920293760979,26.9794897705714));
#43177=CARTESIAN_POINT('Ctrl Pts',(24.7820385125131,0.981581218735328,26.6540081893599));
#43178=CARTESIAN_POINT('Ctrl Pts',(24.7714529770126,1.0074116812225,26.4912673987541));
#43179=CARTESIAN_POINT('Ctrl Pts',(24.760867441512,0.989868351483619,26.320605007945));
#43180=CARTESIAN_POINT('Ctrl Pts',(24.7502819060115,0.933964243597536,26.1650400286325));
#43181=CARTESIAN_POINT('Ctrl Pts',(24.739696370511,0.878060135711457,26.0094750493199));
#43182=CARTESIAN_POINT('Ctrl Pts',(24.7291108350104,0.783795249678182,25.8690074815041));
#43183=CARTESIAN_POINT('Ctrl Pts',(24.7185252995099,0.660857833523188,25.759364860452));
#43184=CARTESIAN_POINT('Ctrl Pts',(24.7079397640094,0.537920417368194,25.6497222393999));
#43185=CARTESIAN_POINT('Ctrl Pts',(24.6973542285088,0.386310471091475,25.5709045651114));
#43186=CARTESIAN_POINT('Ctrl Pts',(24.6867686930083,0.225533816953791,25.5333038896536));
#43187=CARTESIAN_POINT('Ctrl Pts',(24.6761831575078,0.0647571628160969,
25.4957032141958));
#43188=CARTESIAN_POINT('Ctrl Pts',(24.6655976220072,-0.10518619918257,25.4993195375686));
#43189=CARTESIAN_POINT('Ctrl Pts',(24.6550120865067,-0.264162719082483,
25.5432895733726));
#43190=CARTESIAN_POINT('Ctrl Pts',(24.6444265510062,-0.423139238982396,
25.5872596091765));
#43191=CARTESIAN_POINT('Ctrl Pts',(24.6338410155057,-0.571148916783561,
25.6715833574117));
#43192=CARTESIAN_POINT('Ctrl Pts',(24.6232554800051,-0.689810539973791,
25.7862078642024));
#43193=CARTESIAN_POINT('Ctrl Pts',(24.6126699445046,-0.808472163164022,
25.9008323709931));
#43194=CARTESIAN_POINT('Ctrl Pts',(24.602084409004,-0.897785731743322,26.0457576363393));
#43195=CARTESIAN_POINT('Ctrl Pts',(24.5914988735035,-0.947124736504967,
26.2032093172979));
#43196=CARTESIAN_POINT('Ctrl Pts',(24.5850548415477,-0.97716026218375,26.299059325409));
#43197=CARTESIAN_POINT('Ctrl Pts',(24.578610809592,-0.992381750402969,26.3995514552194));
#43198=CARTESIAN_POINT('Ctrl Pts',(24.5721667776362,-0.992469460302077,
26.5000248288071));
#43199=CARTESIAN_POINT('Ctrl Pts',(24.4278332223638,-0.992555410679472,
26.4999811860602));
#43200=CARTESIAN_POINT('Ctrl Pts',(24.4291106988375,-0.992572644057889,
26.4800687555315));
#43201=CARTESIAN_POINT('Ctrl Pts',(24.4303881753112,-0.991985754731688,
26.460157339995));
#43202=CARTESIAN_POINT('Ctrl Pts',(24.4316656517849,-0.990787863821187,
26.4402827510437));
#43203=CARTESIAN_POINT('Ctrl Pts',(24.4422748546831,-0.980839604122276,
26.2752280114485));
#43204=CARTESIAN_POINT('Ctrl Pts',(24.4528840575814,-0.928750617269329,
26.1127131982961));
#43205=CARTESIAN_POINT('Ctrl Pts',(24.4634932604797,-0.840896177802749,
25.972628822294));
#43206=CARTESIAN_POINT('Ctrl Pts',(24.4741024633779,-0.753041738336164,
25.8325444462919));
#43207=CARTESIAN_POINT('Ctrl Pts',(24.4847116662762,-0.629421846255941,
25.7148905074399));
#43208=CARTESIAN_POINT('Ctrl Pts',(24.4953208691745,-0.485166585640924,
25.6340669049541));
#43209=CARTESIAN_POINT('Ctrl Pts',(24.5059300720728,-0.340911325025915,
25.5532433024682));
#43210=CARTESIAN_POINT('Ctrl Pts',(24.516539274971,-0.176020695876084,25.5092500363485));
#43211=CARTESIAN_POINT('Ctrl Pts',(24.5271484778693,-0.0106759897366275,
25.5074715297981));
#43212=CARTESIAN_POINT('Ctrl Pts',(24.5377576807676,0.154668716402848,25.5056930232476));
#43213=CARTESIAN_POINT('Ctrl Pts',(24.5483668836659,0.320467499531954,25.5461292762665));
#43214=CARTESIAN_POINT('Ctrl Pts',(24.5589760865641,0.466427917336639,25.6238312155485));
#43215=CARTESIAN_POINT('Ctrl Pts',(24.5695852894624,0.612388335141316,25.7015331548305));
#43216=CARTESIAN_POINT('Ctrl Pts',(24.5801944923606,0.738510387621547,25.8165007803756));
#43217=CARTESIAN_POINT('Ctrl Pts',(24.5908036952589,0.829357746318288,25.954662976188));
#43218=CARTESIAN_POINT('Ctrl Pts',(24.6014128981572,0.920205105015029,26.0928251720005));
#43219=CARTESIAN_POINT('Ctrl Pts',(24.6120221010555,0.97577776992828,26.2541819380803));
#43220=CARTESIAN_POINT('Ctrl Pts',(24.6226313039538,0.98927409224187,26.4189844994011));
#43221=CARTESIAN_POINT('Ctrl Pts',(24.6332405068521,1.00277041455546,26.583787060722));
#43222=CARTESIAN_POINT('Ctrl Pts',(24.6438497097503,0.974190394269388,26.7520354172838));
#43223=CARTESIAN_POINT('Ctrl Pts',(24.6544589126486,0.907031996821316,26.9031373186156));
#43224=CARTESIAN_POINT('Ctrl Pts',(24.6650681155468,0.839873599373236,27.0542392199475));
#43225=CARTESIAN_POINT('Ctrl Pts',(24.6756773184451,0.734136824763144,27.1881946660494));
#43226=CARTESIAN_POINT('Ctrl Pts',(24.6862865213434,0.60276300681002,27.2886085838612));
#43227=CARTESIAN_POINT('Ctrl Pts',(24.6968957242417,0.471389188856896,27.389022501673));
#43228=CARTESIAN_POINT('Ctrl Pts',(24.7075049271399,0.31437832756074,27.4558948911948));
#43229=CARTESIAN_POINT('Ctrl Pts',(24.7181141300382,0.150947294031265,27.4810411078762));
#43230=CARTESIAN_POINT('Ctrl Pts',(24.7287233329365,-0.0124837394982006,
27.5061873245576));
#43231=CARTESIAN_POINT('Ctrl Pts',(24.7393325358348,-0.182334945260984,
27.4896073683986));
#43232=CARTESIAN_POINT('Ctrl Pts',(24.749941738733,-0.337817896889458,27.4333304931585));
#43233=CARTESIAN_POINT('Ctrl Pts',(24.7605509416313,-0.493300848517933,
27.3770536179183));
#43234=CARTESIAN_POINT('Ctrl Pts',(24.7711601445296,-0.634415546012099,
27.281079823597));
#43235=CARTESIAN_POINT('Ctrl Pts',(24.7817693474278,-0.743890681316928,
27.1571555334684));
#43236=CARTESIAN_POINT('Ctrl Pts',(24.7923785503261,-0.853365816621756,
27.0332312433397));
#43237=CARTESIAN_POINT('Ctrl Pts',(24.8029877532244,-0.931201389737248,
26.8813564574038));
#43238=CARTESIAN_POINT('Ctrl Pts',(24.8135969561227,-0.967870950302176,
26.7201194323076));
#43239=CARTESIAN_POINT('Ctrl Pts',(24.818342378203,-0.984272987670209,26.6479992413373));
#43240=CARTESIAN_POINT('Ctrl Pts',(24.8230878002834,-0.992438898982193,
26.5740059376434));
#43241=CARTESIAN_POINT('Ctrl Pts',(24.8278332223638,-0.992417933442169,
26.5000080784797));
#43242=CARTESIAN_POINT('Origin',(18.,0.,26.5));
#43243=CARTESIAN_POINT('',(25.3721667776362,-0.992387361158253,26.5001400376411));
#43244=CARTESIAN_POINT('',(25.2278332223638,-0.99258529737825,26.5000026553357));
#43245=CARTESIAN_POINT('',(18.,-0.9925,26.5));
#43246=CARTESIAN_POINT('Ctrl Pts',(25.3721667776362,-0.992387361158253,
26.5001400376411));
#43247=CARTESIAN_POINT('Ctrl Pts',(25.3659969949381,-0.992306742378732,
26.5965231262208));
#43248=CARTESIAN_POINT('Ctrl Pts',(25.35982721224,-0.978386398123005,26.6928893412557));
#43249=CARTESIAN_POINT('Ctrl Pts',(25.3536574295418,-0.950854057019746,
26.7848684754603));
#43250=CARTESIAN_POINT('Ctrl Pts',(25.3430718940413,-0.903616643901465,
26.9426776622776));
#43251=CARTESIAN_POINT('Ctrl Pts',(25.3324863585408,-0.81631029856865,27.0875728257978));
#43252=CARTESIAN_POINT('Ctrl Pts',(25.3219008230402,-0.699077270305875,
27.2041153036819));
#43253=CARTESIAN_POINT('Ctrl Pts',(25.3113152875397,-0.581844242043086,
27.320657781566));
#43254=CARTESIAN_POINT('Ctrl Pts',(25.3007297520392,-0.434684530850328,
27.408847573814));
#43255=CARTESIAN_POINT('Ctrl Pts',(25.2901442165386,-0.276325837818277,
27.454392080184));
#43256=CARTESIAN_POINT('Ctrl Pts',(25.2689731455376,0.0403915482457888,
27.5454810929239));
#43257=CARTESIAN_POINT('Ctrl Pts',(25.2478020745365,0.40190486166702,27.465988962152));
#43258=CARTESIAN_POINT('Ctrl Pts',(25.2266310035354,0.6511968846158,27.2504417557882));
#43259=CARTESIAN_POINT('Ctrl Pts',(25.2160454680349,0.77584289609019,27.1426681526063));
#43260=CARTESIAN_POINT('Ctrl Pts',(25.2054599325344,0.872433584946467,27.0008807805265));
#43261=CARTESIAN_POINT('Ctrl Pts',(25.1948743970339,0.929964336340446,26.8459099938888));
#43262=CARTESIAN_POINT('Ctrl Pts',(25.1842888615333,0.987495087734426,26.6909392072512));
#43263=CARTESIAN_POINT('Ctrl Pts',(25.1737033260328,1.00596590166611,26.5227850060558));
#43264=CARTESIAN_POINT('Ctrl Pts',(25.1631177905322,0.982646449396851,26.3597165670864));
#43265=CARTESIAN_POINT('Ctrl Pts',(25.1525322550317,0.95932699712759,26.196648128117));
#43266=CARTESIAN_POINT('Ctrl Pts',(25.1419467195312,0.89421727865738,26.0386654513737));
#43267=CARTESIAN_POINT('Ctrl Pts',(25.1313611840307,0.795532045788893,25.9062865704134));
#43268=CARTESIAN_POINT('Ctrl Pts',(25.1207756485301,0.696846812920429,25.7739076894532));
#43269=CARTESIAN_POINT('Ctrl Pts',(25.1101901130296,0.564586065653703,25.667132604276));
#43270=CARTESIAN_POINT('Ctrl Pts',(25.099604577529,0.414699306759659,25.5982787195903));
#43271=CARTESIAN_POINT('Ctrl Pts',(25.0890190420285,0.26481254786558,25.5294248349045));
#43272=CARTESIAN_POINT('Ctrl Pts',(25.078433506528,0.0972997773441754,25.4984921507102));
#43273=CARTESIAN_POINT('Ctrl Pts',(25.0678479710275,-0.0673058880772577,
25.5096426343912));
#43274=CARTESIAN_POINT('Ctrl Pts',(25.0572624355269,-0.231911553498672,
25.5207931180722));
#43275=CARTESIAN_POINT('Ctrl Pts',(25.0466769000264,-0.393610113820115,
25.5740267696286));
#43276=CARTESIAN_POINT('Ctrl Pts',(25.0360913645259,-0.532820336822596,
25.6626037589608));
#43277=CARTESIAN_POINT('Ctrl Pts',(25.0255058290253,-0.672030559825076,
25.7511807482929));
#43278=CARTESIAN_POINT('Ctrl Pts',(25.0149202935248,-0.788752445508594,
25.8751010754009));
#43279=CARTESIAN_POINT('Ctrl Pts',(25.0043347580243,-0.868585547923311,
26.0194826328588));
#43280=CARTESIAN_POINT('Ctrl Pts',(24.9937492225237,-0.948418650338028,
26.1638641903168));
#43281=CARTESIAN_POINT('Ctrl Pts',(24.9831636870232,-0.991362969483945,
26.3287069781248));
#43282=CARTESIAN_POINT('Ctrl Pts',(24.9725781515227,-0.992490019101772,
26.4936482637001));
#43283=CARTESIAN_POINT('Ctrl Pts',(24.9724410268938,-0.992504618860141,
26.4957849069112));
#43284=CARTESIAN_POINT('Ctrl Pts',(24.972303902265,-0.992512201465668,26.4979215666506));
#43285=CARTESIAN_POINT('Ctrl Pts',(24.9721667776362,-0.99251277648446,26.5000582001704));
#43286=CARTESIAN_POINT('Ctrl Pts',(24.8278332223638,-0.992417933442169,
26.5000080784797));
#43287=CARTESIAN_POINT('Ctrl Pts',(24.8336970031817,-0.992392026930725,
26.408571064073));
#43288=CARTESIAN_POINT('Ctrl Pts',(24.8395607839996,-0.979865717223218,
26.3171270939968));
#43289=CARTESIAN_POINT('Ctrl Pts',(24.8454245648175,-0.954931924032951,
26.2292016222704));
#43290=CARTESIAN_POINT('Ctrl Pts',(24.8560337677157,-0.909819789184432,
26.0701201015859));
#43291=CARTESIAN_POINT('Ctrl Pts',(24.866642970614,-0.824091971473027,25.9225563244732));
#43292=CARTESIAN_POINT('Ctrl Pts',(24.8772521735123,-0.70824086874865,25.8045709146488));
#43293=CARTESIAN_POINT('Ctrl Pts',(24.8878613764106,-0.592389766024272,
25.6865855048243));
#43294=CARTESIAN_POINT('Ctrl Pts',(24.8984705793089,-0.446415378286923,
25.5981784622881));
#43295=CARTESIAN_POINT('Ctrl Pts',(24.9090797822071,-0.288183800730977,
25.5501701005367));
#43296=CARTESIAN_POINT('Ctrl Pts',(24.9196889851054,-0.129952223175031,
25.5021617387853));
#43297=CARTESIAN_POINT('Ctrl Pts',(24.9302981880037,0.0405365441995126,
25.4945520578188));
#43298=CARTESIAN_POINT('Ctrl Pts',(24.9409073909019,0.202416042593281,25.5282724216021));
#43299=CARTESIAN_POINT('Ctrl Pts',(24.9515165938002,0.364295540987049,25.5619927853854));
#43300=CARTESIAN_POINT('Ctrl Pts',(24.9621257966985,0.517565770400043,25.6370431939185));
#43301=CARTESIAN_POINT('Ctrl Pts',(24.9727349995968,0.643467683086959,25.7442380786643));
#43302=CARTESIAN_POINT('Ctrl Pts',(24.983344202495,0.769369595773882,25.8514329634102));
#43303=CARTESIAN_POINT('Ctrl Pts',(24.9939534053933,0.867903191734725,25.9907723243687));
#43304=CARTESIAN_POINT('Ctrl Pts',(25.0045626082916,0.927008748489623,26.145202140449));
#43305=CARTESIAN_POINT('Ctrl Pts',(25.0151718111898,0.986114305244514,26.2996319565293));
#43306=CARTESIAN_POINT('Ctrl Pts',(25.0257810140881,1.00579182279347,26.4691522277313));
#43307=CARTESIAN_POINT('Ctrl Pts',(25.0363902169864,0.983632930687616,26.6330150314256));
#43308=CARTESIAN_POINT('Ctrl Pts',(25.0469994198846,0.961474038581758,26.7968778351198));
#43309=CARTESIAN_POINT('Ctrl Pts',(25.0576086227829,0.897478736821098,26.9550831713063));
#43310=CARTESIAN_POINT('Ctrl Pts',(25.0682178256812,0.799479537471402,27.0882679747214));
#43311=CARTESIAN_POINT('Ctrl Pts',(25.0788270285795,0.701480338121717,27.2214527781364));
#43312=CARTESIAN_POINT('Ctrl Pts',(25.0894362314777,0.569477241183014,27.3296170487802));
#43313=CARTESIAN_POINT('Ctrl Pts',(25.100045434376,0.419626367824316,27.3995223467735));
#43314=CARTESIAN_POINT('Ctrl Pts',(25.1106546372743,0.269775494465601,27.4694276447668));
#43315=CARTESIAN_POINT('Ctrl Pts',(25.1212638401726,0.102076844686887,27.5010739701096));
#43316=CARTESIAN_POINT('Ctrl Pts',(25.1318730430708,-0.0629446107456808,
27.4905880661992));
#43317=CARTESIAN_POINT('Ctrl Pts',(25.1424822459691,-0.22796606617824,27.4801021622889));
#43318=CARTESIAN_POINT('Ctrl Pts',(25.1530914488674,-0.390310327264653,
27.4274840291254));
#43319=CARTESIAN_POINT('Ctrl Pts',(25.1637006517656,-0.530107757503696,
27.3391737045169));
#43320=CARTESIAN_POINT('Ctrl Pts',(25.1743098546639,-0.66990518774273,27.2508633799084));
#43321=CARTESIAN_POINT('Ctrl Pts',(25.1849190575622,-0.787155787134396,
27.126860863855));
#43322=CARTESIAN_POINT('Ctrl Pts',(25.1955282604605,-0.867509021980289,
26.9823430705432));
#43323=CARTESIAN_POINT('Ctrl Pts',(25.2061374633587,-0.947862256826192,
26.8378252772315));
#43324=CARTESIAN_POINT('Ctrl Pts',(25.216746666257,-0.991318127126315,26.6727922066615));
#43325=CARTESIAN_POINT('Ctrl Pts',(25.2273558691553,-0.992557982618985,
26.5074425840666));
#43326=CARTESIAN_POINT('Ctrl Pts',(25.2275149868914,-0.99257657807814,26.504962656227));
#43327=CARTESIAN_POINT('Ctrl Pts',(25.2276741046276,-0.992585677358007,
26.5024826571814));
#43328=CARTESIAN_POINT('Ctrl Pts',(25.2278332223638,-0.99258529737825,26.5000026553357));
#43329=CARTESIAN_POINT('Origin',(18.,0.,26.5));
#43330=CARTESIAN_POINT('',(25.7721667776362,-0.9921765548274,26.4993478195649));
#43331=CARTESIAN_POINT('',(25.6278332223638,-0.99242346011951,26.4999876204483));
#43332=CARTESIAN_POINT('',(18.,-0.9925,26.5));
#43333=CARTESIAN_POINT('Ctrl Pts',(25.7721667776362,-0.9921765548274,26.4993478195649));
#43334=CARTESIAN_POINT('Ctrl Pts',(25.7702756231116,-0.992198777860299,
26.528814111564));
#43335=CARTESIAN_POINT('Ctrl Pts',(25.7683844685871,-0.990919946850656,
26.5583087935269));
#43336=CARTESIAN_POINT('Ctrl Pts',(25.7664933140626,-0.988327533930795,
26.5877272816407));
#43337=CARTESIAN_POINT('Ctrl Pts',(25.755907778562,-0.973816779447677,26.7523941273481));
#43338=CARTESIAN_POINT('Ctrl Pts',(25.7453222430615,-0.918150438689142,
26.9146737579895));
#43339=CARTESIAN_POINT('Ctrl Pts',(25.734736707561,-0.826434186032542,27.0515675368345));
#43340=CARTESIAN_POINT('Ctrl Pts',(25.7135656365599,-0.643001680719363,
27.3253550945245));
#43341=CARTESIAN_POINT('Ctrl Pts',(25.6923945655588,-0.315369527813967,
27.4975992450292));
#43342=CARTESIAN_POINT('Ctrl Pts',(25.6712234945578,0.0141607649234293,
27.4934886431632));
#43343=CARTESIAN_POINT('Ctrl Pts',(25.6606379590572,0.178925911292108,27.4914333422301));
#43344=CARTESIAN_POINT('Ctrl Pts',(25.6500524235567,0.344165592618783,27.4452893532044));
#43345=CARTESIAN_POINT('Ctrl Pts',(25.6394668880562,0.488039692138768,27.3638892577079));
#43346=CARTESIAN_POINT('Ctrl Pts',(25.6288813525557,0.631913791658785,27.2824891622114));
#43347=CARTESIAN_POINT('Ctrl Pts',(25.6182958170551,0.754422309372096,27.1658329602441));
#43348=CARTESIAN_POINT('Ctrl Pts',(25.6077102815546,0.841702064697562,27.0261284257574));
#43349=CARTESIAN_POINT('Ctrl Pts',(25.5971247460541,0.928981820023017,26.8864238912708));
#43350=CARTESIAN_POINT('Ctrl Pts',(25.5865392105535,0.981032812960631,26.7236710242649));
#43351=CARTESIAN_POINT('Ctrl Pts',(25.575953675053,0.990910358314731,26.5588517978137));
#43352=CARTESIAN_POINT('Ctrl Pts',(25.5653681395525,1.00078790366883,26.3940325713625));
#43353=CARTESIAN_POINT('Ctrl Pts',(25.5547826040519,0.968492001439414,26.227146985466));
#43354=CARTESIAN_POINT('Ctrl Pts',(25.5441970685514,0.898277408587982,26.0778928100537));
#43355=CARTESIAN_POINT('Ctrl Pts',(25.5336115330509,0.82806281573653,25.9286386346413));
#43356=CARTESIAN_POINT('Ctrl Pts',(25.5230259975503,0.719929532263041,25.7970158697132));
#43357=CARTESIAN_POINT('Ctrl Pts',(25.5124404620498,0.586893434433857,25.6994415131927));
#43358=CARTESIAN_POINT('Ctrl Pts',(25.5018549265493,0.453857336604717,25.6018671566723));
#43359=CARTESIAN_POINT('Ctrl Pts',(25.4912693910487,0.295918424419905,25.5383412085594));
#43360=CARTESIAN_POINT('Ctrl Pts',(25.4806838555482,0.132391755440172,25.5163321704302));
#43361=CARTESIAN_POINT('Ctrl Pts',(25.4700983200477,-0.0311349135395798,
25.494323132301));
#43362=CARTESIAN_POINT('Ctrl Pts',(25.4595127845471,-0.200249339314248,
25.5138310041554));
#43363=CARTESIAN_POINT('Ctrl Pts',(25.4489272490466,-0.354349175992256,
25.572759763783));
#43364=CARTESIAN_POINT('Ctrl Pts',(25.4383417135461,-0.508449012670264,
25.6316885234106));
#43365=CARTESIAN_POINT('Ctrl Pts',(25.4277561780455,-0.647534260251607,
25.7300381708114));
#43366=CARTESIAN_POINT('Ctrl Pts',(25.417170642545,-0.754711704727708,25.8554171695454));
#43367=CARTESIAN_POINT('Ctrl Pts',(25.4065851070445,-0.861889149203809,
25.9807961682795));
#43368=CARTESIAN_POINT('Ctrl Pts',(25.3959995715439,-0.937158790574664,
26.1332045183467));
#43369=CARTESIAN_POINT('Ctrl Pts',(25.3854140360434,-0.971209370808219,
26.2947702984376));
#43370=CARTESIAN_POINT('Ctrl Pts',(25.380998283241,-0.985413559635735,26.3621674127521));
#43371=CARTESIAN_POINT('Ctrl Pts',(25.3765825304386,-0.992445060532609,
26.4311580468119));
#43372=CARTESIAN_POINT('Ctrl Pts',(25.3721667776362,-0.992387361158253,
26.5001400376411));
#43373=CARTESIAN_POINT('Ctrl Pts',(25.2278332223638,-0.99258529737825,26.5000026553357));
#43374=CARTESIAN_POINT('Ctrl Pts',(25.2382833075259,-0.992560342141212,
26.3371281002211));
#43375=CARTESIAN_POINT('Ctrl Pts',(25.248733392688,-0.951649173128032,26.1742414680339));
#43376=CARTESIAN_POINT('Ctrl Pts',(25.2591834778501,-0.874644658184562,
26.0307202723029));
#43377=CARTESIAN_POINT('Ctrl Pts',(25.2697926807484,-0.796467637572248,
25.8850137577537));
#43378=CARTESIAN_POINT('Ctrl Pts',(25.2804018836467,-0.681089755662396,
25.7592669032749));
#43379=CARTESIAN_POINT('Ctrl Pts',(25.2910110865449,-0.542632340541926,
25.6688701160972));
#43380=CARTESIAN_POINT('Ctrl Pts',(25.3016202894432,-0.404174925421455,
25.5784733289195));
#43381=CARTESIAN_POINT('Ctrl Pts',(25.3122294923414,-0.242637977090366,
25.5234266090428));
#43382=CARTESIAN_POINT('Ctrl Pts',(25.3228386952397,-0.0777923234385866,
25.5104672338259));
#43383=CARTESIAN_POINT('Ctrl Pts',(25.333447898138,0.0870533302131832,25.4975078586089));
#43384=CARTESIAN_POINT('Ctrl Pts',(25.3440571010363,0.255207689185642,25.5266358280516));
#43385=CARTESIAN_POINT('Ctrl Pts',(25.3546663039346,0.406090007559484,25.5942861121311));
#43386=CARTESIAN_POINT('Ctrl Pts',(25.3652755068328,0.556972325933344,25.6619363962105));
#43387=CARTESIAN_POINT('Ctrl Pts',(25.3758847097311,0.690582603708582,25.7681089949267));
#43388=CARTESIAN_POINT('Ctrl Pts',(25.3864939126294,0.790568013661987,25.8998092330827));
#43389=CARTESIAN_POINT('Ctrl Pts',(25.3971031155276,0.890553423615392,26.0315094712387));
#43390=CARTESIAN_POINT('Ctrl Pts',(25.4077123184259,0.956913965746965,26.1887373488345));
#43391=CARTESIAN_POINT('Ctrl Pts',(25.4183215213242,0.98152764152502,26.3522494337047));
#43392=CARTESIAN_POINT('Ctrl Pts',(25.4289307242225,1.00614131730307,26.5157615185749));
#43393=CARTESIAN_POINT('Ctrl Pts',(25.4395399271207,0.989008126727611,26.6855578107195));
#43394=CARTESIAN_POINT('Ctrl Pts',(25.450149130019,0.932225035016547,26.8408566047574));
#43395=CARTESIAN_POINT('Ctrl Pts',(25.4607583329173,0.875441943305496,26.9961553987952));
#43396=CARTESIAN_POINT('Ctrl Pts',(25.4713675358156,0.779008950458864,27.1369566947264));
#43397=CARTESIAN_POINT('Ctrl Pts',(25.4819767387138,0.654728681970098,27.2460275423359));
#43398=CARTESIAN_POINT('Ctrl Pts',(25.4925859416121,0.530448413481304,27.3550983899455));
#43399=CARTESIAN_POINT('Ctrl Pts',(25.5031951445104,0.378320869350364,27.4324387892333));
#43400=CARTESIAN_POINT('Ctrl Pts',(25.5138043474086,0.216965241801435,27.4685828951456));
#43401=CARTESIAN_POINT('Ctrl Pts',(25.5244135503069,0.0556096142525066,
27.5047270010579));
#43402=CARTESIAN_POINT('Ctrl Pts',(25.5350227532052,-0.11497409671441,27.4996748135948));
#43403=CARTESIAN_POINT('Ctrl Pts',(25.5456319561035,-0.273907811964552,
27.4540446800138));
#43404=CARTESIAN_POINT('Ctrl Pts',(25.5562411590017,-0.432841527214676,
27.4084145464327));
#43405=CARTESIAN_POINT('Ctrl Pts',(25.5668503619,-0.580125246748027,27.3222064667338));
#43406=CARTESIAN_POINT('Ctrl Pts',(25.5774595647983,-0.697732623652709,
27.2059716189829));
#43407=CARTESIAN_POINT('Ctrl Pts',(25.5880687676965,-0.815340000557391,
27.0897367712321));
#43408=CARTESIAN_POINT('Ctrl Pts',(25.5986779705948,-0.903271034833404,
26.9434751554294));
#43409=CARTESIAN_POINT('Ctrl Pts',(25.6092871734931,-0.950763672578241,
26.7850880211867));
#43410=CARTESIAN_POINT('Ctrl Pts',(25.6154691897833,-0.978437783726829,
26.692795334032));
#43411=CARTESIAN_POINT('Ctrl Pts',(25.6216512060736,-0.992381320457257,
26.5963855119862));
#43412=CARTESIAN_POINT('Ctrl Pts',(25.6278332223638,-0.99242346011951,26.4999876204483));
#43413=CARTESIAN_POINT('Origin',(18.,0.,26.5));
#43414=CARTESIAN_POINT('',(26.1721667776362,-0.993011273520018,26.5001944908134));
#43415=CARTESIAN_POINT('',(26.0278332223638,-0.992541444115404,26.5000219547962));
#43416=CARTESIAN_POINT('',(18.,-0.9925,26.5));
#43417=CARTESIAN_POINT('Ctrl Pts',(26.1721667776362,-0.993011273520018,
26.5001944908134));
#43418=CARTESIAN_POINT('Ctrl Pts',(26.1533831802842,-0.990681442009467,
26.7921974358648));
#43419=CARTESIAN_POINT('Ctrl Pts',(26.1345995829321,-0.855424830611663,
27.0830337592609));
#43420=CARTESIAN_POINT('Ctrl Pts',(26.1158159855801,-0.629544085260756,
27.2686969039528));
#43421=CARTESIAN_POINT('Ctrl Pts',(26.1052304500796,-0.502248519667636,
27.3733277567359));
#43422=CARTESIAN_POINT('Ctrl Pts',(26.0946449145791,-0.346171548785687,
27.4445565592068));
#43423=CARTESIAN_POINT('Ctrl Pts',(26.0840593790785,-0.183705030547387,
27.4750588526323));
#43424=CARTESIAN_POINT('Ctrl Pts',(26.073473843578,-0.0212385123090691,
27.5055611460579));
#43425=CARTESIAN_POINT('Ctrl Pts',(26.0628883080775,0.147617553285602,27.495336930438));
#43426=CARTESIAN_POINT('Ctrl Pts',(26.0523027725769,0.304395987274318,27.4447838493567));
#43427=CARTESIAN_POINT('Ctrl Pts',(26.0417172370764,0.461174421263017,27.3942307682754));
#43428=CARTESIAN_POINT('Ctrl Pts',(26.0311317015759,0.605875223645765,27.3033488217328));
#43429=CARTESIAN_POINT('Ctrl Pts',(26.0205461660753,0.719664201221994,27.1837034248472));
#43430=CARTESIAN_POINT('Ctrl Pts',(26.0099606305748,0.833453178798223,27.0640580279616));
#43431=CARTESIAN_POINT('Ctrl Pts',(25.9993750950743,0.916330331567933,26.915649180733));
#43432=CARTESIAN_POINT('Ctrl Pts',(25.9887895595738,0.958852278036404,26.7562792338966));
#43433=CARTESIAN_POINT('Ctrl Pts',(25.9782040240732,1.00137422450488,26.5969092870601));
#43434=CARTESIAN_POINT('Ctrl Pts',(25.9676184885727,1.00354096467211,26.4265782406157));
#43435=CARTESIAN_POINT('Ctrl Pts',(25.9570329530721,0.964721792019372,26.2662272832873));
#43436=CARTESIAN_POINT('Ctrl Pts',(25.9464474175716,0.925902619366637,26.1058763259588));
#43437=CARTESIAN_POINT('Ctrl Pts',(25.9358618820711,0.846097533893935,25.9555054577463));
#43438=CARTESIAN_POINT('Ctrl Pts',(25.9252763465706,0.73525991827821,25.8332745556996));
#43439=CARTESIAN_POINT('Ctrl Pts',(25.91469081107,0.624422302662473,25.7110436536529));
#43440=CARTESIAN_POINT('Ctrl Pts',(25.9041052755695,0.482552156903705,25.616952717772));
#43441=CARTESIAN_POINT('Ctrl Pts',(25.8935197400689,0.326751952924584,25.5626788394154));
#43442=CARTESIAN_POINT('Ctrl Pts',(25.8829342045684,0.170951748945481,25.5084049610588));
#43443=CARTESIAN_POINT('Ctrl Pts',(25.8723486690679,0.00122148674602748,
25.4939481402265));
#43444=CARTESIAN_POINT('Ctrl Pts',(25.8617631335674,-0.161535973435497,
25.5207232708255));
#43445=CARTESIAN_POINT('Ctrl Pts',(25.8511775980668,-0.324293433617022,
25.5474984014245));
#43446=CARTESIAN_POINT('Ctrl Pts',(25.8405920625663,-0.480078091780619,
25.6155054834548));
#43447=CARTESIAN_POINT('Ctrl Pts',(25.8300065270658,-0.610251400009936,
25.7170823159535));
#43448=CARTESIAN_POINT('Ctrl Pts',(25.8194209915652,-0.740424708239253,
25.8186591484523));
#43449=CARTESIAN_POINT('Ctrl Pts',(25.8088354560647,-0.84498666653429,25.9538057314195));
#43450=CARTESIAN_POINT('Ctrl Pts',(25.7982499205642,-0.910590061577954,
26.1049060532897));
#43451=CARTESIAN_POINT('Ctrl Pts',(25.7895555395882,-0.964473108855015,
26.2290116088253));
#43452=CARTESIAN_POINT('Ctrl Pts',(25.7808611586122,-0.992074386806777,
26.3638796887133));
#43453=CARTESIAN_POINT('Ctrl Pts',(25.7721667776362,-0.9921765548274,26.4993478195649));
#43454=CARTESIAN_POINT('Ctrl Pts',(25.6278332223638,-0.99242346011951,26.4999876204483));
#43455=CARTESIAN_POINT('Ctrl Pts',(25.6322604089718,-0.992453637999935,
26.4309532739789));
#43456=CARTESIAN_POINT('Ctrl Pts',(25.6366875955799,-0.985354402214821,
26.361925046141));
#43457=CARTESIAN_POINT('Ctrl Pts',(25.6411147821879,-0.971063013632482,
26.2944194453005));
#43458=CARTESIAN_POINT('Ctrl Pts',(25.6517239850862,-0.936815475728224,
26.1326506563395));
#43459=CARTESIAN_POINT('Ctrl Pts',(25.6623331879844,-0.861266158706048,
25.9796257311001));
#43460=CARTESIAN_POINT('Ctrl Pts',(25.6729423908827,-0.753661693496502,
25.8540736940781));
#43461=CARTESIAN_POINT('Ctrl Pts',(25.683551593781,-0.646057228286968,25.7285216570561));
#43462=CARTESIAN_POINT('Ctrl Pts',(25.6941607966793,-0.506397614890069,
25.6304425082515));
#43463=CARTESIAN_POINT('Ctrl Pts',(25.7047699995776,-0.351776070742455,
25.571840349425));
#43464=CARTESIAN_POINT('Ctrl Pts',(25.7153792024758,-0.197154526594824,
25.5132381905986));
#43465=CARTESIAN_POINT('Ctrl Pts',(25.7259884053741,-0.0275710516964692,
25.4941130217504));
#43466=CARTESIAN_POINT('Ctrl Pts',(25.7365976082724,0.136218695723237,25.5168056103299));
#43467=CARTESIAN_POINT('Ctrl Pts',(25.7472068111706,0.300008443142944,25.5394981989094));
#43468=CARTESIAN_POINT('Ctrl Pts',(25.7578160140689,0.458004463084008,25.6040085449167));
#43469=CARTESIAN_POINT('Ctrl Pts',(25.7684252169672,0.59086930886453,25.7024410988939));
#43470=CARTESIAN_POINT('Ctrl Pts',(25.7790344198655,0.723734154645037,25.8008736528711));
#43471=CARTESIAN_POINT('Ctrl Pts',(25.7896436227637,0.831467826265013,25.9332284148183));
#43472=CARTESIAN_POINT('Ctrl Pts',(25.800252825662,0.900884585808005,26.0833062227837));
#43473=CARTESIAN_POINT('Ctrl Pts',(25.8108620285603,0.970301345351009,26.2333840307492));
#43474=CARTESIAN_POINT('Ctrl Pts',(25.8214712314585,1.00140119281702,26.401184884733));
#43475=CARTESIAN_POINT('Ctrl Pts',(25.8320804343568,0.9903777559402,26.5661713046231));
#43476=CARTESIAN_POINT('Ctrl Pts',(25.8426896372551,0.979354319063382,26.7311577245132));
#43477=CARTESIAN_POINT('Ctrl Pts',(25.8532988401534,0.926207597843734,26.8933297103096));
#43478=CARTESIAN_POINT('Ctrl Pts',(25.8639080430516,0.837442325363041,27.0328387113249));
#43479=CARTESIAN_POINT('Ctrl Pts',(25.8745172459499,0.748677052882357,27.1723477123403));
#43480=CARTESIAN_POINT('Ctrl Pts',(25.8851264488482,0.624293229140633,27.2891937285746));
#43481=CARTESIAN_POINT('Ctrl Pts',(25.8957356517464,0.47951443670336,27.3690757427456));
#43482=CARTESIAN_POINT('Ctrl Pts',(25.9063448546447,0.334735644266086,27.4489577569167));
#43483=CARTESIAN_POINT('Ctrl Pts',(25.916954057543,0.169561883133259,27.4918757690245));
#43484=CARTESIAN_POINT('Ctrl Pts',(25.9275632604413,0.00420909911851084,
27.4925769608318));
#43485=CARTESIAN_POINT('Ctrl Pts',(25.9381724633395,-0.161143684896257,
27.4932781526391));
#43486=CARTESIAN_POINT('Ctrl Pts',(25.9487816662378,-0.326675491792952,
27.4517625241458));
#43487=CARTESIAN_POINT('Ctrl Pts',(25.9593908691361,-0.472126557242158,
27.3731112508604));
#43488=CARTESIAN_POINT('Ctrl Pts',(25.9700000720343,-0.617577622691365,
27.2944599775749));
#43489=CARTESIAN_POINT('Ctrl Pts',(25.9806092749326,-0.742947946693088,
27.1786730594973));
#43490=CARTESIAN_POINT('Ctrl Pts',(25.9912184778309,-0.832893202112376,
27.0399218963483));
#43491=CARTESIAN_POINT('Ctrl Pts',(26.0018276807292,-0.922838457531644,
26.9011707331994));
#43492=CARTESIAN_POINT('Ctrl Pts',(26.0124368836274,-0.977358644368497,
26.7394553249791));
#43493=CARTESIAN_POINT('Ctrl Pts',(26.0230460865257,-0.98978093665147,26.5745683248608));
#43494=CARTESIAN_POINT('Ctrl Pts',(26.0246417984717,-0.991649352250928,
26.5497679549974));
#43495=CARTESIAN_POINT('Ctrl Pts',(26.0262375104178,-0.992565401903803,
26.5248958353196));
#43496=CARTESIAN_POINT('Ctrl Pts',(26.0278332223638,-0.992541444115404,
26.5000219547962));
#43497=CARTESIAN_POINT('Origin',(8.83329938588935,0.,26.5));
#43498=CARTESIAN_POINT('',(26.2332993858894,-0.764743745002543,26.5001497824216));
#43499=CARTESIAN_POINT('',(26.3667006141106,-0.764336903008391,26.49996577981));
#43500=CARTESIAN_POINT('',(8.83329938588935,-0.76435,26.5000000000004));
#43501=CARTESIAN_POINT('',(26.4075,0.702460755335647,26.1986212829383));
#43502=CARTESIAN_POINT('Ctrl Pts',(26.2332993858894,-0.764743745002462,
26.5001497824216));
#43503=CARTESIAN_POINT('Ctrl Pts',(26.2356868595384,-0.764971803409263,
26.4715667170256));
#43504=CARTESIAN_POINT('Ctrl Pts',(26.248659868688,-0.757224410481673,26.3161737266801));
#43505=CARTESIAN_POINT('Ctrl Pts',(26.2722184133381,-0.650892539114633,
26.0420259586536));
#43506=CARTESIAN_POINT('Ctrl Pts',(26.3039750198397,-0.355044020423166,
25.7866217100636));
#43507=CARTESIAN_POINT('Ctrl Pts',(26.3357316263413,0.0308983993041465,
25.7036133259667));
#43508=CARTESIAN_POINT('Ctrl Pts',(26.3674882328429,0.407379290301616,25.8154783693755));
#43509=CARTESIAN_POINT('Ctrl Pts',(26.3914110240625,0.616973295240833,26.0251266306013));
#43510=CARTESIAN_POINT('Ctrl Pts',(26.4047482797815,0.689468221294098,26.1682460674036));
#43511=CARTESIAN_POINT('Ctrl Pts',(26.4075,0.702460755335573,26.1986212829383));
#43512=CARTESIAN_POINT('',(26.4075,-0.612682133358436,26.0429972363723));
#43513=CARTESIAN_POINT('Origin',(26.4075,0.,26.5));
#43514=CARTESIAN_POINT('Ctrl Pts',(26.3667006141105,-0.764336903008216,
26.49996577981));
#43515=CARTESIAN_POINT('Ctrl Pts',(26.3696912065087,-0.76437156972657,26.4640569586302));
#43516=CARTESIAN_POINT('Ctrl Pts',(26.3832910018052,-0.75307130558971,26.3007912409091));
#43517=CARTESIAN_POINT('Ctrl Pts',(26.3968907971017,-0.688841172942706,
26.1451000824837));
#43518=CARTESIAN_POINT('Ctrl Pts',(26.4075,-0.612682133358295,26.0429972363724));
#43519=CARTESIAN_POINT('Origin',(8.83329938588935,0.,26.5));
#43520=CARTESIAN_POINT('',(25.8332993858893,-0.76410090648093,26.4994977389265));
#43521=CARTESIAN_POINT('',(25.9667006141106,-0.764381917188524,26.5000169079586));
#43522=CARTESIAN_POINT('',(8.83329938588935,-0.76435,26.5000000000004));
#43523=CARTESIAN_POINT('Ctrl Pts',(25.8332993858894,-0.764100906480849,
26.4994977389265));
#43524=CARTESIAN_POINT('Ctrl Pts',(25.8419937668654,-0.764022224237484,
26.3951702166934));
#43525=CARTESIAN_POINT('Ctrl Pts',(25.8612736833419,-0.716885713953257,
26.1648471626025));
#43526=CARTESIAN_POINT('Ctrl Pts',(25.8911391353189,-0.489694400926831,
25.8712018432531));
#43527=CARTESIAN_POINT('Ctrl Pts',(25.9228957418205,-0.129772979866902,
25.714079788392));
#43528=CARTESIAN_POINT('Ctrl Pts',(25.9546523483221,0.262368055635802,25.7474805067894));
#43529=CARTESIAN_POINT('Ctrl Pts',(25.9864089548237,0.590141695668152,25.9648661194057));
#43530=CARTESIAN_POINT('Ctrl Pts',(26.0181655613253,0.774521596165084,26.3122796401661));
#43531=CARTESIAN_POINT('Ctrl Pts',(26.0499221678269,0.769515607711255,26.7058087142711));
#43532=CARTESIAN_POINT('Ctrl Pts',(26.0816787743285,0.5780380710276,27.0486892252408));
#43533=CARTESIAN_POINT('Ctrl Pts',(26.1134353808301,0.243724544676253,27.2586608600213));
#43534=CARTESIAN_POINT('Ctrl Pts',(26.1451919873318,-0.146396766368369,
27.282282661157));
#43535=CARTESIAN_POINT('Ctrl Pts',(26.1851466556847,-0.600082663475827,
27.0752341583171));
#43536=CARTESIAN_POINT('Ctrl Pts',(26.2145157885374,-0.762949481309626,
26.7250288263006));
#43537=CARTESIAN_POINT('Ctrl Pts',(26.2332993858894,-0.764743745002462,
26.5001497824216));
#43538=CARTESIAN_POINT('Ctrl Pts',(25.9667006141105,-0.764381917188349,
26.5000169079586));
#43539=CARTESIAN_POINT('Ctrl Pts',(25.9757141050628,-0.764277698162404,
26.3918127800182));
#43540=CARTESIAN_POINT('Ctrl Pts',(25.9953367989134,-0.713766127520463,
26.1561543088668));
#43541=CARTESIAN_POINT('Ctrl Pts',(26.0255686956621,-0.479811640722421,
25.8637012684045));
#43542=CARTESIAN_POINT('Ctrl Pts',(26.057396304357,-0.116058362262509,25.7115674057289));
#43543=CARTESIAN_POINT('Ctrl Pts',(26.0892239130518,0.276104304993651,25.7524295460381));
#43544=CARTESIAN_POINT('Ctrl Pts',(26.1210515217466,0.600680758111244,25.9762843069252));
#43545=CARTESIAN_POINT('Ctrl Pts',(26.1528791304414,0.778220766932473,26.3283374916096));
#43546=CARTESIAN_POINT('Ctrl Pts',(26.1847067391362,0.765263715417021,26.7224086099901));
#43547=CARTESIAN_POINT('Ctrl Pts',(26.216534347831,0.564984430859093,27.0620420026143));
#43548=CARTESIAN_POINT('Ctrl Pts',(26.2483619565259,0.226402125810272,27.2640883311776));
#43549=CARTESIAN_POINT('Ctrl Pts',(26.2801895652207,-0.167592445455861,
27.2791135571752));
#43550=CARTESIAN_POINT('Ctrl Pts',(26.3120171739155,-0.520576980781025,
27.1033949839955));
#43551=CARTESIAN_POINT('Ctrl Pts',(26.3408541902121,-0.724914826684035,
26.8104148753484));
#43552=CARTESIAN_POINT('Ctrl Pts',(26.3590820036105,-0.764248588657984,
26.591444418708));
#43553=CARTESIAN_POINT('Ctrl Pts',(26.3667006141105,-0.764336903008216,
26.49996577981));
#43554=CARTESIAN_POINT('Origin',(8.83329938588935,0.,26.5));
#43555=CARTESIAN_POINT('',(25.4332993858893,-0.764263253905602,26.5001078466209));
#43556=CARTESIAN_POINT('',(25.5667006141106,-0.76429105465224,26.4999904661865));
#43557=CARTESIAN_POINT('',(8.83329938588935,-0.76435,26.5000000000004));
#43558=CARTESIAN_POINT('Ctrl Pts',(25.4332993858894,-0.764263253905522,
26.5001078466209));
#43559=CARTESIAN_POINT('Ctrl Pts',(25.4377151386918,-0.764307689690715,
26.4469830257742));
#43560=CARTESIAN_POINT('Ctrl Pts',(25.4527164269947,-0.745911257864019,
26.2664836537655));
#43561=CARTESIAN_POINT('Ctrl Pts',(25.4783032507982,-0.605796091498349,
25.9827740341064));
#43562=CARTESIAN_POINT('Ctrl Pts',(25.5100598572998,-0.284456618484401,
25.7555491887942));
#43563=CARTESIAN_POINT('Ctrl Pts',(25.5418164638014,0.106261602193242,25.710478634078));
#43564=CARTESIAN_POINT('Ctrl Pts',(25.5735730703029,0.471160163992154,25.857247576466));
#43565=CARTESIAN_POINT('Ctrl Pts',(25.6053296768046,0.720988905220201,26.1613458949732));
#43566=CARTESIAN_POINT('Ctrl Pts',(25.6370862833062,0.795604641852137,26.5469146534013));
#43567=CARTESIAN_POINT('Ctrl Pts',(25.6688428898078,0.675347181544284,26.9229352697116));
#43568=CARTESIAN_POINT('Ctrl Pts',(25.7005994963094,0.392306217773594,27.1924551729066));
#43569=CARTESIAN_POINT('Ctrl Pts',(25.7429416383115,-0.116715244884512,
27.3346019054481));
#43570=CARTESIAN_POINT('Ctrl Pts',(25.7852837803136,-0.621351287349472,
27.0693025272348));
#43571=CARTESIAN_POINT('Ctrl Pts',(25.8189315413398,-0.757620506138495,
26.6720477734371));
#43572=CARTESIAN_POINT('Ctrl Pts',(25.8314082313648,-0.764118021015047,
26.5221904948858));
#43573=CARTESIAN_POINT('Ctrl Pts',(25.8332993858894,-0.764100906480849,
26.4994977389265));
#43574=CARTESIAN_POINT('Ctrl Pts',(25.5667006141106,-0.764291054652064,
26.4999904661865));
#43575=CARTESIAN_POINT('Ctrl Pts',(25.5711278007186,-0.764314295420762,
26.4468253249029));
#43576=CARTESIAN_POINT('Ctrl Pts',(25.5861641902249,-0.745745270709442,
26.2662725291791));
#43577=CARTESIAN_POINT('Ctrl Pts',(25.6118097826295,-0.605100924877577,
25.9813978095313));
#43578=CARTESIAN_POINT('Ctrl Pts',(25.6436373913244,-0.282434449814925,
25.7547979181797));
#43579=CARTESIAN_POINT('Ctrl Pts',(25.6754650000191,0.109367451560953,25.710611552006));
#43580=CARTESIAN_POINT('Ctrl Pts',(25.707292608714,0.474397953853924,25.8596548254688));
#43581=CARTESIAN_POINT('Ctrl Pts',(25.7391202174087,0.723303440713549,26.1654443336632));
#43582=CARTESIAN_POINT('Ctrl Pts',(25.7709478261036,0.795155838932149,26.553127707192));
#43583=CARTESIAN_POINT('Ctrl Pts',(25.8027754347984,0.672366832289694,26.9278062684317));
#43584=CARTESIAN_POINT('Ctrl Pts',(25.8346030434933,0.384993203039443,27.1977647143017));
#43585=CARTESIAN_POINT('Ctrl Pts',(25.8664306521881,0.00337940660061129,
27.2969215381445));
#43586=CARTESIAN_POINT('Ctrl Pts',(25.8982582608829,-0.379061610834525,
27.2010047503193));
#43587=CARTESIAN_POINT('Ctrl Pts',(25.9300858695777,-0.668714428418505,
26.9334932213543));
#43588=CARTESIAN_POINT('Ctrl Pts',(25.9528999873202,-0.759004503313977,
26.6656787260802));
#43589=CARTESIAN_POINT('Ctrl Pts',(25.9651049021645,-0.764400367702759,
26.5191729286921));
#43590=CARTESIAN_POINT('Ctrl Pts',(25.9667006141105,-0.764381917188349,
26.5000169079586));
#43591=CARTESIAN_POINT('Origin',(8.83329938588935,0.,26.5));
#43592=CARTESIAN_POINT('',(25.0332993858893,-0.764359839502163,26.5000448214614));
#43593=CARTESIAN_POINT('',(25.1667006141106,-0.764415689723997,26.5000020449434));
#43594=CARTESIAN_POINT('',(8.83329938588935,-0.76435,26.5000000000004));
#43595=CARTESIAN_POINT('Ctrl Pts',(25.0332993858894,-0.764359839502083,
26.5000448214614));
#43596=CARTESIAN_POINT('Ctrl Pts',(25.0334365105182,-0.764359396665192,
26.4983993445537));
#43597=CARTESIAN_POINT('Ctrl Pts',(25.0441591706476,-0.763902763666039,
26.3697273014672));
#43598=CARTESIAN_POINT('Ctrl Pts',(25.0654673662775,-0.697329274606203,
26.1141833843906));
#43599=CARTESIAN_POINT('Ctrl Pts',(25.097223972779,-0.427657617209193,25.827880607489));
#43600=CARTESIAN_POINT('Ctrl Pts',(25.1289805792807,-0.0540728476927859,
25.7048907589234));
#43601=CARTESIAN_POINT('Ctrl Pts',(25.1607371857822,0.33294494419036,25.7763569468244));
#43602=CARTESIAN_POINT('Ctrl Pts',(25.1924937922838,0.638517242951082,26.0230477368148));
#43603=CARTESIAN_POINT('Ctrl Pts',(25.2242503987854,0.788945293266577,26.3880474112795));
#43604=CARTESIAN_POINT('Ctrl Pts',(25.256007005287,0.746270734187485,26.7765471503739));
#43605=CARTESIAN_POINT('Ctrl Pts',(25.2983491472892,0.44872275221358,27.2133236857863));
#43606=CARTESIAN_POINT('Ctrl Pts',(25.3406912892913,-0.108098811743075,
27.335761590382));
#43607=CARTESIAN_POINT('Ctrl Pts',(25.3830334312934,-0.561424858091366,
27.0640926021514));
#43608=CARTESIAN_POINT('Ctrl Pts',(25.4103742849926,-0.735087659068443,
26.7758787289326));
#43609=CARTESIAN_POINT('Ctrl Pts',(25.4271296031913,-0.764201167291771,
26.5743349637552));
#43610=CARTESIAN_POINT('Ctrl Pts',(25.4332993858894,-0.764263253905522,
26.5001078466209));
#43611=CARTESIAN_POINT('Ctrl Pts',(25.1667006141106,-0.764415689723821,
26.5000020449434));
#43612=CARTESIAN_POINT('Ctrl Pts',(25.1771506992727,-0.764396471048405,
26.3745681243369));
#43613=CARTESIAN_POINT('Ctrl Pts',(25.1982099873331,-0.700903229582064,
26.1217716260069));
#43614=CARTESIAN_POINT('Ctrl Pts',(25.2298784782917,-0.435669391136255,
25.832701309116));
#43615=CARTESIAN_POINT('Ctrl Pts',(25.2617060869866,-0.0624580063800852,
25.705522587692));
#43616=CARTESIAN_POINT('Ctrl Pts',(25.2935336956813,0.326042097238796,25.7728192026347));
#43617=CARTESIAN_POINT('Ctrl Pts',(25.3253613043762,0.634732321372251,26.0181180212604));
#43618=CARTESIAN_POINT('Ctrl Pts',(25.357188913071,0.78805024694888,26.3813738245058));
#43619=CARTESIAN_POINT('Ctrl Pts',(25.3890165217658,0.748466103221927,26.7736674141299));
#43620=CARTESIAN_POINT('Ctrl Pts',(25.4208441304606,0.525669454106653,27.0989716072131));
#43621=CARTESIAN_POINT('Ctrl Pts',(25.4526717391554,0.174197348243338,27.2776571513812));
#43622=CARTESIAN_POINT('Ctrl Pts',(25.4844993478503,-0.219915476373876,
27.2659846894545));
#43623=CARTESIAN_POINT('Ctrl Pts',(25.5163269565451,-0.560196517256405,
27.0668114530277));
#43624=CARTESIAN_POINT('Ctrl Pts',(25.5437273786318,-0.735091936016483,
26.7758961151728));
#43625=CARTESIAN_POINT('Ctrl Pts',(25.5605185978203,-0.764258601804826,
26.5742289834629));
#43626=CARTESIAN_POINT('Ctrl Pts',(25.5667006141106,-0.764291054652064,
26.4999904661865));
#43627=CARTESIAN_POINT('Origin',(8.83329938588935,0.,26.5));
#43628=CARTESIAN_POINT('',(24.6332993858894,-0.76435,26.5000000000003));
#43629=CARTESIAN_POINT('',(24.7667006141106,-0.764286798414632,26.5000062214473));
#43630=CARTESIAN_POINT('',(8.83329938588935,-0.76435,26.5000000000004));
#43631=CARTESIAN_POINT('Ctrl Pts',(24.6332993858894,-0.764326480586209,
26.5000191213087));
#43632=CARTESIAN_POINT('Ctrl Pts',(24.6397434178451,-0.764258932917326,
26.4226419695689));
#43633=CARTESIAN_POINT('Ctrl Pts',(24.6567729853014,-0.733280117843162,
26.2181201080417));
#43634=CARTESIAN_POINT('Ctrl Pts',(24.6843880882583,-0.553842691960536,
25.9269547568778));
#43635=CARTESIAN_POINT('Ctrl Pts',(24.7161446947598,-0.211884413187848,
25.7321350380964));
#43636=CARTESIAN_POINT('Ctrl Pts',(24.7479013012615,0.180748963367304,25.7237799647362));
#43637=CARTESIAN_POINT('Ctrl Pts',(24.7796579077631,0.531025222621527,25.90587857232));
#43638=CARTESIAN_POINT('Ctrl Pts',(24.8114145142647,0.74881272581408,26.2304117273629));
#43639=CARTESIAN_POINT('Ctrl Pts',(24.8537566562668,0.802855019359397,26.7561378670706));
#43640=CARTESIAN_POINT('Ctrl Pts',(24.8960987982689,0.456057920405105,27.2086564487069));
#43641=CARTESIAN_POINT('Ctrl Pts',(24.9384409402711,-0.0656403540824771,
27.2931517376899));
#43642=CARTESIAN_POINT('Ctrl Pts',(24.9701975467727,-0.435634749553036,
27.1672259159165));
#43643=CARTESIAN_POINT('Ctrl Pts',(25.0018170286454,-0.701384614530829,
26.8775928202282));
#43644=CARTESIAN_POINT('Ctrl Pts',(25.0228509750177,-0.764393582104101,
26.6254243317562));
#43645=CARTESIAN_POINT('Ctrl Pts',(25.0332993858894,-0.764359839502083,
26.5000448214614));
#43646=CARTESIAN_POINT('Ctrl Pts',(24.7667006141106,-0.764286798414457,
26.5000062214473));
#43647=CARTESIAN_POINT('Ctrl Pts',(24.7725643949285,-0.764266847137901,
26.4295882043572));
#43648=CARTESIAN_POINT('Ctrl Pts',(24.7890373786446,-0.737166213800641,
26.2317494504216));
#43649=CARTESIAN_POINT('Ctrl Pts',(24.8161195652591,-0.568633391362849,
25.9416529507056));
#43650=CARTESIAN_POINT('Ctrl Pts',(24.8479471739539,-0.231377401638892,
25.7373992792821));
#43651=CARTESIAN_POINT('Ctrl Pts',(24.8797747826487,0.16251606740706,25.7198180410551));
#43652=CARTESIAN_POINT('Ctrl Pts',(24.9116023913435,0.516628208017037,25.8932128413441));
#43653=CARTESIAN_POINT('Ctrl Pts',(24.9434300000383,0.744278044004932,26.2151394122719));
#43654=CARTESIAN_POINT('Ctrl Pts',(24.9752576087332,0.78974054437337,26.6067952892288));
#43655=CARTESIAN_POINT('Ctrl Pts',(25.007085217428,0.641887217721265,26.9723093911354));
#43656=CARTESIAN_POINT('Ctrl Pts',(25.0389128261228,0.336910188567394,27.2222097244347));
#43657=CARTESIAN_POINT('Ctrl Pts',(25.0707404348176,-0.0505370546315667,
27.2953246930265));
#43658=CARTESIAN_POINT('Ctrl Pts',(25.1025680435124,-0.425613636882587,
27.1737569245123));
#43659=CARTESIAN_POINT('Ctrl Pts',(25.1343956522073,-0.696506822711343,
26.8872642600927));
#43660=CARTESIAN_POINT('Ctrl Pts',(25.15577317574,-0.763941742375046,26.6311655609095));
#43661=CARTESIAN_POINT('Ctrl Pts',(25.1665414963744,-0.764415982356089,
26.5019119587072));
#43662=CARTESIAN_POINT('Ctrl Pts',(25.1667006141106,-0.764415689723821,
26.5000020449434));
#43663=CARTESIAN_POINT('Origin',(8.83329938588935,0.,26.5));
#43664=CARTESIAN_POINT('',(24.2332993858894,-0.76435,26.5000000000003));
#43665=CARTESIAN_POINT('',(24.3667006141106,-0.764392673201869,26.4999855108973));
#43666=CARTESIAN_POINT('',(8.83329938588935,-0.76435,26.5000000000004));
#43667=CARTESIAN_POINT('Ctrl Pts',(24.2332993858894,-0.76435,26.5000000000003));
#43668=CARTESIAN_POINT('Ctrl Pts',(24.2511698941678,-0.764350000000088,
26.28543985601));
#43669=CARTESIAN_POINT('Ctrl Pts',(24.2690404024462,-0.669038051787615,
26.0726183635796));
#43670=CARTESIAN_POINT('Ctrl Pts',(24.2869109107247,-0.508962945483454,
25.9297477377293));
#43671=CARTESIAN_POINT('Ctrl Pts',(24.3047814190031,-0.348887839179292,
25.7868771118791));
#43672=CARTESIAN_POINT('Ctrl Pts',(24.3226519272816,-0.126643857468994,
25.716272808144));
#43673=CARTESIAN_POINT('Ctrl Pts',(24.34052243556,0.0865367472360207,25.7405644768133));
#43674=CARTESIAN_POINT('Ctrl Pts',(24.3583929438384,0.299717351941035,25.7648561454827));
#43675=CARTESIAN_POINT('Ctrl Pts',(24.3762634521169,0.500379634243882,25.8836500997622));
#43676=CARTESIAN_POINT('Ctrl Pts',(24.3941339603953,0.624208573182235,26.0588712436648));
#43677=CARTESIAN_POINT('Ctrl Pts',(24.4120044686738,0.748037512120589,26.2340923875675));
#43678=CARTESIAN_POINT('Ctrl Pts',(24.4298749769522,0.793026254288728,26.4629009717388));
#43679=CARTESIAN_POINT('Ctrl Pts',(24.4477454852306,0.744755289141838,26.671960698403));
#43680=CARTESIAN_POINT('Ctrl Pts',(24.4656159935091,0.696484323994948,26.8810204250673));
#43681=CARTESIAN_POINT('Ctrl Pts',(24.4834865017875,0.555735962611789,27.0669431344933));
#43682=CARTESIAN_POINT('Ctrl Pts',(24.501357010066,0.367621990370684,27.1701380415227));
#43683=CARTESIAN_POINT('Ctrl Pts',(24.5192275183444,0.179508018129579,27.2733329485521));
#43684=CARTESIAN_POINT('Ctrl Pts',(24.5370980266228,-0.0529228659408549,
27.2921276085011));
#43685=CARTESIAN_POINT('Ctrl Pts',(24.5549685349013,-0.255173367133682,
27.2204980743941));
#43686=CARTESIAN_POINT('Ctrl Pts',(24.5728390431797,-0.457423868326509,
27.1488685402871));
#43687=CARTESIAN_POINT('Ctrl Pts',(24.5907095514582,-0.626216181706892,
26.9879756875681));
#43688=CARTESIAN_POINT('Ctrl Pts',(24.6085800597366,-0.707450049624245,
26.7893878881133));
#43689=CARTESIAN_POINT('Ctrl Pts',(24.6168198351208,-0.744905549759095,
26.6978225651764));
#43690=CARTESIAN_POINT('Ctrl Pts',(24.6250596105051,-0.76434999999996,26.5989298885825));
#43691=CARTESIAN_POINT('Ctrl Pts',(24.6332993858894,-0.76435,26.5000000000003));
#43692=CARTESIAN_POINT('Ctrl Pts',(24.3667006141106,-0.764392673201694,
26.4999855108973));
#43693=CARTESIAN_POINT('Ctrl Pts',(24.3679780905843,-0.764405945073535,
26.4846504315273));
#43694=CARTESIAN_POINT('Ctrl Pts',(24.3798647699562,-0.760200367936652,
26.3419676628929));
#43695=CARTESIAN_POINT('Ctrl Pts',(24.4023606522264,-0.675139866205197,
26.076583512025));
#43696=CARTESIAN_POINT('Ctrl Pts',(24.4341882609213,-0.389531207732191,
25.8047584596478));
#43697=CARTESIAN_POINT('Ctrl Pts',(24.4660158696161,-0.00857155315095306,
25.7031173927703));
#43698=CARTESIAN_POINT('Ctrl Pts',(24.4978434783109,0.37448628025374,25.7965404154251));
#43699=CARTESIAN_POINT('Ctrl Pts',(24.5296710870057,0.66587587465148,26.0621590690836));
#43700=CARTESIAN_POINT('Ctrl Pts',(24.5614986957005,0.79426972782966,26.4349541647604));
#43701=CARTESIAN_POINT('Ctrl Pts',(24.5933263043954,0.728239082472559,26.8236714383262));
#43702=CARTESIAN_POINT('Ctrl Pts',(24.6251539130902,0.483947182200952,27.1331591317105));
#43703=CARTESIAN_POINT('Ctrl Pts',(24.656981521785,0.121192768603945,27.2876596181516));
#43704=CARTESIAN_POINT('Ctrl Pts',(24.6888091304798,-0.271227692226556,
27.2493536549575));
#43705=CARTESIAN_POINT('Ctrl Pts',(24.7206367391747,-0.597255961333821,
27.0276179279363));
#43706=CARTESIAN_POINT('Ctrl Pts',(24.7466005670515,-0.743954520432521,
26.7413759004361));
#43707=CARTESIAN_POINT('Ctrl Pts',(24.7619551920302,-0.76430294452074,26.5569938926328));
#43708=CARTESIAN_POINT('Ctrl Pts',(24.7667006141106,-0.764286798414457,
26.5000062214473));
#43709=CARTESIAN_POINT('Origin',(8.83329938588935,0.,26.5));
#43710=CARTESIAN_POINT('',(23.8332993858894,-0.764350202263794,26.5000021273756));
#43711=CARTESIAN_POINT('',(23.9667006141106,-0.764318926635532,26.5000181819409));
#43712=CARTESIAN_POINT('',(8.83329938588935,-0.76435,26.5000000000004));
#43713=CARTESIAN_POINT('Ctrl Pts',(23.8332993858894,-0.764350202263713,
26.5000021273756));
#43714=CARTESIAN_POINT('Ctrl Pts',(23.8417716969985,-0.764313879349882,
26.3983501280956));
#43715=CARTESIAN_POINT('Ctrl Pts',(23.8608295436081,-0.718603697792442,
26.1696958781128));
#43716=CARTESIAN_POINT('Ctrl Pts',(23.8904729257184,-0.495790608642908,
25.8761733171223));
#43717=CARTESIAN_POINT('Ctrl Pts',(23.9222295322199,-0.139108740631515,
25.7163884295363));
#43718=CARTESIAN_POINT('Ctrl Pts',(23.9645716742221,0.388186146399965,25.752006480776));
#43719=CARTESIAN_POINT('Ctrl Pts',(24.0069138162242,0.775559022505738,26.170316831385));
#43720=CARTESIAN_POINT('Ctrl Pts',(24.0492559582264,0.770636562786746,26.6987904001223));
#43721=CARTESIAN_POINT('Ctrl Pts',(24.0810125647279,0.583970020170633,27.0421688606243));
#43722=CARTESIAN_POINT('Ctrl Pts',(24.1127691712296,0.252144193813407,27.2560496256394));
#43723=CARTESIAN_POINT('Ctrl Pts',(24.1445257777311,-0.139564942859222,
27.2842405440908));
#43724=CARTESIAN_POINT('Ctrl Pts',(24.1762823842328,-0.498157324775064,
27.1220625835686));
#43725=CARTESIAN_POINT('Ctrl Pts',(24.2058735869521,-0.718613983320539,
26.8292929532382));
#43726=CARTESIAN_POINT('Ctrl Pts',(24.224879254171,-0.764289435210411,26.6010635220894));
#43727=CARTESIAN_POINT('Ctrl Pts',(24.2332993858894,-0.764406944917652,
26.4999838305765));
#43728=CARTESIAN_POINT('Ctrl Pts',(23.9667006141106,-0.764318926635357,
26.5000181819409));
#43729=CARTESIAN_POINT('Ctrl Pts',(23.9740009891383,-0.764242150819898,
26.4123586904196));
#43730=CARTESIAN_POINT('Ctrl Pts',(23.9919105670644,-0.727291940328121,
26.1972457893952));
#43731=CARTESIAN_POINT('Ctrl Pts',(24.0204293478886,-0.529560802386153,
25.9044660229636));
#43732=CARTESIAN_POINT('Ctrl Pts',(24.0522569565835,-0.179260354208531,
25.7234943099773));
#43733=CARTESIAN_POINT('Ctrl Pts',(24.0840845652783,0.214920155430682,25.7325987437994));
#43734=CARTESIAN_POINT('Ctrl Pts',(24.1159121739731,0.556491655837079,25.9295507049594));
#43735=CARTESIAN_POINT('Ctrl Pts',(24.1477397826679,0.761842918540557,26.2661395101813));
#43736=CARTESIAN_POINT('Ctrl Pts',(24.1795673913627,0.780707245874303,26.6599736149119));
#43737=CARTESIAN_POINT('Ctrl Pts',(24.2113950000576,0.608466952871163,27.0146487428259));
#43738=CARTESIAN_POINT('Ctrl Pts',(24.2432226087524,0.287283702529686,27.2433461074691));
#43739=CARTESIAN_POINT('Ctrl Pts',(24.2750502174472,-0.104221993505796,
27.2900842596193));
#43740=CARTESIAN_POINT('Ctrl Pts',(24.306877826142,-0.470215816038203,27.1434224487661));
#43741=CARTESIAN_POINT('Ctrl Pts',(24.3374279583631,-0.711038177639814,
26.8514693703178));
#43742=CARTESIAN_POINT('Ctrl Pts',(24.357368887686,-0.76429572466314,26.6120053941018));
#43743=CARTESIAN_POINT('Ctrl Pts',(24.3667006141106,-0.764392673201694,
26.4999855108973));
#43744=CARTESIAN_POINT('Origin',(8.83329938588935,0.,26.5));
#43745=CARTESIAN_POINT('',(23.4332993858894,-0.764263770835984,26.4997503415534));
#43746=CARTESIAN_POINT('',(23.5667006141106,-0.764339792548135,26.4999799994015));
#43747=CARTESIAN_POINT('',(8.83329938588935,-0.76435,26.5000000000004));
#43748=CARTESIAN_POINT('Ctrl Pts',(23.4332993858894,-0.764263770835903,
26.4997503415534));
#43749=CARTESIAN_POINT('Ctrl Pts',(23.4374930688249,-0.764282468728799,
26.4493207649479));
#43750=CARTESIAN_POINT('Ctrl Pts',(23.452272287261,-0.746995563910679,26.2717621776462));
#43751=CARTESIAN_POINT('Ctrl Pts',(23.4776370411976,-0.611445654087914,
25.9905566300544));
#43752=CARTESIAN_POINT('Ctrl Pts',(23.5199791831997,-0.185345401108989,
25.6779112752593));
#43753=CARTESIAN_POINT('Ctrl Pts',(23.5623213252019,0.380448766828713,25.7480415404581));
#43754=CARTESIAN_POINT('Ctrl Pts',(23.604663467204,0.717322101045798,26.1552575766811));
#43755=CARTESIAN_POINT('Ctrl Pts',(23.6364200737056,0.795937182645239,26.538105894183));
#43756=CARTESIAN_POINT('Ctrl Pts',(23.6681766802072,0.680101105708285,26.915511993711));
#43757=CARTESIAN_POINT('Ctrl Pts',(23.6999332867088,0.398791784083484,27.1895481978939));
#43758=CARTESIAN_POINT('Ctrl Pts',(23.7316898932104,0.0200962396143968,
27.296692361741));
#43759=CARTESIAN_POINT('Ctrl Pts',(23.763446499712,-0.363306363014758,27.2089739077987));
#43760=CARTESIAN_POINT('Ctrl Pts',(23.7952031062136,-0.658432051321634,
26.9489875409133));
#43761=CARTESIAN_POINT('Ctrl Pts',(23.8184874016061,-0.756830249032618,
26.6777191819525));
#43762=CARTESIAN_POINT('Ctrl Pts',(23.831186161498,-0.764359262184493,26.5253568955782));
#43763=CARTESIAN_POINT('Ctrl Pts',(23.8332993858894,-0.764350202263713,
26.5000021273756));
#43764=CARTESIAN_POINT('Ctrl Pts',(23.5667006141106,-0.76433979254796,26.4999799994015));
#43765=CARTESIAN_POINT('Ctrl Pts',(23.5694146847941,-0.764372599419905,
26.4673932611465));
#43766=CARTESIAN_POINT('Ctrl Pts',(23.5827379583759,-0.754334726260367,
26.3074462255872));
#43767=CARTESIAN_POINT('Ctrl Pts',(23.6066704348561,-0.644950851448086,
26.0318827492551));
#43768=CARTESIAN_POINT('Ctrl Pts',(23.6384980435508,-0.341608481918587,
25.7800006900629));
#43769=CARTESIAN_POINT('Ctrl Pts',(23.6703256522457,0.0453541685624505,
25.7043629215386));
#43770=CARTESIAN_POINT('Ctrl Pts',(23.7021532609405,0.421214845532138,25.8234843570678));
#43771=CARTESIAN_POINT('Ctrl Pts',(23.7339808696353,0.693968879696766,26.1082059785538));
#43772=CARTESIAN_POINT('Ctrl Pts',(23.7658084783301,0.796850455291405,26.4888324966759));
#43773=CARTESIAN_POINT('Ctrl Pts',(23.797636087025,0.704675811632944,26.8721926406151));
#43774=CARTESIAN_POINT('Ctrl Pts',(23.8294636957197,0.440007824081036,27.1644459917676));
#43775=CARTESIAN_POINT('Ctrl Pts',(23.8612913044146,0.0676329737958395,
27.2940536141119));
#43776=CARTESIAN_POINT('Ctrl Pts',(23.8931189131094,-0.321297344429241,
27.229289639095));
#43777=CARTESIAN_POINT('Ctrl Pts',(23.9249465218042,-0.631579222606048,
26.9860072497412));
#43778=CARTESIAN_POINT('Ctrl Pts',(23.9494737554713,-0.751551611982924,
26.7068480384306));
#43779=CARTESIAN_POINT('Ctrl Pts',(23.9633917862401,-0.76435372456793,26.5397490406375));
#43780=CARTESIAN_POINT('Ctrl Pts',(23.9667006141106,-0.764318926635357,
26.5000181819409));
#43781=CARTESIAN_POINT('Origin',(8.83329938588935,0.,26.5));
#43782=CARTESIAN_POINT('',(23.0332993858893,-0.764131106302846,26.5004425504153));
#43783=CARTESIAN_POINT('',(23.1667006141106,-0.76437181183062,26.5000184759214));
#43784=CARTESIAN_POINT('',(8.83329938588935,-0.76435,26.5000000000004));
#43785=CARTESIAN_POINT('Ctrl Pts',(23.0332993858894,-0.764131106302765,
26.5004425504153));
#43786=CARTESIAN_POINT('Ctrl Pts',(23.0437999761519,-0.764286156156834,
26.374143586));
#43787=CARTESIAN_POINT('Ctrl Pts',(23.0754716374155,-0.670638391197475,
25.9903175893888));
#43788=CARTESIAN_POINT('Ctrl Pts',(23.1177288341795,-0.193816666742857,
25.679867151767));
#43789=CARTESIAN_POINT('Ctrl Pts',(23.1600709761817,0.326217167037633,25.7740656400097));
#43790=CARTESIAN_POINT('Ctrl Pts',(23.1918275826833,0.633093647904743,26.0160986765141));
#43791=CARTESIAN_POINT('Ctrl Pts',(23.2235841891849,0.787795093385811,26.3793077395167));
#43792=CARTESIAN_POINT('Ctrl Pts',(23.2553407956864,0.749355516936845,26.7701442457419));
#43793=CARTESIAN_POINT('Ctrl Pts',(23.2870974021881,0.528886386857991,27.0961558251828));
#43794=CARTESIAN_POINT('Ctrl Pts',(23.3188540086896,0.179216412751493,27.2762196807263));
#43795=CARTESIAN_POINT('Ctrl Pts',(23.3506106151912,-0.213999927519153,
27.2676761095181));
#43796=CARTESIAN_POINT('Ctrl Pts',(23.3823672216928,-0.55507609312846,27.071316142874));
#43797=CARTESIAN_POINT('Ctrl Pts',(23.4099301452589,-0.733777314969458,
26.7810545816172));
#43798=CARTESIAN_POINT('Ctrl Pts',(23.4269075333244,-0.764235272216312,
26.5766131906364));
#43799=CARTESIAN_POINT('Ctrl Pts',(23.4332993858894,-0.764263770835903,
26.4997503415534));
#43800=CARTESIAN_POINT('Ctrl Pts',(23.1667006141106,-0.764371811830445,
26.5000184759214));
#43801=CARTESIAN_POINT('Ctrl Pts',(23.1754375833482,-0.764265346458016,
26.395129905246));
#43802=CARTESIAN_POINT('Ctrl Pts',(23.1947837554841,-0.716081099388898,
26.1627815520115));
#43803=CARTESIAN_POINT('Ctrl Pts',(23.2247391305182,-0.488062159497627,
25.8700073891742));
#43804=CARTESIAN_POINT('Ctrl Pts',(23.2565667392131,-0.126322069100469,
25.7131467124763));
#43805=CARTESIAN_POINT('Ctrl Pts',(23.2883943479078,0.266339639077475,25.7488951086002));
#43806=CARTESIAN_POINT('Ctrl Pts',(23.3202219566027,0.593805672595626,25.9685019431627));
#43807=CARTESIAN_POINT('Ctrl Pts',(23.3520495652975,0.775917595190683,26.3182109829992));
#43808=CARTESIAN_POINT('Ctrl Pts',(23.3838771739923,0.768097327165974,26.7124190604186));
#43809=CARTESIAN_POINT('Ctrl Pts',(23.4157047826871,0.572259144787906,27.0546303565756));
#43810=CARTESIAN_POINT('Ctrl Pts',(23.4475323913819,0.236341096138676,27.2610770312554));
#43811=CARTESIAN_POINT('Ctrl Pts',(23.4793600000768,-0.157429464686238,
27.281224247497));
#43812=CARTESIAN_POINT('Ctrl Pts',(23.5111876087716,-0.512663815891357,
27.1101402896911));
#43813=CARTESIAN_POINT('Ctrl Pts',(23.5403011467829,-0.722815200106324,
26.8170287044339));
#43814=CARTESIAN_POINT('Ctrl Pts',(23.5588054818958,-0.764244358559034,
26.5947736274853));
#43815=CARTESIAN_POINT('Ctrl Pts',(23.5667006141106,-0.76433979254796,26.4999799994015));
#43816=CARTESIAN_POINT('Origin',(8.83329938588935,0.,26.5));
#43817=CARTESIAN_POINT('',(22.6332993858894,-0.764122705815582,26.5000528068419));
#43818=CARTESIAN_POINT('',(22.7667006141106,-0.764296184799811,26.4999878263918));
#43819=CARTESIAN_POINT('',(8.83329938588935,-0.76435,26.5000000000004));
#43820=CARTESIAN_POINT('Ctrl Pts',(22.6332993858894,-0.764122705815501,
26.5000528068419));
#43821=CARTESIAN_POINT('Ctrl Pts',(22.6501068834788,-0.762277025578763,
26.2987504101115));
#43822=CARTESIAN_POINT('Ctrl Pts',(22.6774999165688,-0.629581927431558,
25.9707755262326));
#43823=CARTESIAN_POINT('Ctrl Pts',(22.7154784851593,-0.218505020300182,
25.7347197303026));
#43824=CARTESIAN_POINT('Ctrl Pts',(22.7472350916609,0.172123229852927,25.7219629497037));
#43825=CARTESIAN_POINT('Ctrl Pts',(22.7789916981625,0.524512533349801,25.899938058812));
#43826=CARTESIAN_POINT('Ctrl Pts',(22.8107483046641,0.747044085909005,26.2235280520929));
#43827=CARTESIAN_POINT('Ctrl Pts',(22.8425049111657,0.788621357728243,26.6148866059988));
#43828=CARTESIAN_POINT('Ctrl Pts',(22.8742615176673,0.637345306587861,26.9779398241586));
#43829=CARTESIAN_POINT('Ctrl Pts',(22.9060181241689,0.331205804787041,27.2248622579349));
#43830=CARTESIAN_POINT('Ctrl Pts',(22.9377747306705,-0.0561303630539786,
27.2945822717721));
#43831=CARTESIAN_POINT('Ctrl Pts',(22.9695313371721,-0.429102675280415,
27.1716089821991));
#43832=CARTESIAN_POINT('Ctrl Pts',(23.0012879436737,-0.698667848123337,
26.8831857198376));
#43833=CARTESIAN_POINT('Ctrl Pts',(23.0225439599128,-0.763715786563097,
26.6297987621571));
#43834=CARTESIAN_POINT('Ctrl Pts',(23.0332144406513,-0.764129852016441,
26.501464254465));
#43835=CARTESIAN_POINT('Ctrl Pts',(23.0332993858894,-0.764131106302765,
26.5004425504153));
#43836=CARTESIAN_POINT('Ctrl Pts',(22.7667006141106,-0.764296184799636,
26.4999878263918));
#43837=CARTESIAN_POINT('Ctrl Pts',(22.770851279004,-0.764324242497102,26.450144332975));
#43838=CARTESIAN_POINT('Ctrl Pts',(22.7856111467957,-0.747251188337183,
26.2729185987678));
#43839=CARTESIAN_POINT('Ctrl Pts',(22.8109802174856,-0.611807151357293,
25.9893265517215));
#43840=CARTESIAN_POINT('Ctrl Pts',(22.8428078261804,-0.292120759998493,
25.7585414220562));
#43841=CARTESIAN_POINT('Ctrl Pts',(22.8746354348752,0.0990721111926007,
25.7092534679099));
#43842=CARTESIAN_POINT('Ctrl Pts',(22.9064630435701,0.466013717526745,25.853527590453));
#43843=CARTESIAN_POINT('Ctrl Pts',(22.9382906522649,0.718882635243795,26.1560477969637));
#43844=CARTESIAN_POINT('Ctrl Pts',(22.9701182609597,0.795780606359475,26.5427619897895));
#43845=CARTESIAN_POINT('Ctrl Pts',(23.0019458696545,0.677884240092678,26.9190087329192));
#43846=CARTESIAN_POINT('Ctrl Pts',(23.0337734783493,0.394052677220659,27.1926888542512));
#43847=CARTESIAN_POINT('Ctrl Pts',(23.0656010870442,0.0137633349813457,
27.2968098467256));
#43848=CARTESIAN_POINT('Ctrl Pts',(23.0974286957389,-0.369895051057782,
27.2058845602728));
#43849=CARTESIAN_POINT('Ctrl Pts',(23.1292563044338,-0.663009057407268,
26.9421700476339));
#43850=CARTESIAN_POINT('Ctrl Pts',(23.152346943891,-0.757917784391792,26.6723232455195));
#43851=CARTESIAN_POINT('Ctrl Pts',(23.1648283804499,-0.764394626155245,
26.5224949099452));
#43852=CARTESIAN_POINT('Ctrl Pts',(23.1667006141106,-0.764371811830445,
26.5000184759214));
#43853=CARTESIAN_POINT('Origin',(8.83329938588935,0.,26.5));
#43854=CARTESIAN_POINT('',(22.2332993858894,-0.764862580106952,26.5002046409345));
#43855=CARTESIAN_POINT('',(22.3667006141106,-0.764412916483386,26.5000055227705));
#43856=CARTESIAN_POINT('',(8.83329938588935,-0.76435,26.5000000000004));
#43857=CARTESIAN_POINT('Ctrl Pts',(22.2332993858894,-0.764862580106872,
26.5002046409345));
#43858=CARTESIAN_POINT('Ctrl Pts',(22.2352427198047,-0.765032394802853,
26.4769375526074));
#43859=CARTESIAN_POINT('Ctrl Pts',(22.2477715892206,-0.759009646591559,
26.3268520087914));
#43860=CARTESIAN_POINT('Ctrl Pts',(22.2708859941369,-0.660332128994326,
26.055748028139));
#43861=CARTESIAN_POINT('Ctrl Pts',(22.3026426006386,-0.369900855742956,
25.7942086605736));
#43862=CARTESIAN_POINT('Ctrl Pts',(22.3343992071401,0.01423446586742,25.7031404697911));
#43863=CARTESIAN_POINT('Ctrl Pts',(22.3661558136418,0.392945955132557,25.8071038457199));
#43864=CARTESIAN_POINT('Ctrl Pts',(22.3979124201434,0.676990688980436,26.0795167243078));
#43865=CARTESIAN_POINT('Ctrl Pts',(22.4296690266449,0.79534519032439,26.4545957758109));
#43866=CARTESIAN_POINT('Ctrl Pts',(22.4614256331466,0.720445109942096,26.8407072374687));
#43867=CARTESIAN_POINT('Ctrl Pts',(22.4931822396481,0.469247428456909,27.1436757375867));
#43868=CARTESIAN_POINT('Ctrl Pts',(22.5249388461498,0.104827792755421,27.290062570161));
#43869=CARTESIAN_POINT('Ctrl Pts',(22.5566954526513,-0.287175811024369,
27.2433021669895));
#43870=CARTESIAN_POINT('Ctrl Pts',(22.5884520591529,-0.605484443472687,
27.0165142048358));
#43871=CARTESIAN_POINT('Ctrl Pts',(22.6139867035656,-0.747869186885517,
26.731375214218));
#43872=CARTESIAN_POINT('Ctrl Pts',(22.6289358124778,-0.764601882514145,
26.5523150654794));
#43873=CARTESIAN_POINT('Ctrl Pts',(22.6332993858894,-0.764122705815501,
26.5000528068419));
#43874=CARTESIAN_POINT('Ctrl Pts',(22.3667006141106,-0.764412916483211,
26.5000055227705));
#43875=CARTESIAN_POINT('Ctrl Pts',(22.376874177558,-0.764365640456866,26.377889443069));
#43876=CARTESIAN_POINT('Ctrl Pts',(22.3976569439038,-0.703489322056653,
26.1283827371445));
#43877=CARTESIAN_POINT('Ctrl Pts',(22.4290489131478,-0.444327578628173,
25.8384349131801));
#43878=CARTESIAN_POINT('Ctrl Pts',(22.4608765218426,-0.0728050701817948,
25.7064038917784));
#43879=CARTESIAN_POINT('Ctrl Pts',(22.4927041305374,0.316538952499552,25.768632477629));
#43880=CARTESIAN_POINT('Ctrl Pts',(22.5245317392322,0.628399313207805,26.0098881103375));
#43881=CARTESIAN_POINT('Ctrl Pts',(22.5563593479271,0.786437594250266,26.3711152779478));
#43882=CARTESIAN_POINT('Ctrl Pts',(22.5881869566219,0.751968557521462,26.7638913597064));
#43883=CARTESIAN_POINT('Ctrl Pts',(22.6200145653167,0.533429670730638,27.0920710663534));
#43884=CARTESIAN_POINT('Ctrl Pts',(22.6518421740115,0.184315750545256,27.2753212658824));
#43885=CARTESIAN_POINT('Ctrl Pts',(22.6836697827063,-0.209915711095263,
27.2687852466482));
#43886=CARTESIAN_POINT('Ctrl Pts',(22.7154973914012,-0.552763171263273,
27.0740629213976));
#43887=CARTESIAN_POINT('Ctrl Pts',(22.7431743352025,-0.733237616757187,
26.7825386072601));
#43888=CARTESIAN_POINT('Ctrl Pts',(22.7602420761057,-0.764252526323207,
26.5775455442021));
#43889=CARTESIAN_POINT('Ctrl Pts',(22.7667006141106,-0.764296184799636,
26.4999878263918));
#43890=CARTESIAN_POINT('Origin',(8.83329938588935,0.,26.5));
#43891=CARTESIAN_POINT('',(21.8332993858894,-0.764100887066997,26.4995051871397));
#43892=CARTESIAN_POINT('',(21.9667006141106,-0.764284603309852,26.5000031825945));
#43893=CARTESIAN_POINT('',(8.83329938588935,-0.76435,26.5000000000004));
#43894=CARTESIAN_POINT('Ctrl Pts',(21.8332993858894,-0.764100887066916,
26.4995051871397));
#43895=CARTESIAN_POINT('Ctrl Pts',(21.8415496271317,-0.764046362726459,
26.4005484505602));
#43896=CARTESIAN_POINT('Ctrl Pts',(21.8603854038745,-0.720456291582594,
26.1754869405762));
#43897=CARTESIAN_POINT('Ctrl Pts',(21.8898067161178,-0.502746680944055,
25.8815879159468));
#43898=CARTESIAN_POINT('Ctrl Pts',(21.9215633226194,-0.146192340398604,
25.7169678142758));
#43899=CARTESIAN_POINT('Ctrl Pts',(21.953319929121,0.246561806406779,25.7421544657884));
#43900=CARTESIAN_POINT('Ctrl Pts',(21.9850765356226,0.578813148913968,25.9526327978489));
#43901=CARTESIAN_POINT('Ctrl Pts',(22.0168331421242,0.770423302724975,26.2961115189095));
#43902=CARTESIAN_POINT('Ctrl Pts',(22.0485897486258,0.773654319674137,26.6896591625013));
#43903=CARTESIAN_POINT('Ctrl Pts',(22.0803463551274,0.589394342448357,27.0364718445485));
#43904=CARTESIAN_POINT('Ctrl Pts',(22.112102961629,0.259548714643134,27.253394002243));
#43905=CARTESIAN_POINT('Ctrl Pts',(22.1438595681306,-0.129993482523563,
27.2851751585385));
#43906=CARTESIAN_POINT('Ctrl Pts',(22.1842583762174,-0.593002042557325,
27.0854711589097));
#43907=CARTESIAN_POINT('Ctrl Pts',(22.2140716488037,-0.763182399309391,
26.7304138981164));
#43908=CARTESIAN_POINT('Ctrl Pts',(22.2332993858894,-0.764862580106872,
26.5002046409345));
#43909=CARTESIAN_POINT('Ctrl Pts',(21.9667006141106,-0.764284603309676,
26.5000031825944));
#43910=CARTESIAN_POINT('Ctrl Pts',(21.9722878732138,-0.764274911934341,
26.4329053576406));
#43911=CARTESIAN_POINT('Ctrl Pts',(21.9884843352154,-0.738916987458651,
26.238393611413));
#43912=CARTESIAN_POINT('Ctrl Pts',(22.0152900001152,-0.575860605727061,
25.9491098802844));
#43913=CARTESIAN_POINT('Ctrl Pts',(22.04711760881,-0.241294757923752,25.7404789660404));
#43914=CARTESIAN_POINT('Ctrl Pts',(22.0789452175048,0.152336179061179,25.7177666270366));
#43915=CARTESIAN_POINT('Ctrl Pts',(22.1107728261996,0.508677661110342,25.8865324798199));
#43916=CARTESIAN_POINT('Ctrl Pts',(22.1426004348944,0.740503004985982,26.2054653486679));
#43917=CARTESIAN_POINT('Ctrl Pts',(22.1744280435892,0.791065082286333,26.5964955792559));
#43918=CARTESIAN_POINT('Ctrl Pts',(22.2062556522841,0.647987106915214,26.9639052387075));
#43919=CARTESIAN_POINT('Ctrl Pts',(22.2380832609789,0.346292273938845,27.2177583313615));
#43920=CARTESIAN_POINT('Ctrl Pts',(22.2699108696737,-0.0401693572021401,
27.2959156889838));
#43921=CARTESIAN_POINT('Ctrl Pts',(22.3017384783685,-0.416798173548772,
27.1792456431623));
#43922=CARTESIAN_POINT('Ctrl Pts',(22.3335660870633,-0.691401477599888,
26.8963071510852));
#43923=CARTESIAN_POINT('Ctrl Pts',(22.3552201323107,-0.763083116198193,
26.6378078686346));
#43924=CARTESIAN_POINT('Ctrl Pts',(22.3662649746598,-0.764414940877344,
26.5052346228955));
#43925=CARTESIAN_POINT('Ctrl Pts',(22.3667006141106,-0.764412916483211,
26.5000055227705));
#43926=CARTESIAN_POINT('Origin',(8.83329938588935,0.,26.5));
#43927=CARTESIAN_POINT('',(21.4332993858894,-0.764276746822807,26.5000737456655));
#43928=CARTESIAN_POINT('',(21.5667006141106,-0.76440089280987,26.4999880930546));
#43929=CARTESIAN_POINT('',(8.83329938588935,-0.76435,26.5000000000004));
#43930=CARTESIAN_POINT('Ctrl Pts',(21.4332993858894,-0.764276746822727,
26.5000737456655));
#43931=CARTESIAN_POINT('Ctrl Pts',(21.4372709989581,-0.764328306924678,
26.4522928960755));
#43932=CARTESIAN_POINT('Ctrl Pts',(21.4518281475273,-0.748306393941852,
26.277170782625));
#43933=CARTESIAN_POINT('Ctrl Pts',(21.476970831597,-0.616487950568337,25.9955654541219));
#43934=CARTESIAN_POINT('Ctrl Pts',(21.5087274380987,-0.299974232084392,
25.7616653616493));
#43935=CARTESIAN_POINT('Ctrl Pts',(21.5404840446002,0.0897151756284967,
25.7084277022228));
#43936=CARTESIAN_POINT('Ctrl Pts',(21.5722406511019,0.457605408654088,25.8475278794664));
#43937=CARTESIAN_POINT('Ctrl Pts',(21.6039972576034,0.713743622414307,26.1463311637505));
#43938=CARTESIAN_POINT('Ctrl Pts',(21.6357538641051,0.796412224677964,26.5302539135788));
#43939=CARTESIAN_POINT('Ctrl Pts',(21.6675104706066,0.684050486030751,26.9087089312087));
#43940=CARTESIAN_POINT('Ctrl Pts',(21.6992670771083,0.406712042690736,27.184093304612));
#43941=CARTESIAN_POINT('Ctrl Pts',(21.7416092191103,-0.0992230806999048,
27.3368617384697));
#43942=CARTESIAN_POINT('Ctrl Pts',(21.7839513611125,-0.609300801297396,
27.0821815203151));
#43943=CARTESIAN_POINT('Ctrl Pts',(21.8180432618723,-0.755762004372405,
26.6826607782934));
#43944=CARTESIAN_POINT('Ctrl Pts',(21.8309640916311,-0.764116320600975,
26.5275156527689));
#43945=CARTESIAN_POINT('Ctrl Pts',(21.8332993858894,-0.764100887066916,
26.4995051871397));
#43946=CARTESIAN_POINT('Ctrl Pts',(21.5667006141106,-0.764400892809695,
26.4999880930546));
#43947=CARTESIAN_POINT('Ctrl Pts',(21.5677015688696,-0.764409844848788,
26.4879728090667));
#43948=CARTESIAN_POINT('Ctrl Pts',(21.5793117265269,-0.761192076692281,
26.3486113254963));
#43949=CARTESIAN_POINT('Ctrl Pts',(21.6015310870826,-0.6805998376932,26.0854168091196));
#43950=CARTESIAN_POINT('Ctrl Pts',(21.6333586957773,-0.398557419114277,
25.8098932365948));
#43951=CARTESIAN_POINT('Ctrl Pts',(21.6651863044722,-0.0189545325561093,
25.7032967384752));
#43952=CARTESIAN_POINT('Ctrl Pts',(21.697013913167,0.36528811976181,25.791720428934));
#43953=CARTESIAN_POINT('Ctrl Pts',(21.7288415218618,0.660114095329825,26.053519605833));
#43954=CARTESIAN_POINT('Ctrl Pts',(21.7606691305566,0.793354720904365,26.4246100268778));
#43955=CARTESIAN_POINT('Ctrl Pts',(21.7924967392514,0.732394826972873,26.8141547049655));
#43956=CARTESIAN_POINT('Ctrl Pts',(21.8243243479463,0.492156418482947,27.126799346661));
#43957=CARTESIAN_POINT('Ctrl Pts',(21.856151956641,0.131446007206347,27.2860135548564));
#43958=CARTESIAN_POINT('Ctrl Pts',(21.8879795653359,-0.261440279771059,
27.2528242433277));
#43959=CARTESIAN_POINT('Ctrl Pts',(21.9198071740307,-0.590330176718207,
27.0353556235666));
#43960=CARTESIAN_POINT('Ctrl Pts',(21.9460475236223,-0.74234810236243,26.7480215032879));
#43961=CARTESIAN_POINT('Ctrl Pts',(21.9616786703156,-0.764293314117844,
26.5603120924657));
#43962=CARTESIAN_POINT('Ctrl Pts',(21.9667006141106,-0.764284603309676,
26.5000031825944));
#43963=CARTESIAN_POINT('Origin',(8.83329938588935,0.,26.5));
#43964=CARTESIAN_POINT('',(21.0332993858894,-0.764351912162959,26.5000528856107));
#43965=CARTESIAN_POINT('',(21.1667006141106,-0.764310404172143,26.500016603693));
#43966=CARTESIAN_POINT('',(8.83329938588935,-0.76435,26.5000000000004));
#43967=CARTESIAN_POINT('Ctrl Pts',(21.0332993858894,-0.764351912162878,
26.5000528856107));
#43968=CARTESIAN_POINT('Ctrl Pts',(21.043577906285,-0.764279841884346,26.376700035302));
#43969=CARTESIAN_POINT('Ctrl Pts',(21.0644419621812,-0.702702321442688,
26.1260397749937));
#43970=CARTESIAN_POINT('Ctrl Pts',(21.0958915535779,-0.441630110964222,
25.8369778582611));
#43971=CARTESIAN_POINT('Ctrl Pts',(21.1276481600795,-0.0707011018639236,
25.70619654051));
#43972=CARTESIAN_POINT('Ctrl Pts',(21.1594047665811,0.317727575909635,25.7695475431092));
#43973=CARTESIAN_POINT('Ctrl Pts',(21.1911613730827,0.628395710084807,26.009789267304));
#43974=CARTESIAN_POINT('Ctrl Pts',(21.2229179795843,0.786429550765298,26.3715608331863));
#43975=CARTESIAN_POINT('Ctrl Pts',(21.2546745860859,0.751894885449026,26.7608685805538));
#43976=CARTESIAN_POINT('Ctrl Pts',(21.297016728088,0.463552958450529,27.2037765581276));
#43977=CARTESIAN_POINT('Ctrl Pts',(21.3393588700901,-0.0905842644351466,
27.3378408441313));
#43978=CARTESIAN_POINT('Ctrl Pts',(21.3817010120923,-0.549496531103895,
27.0757185921867));
#43979=CARTESIAN_POINT('Ctrl Pts',(21.4094860055252,-0.732071494044401,
26.7865804303052));
#43980=CARTESIAN_POINT('Ctrl Pts',(21.4266854634575,-0.76419088384741,26.5796431366029));
#43981=CARTESIAN_POINT('Ctrl Pts',(21.4332993858894,-0.764276746822727,
26.5000737456655));
#43982=CARTESIAN_POINT('Ctrl Pts',(21.1667006141106,-0.764310404171968,
26.500016603693));
#43983=CARTESIAN_POINT('Ctrl Pts',(21.1737244674237,-0.76424402040046,26.4156747594692));
#43984=CARTESIAN_POINT('Ctrl Pts',(21.1913575236351,-0.729295132890033,
26.2038848342813));
#43985=CARTESIAN_POINT('Ctrl Pts',(21.2195997827447,-0.537275894906149,
25.9114169778345));
#43986=CARTESIAN_POINT('Ctrl Pts',(21.2514273914396,-0.189363322650899,
25.7258960707611));
#43987=CARTESIAN_POINT('Ctrl Pts',(21.2832550001344,0.204902355806668,25.7298633979523));
#43988=CARTESIAN_POINT('Ctrl Pts',(21.3150826088292,0.549011221810531,25.9223478213019));
#43989=CARTESIAN_POINT('Ctrl Pts',(21.346910217524,0.758730940462114,26.2562322391823));
#43990=CARTESIAN_POINT('Ctrl Pts',(21.3787378262188,0.782725486097683,26.6497870977146));
#43991=CARTESIAN_POINT('Ctrl Pts',(21.4105654349136,0.615121378538741,27.0066764755672));
#43992=CARTESIAN_POINT('Ctrl Pts',(21.4423930436085,0.296945416897534,27.2395395733916));
#43993=CARTESIAN_POINT('Ctrl Pts',(21.4742206523033,-0.0939180232535311,
27.2913752372527));
#43994=CARTESIAN_POINT('Ctrl Pts',(21.5060482609981,-0.461791836663578,
27.1494949274779));
#43995=CARTESIAN_POINT('Ctrl Pts',(21.5368749149339,-0.708612051316828,
26.8580906911256));
#43996=CARTESIAN_POINT('Ctrl Pts',(21.5570923659713,-0.76431496144049,26.6153238052581));
#43997=CARTESIAN_POINT('Ctrl Pts',(21.5667006141106,-0.764400892809695,
26.4999880930546));
#43998=CARTESIAN_POINT('Origin',(8.83329938588935,0.,26.5));
#43999=CARTESIAN_POINT('',(20.6332993858894,-0.76435,26.5000000000002));
#44000=CARTESIAN_POINT('',(20.7667006141106,-0.764350239829443,26.4999799548752));
#44001=CARTESIAN_POINT('',(8.83329938588935,-0.76435,26.5000000000004));
#44002=CARTESIAN_POINT('Ctrl Pts',(20.6332993858894,-0.764313550173299,
26.5000165829699));
#44003=CARTESIAN_POINT('Ctrl Pts',(20.6392992781114,-0.764263692888945,
26.4279696684704));
#44004=CARTESIAN_POINT('Ctrl Pts',(20.655884705834,-0.736231422484058,26.2287857300863));
#44005=CARTESIAN_POINT('Ctrl Pts',(20.6830556690571,-0.565714119049419,
25.9386711181391));
#44006=CARTESIAN_POINT('Ctrl Pts',(20.7148122755588,-0.227907934100152,
25.7367375432753));
#44007=CARTESIAN_POINT('Ctrl Pts',(20.7465688820603,0.164464593988673,25.7201672434249));
#44008=CARTESIAN_POINT('Ctrl Pts',(20.778325488562,0.518475108459405,25.8948953645883));
#44009=CARTESIAN_POINT('Ctrl Pts',(20.8100820950635,0.743006763321614,26.2147995709279));
#44010=CARTESIAN_POINT('Ctrl Pts',(20.8524242370657,0.808039650977486,26.739279567674));
#44011=CARTESIAN_POINT('Ctrl Pts',(20.8947663790678,0.470788843887705,27.1989568323787));
#44012=CARTESIAN_POINT('Ctrl Pts',(20.9371085210699,-0.0490268475710841,
27.2943517503612));
#44013=CARTESIAN_POINT('Ctrl Pts',(20.9688651275715,-0.421575592023053,
27.1761967746885));
#44014=CARTESIAN_POINT('Ctrl Pts',(21.0006217340731,-0.694507228865489,
26.8909570819885));
#44015=CARTESIAN_POINT('Ctrl Pts',(21.0220998201791,-0.763472476586269,
26.6344550186812));
#44016=CARTESIAN_POINT('Ctrl Pts',(21.0329923707845,-0.764354064871952,
26.5037373836531));
#44017=CARTESIAN_POINT('Ctrl Pts',(21.0332993858894,-0.764351912162878,
26.5000528856107));
#44018=CARTESIAN_POINT('Ctrl Pts',(20.7667006141106,-0.764350239829268,
26.4999799548753));
#44019=CARTESIAN_POINT('Ctrl Pts',(20.7691381630795,-0.764380522761163,
26.4707144501526));
#44020=CARTESIAN_POINT('Ctrl Pts',(20.7821849149467,-0.755557485350515,
26.3140917378046));
#44021=CARTESIAN_POINT('Ctrl Pts',(20.8058408697121,-0.650995855233153,
26.0403264661764));
#44022=CARTESIAN_POINT('Ctrl Pts',(20.8376684784069,-0.350961365800501,
25.7845131161621));
#44023=CARTESIAN_POINT('Ctrl Pts',(20.8694960871017,0.034982840646634,25.7038394872333));
#44024=CARTESIAN_POINT('Ctrl Pts',(20.9013236957965,0.412363808420875,25.8180531906862));
#44025=CARTESIAN_POINT('Ctrl Pts',(20.9331513044914,0.688804725407329,26.0991965425734));
#44026=CARTESIAN_POINT('Ctrl Pts',(20.9649789131862,0.796637286020959,26.4784501566183));
#44027=CARTESIAN_POINT('Ctrl Pts',(20.996806521881,0.70946580780214,26.8629788269146));
#44028=CARTESIAN_POINT('Ctrl Pts',(21.0286341305758,0.448628471403418,27.1586560983357));
#44029=CARTESIAN_POINT('Ctrl Pts',(21.0604617392707,0.0779740759816852,
27.2931049140583));
#44030=CARTESIAN_POINT('Ctrl Pts',(21.0922893479654,-0.311767123444173,
27.2334143589867));
#44031=CARTESIAN_POINT('Ctrl Pts',(21.1241169566603,-0.625192728165132,
26.9941957242612));
#44032=CARTESIAN_POINT('Ctrl Pts',(21.148920712042,-0.750185963151055,26.7134941345636));
#44033=CARTESIAN_POINT('Ctrl Pts',(21.1631152645254,-0.764344289991763,
26.543069182202));
#44034=CARTESIAN_POINT('Ctrl Pts',(21.1667006141106,-0.764310404171968,
26.500016603693));
#44035=CARTESIAN_POINT('Origin',(8.83329938588935,0.,26.5));
#44036=CARTESIAN_POINT('',(20.2332993858894,-0.76435,26.5000000000001));
#44037=CARTESIAN_POINT('',(20.3667006141106,-0.764361315646495,26.5000195227112));
#44038=CARTESIAN_POINT('',(8.83329938588935,-0.76435,26.5000000000004));
#44039=CARTESIAN_POINT('Ctrl Pts',(20.2332993858894,-0.76435,26.5000000000001));
#44040=CARTESIAN_POINT('Ctrl Pts',(20.2511698941678,-0.764350000000042,
26.2854398560099));
#44041=CARTESIAN_POINT('Ctrl Pts',(20.2690404024462,-0.669038051787523,
26.0726183635795));
#44042=CARTESIAN_POINT('Ctrl Pts',(20.2869109107247,-0.508962945483331,
25.9297477377292));
#44043=CARTESIAN_POINT('Ctrl Pts',(20.3047814190031,-0.348887839179139,
25.786877111879));
#44044=CARTESIAN_POINT('Ctrl Pts',(20.3226519272816,-0.126643857468825,
25.716272808144));
#44045=CARTESIAN_POINT('Ctrl Pts',(20.34052243556,0.0865367472361844,25.7405644768134));
#44046=CARTESIAN_POINT('Ctrl Pts',(20.3583929438384,0.299717351941194,25.7648561454827));
#44047=CARTESIAN_POINT('Ctrl Pts',(20.3762634521169,0.500379634244014,25.8836500997623));
#44048=CARTESIAN_POINT('Ctrl Pts',(20.3941339603953,0.62420857318233,26.058871243665));
#44049=CARTESIAN_POINT('Ctrl Pts',(20.4120044686738,0.748037512120647,26.2340923875676));
#44050=CARTESIAN_POINT('Ctrl Pts',(20.4298749769522,0.793026254288736,26.462900971739));
#44051=CARTESIAN_POINT('Ctrl Pts',(20.4477454852306,0.744755289141801,26.6719606984032));
#44052=CARTESIAN_POINT('Ctrl Pts',(20.4656159935091,0.696484323994866,26.8810204250674));
#44053=CARTESIAN_POINT('Ctrl Pts',(20.4834865017875,0.555735962611667,27.0669431344934));
#44054=CARTESIAN_POINT('Ctrl Pts',(20.501357010066,0.367621990370539,27.1701380415228));
#44055=CARTESIAN_POINT('Ctrl Pts',(20.5192275183444,0.179508018129412,27.2733329485522));
#44056=CARTESIAN_POINT('Ctrl Pts',(20.5370980266228,-0.0529228659410256,
27.2921276085011));
#44057=CARTESIAN_POINT('Ctrl Pts',(20.5549685349013,-0.255173367133837,
27.2204980743941));
#44058=CARTESIAN_POINT('Ctrl Pts',(20.5728390431797,-0.457423868326649,
27.148868540287));
#44059=CARTESIAN_POINT('Ctrl Pts',(20.5907095514582,-0.626216181706997,
26.987975687568));
#44060=CARTESIAN_POINT('Ctrl Pts',(20.6085800597366,-0.707450049624308,
26.7893878881131));
#44061=CARTESIAN_POINT('Ctrl Pts',(20.6168198351209,-0.744905549759135,
26.6978225651763));
#44062=CARTESIAN_POINT('Ctrl Pts',(20.6250596105051,-0.764349999999979,
26.5989298885823));
#44063=CARTESIAN_POINT('Ctrl Pts',(20.6332993858894,-0.76435,26.5000000000002));
#44064=CARTESIAN_POINT('Ctrl Pts',(20.3667006141106,-0.764361315646319,
26.5000195227112));
#44065=CARTESIAN_POINT('Ctrl Pts',(20.3751610616335,-0.764255842813653,
26.3984466142992));
#44066=CARTESIAN_POINT('Ctrl Pts',(20.3942307120548,-0.718344923715845,
26.1694111801766));
#44067=CARTESIAN_POINT('Ctrl Pts',(20.4239095653743,-0.496229785355027,
25.8764205252295));
#44068=CARTESIAN_POINT('Ctrl Pts',(20.4557371740691,-0.136564365409659,
25.7148595442031));
#44069=CARTESIAN_POINT('Ctrl Pts',(20.4875647827639,0.256529822285824,25.7454883622458));
#44070=CARTESIAN_POINT('Ctrl Pts',(20.5193923914588,0.586829621236875,25.9608095356299));
#44071=CARTESIAN_POINT('Ctrl Pts',(20.5512200001536,0.773482934822817,26.3081158923556));
#44072=CARTESIAN_POINT('Ctrl Pts',(20.5830476088484,0.77080002362345,26.7023924030459));
#44073=CARTESIAN_POINT('Ctrl Pts',(20.6148752175432,0.579437621297725,27.047126497488));
#44074=CARTESIAN_POINT('Ctrl Pts',(20.646702826238,0.2462381767104,27.2579327948828));
#44075=CARTESIAN_POINT('Ctrl Pts',(20.6785304349328,-0.147236426742641,
27.2832092925066));
#44076=CARTESIAN_POINT('Ctrl Pts',(20.7103580436277,-0.504669912886847,
27.1167687088815));
#44077=CARTESIAN_POINT('Ctrl Pts',(20.7397481033536,-0.720654954004773,
26.8236626255095));
#44078=CARTESIAN_POINT('Ctrl Pts',(20.7585289601812,-0.764248719144938,
26.5980898101897));
#44079=CARTESIAN_POINT('Ctrl Pts',(20.7667006141106,-0.764350239829268,
26.4999799548753));
#44080=CARTESIAN_POINT('Origin',(8.83329938588935,0.,26.5));
#44081=CARTESIAN_POINT('',(19.8332993858894,-0.764344534536135,26.5000129791237));
#44082=CARTESIAN_POINT('',(19.9667006141106,-0.764302553547059,26.4999854764565));
#44083=CARTESIAN_POINT('',(8.83329938588935,-0.76435,26.5000000000004));
#44084=CARTESIAN_POINT('Ctrl Pts',(19.8332993858894,-0.764344534536054,
26.5000129791237));
#44085=CARTESIAN_POINT('Ctrl Pts',(19.8413275572648,-0.764313373082258,
26.403688836108));
#44086=CARTESIAN_POINT('Ctrl Pts',(19.8599412641407,-0.722113350608405,
26.1803405233073));
#44087=CARTESIAN_POINT('Ctrl Pts',(19.8891405065173,-0.508737507276705,
25.8866858826192));
#44088=CARTESIAN_POINT('Ctrl Pts',(19.9208971130188,-0.155477746603945,
25.7194713295494));
#44089=CARTESIAN_POINT('Ctrl Pts',(19.963239255021,0.372447071308012,25.7440463187918));
#44090=CARTESIAN_POINT('Ctrl Pts',(20.0055813970231,0.768489532327075,26.154158088483));
#44091=CARTESIAN_POINT('Ctrl Pts',(20.0479235390252,0.774628079308121,26.6826189306506));
#44092=CARTESIAN_POINT('Ctrl Pts',(20.0796801455268,0.595188665990073,27.0298287551329));
#44093=CARTESIAN_POINT('Ctrl Pts',(20.1114367520284,0.267911625081069,27.2506071489466));
#44094=CARTESIAN_POINT('Ctrl Pts',(20.14319335853,-0.12312173971539,27.2869896069711));
#44095=CARTESIAN_POINT('Ctrl Pts',(20.1749499650316,-0.485029654910406,
27.132351810277));
#44096=CARTESIAN_POINT('Ctrl Pts',(20.2049853074847,-0.714965243557672,
26.8399360103876));
#44097=CARTESIAN_POINT('Ctrl Pts',(20.2244351144373,-0.764312601055636,
26.6063935603332));
#44098=CARTESIAN_POINT('Ctrl Pts',(20.2332993858894,-0.764425095983041,
26.4999881455073));
#44099=CARTESIAN_POINT('Ctrl Pts',(19.9667006141106,-0.764302553546884,
26.4999854764565));
#44100=CARTESIAN_POINT('Ctrl Pts',(19.9705747572893,-0.764334137460401,
26.4534637195935));
#44101=CARTESIAN_POINT('Ctrl Pts',(19.9850581033664,-0.74871078126693,26.2795647520368));
#44102=CARTESIAN_POINT('Ctrl Pts',(20.0101506523417,-0.618409493726067,
25.9973420056359));
#44103=CARTESIAN_POINT('Ctrl Pts',(20.0419782610365,-0.301757468419426,
25.7624108247258));
#44104=CARTESIAN_POINT('Ctrl Pts',(20.0738058697313,0.0887599484803642,
25.7080296515813));
#44105=CARTESIAN_POINT('Ctrl Pts',(20.1056334784261,0.457550352668162,25.8475101257477));
#44106=CARTESIAN_POINT('Ctrl Pts',(20.137461087121,0.71433976430242,26.1467096627914));
#44107=CARTESIAN_POINT('Ctrl Pts',(20.1692886958158,0.796270251327002,26.5323890117207));
#44108=CARTESIAN_POINT('Ctrl Pts',(20.2011163045106,0.683286543729253,26.9101400497234));
#44109=CARTESIAN_POINT('Ctrl Pts',(20.2329439132054,0.403045242186098,27.1874953774243));
#44110=CARTESIAN_POINT('Ctrl Pts',(20.2647715219002,0.0241449255081358,
27.2965628561519));
#44111=CARTESIAN_POINT('Ctrl Pts',(20.296599130595,-0.360665681930769,27.210644515286));
#44112=CARTESIAN_POINT('Ctrl Pts',(20.3284267392899,-0.657191111310729,
26.9507717875409));
#44113=CARTESIAN_POINT('Ctrl Pts',(20.3517939004617,-0.756786585457168,
26.6789681317309));
#44114=CARTESIAN_POINT('Ctrl Pts',(20.3645518587353,-0.76438810327375,26.5258166607872));
#44115=CARTESIAN_POINT('Ctrl Pts',(20.3667006141106,-0.764361315646319,
26.5000195227112));
#44116=CARTESIAN_POINT('Origin',(8.83329938588935,0.,26.5));
#44117=CARTESIAN_POINT('',(19.4332993858894,-0.764277110167821,26.4997254257785));
#44118=CARTESIAN_POINT('',(19.5667006141106,-0.764407967391875,26.5000088022807));
#44119=CARTESIAN_POINT('',(8.83329938588935,-0.76435,26.5000000000004));
#44120=CARTESIAN_POINT('Ctrl Pts',(19.4332993858894,-0.764277110167741,
26.4997254257785));
#44121=CARTESIAN_POINT('Ctrl Pts',(19.4370489290912,-0.764304303637347,
26.4546467689379));
#44122=CARTESIAN_POINT('Ctrl Pts',(19.4513840077936,-0.749338609732044,
26.2824728008134));
#44123=CARTESIAN_POINT('Ctrl Pts',(19.4763046219965,-0.621973401147041,
26.0034645799642));
#44124=CARTESIAN_POINT('Ctrl Pts',(19.5186467639986,-0.202509532859472,
25.6819702461652));
#44125=CARTESIAN_POINT('Ctrl Pts',(19.5609889060007,0.364628407821791,25.7402441752329));
#44126=CARTESIAN_POINT('Ctrl Pts',(19.6033310480029,0.709950204635276,26.1403209180076));
#44127=CARTESIAN_POINT('Ctrl Pts',(19.6350876545045,0.796560342324164,26.5214401241865));
#44128=CARTESIAN_POINT('Ctrl Pts',(19.6668442610061,0.688648014289257,26.9011877905904));
#44129=CARTESIAN_POINT('Ctrl Pts',(19.6986008675076,0.413135351067633,27.1810512359355));
#44130=CARTESIAN_POINT('Ctrl Pts',(19.7303574740093,0.0367650668537481,
27.2960972980499));
#44131=CARTESIAN_POINT('Ctrl Pts',(19.7621140805108,-0.348389341911593,
27.2164219300026));
#44132=CARTESIAN_POINT('Ctrl Pts',(19.7938706870124,-0.64889140428939,26.962668913525));
#44133=CARTESIAN_POINT('Ctrl Pts',(19.8175991221386,-0.754929961758368,
26.6883853153909));
#44134=CARTESIAN_POINT('Ctrl Pts',(19.8307420217643,-0.764354460978864,
26.5306969165001));
#44135=CARTESIAN_POINT('Ctrl Pts',(19.8332993858894,-0.764344534536054,
26.5000129791237));
#44136=CARTESIAN_POINT('Ctrl Pts',(19.5667006141106,-0.7644079673917,26.5000088022807));
#44137=CARTESIAN_POINT('Ctrl Pts',(19.5765976558434,-0.764338862078803,
26.3812096529835));
#44138=CARTESIAN_POINT('Ctrl Pts',(19.5971039004745,-0.706022523705182,
26.1349974549268));
#44139=CARTESIAN_POINT('Ctrl Pts',(19.6282193480038,-0.452910319833234,
25.8442808501979));
#44140=CARTESIAN_POINT('Ctrl Pts',(19.6600469566987,-0.0831397717704243,
25.7074199475267));
#44141=CARTESIAN_POINT('Ctrl Pts',(19.6918745653935,0.306982059827983,25.7645699379462));
#44142=CARTESIAN_POINT('Ctrl Pts',(19.7237021740883,0.621959603598031,26.0017414198222));
#44143=CARTESIAN_POINT('Ctrl Pts',(19.7555297827831,0.784691405396808,26.3608786158601));
#44144=CARTESIAN_POINT('Ctrl Pts',(19.787357391478,0.755343328467109,26.7540704968485));
#44145=CARTESIAN_POINT('Ctrl Pts',(19.8191850001728,0.54109931163992,27.0850699925406));
#44146=CARTESIAN_POINT('Ctrl Pts',(19.8510126088676,0.194402856255303,27.2728537317685));
#44147=CARTESIAN_POINT('Ctrl Pts',(19.8828402175624,-0.199880302382556,
27.2714552650336));
#44148=CARTESIAN_POINT('Ctrl Pts',(19.9146678262572,-0.545235966749666,
27.0812169145776));
#44149=CARTESIAN_POINT('Ctrl Pts',(19.9426212917733,-0.731334700262787,
26.7891801156537));
#44150=CARTESIAN_POINT('Ctrl Pts',(19.9599655543911,-0.764247646039883,
26.5808618912586));
#44151=CARTESIAN_POINT('Ctrl Pts',(19.9667006141106,-0.764302553546884,
26.4999854764565));
#44152=CARTESIAN_POINT('Origin',(8.83329938588935,0.,26.5));
#44153=CARTESIAN_POINT('',(19.0332993858894,-0.764142366123107,26.5004047868447));
#44154=CARTESIAN_POINT('',(19.1667006141106,-0.764283845776008,26.5000000693701));
#44155=CARTESIAN_POINT('',(8.83329938588935,-0.76435,26.5000000000004));
#44156=CARTESIAN_POINT('Ctrl Pts',(19.0332993858894,-0.764142366123026,
26.5004047868447));
#44157=CARTESIAN_POINT('Ctrl Pts',(19.0433558364182,-0.764299595706694,
26.3793772227263));
#44158=CARTESIAN_POINT('Ctrl Pts',(19.074583357948,-0.676215978146822,26.0010972569083));
#44159=CARTESIAN_POINT('Ctrl Pts',(19.1163964149784,-0.210938010442085,
25.6841029814942));
#44160=CARTESIAN_POINT('Ctrl Pts',(19.1587385569805,0.310953319631399,25.7673975374766));
#44161=CARTESIAN_POINT('Ctrl Pts',(19.1904951634821,0.622827872514436,26.002955234302));
#44162=CARTESIAN_POINT('Ctrl Pts',(19.2222517699837,0.78509669838758,26.3628471470069));
#44163=CARTESIAN_POINT('Ctrl Pts',(19.2540083764853,0.754844992184846,26.7544025197296));
#44164=CARTESIAN_POINT('Ctrl Pts',(19.2857649829869,0.54124693951236,27.0849566894835));
#44165=CARTESIAN_POINT('Ctrl Pts',(19.3175215894885,0.195421936564938,27.2722990237309));
#44166=CARTESIAN_POINT('Ctrl Pts',(19.3492781959901,-0.197887083474027,
27.2719865803867));
#44167=CARTESIAN_POINT('Ctrl Pts',(19.3810348024917,-0.542997981900108,
27.0828076834802));
#44168=CARTESIAN_POINT('Ctrl Pts',(19.4090418657915,-0.730711463169429,
26.7917336743709));
#44169=CARTESIAN_POINT('Ctrl Pts',(19.4264633935907,-0.764227532302173,
26.5819107306037));
#44170=CARTESIAN_POINT('Ctrl Pts',(19.4332993858894,-0.764277110167741,
26.4997254257785));
#44171=CARTESIAN_POINT('Ctrl Pts',(19.1667006141106,-0.764283845936459,
26.50000006937));
#44172=CARTESIAN_POINT('Ctrl Pts',(19.1720113514992,-0.764283645388312,
26.4362228342538));
#44173=CARTESIAN_POINT('Ctrl Pts',(19.1879312917861,-0.740620064377401,
26.245038357094));
#44174=CARTESIAN_POINT('Ctrl Pts',(19.2144604349712,-0.582990039655113,
25.956660350341));
#44175=CARTESIAN_POINT('Ctrl Pts',(19.2462880436661,-0.251171142649758,
25.7436876185539));
#44176=CARTESIAN_POINT('Ctrl Pts',(19.2781156523609,0.142130424215859,25.7158480353013));
#44177=CARTESIAN_POINT('Ctrl Pts',(19.3099432610557,0.500640741350412,25.8799562843406));
#44178=CARTESIAN_POINT('Ctrl Pts',(19.3417708697505,0.736602229450057,26.1958412966923));
#44179=CARTESIAN_POINT('Ctrl Pts',(19.3735984784453,0.792255298302605,26.58617948445));
#44180=CARTESIAN_POINT('Ctrl Pts',(19.4054260871402,0.653976968680098,26.9554223157297));
#44181=CARTESIAN_POINT('Ctrl Pts',(19.437253695835,0.355615559299935,27.2131850637895));
#44182=CARTESIAN_POINT('Ctrl Pts',(19.4690813045298,-0.0297948390643188,
27.2963715394172));
#44183=CARTESIAN_POINT('Ctrl Pts',(19.5009089132246,-0.407911938387894,
27.1846190267216));
#44184=CARTESIAN_POINT('Ctrl Pts',(19.5327365219194,-0.686178733351599,
26.9052827496015));
#44185=CARTESIAN_POINT('Ctrl Pts',(19.5546670888814,-0.762180946991868,
26.6444506321226));
#44186=CARTESIAN_POINT('Ctrl Pts',(19.5659884529451,-0.764412940000839,
26.5085572294674));
#44187=CARTESIAN_POINT('Ctrl Pts',(19.5667006141106,-0.7644079673917,26.5000088022807));
#44188=CARTESIAN_POINT('Origin',(8.83329938588935,0.,26.5));
#44189=CARTESIAN_POINT('',(18.6332993858894,-0.763975585123095,26.5000842874006));
#44190=CARTESIAN_POINT('',(18.7667006141106,-0.76440770353066,26.4999910584554));
#44191=CARTESIAN_POINT('',(8.83329938588935,-0.76435,26.5000000000004));
#44192=CARTESIAN_POINT('Ctrl Pts',(18.6332993858894,-0.763975585123014,
26.5000842874006));
#44193=CARTESIAN_POINT('Ctrl Pts',(18.6496627437451,-0.762198505857026,
26.3040649899126));
#44194=CARTESIAN_POINT('Ctrl Pts',(18.6766116371014,-0.635771178646696,
25.981206808511));
#44195=CARTESIAN_POINT('Ctrl Pts',(18.7141460659582,-0.234472997417264,
25.7394602274647));
#44196=CARTESIAN_POINT('Ctrl Pts',(18.7459026724598,0.155802722384311,25.7185311453641));
#44197=CARTESIAN_POINT('Ctrl Pts',(18.7776592789614,0.511839522475942,25.8890924505991));
#44198=CARTESIAN_POINT('Ctrl Pts',(18.8094158854629,0.741094448594219,26.2079544172491));
#44199=CARTESIAN_POINT('Ctrl Pts',(18.8411724919646,0.790852991429545,26.5983571259894));
#44200=CARTESIAN_POINT('Ctrl Pts',(18.8729290984662,0.647208072939979,26.964496744374));
#44201=CARTESIAN_POINT('Ctrl Pts',(18.9046857049677,0.346303229108121,27.2177720053648));
#44202=CARTESIAN_POINT('Ctrl Pts',(18.9364423114694,-0.0394890010879801,
27.2955829454142));
#44203=CARTESIAN_POINT('Ctrl Pts',(18.9681989179709,-0.414953219279804,
27.1804421773526));
#44204=CARTESIAN_POINT('Ctrl Pts',(18.9999555244725,-0.690495493529877,
26.8977235614153));
#44205=CARTESIAN_POINT('Ctrl Pts',(19.0216556804454,-0.762301751285678,
26.640488566984));
#44206=CARTESIAN_POINT('Ctrl Pts',(19.0327703009176,-0.764134094038398,
26.5067722288323));
#44207=CARTESIAN_POINT('Ctrl Pts',(19.0332993858894,-0.764142366123026,
26.5004047868447));
#44208=CARTESIAN_POINT('Ctrl Pts',(18.7667006141106,-0.764407703530485,
26.4999910584554));
#44209=CARTESIAN_POINT('Ctrl Pts',(18.767425047155,-0.764412829262714,26.4912953170418));
#44210=CARTESIAN_POINT('Ctrl Pts',(18.7787586830977,-0.762139897682738,
26.3552545553671));
#44211=CARTESIAN_POINT('Ctrl Pts',(18.8007015219386,-0.685944244027812,
26.0943205018872));
#44212=CARTESIAN_POINT('Ctrl Pts',(18.8325291306334,-0.407515955991956,
25.8151451928656));
#44213=CARTESIAN_POINT('Ctrl Pts',(18.8643567393282,-0.0293342934702721,
25.7036113634181));
#44214=CARTESIAN_POINT('Ctrl Pts',(18.8961843480231,0.356027933769703,25.7870207074674));
#44215=CARTESIAN_POINT('Ctrl Pts',(18.9280119567179,0.654240229440685,26.0449559544106));
#44216=CARTESIAN_POINT('Ctrl Pts',(18.9598395654127,0.792305003299414,26.4142786901237));
#44217=CARTESIAN_POINT('Ctrl Pts',(18.9916671741075,0.736426211717768,26.8045846285138));
#44218=CARTESIAN_POINT('Ctrl Pts',(19.0234947828023,0.500282087197375,27.1203331318392));
#44219=CARTESIAN_POINT('Ctrl Pts',(19.0553223914972,0.141676926436067,27.2842340274076));
#44220=CARTESIAN_POINT('Ctrl Pts',(19.087150000192,-0.25160847507182,27.2561670030497));
#44221=CARTESIAN_POINT('Ctrl Pts',(19.1189776088868,-0.5833041547505,27.0430024164579));
#44222=CARTESIAN_POINT('Ctrl Pts',(19.145494480193,-0.740694544999679,26.7546667410442));
#44223=CARTESIAN_POINT('Ctrl Pts',(19.1614021486009,-0.764284046021185,
26.5636299301288));
#44224=CARTESIAN_POINT('Ctrl Pts',(19.1667006141106,-0.764283845936459,
26.50000006937));
#44225=CARTESIAN_POINT('Origin',(8.83329938588935,0.,26.5));
#44226=CARTESIAN_POINT('',(18.2332993858894,-0.764965412428307,26.5002633677415));
#44227=CARTESIAN_POINT('',(18.3667006141106,-0.764302619722667,26.5000145152404));
#44228=CARTESIAN_POINT('',(8.83329938588935,-0.76435,26.5000000000004));
#44229=CARTESIAN_POINT('Ctrl Pts',(18.2332993858894,-0.764965412428226,
26.5002633677415));
#44230=CARTESIAN_POINT('Ctrl Pts',(18.234798580071,-0.76508119305691,26.4823116736568));
#44231=CARTESIAN_POINT('Ctrl Pts',(18.2468833097532,-0.760677492458328,
26.3375307285701));
#44232=CARTESIAN_POINT('Ctrl Pts',(18.2695535749358,-0.669488757599245,
26.0696595117695));
#44233=CARTESIAN_POINT('Ctrl Pts',(18.3013101814374,-0.38458849635973,25.8021075061857));
#44234=CARTESIAN_POINT('Ctrl Pts',(18.333066787939,-0.00244655372769168,
25.7030155094137));
#44235=CARTESIAN_POINT('Ctrl Pts',(18.3648233944406,0.378359542695009,25.7990328449791));
#44236=CARTESIAN_POINT('Ctrl Pts',(18.3965800009422,0.668042185748427,26.0654402662492));
#44237=CARTESIAN_POINT('Ctrl Pts',(18.4283366074438,0.794220949673334,26.4379609214166));
#44238=CARTESIAN_POINT('Ctrl Pts',(18.4600932139454,0.7274175711474,26.8255549708114));
#44239=CARTESIAN_POINT('Ctrl Pts',(18.491849820447,0.482615591725175,27.1337143882872));
#44240=CARTESIAN_POINT('Ctrl Pts',(18.5236064269486,0.121339288012704,27.2876956564317));
#44241=CARTESIAN_POINT('Ctrl Pts',(18.5553630334502,-0.271557026497766,
27.2491494235501));
#44242=CARTESIAN_POINT('Ctrl Pts',(18.5871196399518,-0.594542196765398,
27.0290726886231));
#44243=CARTESIAN_POINT('Ctrl Pts',(18.6130984240982,-0.745442993191746,
26.7420693134418));
#44244=CARTESIAN_POINT('Ctrl Pts',(18.6284916727441,-0.764497708236297,
26.5576766569852));
#44245=CARTESIAN_POINT('Ctrl Pts',(18.6332993858894,-0.763975585123014,
26.5000842874006));
#44246=CARTESIAN_POINT('Ctrl Pts',(18.3667006141106,-0.764302619722492,
26.5000145152404));
#44247=CARTESIAN_POINT('Ctrl Pts',(18.373447945709,-0.764247307603586,26.4189908696697));
#44248=CARTESIAN_POINT('Ctrl Pts',(18.3908044802058,-0.731249504241009,
26.2105253289262));
#44249=CARTESIAN_POINT('Ctrl Pts',(18.4187702176008,-0.544899508122728,
25.9184677654519));
#44250=CARTESIAN_POINT('Ctrl Pts',(18.4505978262956,-0.199434270097742,
25.7284293306239));
#44251=CARTESIAN_POINT('Ctrl Pts',(18.4824254349904,0.194849834271444,25.7272587900961));
#44252=CARTESIAN_POINT('Ctrl Pts',(18.5142530436853,0.541437529129979,25.9152430383213));
#44253=CARTESIAN_POINT('Ctrl Pts',(18.5460806523801,0.755490150492264,26.2463663511633));
#44254=CARTESIAN_POINT('Ctrl Pts',(18.5779082610749,0.784610810040825,26.639575151346));
#44255=CARTESIAN_POINT('Ctrl Pts',(18.6097358697697,0.621671362865706,26.9986181728724));
#44256=CARTESIAN_POINT('Ctrl Pts',(18.6415634784645,0.306556707364476,27.2356074676479));
#44257=CARTESIAN_POINT('Ctrl Pts',(18.6733910871593,-0.0835981042838541,
27.2925318396574));
#44258=CARTESIAN_POINT('Ctrl Pts',(18.7052186958542,-0.453289446413202,
27.1554571230883));
#44259=CARTESIAN_POINT('Ctrl Pts',(18.7363218715046,-0.706133725022458,
26.8647089078388));
#44260=CARTESIAN_POINT('Ctrl Pts',(18.7568158442567,-0.764337763756458,
26.6186430211802));
#44261=CARTESIAN_POINT('Ctrl Pts',(18.7667006141106,-0.764407703530485,
26.4999910584554));
#44262=CARTESIAN_POINT('Origin',(8.83329938588935,0.,26.5));
#44263=CARTESIAN_POINT('',(17.8332993858894,-0.7642638282056,26.5001069462646));
#44264=CARTESIAN_POINT('',(17.9667006141106,-0.764094264662737,26.499903563092));
#44265=CARTESIAN_POINT('',(8.83329938588935,-0.76435,26.5000000000004));
#44266=CARTESIAN_POINT('Ctrl Pts',(17.8332993858894,-0.764263828205519,
26.5001069462646));
#44267=CARTESIAN_POINT('Ctrl Pts',(17.841105487398,-0.764502135910798,26.4059835619486));
#44268=CARTESIAN_POINT('Ctrl Pts',(17.8700826599076,-0.702119382636757,
26.0558542073795));
#44269=CARTESIAN_POINT('Ctrl Pts',(17.9096453679177,-0.29613832160412,25.711027047467));
#44270=CARTESIAN_POINT('Ctrl Pts',(17.9519875099199,0.231694148623007,25.7385828611072));
#44271=CARTESIAN_POINT('Ctrl Pts',(17.9837441164214,0.566653359359628,25.9398584184328));
#44272=CARTESIAN_POINT('Ctrl Pts',(18.0155007229231,0.766296209055916,26.2804493550768));
#44273=CARTESIAN_POINT('Ctrl Pts',(18.0472573294246,0.777290647856074,26.673205973088));
#44274=CARTESIAN_POINT('Ctrl Pts',(18.0790139359263,0.6005784561905,27.0241353676862));
#44275=CARTESIAN_POINT('Ctrl Pts',(18.1107705424278,0.275214785933559,27.2477375493297));
#44276=CARTESIAN_POINT('Ctrl Pts',(18.1425271489295,-0.113511804048443,
27.2877520601354));
#44277=CARTESIAN_POINT('Ctrl Pts',(18.1833700967499,-0.585770293594626,
27.095643467088));
#44278=CARTESIAN_POINT('Ctrl Pts',(18.2136275090699,-0.763446181435014,
26.7358189208944));
#44279=CARTESIAN_POINT('Ctrl Pts',(18.2332993858894,-0.764965412428226,
26.5002633677415));
#44280=CARTESIAN_POINT('Ctrl Pts',(17.9667006141106,-0.764094264662562,
26.499903563092));
#44281=CARTESIAN_POINT('Ctrl Pts',(17.9688616413648,-0.763991946430581,
26.4738963283246));
#44282=CARTESIAN_POINT('Ctrl Pts',(17.9816318715174,-0.755722265230173,
26.3202837748946));
#44283=CARTESIAN_POINT('Ctrl Pts',(18.0050113045682,-0.657888459085232,
26.0492639960516));
#44284=CARTESIAN_POINT('Ctrl Pts',(18.036838913263,-0.35974177500854,25.7889256783384));
#44285=CARTESIAN_POINT('Ctrl Pts',(18.0686665219578,0.0243332818644455,
25.7035686117623));
#44286=CARTESIAN_POINT('Ctrl Pts',(18.1004941306526,0.403587040260669,25.8126756400868));
#44287=CARTESIAN_POINT('Ctrl Pts',(18.1323217393475,0.683447187528216,26.0902880943639));
#44288=CARTESIAN_POINT('Ctrl Pts',(18.1641493480422,0.796329325103614,26.468054034611));
#44289=CARTESIAN_POINT('Ctrl Pts',(18.1959769567371,0.71411390092001,26.8537126167479));
#44290=CARTESIAN_POINT('Ctrl Pts',(18.2278045654319,0.457184295086093,27.1527494739896));
#44291=CARTESIAN_POINT('Ctrl Pts',(18.2596321741268,0.0882959257025597,
27.2920241365189));
#44292=CARTESIAN_POINT('Ctrl Pts',(18.2914597828215,-0.302180780501247,
27.237413173922));
#44293=CARTESIAN_POINT('Ctrl Pts',(18.3232873915164,-0.618701763158597,
27.0023010116041));
#44294=CARTESIAN_POINT('Ctrl Pts',(18.3483676686127,-0.748774141274869,
26.7201401454704));
#44295=CARTESIAN_POINT('Ctrl Pts',(18.3628387428108,-0.764334277909349,
26.5463888317932));
#44296=CARTESIAN_POINT('Ctrl Pts',(18.3667006141106,-0.764302619722492,
26.5000145152404));
#44297=CARTESIAN_POINT('Origin',(8.83329938588935,0.,26.5));
#44298=CARTESIAN_POINT('',(17.4332993858894,-0.76329981703839,26.5001479671982));
#44299=CARTESIAN_POINT('',(17.5667006141106,-0.764350395671289,26.5000203280756));
#44300=CARTESIAN_POINT('',(8.83329938588935,-0.76435,26.5000000000004));
#44301=CARTESIAN_POINT('Ctrl Pts',(17.4332993858894,-0.763299817038309,
26.5001479671982));
#44302=CARTESIAN_POINT('Ctrl Pts',(17.4474123947249,-0.762135941631699,
26.3309054434457));
#44303=CARTESIAN_POINT('Ctrl Pts',(17.472110939061,-0.664721913465502,26.0344563923922));
#44304=CARTESIAN_POINT('Ctrl Pts',(17.5073950188975,-0.313656364480858,
25.7685507409244));
#44305=CARTESIAN_POINT('Ctrl Pts',(17.5391516253991,0.072211731487986,25.7064298750071));
#44306=CARTESIAN_POINT('Ctrl Pts',(17.5709082319007,0.444301753746512,25.8383478091969));
#44307=CARTESIAN_POINT('Ctrl Pts',(17.6026648384023,0.70601938612131,26.1311526579745));
#44308=CARTESIAN_POINT('Ctrl Pts',(17.6344214449039,0.796820980869681,26.5140956120801));
#44309=CARTESIAN_POINT('Ctrl Pts',(17.6661780514055,0.692738004319475,26.8933825384317));
#44310=CARTESIAN_POINT('Ctrl Pts',(17.6979346579071,0.420331066798412,27.1770851633445));
#44311=CARTESIAN_POINT('Ctrl Pts',(17.7296912644087,0.0449434652133512,
27.2952930157502));
#44312=CARTESIAN_POINT('Ctrl Pts',(17.7614478709103,-0.34060148631374,27.2205420816171));
#44313=CARTESIAN_POINT('Ctrl Pts',(17.7932044774119,-0.644515709678365,
26.9685741610806));
#44314=CARTESIAN_POINT('Ctrl Pts',(17.8171549824049,-0.753381002992764,
26.6946505652555));
#44315=CARTESIAN_POINT('Ctrl Pts',(17.8305199518974,-0.764178976562752,
26.5336204399747));
#44316=CARTESIAN_POINT('Ctrl Pts',(17.8332993858894,-0.764263828205519,
26.5001069462646));
#44317=CARTESIAN_POINT('Ctrl Pts',(17.5667006141106,-0.764350395671114,
26.5000203280756));
#44318=CARTESIAN_POINT('Ctrl Pts',(17.5748845399189,-0.764254594178374,
26.4017577472398));
#44319=CARTESIAN_POINT('Ctrl Pts',(17.5936776686255,-0.720583009812041,
26.1760195175961));
#44320=CARTESIAN_POINT('Ctrl Pts',(17.6230800002304,-0.504252400540365,
25.882996417912));
#44321=CARTESIAN_POINT('Ctrl Pts',(17.6549076089252,-0.146898168000676,
25.7165983131021));
#44322=CARTESIAN_POINT('Ctrl Pts',(17.68673521762,0.246892880351082,25.7424124008351));
#44323=CARTESIAN_POINT('Ctrl Pts',(17.7185628263148,0.579346349872695,25.9528266796507));
#44324=CARTESIAN_POINT('Ctrl Pts',(17.7503904350096,0.771677592213418,26.2987691287884));
#44325=CARTESIAN_POINT('Ctrl Pts',(17.7822180437045,0.772008340680367,26.6910250850529));
#44326=CARTESIAN_POINT('Ctrl Pts',(17.8246548552975,0.527363192762192,27.1585233970218));
#44327=CARTESIAN_POINT('Ctrl Pts',(17.8777008697889,-0.155425403013523,
27.3905262878577));
#44328=CARTESIAN_POINT('Ctrl Pts',(17.928585857026,-0.696286520605016,26.9592635474336));
#44329=CARTESIAN_POINT('Ctrl Pts',(17.9582524384666,-0.764494260726312,
26.6015745100437));
#44330=CARTESIAN_POINT('Ctrl Pts',(17.9667006141106,-0.764094264662562,
26.499903563092));
#44331=CARTESIAN_POINT('Origin',(8.83329938588935,0.,26.5));
#44332=CARTESIAN_POINT('',(17.0332993858894,-0.765203811462457,26.5004911225311));
#44333=CARTESIAN_POINT('',(17.1667006141106,-0.764310045233437,26.4999834783144));
#44334=CARTESIAN_POINT('',(8.83329938588935,-0.76435,26.5000000000004));
#44335=CARTESIAN_POINT('Ctrl Pts',(17.0332993858894,-0.765203811462376,
26.5004911225311));
#44336=CARTESIAN_POINT('Ctrl Pts',(17.0431337665513,-0.76521128941822,26.382487512764));
#44337=CARTESIAN_POINT('Ctrl Pts',(17.0635536827138,-0.705242476473079,
26.1359384245521));
#44338=CARTESIAN_POINT('Ctrl Pts',(17.0945591343768,-0.456300068822577,
25.846732592974));
#44339=CARTESIAN_POINT('Ctrl Pts',(17.1263157408784,-0.0867895361857581,
25.7077530010661));
#44340=CARTESIAN_POINT('Ctrl Pts',(17.1580723473799,0.30203843095996,25.7629217202603));
#44341=CARTESIAN_POINT('Ctrl Pts',(17.1898289538815,0.618293167806677,25.9971718615475));
#44342=CARTESIAN_POINT('Ctrl Pts',(17.2215855603831,0.78319257186756,26.3542436602263));
#44343=CARTESIAN_POINT('Ctrl Pts',(17.2533421668847,0.757790262318726,26.7467316287404));
#44344=CARTESIAN_POINT('Ctrl Pts',(17.2850987733863,0.546980915086662,27.0790712241793));
#44345=CARTESIAN_POINT('Ctrl Pts',(17.316855379888,0.20403256237055,27.2704274425122));
#44346=CARTESIAN_POINT('Ctrl Pts',(17.3486119863895,-0.190736679054125,
27.2736844177905));
#44347=CARTESIAN_POINT('Ctrl Pts',(17.3803685928912,-0.535201811279513,
27.0890308594029));
#44348=CARTESIAN_POINT('Ctrl Pts',(17.4085977260577,-0.731262683123162,
26.7962743064247));
#44349=CARTESIAN_POINT('Ctrl Pts',(17.4262413237238,-0.763881883206379,
26.5847879095112));
#44350=CARTESIAN_POINT('Ctrl Pts',(17.4332993858894,-0.763299817038309,
26.5001479671982));
#44351=CARTESIAN_POINT('Ctrl Pts',(17.1667006141106,-0.764310045233262,
26.4999834783144));
#44352=CARTESIAN_POINT('Ctrl Pts',(17.1702982355747,-0.764343861225088,
26.4567834827247));
#44353=CARTESIAN_POINT('Ctrl Pts',(17.1845050599371,-0.750124293143909,
26.2862109162653));
#44354=CARTESIAN_POINT('Ctrl Pts',(17.2093210871977,-0.624906846574195,
26.0054427956063));
#44355=CARTESIAN_POINT('Ctrl Pts',(17.2411486958926,-0.311342909206791,
25.7664054968385));
#44356=CARTESIAN_POINT('Ctrl Pts',(17.2729763045874,0.0784326585839467,
25.7069402585764));
#44357=CARTESIAN_POINT('Ctrl Pts',(17.3048039132822,0.449009401771598,25.8416035517627));
#44358=CARTESIAN_POINT('Ctrl Pts',(17.336631521977,0.709675400200942,26.1374313304758));
#44359=CARTESIAN_POINT('Ctrl Pts',(17.3684591306719,0.796625066564042,26.5220108860288));
#44360=CARTESIAN_POINT('Ctrl Pts',(17.4002867393666,0.688572116174983,26.9012010606094));
#44361=CARTESIAN_POINT('Ctrl Pts',(17.4321143480615,0.411970711104484,27.1821864196729));
#44362=CARTESIAN_POINT('Ctrl Pts',(17.4639419567563,0.0345198850269114,
27.296178240544));
#44363=CARTESIAN_POINT('Ctrl Pts',(17.4957695654511,-0.351370292731717,
27.2152882780459));
#44364=CARTESIAN_POINT('Ctrl Pts',(17.5275971741459,-0.651270599572141,
26.9592885385028));
#44365=CARTESIAN_POINT('Ctrl Pts',(17.5512408570324,-0.75560037060335,26.6856230225073));
#44366=CARTESIAN_POINT('Ctrl Pts',(17.5642753370206,-0.764378786100226,
26.5291400918272));
#44367=CARTESIAN_POINT('Ctrl Pts',(17.5667006141106,-0.764350395671114,
26.5000203280756));
#44368=CARTESIAN_POINT('Origin',(8.83329938588935,0.,26.5));
#44369=CARTESIAN_POINT('',(16.6332993858894,-0.764172016402676,26.4996705939536));
#44370=CARTESIAN_POINT('',(16.7667006141106,-0.764401227565655,26.5000117829436));
#44371=CARTESIAN_POINT('',(8.83329938588935,-0.76435,26.5000000000004));
#44372=CARTESIAN_POINT('Ctrl Pts',(16.6332993858894,-0.764172016402596,
26.4996705939536));
#44373=CARTESIAN_POINT('Ctrl Pts',(16.6388551383777,-0.76423249137171,26.4331523910536));
#44374=CARTESIAN_POINT('Ctrl Pts',(16.6549964263666,-0.739381154229132,
26.2401092740816));
#44375=CARTESIAN_POINT('Ctrl Pts',(16.681723249856,-0.577011248722235,25.9502311851775));
#44376=CARTESIAN_POINT('Ctrl Pts',(16.7134798563576,-0.244173820480448,
25.7417844965558));
#44377=CARTESIAN_POINT('Ctrl Pts',(16.7452364628592,0.148607952543154,25.7170324051763));
#44378=CARTESIAN_POINT('Ctrl Pts',(16.7769930693608,0.504838200497434,25.8837420128997));
#44379=CARTESIAN_POINT('Ctrl Pts',(16.8087496758624,0.738401842223993,26.2001912317773));
#44380=CARTESIAN_POINT('Ctrl Pts',(16.840506282364,0.791443309939019,26.5901614741675));
#44381=CARTESIAN_POINT('Ctrl Pts',(16.8722628888656,0.652584945679744,26.9575157041844));
#44382=CARTESIAN_POINT('Ctrl Pts',(16.9040194953672,0.352864424260747,27.2144611647807));
#44383=CARTESIAN_POINT('Ctrl Pts',(16.9357761018688,-0.0295172027510032,
27.2953157045016));
#44384=CARTESIAN_POINT('Ctrl Pts',(16.9781182438709,-0.537397266224523,
27.1491432563852));
#44385=CARTESIAN_POINT('Ctrl Pts',(17.0106260052111,-0.760267862974393,
26.7724256846253));
#44386=CARTESIAN_POINT('Ctrl Pts',(17.0325482310508,-0.765203240292426,
26.5095042963645));
#44387=CARTESIAN_POINT('Ctrl Pts',(17.0332993858894,-0.765203811462376,
26.5004911225311));
#44388=CARTESIAN_POINT('Ctrl Pts',(16.7667006141106,-0.764401227565479,
26.5000117829436));
#44389=CARTESIAN_POINT('Ctrl Pts',(16.7763211341288,-0.764315896056895,
26.3845289078875));
#44390=CARTESIAN_POINT('Ctrl Pts',(16.7965508570452,-0.708503173963334,
26.1416155285519));
#44391=CARTESIAN_POINT('Ctrl Pts',(16.8273897828599,-0.461416157419982,
25.8502381275293));
#44392=CARTESIAN_POINT('Ctrl Pts',(16.8592173915548,-0.0934603563117058,
25.7085705824253));
#44393=CARTESIAN_POINT('Ctrl Pts',(16.8910450002496,0.29737304194578,25.7606322733754));
#44394=CARTESIAN_POINT('Ctrl Pts',(16.9228726089444,0.615414286049196,25.9936793330608));
#44395=CARTESIAN_POINT('Ctrl Pts',(16.9547002176392,0.782811976792353,26.3506655763249));
#44396=CARTESIAN_POINT('Ctrl Pts',(16.986527826334,0.758589843209824,26.7442064932981));
#44397=CARTESIAN_POINT('Ctrl Pts',(17.0183554350289,0.548677074193156,27.0779695742253));
#44398=CARTESIAN_POINT('Ctrl Pts',(17.0501830437237,0.204456953247554,27.270254968634));
#44399=CARTESIAN_POINT('Ctrl Pts',(17.0820106524185,-0.189810955467986,
27.273994290092));
#44400=CARTESIAN_POINT('Ctrl Pts',(17.1138382611133,-0.537616179499631,
27.0882722200051));
#44401=CARTESIAN_POINT('Ctrl Pts',(17.142068248344,-0.729382894522571,26.7958204943258));
#44402=CARTESIAN_POINT('Ctrl Pts',(17.1596890326764,-0.764244139583423,
26.5841780746757));
#44403=CARTESIAN_POINT('Ctrl Pts',(17.1667006141106,-0.764310045233262,
26.4999834783144));
#44404=CARTESIAN_POINT('Origin',(8.83329938588935,0.,26.5));
#44405=CARTESIAN_POINT('',(16.2332993858894,-0.764419552496706,26.4999089030413));
#44406=CARTESIAN_POINT('',(16.3667006141106,-0.764284539029021,26.4999969545263));
#44407=CARTESIAN_POINT('',(8.83329938588935,-0.76435,26.5000000000004));
#44408=CARTESIAN_POINT('Ctrl Pts',(16.2332993858894,-0.764419552496625,
26.4999089030413));
#44409=CARTESIAN_POINT('Ctrl Pts',(16.2345765102041,-0.764440883098184,
26.4845572251809));
#44410=CARTESIAN_POINT('Ctrl Pts',(16.2464391700194,-0.760308610213227,
26.3420005829642));
#44411=CARTESIAN_POINT('Ctrl Pts',(16.2688873653352,-0.675403430232317,
26.0776946475575));
#44412=CARTESIAN_POINT('Ctrl Pts',(16.3006439718369,-0.391057471568795,
25.8055962039035));
#44413=CARTESIAN_POINT('Ctrl Pts',(16.3324005783384,-0.0112469392005812,
25.7034392542279));
#44414=CARTESIAN_POINT('Ctrl Pts',(16.3641571848401,0.371296397184491,25.7948322443979));
#44415=CARTESIAN_POINT('Ctrl Pts',(16.3959137913416,0.663211193852015,26.0587942468411));
#44416=CARTESIAN_POINT('Ctrl Pts',(16.4276703978433,0.79383189911164,26.4291575914007));
#44417=CARTESIAN_POINT('Ctrl Pts',(16.4594270043448,0.730299950020167,26.8187946688532));
#44418=CARTESIAN_POINT('Ctrl Pts',(16.4911836108465,0.490067202099917,27.127082508535));
#44419=CARTESIAN_POINT('Ctrl Pts',(16.5335257528485,0.00755075451268908,
27.3426896078416));
#44420=CARTESIAN_POINT('Ctrl Pts',(16.5758678948507,-0.530671740917147,
27.1546528029804));
#44421=CARTESIAN_POINT('Ctrl Pts',(16.6126542843645,-0.742027902742413,
26.7470388885421));
#44422=CARTESIAN_POINT('Ctrl Pts',(16.6282696028772,-0.764117266668342,
26.5598914421017));
#44423=CARTESIAN_POINT('Ctrl Pts',(16.6332993858894,-0.764172016402596,
26.4996705939536));
#44424=CARTESIAN_POINT('Ctrl Pts',(16.3667006141106,-0.764284539028846,
26.4999969545263));
#44425=CARTESIAN_POINT('Ctrl Pts',(16.3717348297846,-0.764292894067563,
26.4395406561741));
#44426=CARTESIAN_POINT('Ctrl Pts',(16.3873782483568,-0.742275719971854,
26.2516835762977));
#44427=CARTESIAN_POINT('Ctrl Pts',(16.4136308698273,-0.590020482577639,
25.9643030788146));
#44428=CARTESIAN_POINT('Ctrl Pts',(16.4454584785221,-0.261004878818793,
25.7470246919976));
#44429=CARTESIAN_POINT('Ctrl Pts',(16.477286087217,0.131900535795971,25.7140625916236));
#44430=CARTESIAN_POINT('Ctrl Pts',(16.5091136959118,0.492518813396506,25.8734853715362));
#44431=CARTESIAN_POINT('Ctrl Pts',(16.5409413046066,0.732576379744177,26.1862688904977));
#44432=CARTESIAN_POINT('Ctrl Pts',(16.5727689133014,0.793310990324887,26.5758487564716));
#44433=CARTESIAN_POINT('Ctrl Pts',(16.6045965219962,0.659855785944694,26.9468620625921));
#44434=CARTESIAN_POINT('Ctrl Pts',(16.636424130691,0.364878461567863,27.2084906982538));
#44435=CARTESIAN_POINT('Ctrl Pts',(16.6682517393859,-0.0194152617984515,
27.2966921669241));
#44436=CARTESIAN_POINT('Ctrl Pts',(16.7000793480807,-0.398956440272542,
27.1898761627955));
#44437=CARTESIAN_POINT('Ctrl Pts',(16.7319069567755,-0.680839476780989,
26.9141895315969));
#44438=CARTESIAN_POINT('Ctrl Pts',(16.7541140454521,-0.761235069795498,
26.651093842388));
#44439=CARTESIAN_POINT('Ctrl Pts',(16.7657119312305,-0.764409996925297,
26.5118797423986));
#44440=CARTESIAN_POINT('Ctrl Pts',(16.7667006141106,-0.764401227565479,
26.5000117829436));
#44441=CARTESIAN_POINT('Origin',(8.83329938588935,0.,26.5));
#44442=CARTESIAN_POINT('',(15.8332993858894,-0.7642585736457,26.5000568905623));
#44443=CARTESIAN_POINT('',(15.9667006141106,-0.764412740073756,26.4999943266675));
#44444=CARTESIAN_POINT('',(8.83329938588935,-0.76435,26.5000000000004));
#44445=CARTESIAN_POINT('Ctrl Pts',(15.8332993858894,-0.764258573645619,
26.5000568905623));
#44446=CARTESIAN_POINT('Ctrl Pts',(15.8408834175311,-0.764191761169323,
26.4089790323552));
#44447=CARTESIAN_POINT('Ctrl Pts',(15.8590529846733,-0.725349790004131,
26.1906373179569));
#44448=CARTESIAN_POINT('Ctrl Pts',(15.8878080873161,-0.522035840432493,
25.8982408316857));
#44449=CARTESIAN_POINT('Ctrl Pts',(15.9195646938177,-0.17065433029262,25.7215401887988));
#44450=CARTESIAN_POINT('Ctrl Pts',(15.9513213003193,0.222669695330672,25.7351929582878));
#44451=CARTESIAN_POINT('Ctrl Pts',(15.9830779068209,0.561259543601463,25.9341595139798));
#44452=CARTESIAN_POINT('Ctrl Pts',(16.0148345133225,0.763833671200898,26.2730062101543));
#44453=CARTESIAN_POINT('Ctrl Pts',(16.0465911198241,0.778876573811572,26.6635531040737));
#44454=CARTESIAN_POINT('Ctrl Pts',(16.0889332618262,0.548943088162816,27.1394093172736));
#44455=CARTESIAN_POINT('Ctrl Pts',(16.1312754038283,0.016244012154183,27.3425668644846));
#44456=CARTESIAN_POINT('Ctrl Pts',(16.1736175458305,-0.47216734905144,27.1406686581801));
#44457=CARTESIAN_POINT('Ctrl Pts',(16.2040970280173,-0.711000868579955,
26.8514066340567));
#44458=CARTESIAN_POINT('Ctrl Pts',(16.2239909747036,-0.764264082893658,
26.6118006963973));
#44459=CARTESIAN_POINT('Ctrl Pts',(16.2332993858894,-0.764419552496625,
26.4999089030413));
#44460=CARTESIAN_POINT('Ctrl Pts',(15.9667006141106,-0.764412740073581,
26.4999943266675));
#44461=CARTESIAN_POINT('Ctrl Pts',(15.9671485254403,-0.764414872326465,
26.4946179201944));
#44462=CARTESIAN_POINT('Ctrl Pts',(15.9782056396684,-0.763044002953407,
26.3618973388524));
#44463=CARTESIAN_POINT('Ctrl Pts',(15.9998719567947,-0.691172178101171,
26.1032930786494));
#44464=CARTESIAN_POINT('Ctrl Pts',(16.0316995654895,-0.416405297022751,
25.8205134366008));
#44465=CARTESIAN_POINT('Ctrl Pts',(16.0635271741844,-0.0397090735252242,
25.7040612142204));
#44466=CARTESIAN_POINT('Ctrl Pts',(16.0953547828791,0.346707294700135,25.782442049009));
#44467=CARTESIAN_POINT('Ctrl Pts',(16.127182391574,0.648255274330614,26.0364695689265));
#44468=CARTESIAN_POINT('Ctrl Pts',(16.1590100002688,0.791120753270836,26.4039619087403));
#44469=CARTESIAN_POINT('Ctrl Pts',(16.1908376089636,0.740332552174896,26.7949628339619));
#44470=CARTESIAN_POINT('Ctrl Pts',(16.2226652176584,0.508322808619745,27.1137615851986));
#44471=CARTESIAN_POINT('Ctrl Pts',(16.2544928263532,0.151883789093077,27.2823213379676));
#44472=CARTESIAN_POINT('Ctrl Pts',(16.2863204350481,-0.24173394755624,27.2593813665264));
#44473=CARTESIAN_POINT('Ctrl Pts',(16.3181480437429,-0.576179088441399,
27.0505570081939));
#44474=CARTESIAN_POINT('Ctrl Pts',(16.3449414367637,-0.738993578414591,
26.7613115100435));
#44475=CARTESIAN_POINT('Ctrl Pts',(16.3611256268863,-0.764275286498338,
26.5669474216436));
#44476=CARTESIAN_POINT('Ctrl Pts',(16.3667006141106,-0.764284539028846,
26.4999969545263));
#44477=CARTESIAN_POINT('Origin',(8.83329938588935,0.,26.5));
#44478=CARTESIAN_POINT('',(15.4332993858894,-0.764307134319736,26.4999943060657));
#44479=CARTESIAN_POINT('',(15.5667006141106,-0.764296441926655,26.5000122845045));
#44480=CARTESIAN_POINT('',(8.83329938588935,-0.76435,26.5000000000004));
#44481=CARTESIAN_POINT('Ctrl Pts',(15.4332993858894,-0.764307134319656,
26.4999943060657));
#44482=CARTESIAN_POINT('Ctrl Pts',(15.4366047893575,-0.764328149531655,
26.4603037681963));
#44483=CARTESIAN_POINT('Ctrl Pts',(15.4504957283262,-0.751518870125793,
26.2935211503543));
#44484=CARTESIAN_POINT('Ctrl Pts',(15.4749722027953,-0.632243102185288,
26.0148286510498));
#44485=CARTESIAN_POINT('Ctrl Pts',(15.5067288092969,-0.32272804759704,25.7717430319143));
#44486=CARTESIAN_POINT('Ctrl Pts',(15.5384854157985,0.0643873344812935,
25.7056184782728));
#44487=CARTESIAN_POINT('Ctrl Pts',(15.5702420223001,0.43767439511808,25.8341102330364));
#44488=CARTESIAN_POINT('Ctrl Pts',(15.6019986288018,0.700909172129369,26.1230057460524));
#44489=CARTESIAN_POINT('Ctrl Pts',(15.6443407708038,0.831835447076346,26.6350280639177));
#44490=CARTESIAN_POINT('Ctrl Pts',(15.686682912806,0.555510380759211,27.1337120844097));
#44491=CARTESIAN_POINT('Ctrl Pts',(15.7290250548081,0.0519596797800127,
27.2941653019125));
#44492=CARTESIAN_POINT('Ctrl Pts',(15.7607816613097,-0.332552292829113,
27.2241388198563));
#44493=CARTESIAN_POINT('Ctrl Pts',(15.7925382678113,-0.639407707442898,
26.9757578318493));
#44494=CARTESIAN_POINT('Ctrl Pts',(15.8167108426712,-0.752956785112338,
26.6992298118808));
#44495=CARTESIAN_POINT('Ctrl Pts',(15.8302978820306,-0.764285015769663,
26.5361024341171));
#44496=CARTESIAN_POINT('Ctrl Pts',(15.8332993858894,-0.764258573645619,
26.5000568905623));
#44497=CARTESIAN_POINT('Ctrl Pts',(15.5667006141106,-0.764296441926479,
26.5000122845045));
#44498=CARTESIAN_POINT('Ctrl Pts',(15.5731714239944,-0.764252283086693,
26.4223072739739));
#44499=CARTESIAN_POINT('Ctrl Pts',(15.5902514367765,-0.733154199056112,
26.2171666244304));
#44500=CARTESIAN_POINT('Ctrl Pts',(15.6179406524569,-0.552431099026793,
25.9256175124043));
#44501=CARTESIAN_POINT('Ctrl Pts',(15.6497682611517,-0.209471088532158,
25.7310934879338));
#44502=CARTESIAN_POINT('Ctrl Pts',(15.6815958698465,0.184764086958111,25.7247854533105));
#44503=CARTESIAN_POINT('Ctrl Pts',(15.7134234785413,0.533771975425466,25.9082375143023));
#44504=CARTESIAN_POINT('Ctrl Pts',(15.7452510872362,0.752121039795552,26.2365435468138));
#44505=CARTESIAN_POINT('Ctrl Pts',(15.7770786959309,0.78636292888696,26.6293394962914));
#44506=CARTESIAN_POINT('Ctrl Pts',(15.8089063046258,0.628115777091278,26.9904752101765));
#44507=CARTESIAN_POINT('Ctrl Pts',(15.8407339133206,0.316115950726511,27.2315504541211));
#44508=CARTESIAN_POINT('Ctrl Pts',(15.8725615220154,-0.073263993557323,
27.2935538724477));
#44509=CARTESIAN_POINT('Ctrl Pts',(15.9043891307102,-0.444710086519647,
27.1613080221623));
#44510=CARTESIAN_POINT('Ctrl Pts',(15.9357688280753,-0.703602863161262,
26.8713237799752));
#44511=CARTESIAN_POINT('Ctrl Pts',(15.9565393225421,-0.764364367902979,
26.6219631855317));
#44512=CARTESIAN_POINT('Ctrl Pts',(15.9667006141106,-0.764412740073581,
26.4999943266675));
#44513=CARTESIAN_POINT('Origin',(8.83329938588935,0.,26.5));
#44514=CARTESIAN_POINT('',(15.0332993858894,-0.764434241529034,26.5000259538096));
#44515=CARTESIAN_POINT('',(15.1667006141106,-0.764371352146507,26.4999814664004));
#44516=CARTESIAN_POINT('',(8.83329938588935,-0.76435,26.5000000000004));
#44517=CARTESIAN_POINT('Ctrl Pts',(15.0332993858894,-0.764434241528954,
26.5000259538096));
#44518=CARTESIAN_POINT('Ctrl Pts',(15.0429116966845,-0.764309333684609,
26.3846361440151));
#44519=CARTESIAN_POINT('Ctrl Pts',(15.0631095429801,-0.708387433195622,
26.1420365804305));
#44520=CARTESIAN_POINT('Ctrl Pts',(15.0938929247762,-0.462805184149422,
25.8511555714751));
#44521=CARTESIAN_POINT('Ctrl Pts',(15.1256495312778,-0.0945878860313145,
25.7087849914816));
#44522=CARTESIAN_POINT('Ctrl Pts',(15.1574061377794,0.292880226372572,25.7599868189792));
#44523=CARTESIAN_POINT('Ctrl Pts',(15.1997482797815,0.723012441153252,26.067061437389));
#44524=CARTESIAN_POINT('Ctrl Pts',(15.2420904217837,0.833184204547314,26.6264391962602));
#44525=CARTESIAN_POINT('Ctrl Pts',(15.2844325637858,0.551618642248873,27.0736856356996));
#44526=CARTESIAN_POINT('Ctrl Pts',(15.3161891702874,0.21250416882743,27.2679909088782));
#44527=CARTESIAN_POINT('Ctrl Pts',(15.347945776789,-0.182199657223414,27.2758808000015));
#44528=CARTESIAN_POINT('Ctrl Pts',(15.3797023832906,-0.530413882922957,
27.0942833642916));
#44529=CARTESIAN_POINT('Ctrl Pts',(15.408153586324,-0.727612087344244,26.8019865156775));
#44530=CARTESIAN_POINT('Ctrl Pts',(15.426019253857,-0.7642608484367,26.587412486301));
#44531=CARTESIAN_POINT('Ctrl Pts',(15.4332993858894,-0.764307134319656,
26.4999943060657));
#44532=CARTESIAN_POINT('Ctrl Pts',(15.1667006141106,-0.764371352146331,
26.4999814664004));
#44533=CARTESIAN_POINT('Ctrl Pts',(15.1685851196502,-0.764394352807559,
26.4773576674607));
#44534=CARTESIAN_POINT('Ctrl Pts',(15.1810788280881,-0.757868527003245,
26.3273818655522));
#44535=CARTESIAN_POINT('Ctrl Pts',(15.2041817394243,-0.6627532402055,26.0574466090676));
#44536=CARTESIAN_POINT('Ctrl Pts',(15.2360093481191,-0.369486777125133,
25.7939016479567));
#44537=CARTESIAN_POINT('Ctrl Pts',(15.2678369568139,0.0142241267301174,
25.7031982458306));
#44538=CARTESIAN_POINT('Ctrl Pts',(15.2996645655087,0.394453192351198,25.8075391417037));
#44539=CARTESIAN_POINT('Ctrl Pts',(15.3314921742035,0.678126438920626,26.0813833566788));
#44540=CARTESIAN_POINT('Ctrl Pts',(15.3633197828983,0.795805202493795,26.4576982162029));
#44541=CARTESIAN_POINT('Ctrl Pts',(15.3951473915932,0.718683607945039,26.8443678743723));
#44542=CARTESIAN_POINT('Ctrl Pts',(15.426975000288,0.465639785487568,27.1467417965461));
#44543=CARTESIAN_POINT('Ctrl Pts',(15.4588026089828,0.0986148069826778,
27.2908036931327));
#44544=CARTESIAN_POINT('Ctrl Pts',(15.4906302176776,-0.292549495638406,
27.2412895209231));
#44545=CARTESIAN_POINT('Ctrl Pts',(15.5224578263724,-0.612102370814474,
27.0103195556432));
#44546=CARTESIAN_POINT('Ctrl Pts',(15.5478146251834,-0.747316944725573,
26.7267864498628));
#44547=CARTESIAN_POINT('Ctrl Pts',(15.5625622210961,-0.7643246836207,26.5497083625134));
#44548=CARTESIAN_POINT('Ctrl Pts',(15.5667006141106,-0.764296441926479,
26.5000122845045));
#44549=CARTESIAN_POINT('Origin',(8.83329938588935,0.,26.5));
#44550=CARTESIAN_POINT('',(14.6332993858894,-0.764344384160412,26.5000700212582));
#44551=CARTESIAN_POINT('',(14.7667006141106,-0.764340249516096,26.5000200137165));
#44552=CARTESIAN_POINT('',(8.83329938588935,-0.76435,26.5000000000004));
#44553=CARTESIAN_POINT('Ctrl Pts',(14.6332993858894,-0.764344384160332,
26.5000700212582));
#44554=CARTESIAN_POINT('Ctrl Pts',(14.6386330685109,-0.764379701483647,
26.43606499794));
#44555=CARTESIAN_POINT('Ctrl Pts',(14.6545522866329,-0.740679592119133,
26.2449843755321));
#44556=CARTESIAN_POINT('Ctrl Pts',(14.6810570402554,-0.582308270804313,
25.9560467523384));
#44557=CARTESIAN_POINT('Ctrl Pts',(14.712813646757,-0.25306744493287,25.7454437042873));
#44558=CARTESIAN_POINT('Ctrl Pts',(14.7551557887592,0.273719354082281,25.7029676893257));
#44559=CARTESIAN_POINT('Ctrl Pts',(14.7974979307613,0.718507527034393,26.059625474564));
#44560=CARTESIAN_POINT('Ctrl Pts',(14.8398400727634,0.791517698526367,26.5830546085662));
#44561=CARTESIAN_POINT('Ctrl Pts',(14.871596679265,0.657491382035733,26.9501923371599));
#44562=CARTESIAN_POINT('Ctrl Pts',(14.9033532857666,0.360807099282544,27.2106377192428));
#44563=CARTESIAN_POINT('Ctrl Pts',(14.9351098922682,-0.0224710100972664,
27.2962453503641));
#44564=CARTESIAN_POINT('Ctrl Pts',(14.9668664987698,-0.401047778060038,
27.1886822618713));
#44565=CARTESIAN_POINT('Ctrl Pts',(14.9986231052714,-0.681355176354821,
26.912784010108));
#44566=CARTESIAN_POINT('Ctrl Pts',(15.0207674009779,-0.761372084745381,
26.6504566973273));
#44567=CARTESIAN_POINT('Ctrl Pts',(15.0323261611839,-0.764446888165399,
26.5117089108056));
#44568=CARTESIAN_POINT('Ctrl Pts',(15.0332993858894,-0.764434241528954,
26.5000259538096));
#44569=CARTESIAN_POINT('Ctrl Pts',(14.7667006141106,-0.764340249515921,
26.5000200137165));
#44570=CARTESIAN_POINT('Ctrl Pts',(14.7746080182043,-0.764244504017631,
26.4050792053235));
#44571=CARTESIAN_POINT('Ctrl Pts',(14.7931246251962,-0.722720395989046,
26.1826768460789));
#44572=CARTESIAN_POINT('Ctrl Pts',(14.8222504350865,-0.512310886867079,
25.8895633395461));
#44573=CARTESIAN_POINT('Ctrl Pts',(14.8540780437813,-0.156977657442333,
25.71868484189));
#44574=CARTESIAN_POINT('Ctrl Pts',(14.8859056524761,0.236781186430625,25.7390597717421));
#44575=CARTESIAN_POINT('Ctrl Pts',(14.9177332611709,0.572579791078355,25.9457006728515));
#44576=CARTESIAN_POINT('Ctrl Pts',(14.9495608698657,0.768220040382449,26.2880251647402));
#44577=CARTESIAN_POINT('Ctrl Pts',(14.9813884785605,0.775812337104691,26.6822376986926));
#44578=CARTESIAN_POINT('Ctrl Pts',(15.0132160872554,0.593498208699499,27.0318413649756));
#44579=CARTESIAN_POINT('Ctrl Pts',(15.0450436959502,0.265905231604842,27.2512587896549));
#44580=CARTESIAN_POINT('Ctrl Pts',(15.076871304645,-0.126777084163142,27.2867801040696));
#44581=CARTESIAN_POINT('Ctrl Pts',(15.1086989133398,-0.488426401756141,
27.129710259799));
#44582=CARTESIAN_POINT('Ctrl Pts',(15.138642016495,-0.716182649017405,26.8369242782581));
#44583=CARTESIAN_POINT('Ctrl Pts',(15.1579759167519,-0.764264865959882,
26.6047228931048));
#44584=CARTESIAN_POINT('Ctrl Pts',(15.1667006141106,-0.764371352146331,
26.4999814664004));
#44585=CARTESIAN_POINT('Origin',(8.83329938588935,0.,26.5));
#44586=CARTESIAN_POINT('',(14.2332993858894,-0.764405081589298,26.4996880256457));
#44587=CARTESIAN_POINT('',(14.3667006141106,-0.764318529753706,26.4999818788456));
#44588=CARTESIAN_POINT('',(8.83329938588935,-0.76435,26.5000000000004));
#44589=CARTESIAN_POINT('Ctrl Pts',(14.2332993858894,-0.764405081589217,
26.4996880256457));
#44590=CARTESIAN_POINT('Ctrl Pts',(14.2343544403373,-0.764414798326942,
26.4870305763771));
#44591=CARTESIAN_POINT('Ctrl Pts',(14.2459950302857,-0.761012346251615,
26.3474474462872));
#44592=CARTESIAN_POINT('Ctrl Pts',(14.2682211557347,-0.679844423442565,
26.0862248255409));
#44593=CARTESIAN_POINT('Ctrl Pts',(14.3105632977368,-0.304469510421639,
25.714200339602));
#44594=CARTESIAN_POINT('Ctrl Pts',(14.352905439739,0.26548215438068,25.7001862624564));
#44595=CARTESIAN_POINT('Ctrl Pts',(14.3952475817411,0.658687214192637,26.0533127616064));
#44596=CARTESIAN_POINT('Ctrl Pts',(14.4270041882427,0.79286270006155,26.4203960004784));
#44597=CARTESIAN_POINT('Ctrl Pts',(14.4587607947443,0.73390803483815,26.8107518741751));
#44598=CARTESIAN_POINT('Ctrl Pts',(14.4905174012459,0.496053570864849,27.1232515215411));
#44599=CARTESIAN_POINT('Ctrl Pts',(14.5222740077474,0.137281974103891,27.2850326347925));
#44600=CARTESIAN_POINT('Ctrl Pts',(14.5540306142491,-0.254861359535286,
27.2547722853697));
#44601=CARTESIAN_POINT('Ctrl Pts',(14.5857872207506,-0.58507796496343,27.0411158406638));
#44602=CARTESIAN_POINT('Ctrl Pts',(14.6122101446308,-0.740884937302533,
26.7530976530099));
#44603=CARTESIAN_POINT('Ctrl Pts',(14.6280475330103,-0.764309608677931,
26.5630930749048));
#44604=CARTESIAN_POINT('Ctrl Pts',(14.6332993858894,-0.764344384160332,
26.5000700212582));
#44605=CARTESIAN_POINT('Ctrl Pts',(14.3667006141106,-0.76431852975353,26.4999818788456));
#44606=CARTESIAN_POINT('Ctrl Pts',(14.3700217138601,-0.764353313265897,
26.4601036057722));
#44607=CARTESIAN_POINT('Ctrl Pts',(14.3839520165078,-0.751491973744368,
26.292857013788));
#44608=CARTESIAN_POINT('Ctrl Pts',(14.4084915220538,-0.631298059665474,
26.0136275901214));
#44609=CARTESIAN_POINT('Ctrl Pts',(14.4403191307486,-0.3208755434976,25.7705246770357));
#44610=CARTESIAN_POINT('Ctrl Pts',(14.4721467394435,0.0680921626112602,
25.7059856307223));
#44611=CARTESIAN_POINT('Ctrl Pts',(14.5039743481383,0.440391998718261,25.8358085752634));
#44612=CARTESIAN_POINT('Ctrl Pts',(14.5358019568331,0.704890932298469,26.128214934684));
#44613=CARTESIAN_POINT('Ctrl Pts',(14.5676295655279,0.79684386389434,26.5116283189908));
#44614=CARTESIAN_POINT('Ctrl Pts',(14.5994571742227,0.693742189705464,26.8921952771914));
#44615=CARTESIAN_POINT('Ctrl Pts',(14.6312847829175,0.42082354702301,27.1767591177809));
#44616=CARTESIAN_POINT('Ctrl Pts',(14.6631123916124,0.0448940451386551,
27.2956631736732));
#44617=CARTESIAN_POINT('Ctrl Pts',(14.6949400003072,-0.342024799417935,
27.2198016378223));
#44618=CARTESIAN_POINT('Ctrl Pts',(14.726767609002,-0.645221455172022,26.967744198269));
#44619=CARTESIAN_POINT('Ctrl Pts',(14.7506878136031,-0.754389946559197,
26.6922588448303));
#44620=CARTESIAN_POINT('Ctrl Pts',(14.763998815306,-0.764372963801135,26.5324593527946));
#44621=CARTESIAN_POINT('Ctrl Pts',(14.7667006141106,-0.764340249515921,
26.5000200137165));
#44622=CARTESIAN_POINT('Origin',(8.83329938588935,0.,26.5));
#44623=CARTESIAN_POINT('',(13.8332993858894,-0.764305323848687,26.5000357755724));
#44624=CARTESIAN_POINT('',(13.9667006141106,-0.764393063012862,26.5000143835574));
#44625=CARTESIAN_POINT('',(8.83329938588935,-0.76435,26.5000000000004));
#44626=CARTESIAN_POINT('Ctrl Pts',(13.8332993858894,-0.764305323848606,
26.5000357755724));
#44627=CARTESIAN_POINT('Ctrl Pts',(13.8406613476642,-0.764560699159756,
26.4112555362681));
#44628=CARTESIAN_POINT('Ctrl Pts',(13.8691943804402,-0.706795172742057,
26.0666855489971));
#44629=CARTESIAN_POINT('Ctrl Pts',(13.9083129487166,-0.3125600582338,25.7173832361526));
#44630=CARTESIAN_POINT('Ctrl Pts',(13.9506550907188,0.21567771148749,25.7339181115233));
#44631=CARTESIAN_POINT('Ctrl Pts',(13.9824116972203,0.554871109700202,25.9280855750125));
#44632=CARTESIAN_POINT('Ctrl Pts',(14.0141683037219,0.761408101094941,26.2645314575356));
#44633=CARTESIAN_POINT('Ctrl Pts',(14.0459249102235,0.780984108470458,26.6567655146636));
#44634=CARTESIAN_POINT('Ctrl Pts',(14.0776815167251,0.610964975807012,27.0117073152108));
#44635=CARTESIAN_POINT('Ctrl Pts',(14.1094381232267,0.291647913206453,27.241334614104));
#44636=CARTESIAN_POINT('Ctrl Pts',(14.1411947297283,-0.0985343487612529,
27.2908309302356));
#44637=CARTESIAN_POINT('Ctrl Pts',(14.1729513362299,-0.464823397167573,
27.1468777424806));
#44638=CARTESIAN_POINT('Ctrl Pts',(14.2036528882836,-0.70934576818595,26.8564267856704));
#44639=CARTESIAN_POINT('Ctrl Pts',(14.2237689048368,-0.764317308692789,
26.6140248550565));
#44640=CARTESIAN_POINT('Ctrl Pts',(14.2332993858894,-0.764405081589217,
26.4996880256457));
#44641=CARTESIAN_POINT('Ctrl Pts',(13.9667006141106,-0.764393063012687,
26.5000143835574));
#44642=CARTESIAN_POINT('Ctrl Pts',(13.9760446124141,-0.764296506000937,
26.3878473518458));
#44643=CARTESIAN_POINT('Ctrl Pts',(13.9959978136159,-0.710931609772101,
26.1482367165881));
#44644=CARTESIAN_POINT('Ctrl Pts',(14.026560217716,-0.469843647084554,25.856305733657));
#44645=CARTESIAN_POINT('Ctrl Pts',(14.0583878264108,-0.10376507142601,25.7098556010573));
#44646=CARTESIAN_POINT('Ctrl Pts',(14.0902154351057,0.287713530534183,25.7568201526036));
#44647=CARTESIAN_POINT('Ctrl Pts',(14.1220430438004,0.608764471794302,25.9857032188419));
#44648=CARTESIAN_POINT('Ctrl Pts',(14.1538706524953,0.780799627852441,26.3404778937761));
#44649=CARTESIAN_POINT('Ctrl Pts',(14.1856982611901,0.761707549946172,26.734301023437));
#44650=CARTESIAN_POINT('Ctrl Pts',(14.2175258698849,0.556161672732346,27.0707710180205));
#44651=CARTESIAN_POINT('Ctrl Pts',(14.2493534785797,0.214476332390549,27.2675254159133));
#44652=CARTESIAN_POINT('Ctrl Pts',(14.2811810872745,-0.17970937641759,27.2764018941606));
#44653=CARTESIAN_POINT('Ctrl Pts',(14.3130086959694,-0.529905110324446,
27.0952276331628));
#44654=CARTESIAN_POINT('Ctrl Pts',(14.3415152049147,-0.727381888508666,
26.8024596028993));
#44655=CARTESIAN_POINT('Ctrl Pts',(14.3594125109618,-0.76424219786195,26.5874941457083));
#44656=CARTESIAN_POINT('Ctrl Pts',(14.3667006141106,-0.76431852975353,26.4999818788456));
#44657=CARTESIAN_POINT('Origin',(8.83329938588935,0.,26.5));
#44658=CARTESIAN_POINT('',(13.4332993858894,-0.763192368143962,26.5001425072106));
#44659=CARTESIAN_POINT('',(13.5667006141106,-0.764286670935071,26.4999939108431));
#44660=CARTESIAN_POINT('',(8.83329938588935,-0.76435,26.5000000000004));
#44661=CARTESIAN_POINT('Ctrl Pts',(13.4332993858894,-0.763192368143881,
26.5001425072106));
#44662=CARTESIAN_POINT('Ctrl Pts',(13.4469682549912,-0.762179560466138,
26.3361944380773));
#44663=CARTESIAN_POINT('Ctrl Pts',(13.4712226595935,-0.669971224498844,
26.0450308521942));
#44664=CARTESIAN_POINT('Ctrl Pts',(13.5060625996964,-0.328895476366436,
25.7752751551725));
#44665=CARTESIAN_POINT('Ctrl Pts',(13.537819206198,0.0555880103782207,25.7050924387132));
#44666=CARTESIAN_POINT('Ctrl Pts',(13.5695758126996,0.430357382868759,25.8291943247753));
#44667=CARTESIAN_POINT('Ctrl Pts',(13.6013324192012,0.698145424343159,26.1164578631495));
#44668=CARTESIAN_POINT('Ctrl Pts',(13.6330890257028,0.796941593703338,26.497416527793));
#44669=CARTESIAN_POINT('Ctrl Pts',(13.6648456322043,0.700818762673457,26.8787988611799));
#44670=CARTESIAN_POINT('Ctrl Pts',(13.696602238706,0.434409572344521,27.1681398817303));
#44671=CARTESIAN_POINT('Ctrl Pts',(13.7283588452075,0.0615766530934091,
27.2941787708476));
#44672=CARTESIAN_POINT('Ctrl Pts',(13.7601154517091,-0.325445621555236,
27.2275114283046));
#44673=CARTESIAN_POINT('Ctrl Pts',(13.7918720582108,-0.634571402982474,
26.9819618163357));
#44674=CARTESIAN_POINT('Ctrl Pts',(13.8162667029375,-0.751263355401409,
26.7053363730211));
#44675=CARTESIAN_POINT('Ctrl Pts',(13.8300758121637,-0.764193502955155,
26.5389098767338));
#44676=CARTESIAN_POINT('Ctrl Pts',(13.8332993858894,-0.764305323848606,
26.5000357755724));
#44677=CARTESIAN_POINT('Ctrl Pts',(13.5667006141106,-0.764286670934895,
26.4999939108431));
#44678=CARTESIAN_POINT('Ctrl Pts',(13.5714583080699,-0.764302511396769,
26.4428588396704));
#44679=CARTESIAN_POINT('Ctrl Pts',(13.5868252049275,-0.743884224407635,
26.2583291650472));
#44680=CARTESIAN_POINT('Ctrl Pts',(13.6128013046834,-0.59695074073402,25.9720367679793));
#44681=CARTESIAN_POINT('Ctrl Pts',(13.6446289133782,-0.270794296674234,
25.7504896197401));
#44682=CARTESIAN_POINT('Ctrl Pts',(13.676456522073,0.121648250824199,25.7124105991698));
#44683=CARTESIAN_POINT('Ctrl Pts',(13.7082841307678,0.484313256342262,25.86712084016));
#44684=CARTESIAN_POINT('Ctrl Pts',(13.7401117394627,0.728426139452693,26.176749755467));
#44685=CARTESIAN_POINT('Ctrl Pts',(13.7719393481575,0.794231979098091,26.5655051494659));
#44686=CARTESIAN_POINT('Ctrl Pts',(13.8037669568523,0.665622560492644,26.9382259328153));
#44687=CARTESIAN_POINT('Ctrl Pts',(13.8355945655471,0.374079407913512,27.2036760318525));
#44688=CARTESIAN_POINT('Ctrl Pts',(13.8674221742419,-0.00903238784518047,
27.2968775170617));
#44689=CARTESIAN_POINT('Ctrl Pts',(13.8992497829368,-0.389933199833693,
27.1950161587302));
#44690=CARTESIAN_POINT('Ctrl Pts',(13.9310773916315,-0.675384614490799,
26.9230259847075));
#44691=CARTESIAN_POINT('Ctrl Pts',(13.9535610020228,-0.760245312512092,
26.6577374861337));
#44692=CARTESIAN_POINT('Ctrl Pts',(13.9654354095158,-0.764406137113403,
26.5152021264581));
#44693=CARTESIAN_POINT('Ctrl Pts',(13.9667006141106,-0.764393063012687,
26.5000143835574));
#44694=CARTESIAN_POINT('Origin',(8.83329938588935,0.,26.5));
#44695=CARTESIAN_POINT('',(13.0332993858894,-0.765185328759249,26.5005140269729));
#44696=CARTESIAN_POINT('',(13.1667006141106,-0.76441561830137,26.4999977981034));
#44697=CARTESIAN_POINT('',(8.83329938588935,-0.76435,26.5000000000004));
#44698=CARTESIAN_POINT('Ctrl Pts',(13.0332993858894,-0.765185328759169,
26.5005140269729));
#44699=CARTESIAN_POINT('Ctrl Pts',(13.0426896268176,-0.765069612564117,
26.3877758463834));
#44700=CARTESIAN_POINT('Ctrl Pts',(13.0626654032463,-0.709228609067927,
26.1465610485235));
#44701=CARTESIAN_POINT('Ctrl Pts',(13.0932267151756,-0.469871753862732,
25.8564251459149));
#44702=CARTESIAN_POINT('Ctrl Pts',(13.1249833216772,-0.103350723706369,
25.7097428527291));
#44703=CARTESIAN_POINT('Ctrl Pts',(13.1567399281788,0.286546658439126,25.7567620725444));
#44704=CARTESIAN_POINT('Ctrl Pts',(13.1884965346804,0.607634532323689,25.9843423100245));
#44705=CARTESIAN_POINT('Ctrl Pts',(13.220253141182,0.779970642319146,26.3378848789699));
#44706=CARTESIAN_POINT('Ctrl Pts',(13.2520097476836,0.762787909334418,26.7308185076554));
#44707=CARTESIAN_POINT('Ctrl Pts',(13.2837663541852,0.558979957403396,27.0674971466822));
#44708=CARTESIAN_POINT('Ctrl Pts',(13.3155229606868,0.220111430206846,27.265988700436));
#44709=CARTESIAN_POINT('Ctrl Pts',(13.3472795671884,-0.17450318681229,27.2775067174508));
#44710=CARTESIAN_POINT('Ctrl Pts',(13.37903617369,-0.522757319830727,27.1001025909359));
#44711=CARTESIAN_POINT('Ctrl Pts',(13.4077094465903,-0.728082495975273,
26.8069728435505));
#44712=CARTESIAN_POINT('Ctrl Pts',(13.4257971839901,-0.763748250830808,
26.5901259218205));
#44713=CARTESIAN_POINT('Ctrl Pts',(13.4332993858894,-0.763192368143881,
26.5001425072106));
#44714=CARTESIAN_POINT('Ctrl Pts',(13.1667006141106,-0.764415618301195,
26.4999977981034));
#44715=CARTESIAN_POINT('Ctrl Pts',(13.1668720037257,-0.764415956632992,
26.4979405825976));
#44716=CARTESIAN_POINT('Ctrl Pts',(13.1776525962391,-0.76390455814698,26.3685396669369));
#44717=CARTESIAN_POINT('Ctrl Pts',(13.1990423916508,-0.696282751850487,
26.1123330157156));
#44718=CARTESIAN_POINT('Ctrl Pts',(13.2308700003456,-0.425223933001015,
25.8259970563627));
#44719=CARTESIAN_POINT('Ctrl Pts',(13.2626976090404,-0.0500771109931841,
25.7046462144535));
#44720=CARTESIAN_POINT('Ctrl Pts',(13.2945252177352,0.337327785132049,25.777985231033));
#44721=CARTESIAN_POINT('Ctrl Pts',(13.32635282643,0.64216024626656,26.0280618903463));
#44722=CARTESIAN_POINT('Ctrl Pts',(13.3581804351249,0.789802171887619,26.3936614345112));
#44723=CARTESIAN_POINT('Ctrl Pts',(13.3900080438197,0.744113185060425,26.7852909550754));
#44724=CARTESIAN_POINT('Ctrl Pts',(13.4218356525145,0.516277217440969,27.107085822582));
#44725=CARTESIAN_POINT('Ctrl Pts',(13.4536632612093,0.162064862066652,27.2802758113077));
#44726=CARTESIAN_POINT('Ctrl Pts',(13.4854908699041,-0.231818373908386,
27.2624667879633));
#44727=CARTESIAN_POINT('Ctrl Pts',(13.5173184785989,-0.568956187617919,
27.058018116014));
#44728=CARTESIAN_POINT('Ctrl Pts',(13.5443883933344,-0.737244927422413,
26.7679556994413));
#44729=CARTESIAN_POINT('Ctrl Pts',(13.5608491051716,-0.764267188680458,
26.5702645887285));
#44730=CARTESIAN_POINT('Ctrl Pts',(13.5667006141106,-0.764286670934895,
26.4999939108431));
#44731=CARTESIAN_POINT('Origin',(8.83329938588935,0.,26.5));
#44732=CARTESIAN_POINT('',(12.6332993858894,-0.764194707759887,26.4997132521735));
#44733=CARTESIAN_POINT('',(12.7667006141106,-0.764291254740594,26.5000096562347));
#44734=CARTESIAN_POINT('',(8.83329938588935,-0.76435,26.5000000000004));
#44735=CARTESIAN_POINT('Ctrl Pts',(12.6332993858894,-0.764194707759806,
26.4997132521735));
#44736=CARTESIAN_POINT('Ctrl Pts',(12.638410998644,-0.764263423596555,26.4385236355121));
#44737=CARTESIAN_POINT('Ctrl Pts',(12.6541081468992,-0.742061408822202,
26.2507674744643));
#44738=CARTESIAN_POINT('Ctrl Pts',(12.6803908306549,-0.588390470950266,
25.9624273215664));
#44739=CARTESIAN_POINT('Ctrl Pts',(12.7121474371564,-0.259988325015747,
25.7470606431281));
#44740=CARTESIAN_POINT('Ctrl Pts',(12.7439040436581,0.132189409199892,25.7140938108156));
#44741=CARTESIAN_POINT('Ctrl Pts',(12.7756606501597,0.491830546380316,25.8733116970985));
#44742=CARTESIAN_POINT('Ctrl Pts',(12.8074172566613,0.731965703418775,26.1848035737485));
#44743=CARTESIAN_POINT('Ctrl Pts',(12.8391738631629,0.793156876350488,26.5735783512257));
#44744=CARTESIAN_POINT('Ctrl Pts',(12.8709304696645,0.662016937073565,26.9437581615374));
#44745=CARTESIAN_POINT('Ctrl Pts',(12.902687076166,0.367739430229575,27.2069199172065));
#44746=CARTESIAN_POINT('Ctrl Pts',(12.9344436826677,-0.0128663201484088,
27.2957592556109));
#44747=CARTESIAN_POINT('Ctrl Pts',(12.9767858246698,-0.523694256138937,
27.1602477679971));
#44748=CARTESIAN_POINT('Ctrl Pts',(13.0097377257437,-0.757552044794858,
26.7831948742396));
#44749=CARTESIAN_POINT('Ctrl Pts',(13.0321040913171,-0.765200058406782,
26.5148645996986));
#44750=CARTESIAN_POINT('Ctrl Pts',(13.0332993858894,-0.765185328759169,
26.5005140269729));
#44751=CARTESIAN_POINT('Ctrl Pts',(12.7667006141106,-0.764291254740419,
26.5000096562347));
#44752=CARTESIAN_POINT('Ctrl Pts',(12.7728949022798,-0.764258309262706,
26.4256238242962));
#44753=CARTESIAN_POINT('Ctrl Pts',(12.7896983933472,-0.735010668826852,
26.2238090757755));
#44754=CARTESIAN_POINT('Ctrl Pts',(12.817111087313,-0.559868637292059,25.9328646808695));
#44755=CARTESIAN_POINT('Ctrl Pts',(12.8489386960078,-0.219472471696671,
25.7338882618077));
#44756=CARTESIAN_POINT('Ctrl Pts',(12.8807663047026,0.174647037187299,25.7224437167444));
#44757=CARTESIAN_POINT('Ctrl Pts',(12.9125939133974,0.526015750672588,25.9013324868735));
#44758=CARTESIAN_POINT('Ctrl Pts',(12.9444215220922,0.748624239560586,26.2267654685606));
#44759=CARTESIAN_POINT('Ctrl Pts',(12.976249130787,0.787981513819465,26.6190818840437));
#44760=CARTESIAN_POINT('Ctrl Pts',(13.0080767394819,0.634453543543031,26.9822489629997));
#44761=CARTESIAN_POINT('Ctrl Pts',(13.0399043481767,0.325621515054088,27.2273692254711));
#44762=CARTESIAN_POINT('Ctrl Pts',(13.0717319568715,-0.0629174411427496,
27.2944411600796));
#44763=CARTESIAN_POINT('Ctrl Pts',(13.1035595655663,-0.436055216210945,
27.1670466322858));
#44764=CARTESIAN_POINT('Ctrl Pts',(13.135215784646,-0.701019125182456,26.8779350566227));
#44765=CARTESIAN_POINT('Ctrl Pts',(13.1562628008274,-0.764395013528092,
26.6252844516571));
#44766=CARTESIAN_POINT('Ctrl Pts',(13.1667006141106,-0.764415618301195,
26.4999977981034));
#44767=CARTESIAN_POINT('Origin',(8.83329938588935,0.,26.5));
#44768=CARTESIAN_POINT('',(12.2332993858894,-0.76444205887302,26.49989355797));
#44769=CARTESIAN_POINT('',(12.3667006141106,-0.764381481730865,26.4999830130677));
#44770=CARTESIAN_POINT('',(8.83329938588935,-0.76435,26.5000000000004));
#44771=CARTESIAN_POINT('Ctrl Pts',(12.2332993858894,-0.764442058872939,
26.49989355797));
#44772=CARTESIAN_POINT('Ctrl Pts',(12.2341323704704,-0.764453514406101,
26.4898829023171));
#44773=CARTESIAN_POINT('Ctrl Pts',(12.245550890552,-0.76187866258566,26.3526836449442));
#44774=CARTESIAN_POINT('Ctrl Pts',(12.2675549461341,-0.684093539524432,
26.0919220252794));
#44775=CARTESIAN_POINT('Ctrl Pts',(12.2993115526357,-0.405504350759794,
25.8139323651287));
#44776=CARTESIAN_POINT('Ctrl Pts',(12.3310681591373,-0.0279149501101425,
25.7038490903687));
#44777=CARTESIAN_POINT('Ctrl Pts',(12.3628247656389,0.356457281532983,25.7872161726406));
#44778=CARTESIAN_POINT('Ctrl Pts',(12.3945813721405,0.653832357862692,26.0450111516939));
#44779=CARTESIAN_POINT('Ctrl Pts',(12.4263379786421,0.792175442841407,26.4125597423245));
#44780=CARTESIAN_POINT('Ctrl Pts',(12.4580945851437,0.736811757902941,26.8034410837456));
#44781=CARTESIAN_POINT('Ctrl Pts',(12.4898511916453,0.503083492378146,27.1166890097782));
#44782=CARTESIAN_POINT('Ctrl Pts',(12.5321933336474,0.0251849627174119,
27.3423470227353));
#44783=CARTESIAN_POINT('Ctrl Pts',(12.5745354756495,-0.516854899684397,
27.16561535569));
#44784=CARTESIAN_POINT('Ctrl Pts',(12.6117660048971,-0.739349580332478,
26.7576471542168));
#44785=CARTESIAN_POINT('Ctrl Pts',(12.6278254631435,-0.764121121359616,
26.5652399754475));
#44786=CARTESIAN_POINT('Ctrl Pts',(12.6332993858894,-0.764194707759806,
26.4997132521735));
#44787=CARTESIAN_POINT('Ctrl Pts',(12.3667006141106,-0.764381481730689,
26.4999830130677));
#44788=CARTESIAN_POINT('Ctrl Pts',(12.3683085979355,-0.764400131171695,
26.4806796412007));
#44789=CARTESIAN_POINT('Ctrl Pts',(12.3805257846588,-0.758957218875831,
26.334026408485));
#44790=CARTESIAN_POINT('Ctrl Pts',(12.4033521742804,-0.668463625002977,
26.0661201280579));
#44791=CARTESIAN_POINT('Ctrl Pts',(12.4351797829751,-0.378656158975322,
25.7987761594907));
#44792=CARTESIAN_POINT('Ctrl Pts',(12.46700739167,0.00384026553403038,25.7030805476152));
#44793=CARTESIAN_POINT('Ctrl Pts',(12.4988350003648,0.385396654593795,25.8024580443755));
#44794=CARTESIAN_POINT('Ctrl Pts',(12.5306626090596,0.672614119883514,26.0725826314222));
#44795=CARTESIAN_POINT('Ctrl Pts',(12.5624902177544,0.79518642952386,26.4473321394994));
#44796=CARTESIAN_POINT('Ctrl Pts',(12.5943178264493,0.723109846747402,26.8349738956479));
#44797=CARTESIAN_POINT('Ctrl Pts',(12.626145435144,0.474027563748743,27.1406194112225));
#44798=CARTESIAN_POINT('Ctrl Pts',(12.6579730438389,0.108910931026614,27.2894515630053));
#44799=CARTESIAN_POINT('Ctrl Pts',(12.6898006525337,-0.282865351947728,
27.2450386257746));
#44800=CARTESIAN_POINT('Ctrl Pts',(12.7216282612285,-0.605400730631636,
27.0182521746981));
#44801=CARTESIAN_POINT('Ctrl Pts',(12.7472615817541,-0.745813088274415,
26.7334325248592));
#44802=CARTESIAN_POINT('Ctrl Pts',(12.7622856993815,-0.764314736288392,
26.5530273874235));
#44803=CARTESIAN_POINT('Ctrl Pts',(12.7667006141106,-0.764291254740419,
26.5000096562347));
#44804=CARTESIAN_POINT('Origin',(8.83329938588935,0.,26.5));
#44805=CARTESIAN_POINT('',(11.8332993858894,-0.764247147692772,26.500050461596));
#44806=CARTESIAN_POINT('',(11.9667006141106,-0.764330172794767,26.5000194733099));
#44807=CARTESIAN_POINT('',(8.83329938588935,-0.76435,26.5000000000004));
#44808=CARTESIAN_POINT('Ctrl Pts',(11.8332993858894,-0.764247147692691,
26.500050461596));
#44809=CARTESIAN_POINT('Ctrl Pts',(11.8404392777974,-0.764200213145106,
26.4142992027336));
#44810=CARTESIAN_POINT('Ctrl Pts',(11.8581647052059,-0.728620187353754,
26.2013042703026));
#44811=CARTESIAN_POINT('Ctrl Pts',(11.8864756681149,-0.534515160588541,
25.9092978259331));
#44812=CARTESIAN_POINT('Ctrl Pts',(11.9182322746166,-0.186908610932021,
25.7252821486098));
#44813=CARTESIAN_POINT('Ctrl Pts',(11.9499888811181,0.206614996502733,25.7307004175932));
#44814=CARTESIAN_POINT('Ctrl Pts',(11.9817454876198,0.549294672995457,25.9225373664711));
#44815=CARTESIAN_POINT('Ctrl Pts',(12.0135020941213,0.758915838938966,26.2570703655453));
#44816=CARTESIAN_POINT('Ctrl Pts',(12.0452587006229,0.782128837256907,26.6472169046534));
#44817=CARTESIAN_POINT('Ctrl Pts',(12.0876008426251,0.562204459925782,27.1277809604453));
#44818=CARTESIAN_POINT('Ctrl Pts',(12.1299429846272,0.0338737476163272,
27.3420423732096));
#44819=CARTESIAN_POINT('Ctrl Pts',(12.1722851266293,-0.458655982287092,
27.15040988999));
#44820=CARTESIAN_POINT('Ctrl Pts',(12.2032087485499,-0.707058563347677,
26.862068242422));
#44821=CARTESIAN_POINT('Ctrl Pts',(12.2235468349699,-0.764307937938393,
26.617097923109));
#44822=CARTESIAN_POINT('Ctrl Pts',(12.2332993858894,-0.764442058872939,
26.49989355797));
#44823=CARTESIAN_POINT('Ctrl Pts',(11.9667006141106,-0.764330172794591,
26.5000194733099));
#44824=CARTESIAN_POINT('Ctrl Pts',(11.9743314964896,-0.7642422449594,26.4083952726879));
#44825=CARTESIAN_POINT('Ctrl Pts',(11.9925715817669,-0.724832682225659,
26.1893125034889));
#44826=CARTESIAN_POINT('Ctrl Pts',(12.0214208699425,-0.520221631970104,
25.8962907861735));
#44827=CARTESIAN_POINT('Ctrl Pts',(12.0532484786374,-0.167145187013454,
25.720796658319));
#44828=CARTESIAN_POINT('Ctrl Pts',(12.0850760873322,0.226845720661642,25.7360390191599));
#44829=CARTESIAN_POINT('Ctrl Pts',(12.116903696027,0.565308431882582,25.9382867830725));
#44830=CARTESIAN_POINT('Ctrl Pts',(12.1487313047218,0.76539269994308,26.2780329391498));
#44831=CARTESIAN_POINT('Ctrl Pts',(12.1805589134166,0.778121103043664,26.6721130739564));
#44832=CARTESIAN_POINT('Ctrl Pts',(12.2123865221114,0.600377932120684,27.0240626869479));
#44833=CARTESIAN_POINT('Ctrl Pts',(12.2442141308062,0.275671866485382,27.2477301540376));
#44834=CARTESIAN_POINT('Ctrl Pts',(12.2760417395011,-0.116514253498911,
27.2883652643034));
#44835=CARTESIAN_POINT('Ctrl Pts',(12.3078693481959,-0.480179551758527,
27.1360211940663));
#44836=CARTESIAN_POINT('Ctrl Pts',(12.3380889730657,-0.713869945077878,
26.8435516129409));
#44837=CARTESIAN_POINT('Ctrl Pts',(12.3576993950373,-0.764277085342196,
26.6080399949409));
#44838=CARTESIAN_POINT('Ctrl Pts',(12.3667006141106,-0.764381481730689,
26.4999830130677));
#44839=CARTESIAN_POINT('Origin',(8.83329938588935,0.,26.5));
#44840=CARTESIAN_POINT('',(11.4332993858894,-0.764316846204452,26.499991976129));
#44841=CARTESIAN_POINT('',(11.5667006141106,-0.76432783921912,26.4999807307349));
#44842=CARTESIAN_POINT('',(8.83329938588935,-0.76435,26.5000000000004));
#44843=CARTESIAN_POINT('Ctrl Pts',(11.4332993858894,-0.764316846204371,
26.499991976129));
#44844=CARTESIAN_POINT('Ctrl Pts',(11.4361606496238,-0.764339507108424,
26.4656360034336));
#44845=CARTESIAN_POINT('Ctrl Pts',(11.4496074488587,-0.753617458541854,
26.3041929838167));
#44846=CARTESIAN_POINT('Ctrl Pts',(11.4736397835942,-0.64225832786655,26.028166535323));
#44847=CARTESIAN_POINT('Ctrl Pts',(11.5053963900958,-0.337898373364977,
25.7786566049734));
#44848=CARTESIAN_POINT('Ctrl Pts',(11.5371529965974,0.0477483654022483,
25.704444958218));
#44849=CARTESIAN_POINT('Ctrl Pts',(11.568909603099,0.423642753883886,25.8250963957939));
#44850=CARTESIAN_POINT('Ctrl Pts',(11.6006662096006,0.692865902039955,26.1084196418678));
#44851=CARTESIAN_POINT('Ctrl Pts',(11.6430083516027,0.834479137823284,26.6175897852527));
#44852=CARTESIAN_POINT('Ctrl Pts',(11.6853504936048,0.568651082127304,27.1219475346471));
#44853=CARTESIAN_POINT('Ctrl Pts',(11.727692635607,0.0685686419494346,27.2929039515766));
#44854=CARTESIAN_POINT('Ctrl Pts',(11.7594492421086,-0.31732463510849,27.2309398975579));
#44855=CARTESIAN_POINT('Ctrl Pts',(11.7912058486102,-0.629310976686018,
26.9890351986573));
#44856=CARTESIAN_POINT('Ctrl Pts',(11.8158225632038,-0.750814573790938,
26.7099080364726));
#44857=CARTESIAN_POINT('Ctrl Pts',(11.8298537422968,-0.764269797856761,
26.5414331995225));
#44858=CARTESIAN_POINT('Ctrl Pts',(11.8332993858894,-0.764247147692691,
26.500050461596));
#44859=CARTESIAN_POINT('Ctrl Pts',(11.5667006141106,-0.764327839218945,
26.4999807307349));
#44860=CARTESIAN_POINT('Ctrl Pts',(11.5697451921454,-0.764362384129928,
26.4634240836987));
#44861=CARTESIAN_POINT('Ctrl Pts',(11.5833989730785,-0.752814048677305,
26.2995029900743));
#44862=CARTESIAN_POINT('Ctrl Pts',(11.6076619569099,-0.637582094773173,
26.0218949554196));
#44863=CARTESIAN_POINT('Ctrl Pts',(11.6394895656047,-0.330353663928771,
25.7747677489538));
#44864=CARTESIAN_POINT('Ctrl Pts',(11.6713171742995,0.0577400488194873,
25.7051657732641));
#44865=CARTESIAN_POINT('Ctrl Pts',(11.7031447829944,0.431699923094752,25.8301264763938));
#44866=CARTESIAN_POINT('Ctrl Pts',(11.7349723916892,0.69998657563618,26.1190614811315));
#44867=CARTESIAN_POINT('Ctrl Pts',(11.766800000384,0.796927734095428,26.5012441294702));
#44868=CARTESIAN_POINT('Ctrl Pts',(11.7986276090788,0.698793756689006,26.883122234856));
#44869=CARTESIAN_POINT('Ctrl Pts',(11.8304552177736,0.42960626815974,27.1712181579684));
#44870=CARTESIAN_POINT('Ctrl Pts',(11.8622828264684,0.055258051066885,27.2950106345332));
#44871=CARTESIAN_POINT('Ctrl Pts',(11.8941104351633,-0.332616451231466,
27.2241972504773));
#44872=CARTESIAN_POINT('Ctrl Pts',(11.9259380438581,-0.639071777563019,
26.9761119871953));
#44873=CARTESIAN_POINT('Ctrl Pts',(11.9501347701738,-0.753124084686165,
26.698904588869));
#44874=CARTESIAN_POINT('Ctrl Pts',(11.9637222935913,-0.764364490880332,
26.5357802442425));
#44875=CARTESIAN_POINT('Ctrl Pts',(11.9667006141106,-0.764330172794591,
26.5000194733099));
#44876=CARTESIAN_POINT('Origin',(8.83329938588935,0.,26.5));
#44877=CARTESIAN_POINT('',(11.0332993858894,-0.764414335147055,26.5000295538604));
#44878=CARTESIAN_POINT('',(11.1667006141106,-0.764383820028244,26.5000165411639));
#44879=CARTESIAN_POINT('',(8.83329938588935,-0.76435,26.5000000000004));
#44880=CARTESIAN_POINT('Ctrl Pts',(11.0332993858894,-0.764414335146974,
26.5000295538604));
#44881=CARTESIAN_POINT('Ctrl Pts',(11.0424675569507,-0.764269334783866,
26.3899624749499));
#44882=CARTESIAN_POINT('Ctrl Pts',(11.0622212635126,-0.712269135825712,
26.1526701198256));
#44883=CARTESIAN_POINT('Ctrl Pts',(11.092560505575,-0.476282880095,25.8609832951857));
#44884=CARTESIAN_POINT('Ctrl Pts',(11.1243171120767,-0.111125768016633,
25.7109378214796));
#44885=CARTESIAN_POINT('Ctrl Pts',(11.1560737185782,0.277329037821362,25.7540194775561));
#44886=CARTESIAN_POINT('Ctrl Pts',(11.1984158605804,0.713793524031026,26.0520250072723));
#44887=CARTESIAN_POINT('Ctrl Pts',(11.2407580025825,0.835647851523945,26.6089745718114));
#44888=CARTESIAN_POINT('Ctrl Pts',(11.2831001445846,0.563503958616806,27.0620156792366));
#44889=CARTESIAN_POINT('Ctrl Pts',(11.3148567510862,0.228530189829721,27.2633754058293));
#44890=CARTESIAN_POINT('Ctrl Pts',(11.3466133575878,-0.165922069656989,
27.2795239558244));
#44891=CARTESIAN_POINT('Ctrl Pts',(11.3783699640894,-0.517860513634208,
27.1052537424003));
#44892=CARTESIAN_POINT('Ctrl Pts',(11.4072653068566,-0.724305932574169,
26.8126503890575));
#44893=CARTESIAN_POINT('Ctrl Pts',(11.4255751141233,-0.764255670794614,
26.5927394103127));
#44894=CARTESIAN_POINT('Ctrl Pts',(11.4332993858894,-0.764316846204371,
26.499991976129));
#44895=CARTESIAN_POINT('Ctrl Pts',(11.1667006141106,-0.764383820028068,
26.5000165411639));
#44896=CARTESIAN_POINT('Ctrl Pts',(11.1757680906995,-0.764280459239413,
26.3911651193886));
#44897=CARTESIAN_POINT('Ctrl Pts',(11.1954447701866,-0.713308165354942,
26.1548607868991));
#44898=CARTESIAN_POINT('Ctrl Pts',(11.2257306525721,-0.478191357872257,
25.8624826382875));
#44899=CARTESIAN_POINT('Ctrl Pts',(11.2575582612669,-0.114052167341973,
25.7112747852685));
#44900=CARTESIAN_POINT('Ctrl Pts',(11.2893858699617,0.278005165684963,25.7531342228479));
#44901=CARTESIAN_POINT('Ctrl Pts',(11.3212134786565,0.6020112901178,25.977814431644));
#44902=CARTESIAN_POINT('Ctrl Pts',(11.3530410873514,0.778654699980662,26.3303172977978));
#44903=CARTESIAN_POINT('Ctrl Pts',(11.3848686960462,0.764695919842463,26.7243557697161));
#44904=CARTESIAN_POINT('Ctrl Pts',(11.416696304741,0.563551835344745,27.0634755452618));
#44905=CARTESIAN_POINT('Ctrl Pts',(11.4485239134358,0.224459294363696,27.2646655389139));
#44906=CARTESIAN_POINT('Ctrl Pts',(11.4803515221306,-0.169577284164262,
27.2786776649706));
#44907=CARTESIAN_POINT('Ctrl Pts',(11.5121791308255,-0.522104061573776,
27.1020819795649));
#44908=CARTESIAN_POINT('Ctrl Pts',(11.5409621614854,-0.725331388674681,
26.8090972724894));
#44909=CARTESIAN_POINT('Ctrl Pts',(11.5591359892471,-0.7642420081811,26.5908101717706));
#44910=CARTESIAN_POINT('Ctrl Pts',(11.5667006141106,-0.764327839218945,
26.4999807307349));
#44911=CARTESIAN_POINT('Origin',(8.83329938588935,0.,26.5));
#44912=CARTESIAN_POINT('',(10.6332993858894,-0.764353038715178,26.5000780441916));
#44913=CARTESIAN_POINT('',(10.7667006141106,-0.76429020563518,26.4999910099171));
#44914=CARTESIAN_POINT('',(8.83329938588935,-0.76435,26.5000000000004));
#44915=CARTESIAN_POINT('Ctrl Pts',(10.6332993858894,-0.764353038715098,
26.5000780441916));
#44916=CARTESIAN_POINT('Ctrl Pts',(10.6381889287772,-0.76439544040222,26.4414009892152));
#44917=CARTESIAN_POINT('Ctrl Pts',(10.6536640071655,-0.743302438196824,
26.2556450156638));
#44918=CARTESIAN_POINT('Ctrl Pts',(10.6797246210543,-0.593564624338813,
25.9683524714423));
#44919=CARTESIAN_POINT('Ctrl Pts',(10.7114812275559,-0.268803421489938,
25.7509051757754));
#44920=CARTESIAN_POINT('Ctrl Pts',(10.753823369558,0.25697906207964,25.6974138359586));
#44921=CARTESIAN_POINT('Ctrl Pts',(10.7961655115601,0.709133976254987,26.0446849521718));
#44922=CARTESIAN_POINT('Ctrl Pts',(10.8385076535623,0.793082515708411,26.5664714853321));
#44923=CARTESIAN_POINT('Ctrl Pts',(10.8702642600639,0.666769034948869,26.9363337162334));
#44924=CARTESIAN_POINT('Ctrl Pts',(10.9020208665655,0.375600348367009,27.2029310842536));
#44925=CARTESIAN_POINT('Ctrl Pts',(10.9337774730671,-0.00580221503551052,
27.2965412346965));
#44926=CARTESIAN_POINT('Ctrl Pts',(10.9655340795687,-0.386547155848502,
27.1969245830134));
#44927=CARTESIAN_POINT('Ctrl Pts',(10.9972906860703,-0.672567178598631,
26.9269530484939));
#44928=CARTESIAN_POINT('Ctrl Pts',(11.0198791215105,-0.759771192940516,
26.6611311283238));
#44929=CARTESIAN_POINT('Ctrl Pts',(11.0318820214502,-0.764436751652618,
26.517045506391));
#44930=CARTESIAN_POINT('Ctrl Pts',(11.0332993858894,-0.764414335146974,
26.5000295538604));
#44931=CARTESIAN_POINT('Ctrl Pts',(10.7667006141106,-0.764290205635005,
26.4999910099171));
#44932=CARTESIAN_POINT('Ctrl Pts',(10.7711817863553,-0.764312357801265,
26.4461773955807));
#44933=CARTESIAN_POINT('Ctrl Pts',(10.7862721614982,-0.745445842461897,
26.2649750263996));
#44934=CARTESIAN_POINT('Ctrl Pts',(10.8119717395395,-0.603779637374724,
25.9798601046639));
#44935=CARTESIAN_POINT('Ctrl Pts',(10.8437993482343,-0.280537733984753,
25.7540818134411));
#44936=CARTESIAN_POINT('Ctrl Pts',(10.8756269569291,0.111375310126204,25.7108923384462));
#44937=CARTESIAN_POINT('Ctrl Pts',(10.9074545656239,0.476025463481309,25.8608637709017));
#44938=CARTESIAN_POINT('Ctrl Pts',(10.9392821743187,0.724152213281463,26.1672855079379));
#44939=CARTESIAN_POINT('Ctrl Pts',(10.9711097830136,0.795018108239294,26.5551504197647));
#44940=CARTESIAN_POINT('Ctrl Pts',(11.0029373917084,0.671276313132874,26.9295153928038));
#44941=CARTESIAN_POINT('Ctrl Pts',(11.0347650004032,0.383216836026789,27.1987418821097));
#44942=CARTESIAN_POINT('Ctrl Pts',(11.066592609098,0.00135201979696231,
27.2969275583584));
#44943=CARTESIAN_POINT('Ctrl Pts',(11.0984202177928,-0.380843749208507,
27.2000381417591));
#44944=CARTESIAN_POINT('Ctrl Pts',(11.1302478264876,-0.669815072706669,
26.9317906085171));
#44945=CARTESIAN_POINT('Ctrl Pts',(11.1530079585936,-0.759211496005515,
26.6643815455522));
#44946=CARTESIAN_POINT('Ctrl Pts',(11.1651588878012,-0.7644013942722,26.5185243475109));
#44947=CARTESIAN_POINT('Ctrl Pts',(11.1667006141106,-0.764383820028068,
26.5000165411639));
#44948=CARTESIAN_POINT('Origin',(8.83329938588935,0.,26.5));
#44949=CARTESIAN_POINT('',(10.2332993858894,-0.764421590778621,26.4997053810623));
#44950=CARTESIAN_POINT('',(10.3667006141106,-0.764415943136787,26.5000013527853));
#44951=CARTESIAN_POINT('',(8.83329938588935,-0.76435,26.5000000000004));
#44952=CARTESIAN_POINT('Ctrl Pts',(10.2332993858894,-0.764421590778541,
26.4997053810623));
#44953=CARTESIAN_POINT('Ctrl Pts',(10.2339103006036,-0.764425134242162,
26.4923794589594));
#44954=CARTESIAN_POINT('Ctrl Pts',(10.2451067508183,-0.762525940900646,
26.3581546174279));
#44955=CARTESIAN_POINT('Ctrl Pts',(10.2668887365335,-0.688355039348421,
26.1005432767371));
#44956=CARTESIAN_POINT('Ctrl Pts',(10.3092308785357,-0.320848092753299,
25.720744399325));
#44957=CARTESIAN_POINT('Ctrl Pts',(10.3515730205378,0.24868545684196,25.6948054070466));
#44958=CARTESIAN_POINT('Ctrl Pts',(10.3939151625399,0.649194652036547,26.0396255450656));
#44959=CARTESIAN_POINT('Ctrl Pts',(10.4256717690415,0.791023092992396,26.403820353824));
#44960=CARTESIAN_POINT('Ctrl Pts',(10.4574283755431,0.740250732337037,26.7953245403195));
#44961=CARTESIAN_POINT('Ctrl Pts',(10.4891849820447,0.508988374911209,27.1127335787333));
#44962=CARTESIAN_POINT('Ctrl Pts',(10.5209415885463,0.153681120282412,27.2819876542253));
#44963=CARTESIAN_POINT('Ctrl Pts',(10.5526981950479,-0.239009618237098,
27.2599407330431));
#44964=CARTESIAN_POINT('Ctrl Pts',(10.5844548015495,-0.573625316704213,
27.0532418767055));
#44965=CARTESIAN_POINT('Ctrl Pts',(10.6113218651633,-0.738145513096974,
26.7637621146551));
#44966=CARTESIAN_POINT('Ctrl Pts',(10.6276033932766,-0.764303643566683,
26.5684329148525));
#44967=CARTESIAN_POINT('Ctrl Pts',(10.6332993858894,-0.764353038715098,
26.5000780441916));
#44968=CARTESIAN_POINT('Ctrl Pts',(10.3667006141106,-0.764415943136612,
26.5000013527853));
#44969=CARTESIAN_POINT('Ctrl Pts',(10.3772046849093,-0.764402983620275,
26.3739195564708));
#44970=CARTESIAN_POINT('Ctrl Pts',(10.3983179586064,-0.700392143844539,
26.1204813744118));
#44971=CARTESIAN_POINT('Ctrl Pts',(10.4300404352017,-0.433970366467297,
25.8315951210098));
#44972=CARTESIAN_POINT('Ctrl Pts',(10.4618680438965,-0.0604366454286784,
25.7053662648007));
#44973=CARTESIAN_POINT('Ctrl Pts',(10.4936956525913,0.327890997713297,25.7736510102933));
#44974=CARTESIAN_POINT('Ctrl Pts',(10.5255232612861,0.635956180167181,26.0197343462881));
#44975=CARTESIAN_POINT('Ctrl Pts',(10.5573508699809,0.78834948304845,26.3833790164421));
#44976=CARTESIAN_POINT('Ctrl Pts',(10.5891784786757,0.747767468424727,26.775570634129));
#44977=CARTESIAN_POINT('Ctrl Pts',(10.6210060873706,0.524143963013505,27.1003069775249));
#44978=CARTESIAN_POINT('Ctrl Pts',(10.6528336960654,0.172218416622154,27.2780977947564));
#44979=CARTESIAN_POINT('Ctrl Pts',(10.6846613047602,-0.221863437780272,
27.2654227434594));
#44980=CARTESIAN_POINT('Ctrl Pts',(10.716488913455,-0.561636678720128,27.0653844730313));
#44981=CARTESIAN_POINT('Ctrl Pts',(10.7438353499051,-0.735448311725334,
26.7745991910558));
#44982=CARTESIAN_POINT('Ctrl Pts',(10.760572583457,-0.764259912411162,26.5735814590732));
#44983=CARTESIAN_POINT('Ctrl Pts',(10.7667006141106,-0.764290205635005,
26.4999910099171));
#44984=CARTESIAN_POINT('Origin',(8.83329938588935,0.,26.5));
#44985=CARTESIAN_POINT('',(9.83329938588937,-0.764354837691132,26.4999637734947));
#44986=CARTESIAN_POINT('',(9.96670061411062,-0.764287395473983,26.5000068045578));
#44987=CARTESIAN_POINT('',(8.83329938588935,-0.76435,26.5000000000004));
#44988=CARTESIAN_POINT('Ctrl Pts',(9.83329938588939,-0.764354837691052,
26.4999637734947));
#44989=CARTESIAN_POINT('Ctrl Pts',(9.84021720793052,-0.764621482654753,
26.4165337381156));
#44990=CARTESIAN_POINT('Ctrl Pts',(9.86830610097272,-0.711315275771919,
26.0775144141055));
#44991=CARTESIAN_POINT('Ctrl Pts',(9.90698052951547,-0.328871142664085,
25.7240954537507));
#44992=CARTESIAN_POINT('Ctrl Pts',(9.94932267151757,0.199598255234956,25.7295723838951));
#44993=CARTESIAN_POINT('Ctrl Pts',(9.98107927801918,0.542780303630156,25.9165983405945));
#44994=CARTESIAN_POINT('Ctrl Pts',(10.0128358845208,0.756313557236772,26.2486482930385));
#44995=CARTESIAN_POINT('Ctrl Pts',(10.0445924910224,0.784093796915711,26.6403866625412));
#44996=CARTESIAN_POINT('Ctrl Pts',(10.076349097524,0.621540241153639,26.9988089464404));
#44997=CARTESIAN_POINT('Ctrl Pts',(10.1081057040256,0.307098718342552,27.235068614701));
#44998=CARTESIAN_POINT('Ctrl Pts',(10.1398623105272,-0.0819621986926931,
27.2927198636753));
#44999=CARTESIAN_POINT('Ctrl Pts',(10.1716189170288,-0.451183699623203,
27.1564639171439));
#45000=CARTESIAN_POINT('Ctrl Pts',(10.2027646088162,-0.70535559423304,26.8670671390887));
#45001=CARTESIAN_POINT('Ctrl Pts',(10.223324765103,-0.764363735393704,26.619318304422));
#45002=CARTESIAN_POINT('Ctrl Pts',(10.2332993858894,-0.764421590778541,
26.4997053810623));
#45003=CARTESIAN_POINT('Ctrl Pts',(9.96670061411058,-0.764287395473808,
26.5000068045578));
#45004=CARTESIAN_POINT('Ctrl Pts',(9.97261838056512,-0.764265365977669,
26.4289406306763));
#45005=CARTESIAN_POINT('Ctrl Pts',(9.98914534991794,-0.736818813278755,
26.2304523735062));
#45006=CARTESIAN_POINT('Ctrl Pts',(10.016281522169,-0.567211114828819,25.9402081539091));
#45007=CARTESIAN_POINT('Ctrl Pts',(10.0481091308639,-0.229436586427856,
25.7368131175217));
#45008=CARTESIAN_POINT('Ctrl Pts',(10.0799367395587,0.164500331356799,25.7202340098908));
#45009=CARTESIAN_POINT('Ctrl Pts',(10.1117643482535,0.518170209717155,25.8945291116224));
#45010=CARTESIAN_POINT('Ctrl Pts',(10.1435919569483,0.745000323495275,26.2170337856481));
#45011=CARTESIAN_POINT('Ctrl Pts',(10.1754195656431,0.789466300620247,26.608804051599));
#45012=CARTESIAN_POINT('Ctrl Pts',(10.207247174338,0.640683580453765,26.9739408306562));
#45013=CARTESIAN_POINT('Ctrl Pts',(10.2390747830327,0.335071789291362,27.2230644903377));
#45014=CARTESIAN_POINT('Ctrl Pts',(10.2709023917276,-0.0525602054491083,
27.2951935525961));
#45015=CARTESIAN_POINT('Ctrl Pts',(10.3027300004224,-0.427326304238472,
27.1726719786772));
#45016=CARTESIAN_POINT('Ctrl Pts',(10.3345576091172,-0.697489773146787,
26.8854910862812));
#45017=CARTESIAN_POINT('Ctrl Pts',(10.3558811470133,-0.764104306192731,
26.629868829569));
#45018=CARTESIAN_POINT('Ctrl Pts',(10.3665954820111,-0.764416072844531,
26.5012632677334));
#45019=CARTESIAN_POINT('Ctrl Pts',(10.3667006141106,-0.764415943136612,
26.5000013527853));
#45020=CARTESIAN_POINT('Origin',(26.4823223304703,0.,26.5));
#45021=CARTESIAN_POINT('',(26.5,0.85,26.5));
#45022=CARTESIAN_POINT('Origin',(26.5,0.,26.5));
#45023=CARTESIAN_POINT('',(26.4646446609407,0.935355339059328,26.5));
#45024=CARTESIAN_POINT('',(26.4823223304703,0.892677669529664,26.5));
#45025=CARTESIAN_POINT('',(26.4646446609407,-0.935355339059328,26.5));
#45026=CARTESIAN_POINT('Origin',(26.4646446609407,0.,26.5));
#45027=CARTESIAN_POINT('Origin',(26.4646446609407,0.,26.5));
#45028=CARTESIAN_POINT('Origin',(26.45,0.,26.5));
#45029=CARTESIAN_POINT('',(26.4428553390593,-0.957144660940674,26.5));
#45030=CARTESIAN_POINT('',(26.45,-0.95,26.5));
#45031=CARTESIAN_POINT('',(26.4428553390593,-0.887111235409736,26.1407706464662));
#45032=CARTESIAN_POINT('Origin',(26.4428553390593,0.,26.5));
#45033=CARTESIAN_POINT('',(26.4428553390593,0.547713856063688,27.2849429494193));
#45034=CARTESIAN_POINT('Origin',(26.4428553390593,0.,26.5));
#45035=CARTESIAN_POINT('Origin',(26.4428553390593,0.,26.5));
#45036=CARTESIAN_POINT('Origin',(26.5,0.,26.5));
#45037=CARTESIAN_POINT('Origin',(1.375,0.,26.5));
#45038=CARTESIAN_POINT('',(1.35,-5.57214293612048E-17,26.045));
#45039=CARTESIAN_POINT('Origin',(1.35,0.,26.5));
#45040=CARTESIAN_POINT('',(1.4,4.95981953654679E-17,26.095));
#45041=CARTESIAN_POINT('',(1.375,-5.26598123633364E-17,26.07));
#45042=CARTESIAN_POINT('Origin',(1.4,0.,26.5));
#45043=CARTESIAN_POINT('Origin',(2.16,0.,26.5));
#45044=CARTESIAN_POINT('',(3.,-4.95981953654679E-17,26.095));
#45045=CARTESIAN_POINT('Origin',(3.,0.,26.5));
#45046=CARTESIAN_POINT('',(2.16,-4.95981953654679E-17,26.095));
#45047=CARTESIAN_POINT('Origin',(1.35,0.95,26.5));
#45048=CARTESIAN_POINT('',(1.35,-0.95,26.5));
#45049=CARTESIAN_POINT('Origin',(1.35,0.,26.5));
#45050=CARTESIAN_POINT('Origin',(26.4001776695297,0.,26.5));
#45051=CARTESIAN_POINT('',(26.3575,-0.445914884024654,27.3865897013136));
#45052=CARTESIAN_POINT('Ctrl Pts',(26.3575,-0.445914873067339,27.3865896766146));
#45053=CARTESIAN_POINT('Ctrl Pts',(26.3600385435018,-0.48473316469248,27.3658905669609));
#45054=CARTESIAN_POINT('Ctrl Pts',(26.3625749249413,-0.52209630504398,27.3426935917771));
#45055=CARTESIAN_POINT('Ctrl Pts',(26.3651148458502,-0.557748585913535,
27.3171415526578));
#45056=CARTESIAN_POINT('Ctrl Pts',(26.3672683153527,-0.587976337997584,
27.2954772808384));
#45057=CARTESIAN_POINT('Ctrl Pts',(26.3694243291957,-0.61697427499121,27.2721190586853));
#45058=CARTESIAN_POINT('Ctrl Pts',(26.3715863623179,-0.644568450298925,
27.2471307664931));
#45059=CARTESIAN_POINT('Ctrl Pts',(26.3723323070778,-0.654088993838404,
27.2385093048571));
#45060=CARTESIAN_POINT('Ctrl Pts',(26.3730789683657,-0.663442253748417,
27.2296936320192));
#45061=CARTESIAN_POINT('Ctrl Pts',(26.3738264888999,-0.672623694624938,
27.2206895691609));
#45062=CARTESIAN_POINT('Ctrl Pts',(26.3744393486039,-0.680151160265756,
27.2133075280732));
#45063=CARTESIAN_POINT('Ctrl Pts',(26.3750523299018,-0.687557476799255,
27.2058043027306));
#45064=CARTESIAN_POINT('Ctrl Pts',(26.3756651421252,-0.694836304461934,
27.1981882490307));
#45065=CARTESIAN_POINT('Ctrl Pts',(26.3782136366893,-0.725106674441304,
27.1665154613291));
#45066=CARTESIAN_POINT('Ctrl Pts',(26.3807612316211,-0.753200182626468,
27.1328697487299));
#45067=CARTESIAN_POINT('Ctrl Pts',(26.3833137014739,-0.778965752445576,
27.0975076461287));
#45068=CARTESIAN_POINT('Ctrl Pts',(26.3847185728135,-0.793147040638668,
27.0780444566234));
#45069=CARTESIAN_POINT('Ctrl Pts',(26.3861249209455,-0.806622431718545,
27.0580606680849));
#45070=CARTESIAN_POINT('Ctrl Pts',(26.3875337086924,-0.819361091867474,
27.037595384434));
#45071=CARTESIAN_POINT('Ctrl Pts',(26.3882388148024,-0.825736862188447,
27.0273523960361));
#45072=CARTESIAN_POINT('Ctrl Pts',(26.3889445320502,-0.831928009592696,
27.016988757215));
#45073=CARTESIAN_POINT('Ctrl Pts',(26.389650981154,-0.837930241239925,27.0065092037505));
#45074=CARTESIAN_POINT('Ctrl Pts',(26.3903079381786,-0.843511971364541,
26.9967638219154));
#45075=CARTESIAN_POINT('Ctrl Pts',(26.3909656943287,-0.848931490642638,
26.9869156056837));
#45076=CARTESIAN_POINT('Ctrl Pts',(26.3916229242783,-0.854174248581219,
26.9769900217494));
#45077=CARTESIAN_POINT('Ctrl Pts',(26.3941734457713,-0.874519892922855,
26.9384716688187));
#45078=CARTESIAN_POINT('Ctrl Pts',(26.3967204402416,-0.892245792594232,
26.8987257442745));
#45079=CARTESIAN_POINT('Ctrl Pts',(26.3992697018428,-0.907198345124913,
26.8579958866988));
#45080=CARTESIAN_POINT('Ctrl Pts',(26.3995912211097,-0.909084198552438,
26.8528589349072));
#45081=CARTESIAN_POINT('Ctrl Pts',(26.3999127764396,-0.910925876275156,
26.8477063004776));
#45082=CARTESIAN_POINT('Ctrl Pts',(26.4002343794568,-0.91272301636638,26.8425384475368));
#45083=CARTESIAN_POINT('Ctrl Pts',(26.4026046454671,-0.925968228151,26.8044505394169));
#45084=CARTESIAN_POINT('Ctrl Pts',(26.404977501818,-0.936797324660802,26.7655365317526));
#45085=CARTESIAN_POINT('Ctrl Pts',(26.4073576022132,-0.945188176582006,
26.7260336212008));
#45086=CARTESIAN_POINT('Ctrl Pts',(26.4085446489769,-0.949373014178511,
26.7063320144032));
#45087=CARTESIAN_POINT('Ctrl Pts',(26.409733497622,-0.95295076699331,26.6864838163494));
#45088=CARTESIAN_POINT('Ctrl Pts',(26.4109247254682,-0.9559150864139,26.6665183261861));
#45089=CARTESIAN_POINT('Ctrl Pts',(26.4115344172028,-0.957432278154629,
26.6562996309385));
#45090=CARTESIAN_POINT('Ctrl Pts',(26.4121447321872,-0.958788737392734,
26.6460502130111));
#45091=CARTESIAN_POINT('Ctrl Pts',(26.4127557478252,-0.959983365913965,
26.6357740370122));
#45092=CARTESIAN_POINT('Ctrl Pts',(26.4132604827156,-0.960970199405942,
26.6272853106299));
#45093=CARTESIAN_POINT('Ctrl Pts',(26.4137651979061,-0.961845594431708,
26.6187866986054));
#45094=CARTESIAN_POINT('Ctrl Pts',(26.4142697129421,-0.962609265207646,
26.610284282333));
#45095=CARTESIAN_POINT('Ctrl Pts',(26.4168249481992,-0.966477055763842,
26.5672217920562));
#45096=CARTESIAN_POINT('Ctrl Pts',(26.4193769127223,-0.967486752456094,
26.5240309369813));
#45097=CARTESIAN_POINT('Ctrl Pts',(26.4219314366751,-0.965628032162785,
26.4810033974626));
#45098=CARTESIAN_POINT('Ctrl Pts',(26.4242448807101,-0.963944726210391,
26.4420365267346));
#45099=CARTESIAN_POINT('Ctrl Pts',(26.4265604238843,-0.959908265275576,
26.4032027997282));
#45100=CARTESIAN_POINT('Ctrl Pts',(26.4288823965957,-0.953474131147185,
26.3647208517404));
#45101=CARTESIAN_POINT('Ctrl Pts',(26.4300930314562,-0.950119489193485,
26.3446570553377));
#45102=CARTESIAN_POINT('Ctrl Pts',(26.4313054141171,-0.946112458815371,
26.3246889932157));
#45103=CARTESIAN_POINT('Ctrl Pts',(26.4325201583348,-0.941463409934123,
26.3048454980279));
#45104=CARTESIAN_POINT('Ctrl Pts',(26.4332726276574,-0.938583571848533,
26.2925535099993));
#45105=CARTESIAN_POINT('Ctrl Pts',(26.434026003143,-0.935457335204475,26.2803093396821));
#45106=CARTESIAN_POINT('Ctrl Pts',(26.4347804306756,-0.93208672886211,26.2681200827888));
#45107=CARTESIAN_POINT('Ctrl Pts',(26.4352708940567,-0.929895452813088,
26.2601956846323));
#45108=CARTESIAN_POINT('Ctrl Pts',(26.4357617442608,-0.927601043197031,
26.2522954678643));
#45109=CARTESIAN_POINT('Ctrl Pts',(26.4362522637174,-0.925208062189623,
26.2444334515549));
#45110=CARTESIAN_POINT('Ctrl Pts',(26.4384546480274,-0.914463811876937,
26.2091337684695));
#45111=CARTESIAN_POINT('Ctrl Pts',(26.4406544289207,-0.901716958129345,
26.1745378725213));
#45112=CARTESIAN_POINT('Ctrl Pts',(26.4428553390593,-0.88706152092118,26.1408063078486));
#45113=CARTESIAN_POINT('',(26.3575,0.966230510866419,26.2733743026085));
#45114=CARTESIAN_POINT('Ctrl Pts',(26.4428553390593,0.547713856063654,27.2849429494193));
#45115=CARTESIAN_POINT('Ctrl Pts',(26.4398527288292,0.581338330917549,27.2629971879954));
#45116=CARTESIAN_POINT('Ctrl Pts',(26.436860740363,0.613498955065304,27.2389352067906));
#45117=CARTESIAN_POINT('Ctrl Pts',(26.43387340856,0.64405462111651,27.2129570307588));
#45118=CARTESIAN_POINT('Ctrl Pts',(26.4325435063468,0.657657411361345,27.201392050342));
#45119=CARTESIAN_POINT('Ctrl Pts',(26.431214527018,0.670941868034084,27.1894468235091));
#45120=CARTESIAN_POINT('Ctrl Pts',(26.429885944282,0.683894109675807,27.17713688103));
#45121=CARTESIAN_POINT('Ctrl Pts',(26.4286990874112,0.695464677746311,27.1661400951964));
#45122=CARTESIAN_POINT('Ctrl Pts',(26.4275121669376,0.706773475320743,27.1548483470153));
#45123=CARTESIAN_POINT('Ctrl Pts',(26.4263270971742,0.717789124043923,27.1432948309583));
#45124=CARTESIAN_POINT('Ctrl Pts',(26.4231131118946,0.747664270584715,27.1119609536771));
#45125=CARTESIAN_POINT('Ctrl Pts',(26.4199099302131,0.775414440024102,27.0786797677372));
#45126=CARTESIAN_POINT('Ctrl Pts',(26.4167102083011,0.800845389198238,27.0436744066156));
#45127=CARTESIAN_POINT('Ctrl Pts',(26.4158576282968,0.807621577677036,27.03434707388));
#45128=CARTESIAN_POINT('Ctrl Pts',(26.4150052939291,0.814232902380581,27.0248971262858));
#45129=CARTESIAN_POINT('Ctrl Pts',(26.4141530662695,0.820675210986602,27.0153283782149));
#45130=CARTESIAN_POINT('Ctrl Pts',(26.4134180785672,0.826231258770111,27.0070759915688));
#45131=CARTESIAN_POINT('Ctrl Pts',(26.4126831307285,0.831661755957179,26.9987347062046));
#45132=CARTESIAN_POINT('Ctrl Pts',(26.4119492862705,0.83695594675194,26.9903203427592));
#45133=CARTESIAN_POINT('Ctrl Pts',(26.4103406081986,0.848561469622691,26.9718750144373));
#45134=CARTESIAN_POINT('Ctrl Pts',(26.4087359032515,0.859522353428771,26.9530638762961));
#45135=CARTESIAN_POINT('Ctrl Pts',(26.4071342608444,0.869816503695763,26.9339165277584));
#45136=CARTESIAN_POINT('Ctrl Pts',(26.4039408162305,0.890341558838379,26.8957394685182));
#45137=CARTESIAN_POINT('Ctrl Pts',(26.4007595466296,0.908219032919032,26.8562276023525));
#45138=CARTESIAN_POINT('Ctrl Pts',(26.397583234291,0.923418683717435,26.8156799699147));
#45139=CARTESIAN_POINT('Ctrl Pts',(26.3953941841655,0.933893975168751,26.7877353629575));
#45140=CARTESIAN_POINT('Ctrl Pts',(26.3932074885846,0.943096493319833,26.7592980148124));
#45141=CARTESIAN_POINT('Ctrl Pts',(26.3910207848981,0.951003299464193,26.7304596282699));
#45142=CARTESIAN_POINT('Ctrl Pts',(26.3898435664395,0.955259952160194,26.7149343967689));
#45143=CARTESIAN_POINT('Ctrl Pts',(26.3886663456316,0.959140888050434,26.6992928697601));
#45144=CARTESIAN_POINT('Ctrl Pts',(26.3874887538361,0.962641160833331,26.6835490619002));
#45145=CARTESIAN_POINT('Ctrl Pts',(26.3868658035192,0.964492817789051,26.6752205306281));
#45146=CARTESIAN_POINT('Ctrl Pts',(26.3862427493833,0.966237931701423,26.6668633743709));
#45147=CARTESIAN_POINT('Ctrl Pts',(26.3856195368556,0.967875657393992,26.6584796596185));
#45148=CARTESIAN_POINT('Ctrl Pts',(26.3849599332623,0.969609014320487,26.6496063970802));
#45149=CARTESIAN_POINT('Ctrl Pts',(26.3843007260322,0.97122051053719,26.640711093987));
#45150=CARTESIAN_POINT('Ctrl Pts',(26.3836423162498,0.97270880060374,26.631802662497));
#45151=CARTESIAN_POINT('Ctrl Pts',(26.3804362994795,0.979955781192868,26.5884245391464));
#45152=CARTESIAN_POINT('Ctrl Pts',(26.3772457209939,0.984294585326509,26.5446899966097));
#45153=CARTESIAN_POINT('Ctrl Pts',(26.3740633661155,0.985682557969509,26.5008948307824));
#45154=CARTESIAN_POINT('Ctrl Pts',(26.3731793337966,0.98606812548825,26.488728889684));
#45155=CARTESIAN_POINT('Ctrl Pts',(26.3722959360797,0.986225688641236,26.4765581716034));
#45156=CARTESIAN_POINT('Ctrl Pts',(26.3714130183056,0.986153641580633,26.4643888432541));
#45157=CARTESIAN_POINT('Ctrl Pts',(26.3682371159129,0.985894484455392,26.4206151191807));
#45158=CARTESIAN_POINT('Ctrl Pts',(26.3650674234017,0.982668492420396,26.3768591088312));
#45159=CARTESIAN_POINT('Ctrl Pts',(26.3618967427,0.976554405390113,26.3334004690451));
#45160=CARTESIAN_POINT('Ctrl Pts',(26.360431609542,0.973729159809769,26.3133187578467));
#45161=CARTESIAN_POINT('Ctrl Pts',(26.3589662653804,0.970286500015859,26.2933005906444));
#45162=CARTESIAN_POINT('Ctrl Pts',(26.3575,0.96623051086643,26.2733743026086));
#45163=CARTESIAN_POINT('Origin',(26.3575,0.,26.5));
#45164=CARTESIAN_POINT('Ctrl Pts',(9.53886739174684,0.859794713971473,26.0042084108955));
#45165=CARTESIAN_POINT('Ctrl Pts',(9.54945292724737,0.942233552586438,26.1471726709289));
#45166=CARTESIAN_POINT('Ctrl Pts',(9.57062399824843,1.0343832675773,26.4749075185653));
#45167=CARTESIAN_POINT('Ctrl Pts',(9.60238060475003,0.920175290048848,26.97275433311));
#45168=CARTESIAN_POINT('Ctrl Pts',(9.63413721125163,0.582068997229128,27.3555560520742));
#45169=CARTESIAN_POINT('Ctrl Pts',(9.66589381775322,0.101541985274178,27.5293442666035));
#45170=CARTESIAN_POINT('Ctrl Pts',(9.69765042425481,-0.402736095057523,
27.4532967233332));
#45171=CARTESIAN_POINT('Ctrl Pts',(9.72940703075643,-0.810700494112901,
27.142932400863));
#45172=CARTESIAN_POINT('Ctrl Pts',(9.76116363725799,-1.01770239046896,26.6795633494522));
#45173=CARTESIAN_POINT('Ctrl Pts',(9.80350577926016,-0.970730317561869,
25.9949282231766));
#45174=CARTESIAN_POINT('Ctrl Pts',(9.84584792126225,-0.427035532274557,
25.4924965498102));
#45175=CARTESIAN_POINT('Ctrl Pts',(9.8881900632644,0.259176121306736,25.4996082828754));
#45176=CARTESIAN_POINT('Ctrl Pts',(9.91994666976598,0.704794205996023,25.7424594139335));
#45177=CARTESIAN_POINT('Ctrl Pts',(9.95170327626759,0.982064768178995,26.1736225954612));
#45178=CARTESIAN_POINT('Ctrl Pts',(9.98345988276918,1.01813710137885,26.6822905247233));
#45179=CARTESIAN_POINT('Ctrl Pts',(10.0152164892708,0.807063111591556,27.1476978862331));
#45180=CARTESIAN_POINT('Ctrl Pts',(10.0469730957724,0.398764280702476,27.454478445857));
#45181=CARTESIAN_POINT('Ctrl Pts',(10.078729702274,-0.106427006217827,27.5293379534217));
#45182=CARTESIAN_POINT('Ctrl Pts',(10.1104863087756,-0.585857031302619,
27.3524111176363));
#45183=CARTESIAN_POINT('Ctrl Pts',(10.1422429152771,-0.922370055714352,
26.9692618115817));
#45184=CARTESIAN_POINT('Ctrl Pts',(10.1739995217788,-1.03423474310886,26.4689953727654));
#45185=CARTESIAN_POINT('Ctrl Pts',(10.2057561282803,-0.893821386214883,
25.9813098739602));
#45186=CARTESIAN_POINT('Ctrl Pts',(10.2480982702825,-0.416617690923792,
25.4881452427944));
#45187=CARTESIAN_POINT('Ctrl Pts',(10.2904404122846,0.322915308321796,25.4544637489288));
#45188=CARTESIAN_POINT('Ctrl Pts',(10.3327825542867,0.84297205749513,25.9022088748317));
#45189=CARTESIAN_POINT('Ctrl Pts',(10.3645391607883,1.02713471550344,26.3751117958663));
#45190=CARTESIAN_POINT('Ctrl Pts',(10.39629576729,0.961207368148842,26.8834756410901));
#45191=CARTESIAN_POINT('Ctrl Pts',(10.4280523737915,0.660915761234207,27.2956277580859));
#45192=CARTESIAN_POINT('Ctrl Pts',(10.4598089802931,0.199553230693041,27.5154022984479));
#45193=CARTESIAN_POINT('Ctrl Pts',(10.4915655867947,-0.310351339177647,
27.4867746157459));
#45194=CARTESIAN_POINT('Ctrl Pts',(10.5233221932963,-0.744846113467733,
27.2183784426378));
#45195=CARTESIAN_POINT('Ctrl Pts',(10.5550787997979,-0.997351908038651,
26.7740845569543));
#45196=CARTESIAN_POINT('Ctrl Pts',(10.5868354062995,-1.00766660609549,26.2642433819351));
#45197=CARTESIAN_POINT('Ctrl Pts',(10.6185920128011,-0.770737083347005,
25.809661578997));
#45198=CARTESIAN_POINT('Ctrl Pts',(10.6503486193027,-0.34903826235195,25.527308676597));
#45199=CARTESIAN_POINT('Ctrl Pts',(10.6926907613048,0.333684462764655,25.4578507649491));
#45200=CARTESIAN_POINT('Ctrl Pts',(10.735032903307,0.920802605394399,25.9087784588611));
#45201=CARTESIAN_POINT('Ctrl Pts',(10.7773750453091,1.02980885306559,26.5863124866778));
#45202=CARTESIAN_POINT('Ctrl Pts',(10.8091316518107,0.865792198844485,27.0665744925254));
#45203=CARTESIAN_POINT('Ctrl Pts',(10.8408882583123,0.487712887753285,27.4127482189073));
#45204=CARTESIAN_POINT('Ctrl Pts',(10.8726448648139,-0.00753411188962321,
27.5342999613219));
#45205=CARTESIAN_POINT('Ctrl Pts',(10.9044014713155,-0.501927195891623,
27.4049488436461));
#45206=CARTESIAN_POINT('Ctrl Pts',(10.9361580778171,-0.873321024084869,
27.0543937994769));
#45207=CARTESIAN_POINT('Ctrl Pts',(10.9679146843187,-1.03251354487671,26.5691310294889));
#45208=CARTESIAN_POINT('Ctrl Pts',(10.9996712908203,-0.939188918406778,
26.0666902396964));
#45209=CARTESIAN_POINT('Ctrl Pts',(11.0314278973219,-0.618448038849054,
25.6702438941213));
#45210=CARTESIAN_POINT('Ctrl Pts',(11.0631845038235,-0.144295577623383,
25.4754115101961));
#45211=CARTESIAN_POINT('Ctrl Pts',(11.0949411103251,0.360108680627746,25.5313525629285));
#45212=CARTESIAN_POINT('Ctrl Pts',(11.1372832523272,0.92685297651721,25.9183094390236));
#45213=CARTESIAN_POINT('Ctrl Pts',(11.1796253943293,1.0850794696639,26.6415022732033));
#45214=CARTESIAN_POINT('Ctrl Pts',(11.2219675363315,0.731703642215195,27.229771127942));
#45215=CARTESIAN_POINT('Ctrl Pts',(11.253724142833,0.296743917584798,27.4912345002757));
#45216=CARTESIAN_POINT('Ctrl Pts',(11.2854807493346,-0.215447967730317,
27.5122032133915));
#45217=CARTESIAN_POINT('Ctrl Pts',(11.3172373558362,-0.672436134993237,
27.2859152735427));
#45218=CARTESIAN_POINT('Ctrl Pts',(11.3489939623378,-0.967047660490463,
26.8683505693385));
#45219=CARTESIAN_POINT('Ctrl Pts',(11.3807505688394,-1.02503958381233,26.3609462419604));
#45220=CARTESIAN_POINT('Ctrl Pts',(11.412507175341,-0.833965317469191,25.8873294777365));
#45221=CARTESIAN_POINT('Ctrl Pts',(11.4442637818426,-0.438757291247072,
25.5633435997069));
#45222=CARTESIAN_POINT('Ctrl Pts',(11.4760203883442,0.0620007230481136,
25.4669805992429));
#45223=CARTESIAN_POINT('Ctrl Pts',(11.5077769948458,0.550095418630056,25.6236451531699));
#45224=CARTESIAN_POINT('Ctrl Pts',(11.5395336013474,0.899678691404176,25.9915372467506));
#45225=CARTESIAN_POINT('Ctrl Pts',(11.5818757433495,1.08356190788212,26.6526890323327));
#45226=CARTESIAN_POINT('Ctrl Pts',(11.6242178853517,0.738387125023024,27.3075919776769));
#45227=CARTESIAN_POINT('Ctrl Pts',(11.6665600273538,0.089035621292253,27.5295769895203));
#45228=CARTESIAN_POINT('Ctrl Pts',(11.6983166338554,-0.412042520239806,
27.4491173524253));
#45229=CARTESIAN_POINT('Ctrl Pts',(11.730073240357,-0.817153325519727,27.1350067831064));
#45230=CARTESIAN_POINT('Ctrl Pts',(11.7618298468586,-1.02068470593394,26.6674392543729));
#45231=CARTESIAN_POINT('Ctrl Pts',(11.7935864533602,-0.976780670184819,
26.1582942172784));
#45232=CARTESIAN_POINT('Ctrl Pts',(11.8253430598618,-0.694062009399,25.7329797765925));
#45233=CARTESIAN_POINT('Ctrl Pts',(11.8570996663634,-0.242698758880051,
25.494037459927));
#45234=CARTESIAN_POINT('Ctrl Pts',(11.888856272865,0.268287282042353,25.5010730221249));
#45235=CARTESIAN_POINT('Ctrl Pts',(11.9206128793666,0.713253042386499,25.7501711731831));
#45236=CARTESIAN_POINT('Ctrl Pts',(11.9523694858682,0.985443802115579,26.1845585632287));
#45237=CARTESIAN_POINT('Ctrl Pts',(11.9841260923698,1.01558562304907,26.6911595183732));
#45238=CARTESIAN_POINT('Ctrl Pts',(12.0264682343719,0.730016257573543,27.3151666163958));
#45239=CARTESIAN_POINT('Ctrl Pts',(12.068810376374,0.0439846856925677,27.5933826851713));
#45240=CARTESIAN_POINT('Ctrl Pts',(12.1111525183761,-0.59555970749011,27.3445500305032));
#45241=CARTESIAN_POINT('Ctrl Pts',(12.1429091248777,-0.926796127759782,
26.960056219097));
#45242=CARTESIAN_POINT('Ctrl Pts',(12.1746657313793,-1.03405720104669,26.4587825648226));
#45243=CARTESIAN_POINT('Ctrl Pts',(12.2064223378809,-0.888287875944312,
25.9701152745334));
#45244=CARTESIAN_POINT('Ctrl Pts',(12.2381789443825,-0.526542903289158,
25.6091487831361));
#45245=CARTESIAN_POINT('Ctrl Pts',(12.2699355508841,-0.0362472532010614,
25.4662068714475));
#45246=CARTESIAN_POINT('Ctrl Pts',(12.3016921573857,0.462855827725006,25.5744581034156));
#45247=CARTESIAN_POINT('Ctrl Pts',(12.3334487638873,0.84899406708818,25.9092020253238));
#45248=CARTESIAN_POINT('Ctrl Pts',(12.3652053703889,1.0286310290053,26.3864597949332));
#45249=CARTESIAN_POINT('Ctrl Pts',(12.3969619768905,0.956741897977003,26.8940148827339));
#45250=CARTESIAN_POINT('Ctrl Pts',(12.4287185833921,0.653248336737492,27.3007638414404));
#45251=CARTESIAN_POINT('Ctrl Pts',(12.4710607253942,0.0327023948412893,
27.5937782692024));
#45252=CARTESIAN_POINT('Ctrl Pts',(12.5134028673963,-0.671130356429513,
27.3642941591187));
#45253=CARTESIAN_POINT('Ctrl Pts',(12.5557450093985,-0.99970306837254,26.7618203473666));
#45254=CARTESIAN_POINT('Ctrl Pts',(12.5875016159001,-1.00511692324876,26.2543523707434));
#45255=CARTESIAN_POINT('Ctrl Pts',(12.6192582224017,-0.764018502542225,
25.8019678375804));
#45256=CARTESIAN_POINT('Ctrl Pts',(12.6510148289033,-0.337591957320698,
25.5223165935821));
#45257=CARTESIAN_POINT('Ctrl Pts',(12.6827714354049,0.171646482149533,25.4795095273557));
#45258=CARTESIAN_POINT('Ctrl Pts',(12.7145280419065,0.638636511130495,25.6862521873097));
#45259=CARTESIAN_POINT('Ctrl Pts',(12.7462846484081,0.95044934996174,26.090720935364));
#45260=CARTESIAN_POINT('Ctrl Pts',(12.7780412549097,1.02990540953483,26.5955406732408));
#45261=CARTESIAN_POINT('Ctrl Pts',(12.8097978614112,0.859621652443963,27.0762150524315));
#45262=CARTESIAN_POINT('Ctrl Pts',(12.8415544679129,0.477505572712525,27.417927674269));
#45263=CARTESIAN_POINT('Ctrl Pts',(12.8733110744144,-0.0167067740529667,
27.5332845701497));
#45264=CARTESIAN_POINT('Ctrl Pts',(12.9156532164166,-0.680011184951963,
27.3573244060144));
#45265=CARTESIAN_POINT('Ctrl Pts',(12.9579953584187,-1.07020684387626,26.7282053025858));
#45266=CARTESIAN_POINT('Ctrl Pts',(13.0003375004208,-0.933081383677509,
26.055798187033));
#45267=CARTESIAN_POINT('Ctrl Pts',(13.0320941069224,-0.610123262522071,
25.6643251878333));
#45268=CARTESIAN_POINT('Ctrl Pts',(13.063850713424,-0.134199768795049,25.4738598565232));
#45269=CARTESIAN_POINT('Ctrl Pts',(13.0956073199256,0.372077658796297,25.5349137921113));
#45270=CARTESIAN_POINT('Ctrl Pts',(13.1273639264272,0.789006702860459,25.8304242071032));
#45271=CARTESIAN_POINT('Ctrl Pts',(13.1591205329288,1.01278323085218,26.289495312851));
#45272=CARTESIAN_POINT('Ctrl Pts',(13.1908771394304,0.990471642591059,26.7997152729092));
#45273=CARTESIAN_POINT('Ctrl Pts',(13.222633745932,0.725829276801039,27.2368887526424));
#45274=CARTESIAN_POINT('Ctrl Pts',(13.2543903524336,0.285812251560458,27.4946278343466));
#45275=CARTESIAN_POINT('Ctrl Pts',(13.2861469589352,-0.226590453210316,
27.5095838517302));
#45276=CARTESIAN_POINT('Ctrl Pts',(13.3179035654368,-0.678794583544352,
27.2792265604813));
#45277=CARTESIAN_POINT('Ctrl Pts',(13.3602457074389,-1.07250418465013,26.7171523030405));
#45278=CARTESIAN_POINT('Ctrl Pts',(13.4025878494411,-0.965317714357462,
25.9846534572198));
#45279=CARTESIAN_POINT('Ctrl Pts',(13.4449299914432,-0.427067129317259,
25.5589528246334));
#45280=CARTESIAN_POINT('Ctrl Pts',(13.4766865979448,0.0721804151245883,
25.4678213454867));
#45281=CARTESIAN_POINT('Ctrl Pts',(13.5084432044464,0.558814289916099,25.628966268515));
#45282=CARTESIAN_POINT('Ctrl Pts',(13.540199810948,0.906534092576322,26.0019747879583));
#45283=CARTESIAN_POINT('Ctrl Pts',(13.5719564174496,1.03481982305313,26.4966453899845));
#45284=CARTESIAN_POINT('Ctrl Pts',(13.6037130239512,0.910005392756522,26.9918661211764));
#45285=CARTESIAN_POINT('Ctrl Pts',(13.6354696304527,0.564076013020103,27.3675722281905));
#45286=CARTESIAN_POINT('Ctrl Pts',(13.6672262369544,0.0799566012888428,
27.5312323282087));
#45287=CARTESIAN_POINT('Ctrl Pts',(13.6989828434559,-0.422587531096607,
27.4446655231143));
#45288=CARTESIAN_POINT('Ctrl Pts',(13.7307394499576,-0.823983930738844,
27.1258220745904));
#45289=CARTESIAN_POINT('Ctrl Pts',(13.7624960564592,-1.02123471647093,26.6582269669911));
#45290=CARTESIAN_POINT('Ctrl Pts',(13.8048381984613,-0.959949738419397,
25.974722122571));
#45291=CARTESIAN_POINT('Ctrl Pts',(13.8471803404634,-0.405855769996725,
25.4837808096832));
#45292=CARTESIAN_POINT('Ctrl Pts',(13.8895224824656,0.280055116964015,25.5052511620158));
#45293=CARTESIAN_POINT('Ctrl Pts',(13.9212790889671,0.720493983616905,25.7573754604565));
#45294=CARTESIAN_POINT('Ctrl Pts',(13.9530356954688,0.988679976891274,26.1942467084504));
#45295=CARTESIAN_POINT('Ctrl Pts',(13.9847923019703,1.01409920541245,26.703558282598));
#45296=CARTESIAN_POINT('Ctrl Pts',(14.0165489084719,0.793331246795938,27.1644462750661));
#45297=CARTESIAN_POINT('Ctrl Pts',(14.0483055149735,0.378701581549496,27.4626147766054));
#45298=CARTESIAN_POINT('Ctrl Pts',(14.0800621214751,-0.1279457593323,27.5268851942944));
#45299=CARTESIAN_POINT('Ctrl Pts',(14.1118187279767,-0.60356802732903,27.3399635761261));
#45300=CARTESIAN_POINT('Ctrl Pts',(14.1435753344783,-0.931988786459939,
26.9498556145165));
#45301=CARTESIAN_POINT('Ctrl Pts',(14.1753319409799,-1.03335936072766,26.447357633441));
#45302=CARTESIAN_POINT('Ctrl Pts',(14.2070885474815,-0.88277044582558,25.9627175238428));
#45303=CARTESIAN_POINT('Ctrl Pts',(14.2494306894837,-0.395350283369432,
25.4796478538037));
#45304=CARTESIAN_POINT('Ctrl Pts',(14.2917728314857,0.344725633836522,25.4614507300162));
#45305=CARTESIAN_POINT('Ctrl Pts',(14.3341149734879,0.855298044202682,25.9199815737481));
#45306=CARTESIAN_POINT('Ctrl Pts',(14.3658715799895,1.02952342488545,26.3966350892587));
#45307=CARTESIAN_POINT('Ctrl Pts',(14.3976281864911,0.952971445773425,26.9035078630456));
#45308=CARTESIAN_POINT('Ctrl Pts',(14.4293847929927,0.644120061599205,27.3092851902005));
#45309=CARTESIAN_POINT('Ctrl Pts',(14.4611413994943,0.178259121211541,27.5193561719522));
#45310=CARTESIAN_POINT('Ctrl Pts',(14.4928980059959,-0.330934649491577,
27.4800634437489));
#45311=CARTESIAN_POINT('Ctrl Pts',(14.5246546124975,-0.759717250247051,
27.2026329192894));
#45312=CARTESIAN_POINT('Ctrl Pts',(14.5564112189991,-1.00286953121726,26.7531518836361));
#45313=CARTESIAN_POINT('Ctrl Pts',(14.5881678255007,-1.00251198151107,26.243206505289));
#45314=CARTESIAN_POINT('Ctrl Pts',(14.6199244320022,-0.756120833091242,
25.7936827391846));
#45315=CARTESIAN_POINT('Ctrl Pts',(14.6516810385039,-0.328605271270778,
25.5202170164257));
#45316=CARTESIAN_POINT('Ctrl Pts',(14.6940231805059,0.355421546316196,25.4650623819659));
#45317=CARTESIAN_POINT('Ctrl Pts',(14.7363653225081,0.932974057148912,25.9281785615292));
#45318=CARTESIAN_POINT('Ctrl Pts',(14.7787074645102,1.02777695530517,26.6078454883261));
#45319=CARTESIAN_POINT('Ctrl Pts',(14.8104640710118,0.853745269406024,27.0845697581361));
#45320=CARTESIAN_POINT('Ctrl Pts',(14.8422206775134,0.468504017842465,27.4227551989908));
#45321=CARTESIAN_POINT('Ctrl Pts',(14.873977284015,-0.0291783574561754,
27.5339157587969));
#45322=CARTESIAN_POINT('Ctrl Pts',(14.9057338905166,-0.520756093052546,
27.3942462810327));
#45323=CARTESIAN_POINT('Ctrl Pts',(14.9374904970182,-0.884732141731258,
27.035995460237));
#45324=CARTESIAN_POINT('Ctrl Pts',(14.9692471035198,-1.03373418658115,26.5475073792739));
#45325=CARTESIAN_POINT('Ctrl Pts',(15.0010037100214,-0.929914886747041,
26.0471297357535));
#45326=CARTESIAN_POINT('Ctrl Pts',(15.032760316523,-0.60094740010242,25.6574827038516));
#45327=CARTESIAN_POINT('Ctrl Pts',(15.0645169230246,-0.12282132123504,25.4726160843139));
#45328=CARTESIAN_POINT('Ctrl Pts',(15.0962735295262,0.380301726532211,25.5391010896014));
#45329=CARTESIAN_POINT('Ctrl Pts',(15.1386156715283,0.938823638182425,25.9378340768085));
#45330=CARTESIAN_POINT('Ctrl Pts',(15.1809578135304,1.0818804513813,26.6641798944049));
#45331=CARTESIAN_POINT('Ctrl Pts',(15.2232999555326,0.716270690694064,27.2449244370145));
#45332=CARTESIAN_POINT('Ctrl Pts',(15.2550565620342,0.275934307007477,27.4972276798087));
#45333=CARTESIAN_POINT('Ctrl Pts',(15.2868131685358,-0.236584234701834,
27.5074726159503));
#45334=CARTESIAN_POINT('Ctrl Pts',(15.3185697750374,-0.688736545824772,
27.2716703592064));
#45335=CARTESIAN_POINT('Ctrl Pts',(15.350326381539,-0.974544725908092,26.848031459493));
#45336=CARTESIAN_POINT('Ctrl Pts',(15.3820829880406,-1.02190495790187,26.3395246030613));
#45337=CARTESIAN_POINT('Ctrl Pts',(15.4138395945422,-0.820960657969412,
25.8700103828963));
#45338=CARTESIAN_POINT('Ctrl Pts',(15.4455962010437,-0.419058791443737,
25.5543664017463));
#45339=CARTESIAN_POINT('Ctrl Pts',(15.4773528075454,0.083606239906823,25.4685044020221));
#45340=CARTESIAN_POINT('Ctrl Pts',(15.5091094140469,0.568315349191889,25.6353495208853));
#45341=CARTESIAN_POINT('Ctrl Pts',(15.5408660205486,0.910122788432687,26.0104771413058));
#45342=CARTESIAN_POINT('Ctrl Pts',(15.5832081625506,1.08012910476007,26.675332443826));
#45343=CARTESIAN_POINT('Ctrl Pts',(15.6255503045528,0.721324069998707,27.3228681151001));
#45344=CARTESIAN_POINT('Ctrl Pts',(15.6678924465549,0.0674690680729783,
27.5312148389458));
#45345=CARTESIAN_POINT('Ctrl Pts',(15.6996490530565,-0.431815464948015,
27.4402862284391));
#45346=CARTESIAN_POINT('Ctrl Pts',(15.7314056595581,-0.830263818456473,
27.1177662695237));
#45347=CARTESIAN_POINT('Ctrl Pts',(15.7631622660597,-1.0239653391522,26.6460416277893));
#45348=CARTESIAN_POINT('Ctrl Pts',(15.7949188725613,-0.969415499227341,
26.1379269280244));
#45349=CARTESIAN_POINT('Ctrl Pts',(15.8266754790629,-0.677857750545228,
25.7186223921606));
#45350=CARTESIAN_POINT('Ctrl Pts',(15.8584320855645,-0.221592755694851,
25.4891785666026));
#45351=CARTESIAN_POINT('Ctrl Pts',(15.8901886920661,0.289134130458304,25.5069065364043));
#45352=CARTESIAN_POINT('Ctrl Pts',(15.9219452985677,0.728789294203679,25.7652624028585));
#45353=CARTESIAN_POINT('Ctrl Pts',(15.9537019050693,0.991829552779497,26.2052510807591));
#45354=CARTESIAN_POINT('Ctrl Pts',(15.9854585115709,1.01136259502592,26.7123718921871));
#45355=CARTESIAN_POINT('Ctrl Pts',(16.027800653573,0.712796513379461,27.3302659088038));
#45356=CARTESIAN_POINT('Ctrl Pts',(16.0701427955751,0.0210926696708751,
27.5940637312762));
#45357=CARTESIAN_POINT('Ctrl Pts',(16.1124849375773,-0.613104067421575,
27.3319011490073));
#45358=CARTESIAN_POINT('Ctrl Pts',(16.1442415440789,-0.936221230599484,
26.940559410903));
#45359=CARTESIAN_POINT('Ctrl Pts',(16.1759981505805,-1.03296812494877,26.4371507769423));
#45360=CARTESIAN_POINT('Ctrl Pts',(16.207754757082,-0.877003865383148,25.9516411823127));
#45361=CARTESIAN_POINT('Ctrl Pts',(16.2395113635837,-0.507783790844506,
25.5983243702152));
#45362=CARTESIAN_POINT('Ctrl Pts',(16.2712679700852,-0.0146040258474385,
25.4656747037629));
#45363=CARTESIAN_POINT('Ctrl Pts',(16.3030245765869,0.482124254864565,25.5843474881466));
#45364=CARTESIAN_POINT('Ctrl Pts',(16.3347811830884,0.861172381629166,25.9270992215475));
#45365=CARTESIAN_POINT('Ctrl Pts',(16.3665377895901,1.03078191910565,26.4080119179241));
#45366=CARTESIAN_POINT('Ctrl Pts',(16.3982943960916,0.948286387643184,26.9139513427579));
#45367=CARTESIAN_POINT('Ctrl Pts',(16.4300510025932,0.636346828133913,27.3142596843346));
#45368=CARTESIAN_POINT('Ctrl Pts',(16.4723931445954,0.00980457101295316,
27.5942231121645));
#45369=CARTESIAN_POINT('Ctrl Pts',(16.5147352865975,-0.689071371571145,
27.3500594059764));
#45370=CARTESIAN_POINT('Ctrl Pts',(16.5570774285996,-1.00496351044611,26.7408411548729));
#45371=CARTESIAN_POINT('Ctrl Pts',(16.5888340351012,-0.999755857372427,
26.2333710203111));
#45372=CARTESIAN_POINT('Ctrl Pts',(16.6205906416028,-0.749242708650261,
25.7861312897083));
#45373=CARTESIAN_POINT('Ctrl Pts',(16.6523472481044,-0.317056998530502,
25.5154655757592));
#45374=CARTESIAN_POINT('Ctrl Pts',(16.684103854606,0.192965778634376,25.4833252595505));
#45375=CARTESIAN_POINT('Ctrl Pts',(16.7158604611076,0.655526805774623,25.6997958367279));
#45376=CARTESIAN_POINT('Ctrl Pts',(16.7476170676092,0.958806604837357,26.1107016386983));
#45377=CARTESIAN_POINT('Ctrl Pts',(16.7793736741108,1.02768036254931,26.6170736745095));
#45378=CARTESIAN_POINT('Ctrl Pts',(16.8111302806124,0.84737431619961,27.0940790690171));
#45379=CARTESIAN_POINT('Ctrl Pts',(16.842886887114,0.45819054239387,27.4277199006279));
#45380=CARTESIAN_POINT('Ctrl Pts',(16.8746434936156,-0.03832776048991,27.5327086239523));
#45381=CARTESIAN_POINT('Ctrl Pts',(16.9169856356177,-0.697804391611141,
27.3429053208116));
#45382=CARTESIAN_POINT('Ctrl Pts',(16.9593277776199,-1.07474834669968,26.705757964806));
#45383=CARTESIAN_POINT('Ctrl Pts',(17.001669919622,-0.923580740087578,26.036367887498));
#45384=CARTESIAN_POINT('Ctrl Pts',(17.0334265261236,-0.592500579978268,
25.6517395153092));
#45385=CARTESIAN_POINT('Ctrl Pts',(17.0651831326252,-0.112695250427537,
25.471276056202));
#45386=CARTESIAN_POINT('Ctrl Pts',(17.0969397391268,0.392193553644114,25.5429120263731));
#45387=CARTESIAN_POINT('Ctrl Pts',(17.1286963456284,0.802846822853741,25.8470832375036));
#45388=CARTESIAN_POINT('Ctrl Pts',(17.1604529521299,1.01696687064652,26.3107370089288));
#45389=CARTESIAN_POINT('Ctrl Pts',(17.1922095586316,0.983982253354352,26.8203782841956));
#45390=CARTESIAN_POINT('Ctrl Pts',(17.2239661651331,0.710248653396368,27.2519175639406));
#45391=CARTESIAN_POINT('Ctrl Pts',(17.2557227716348,0.264934019955137,27.5003914917165));
#45392=CARTESIAN_POINT('Ctrl Pts',(17.2874793781363,-0.247669462891774,
27.5046206380023));
#45393=CARTESIAN_POINT('Ctrl Pts',(17.319235984638,-0.694953617707919,27.2648500398476));
#45394=CARTESIAN_POINT('Ctrl Pts',(17.36157812664,-1.07681387153837,26.6946593098991));
#45395=CARTESIAN_POINT('Ctrl Pts',(17.4039202686422,-0.954321079185971,
25.9645640902068));
#45396=CARTESIAN_POINT('Ctrl Pts',(17.4462624106443,-0.407279311502855,
25.5502212472916));
#45397=CARTESIAN_POINT('Ctrl Pts',(17.4780190171459,0.093766132664254,25.469557991685));
#45398=CARTESIAN_POINT('Ctrl Pts',(17.5097756236475,0.576920900887735,25.6408519665439));
#45399=CARTESIAN_POINT('Ctrl Pts',(17.5415322301491,0.916758344639924,26.0210558161049));
#45400=CARTESIAN_POINT('Ctrl Pts',(17.5732888366507,1.03466320862596,26.5183029959961));
#45401=CARTESIAN_POINT('Ctrl Pts',(17.6050454431523,0.89951261763213,27.0108028643862));
#45402=CARTESIAN_POINT('Ctrl Pts',(17.6368020496539,0.545795229668867,27.3791875771826));
#45403=CARTESIAN_POINT('Ctrl Pts',(17.6685586561555,0.0583585912529178,
27.5326791628602));
#45404=CARTESIAN_POINT('Ctrl Pts',(17.7003152626571,-0.442267253439534,
27.4356159037157));
#45405=CARTESIAN_POINT('Ctrl Pts',(17.7320718691587,-0.836896502722454,
27.1084383526819));
#45406=CARTESIAN_POINT('Ctrl Pts',(17.7638284756603,-1.02432995541793,26.6368239035113));
#45407=CARTESIAN_POINT('Ctrl Pts',(17.8061706176624,-0.948729406006919,
25.9547380886554));
#45408=CARTESIAN_POINT('Ctrl Pts',(17.8485127596645,-0.384532327064874,
25.4755273691514));
#45409=CARTESIAN_POINT('Ctrl Pts',(17.8908549016667,0.300852282996595,25.5113082876285));
#45410=CARTESIAN_POINT('Ctrl Pts',(17.9226115081683,0.735793104159824,25.7726623671022));
#45411=CARTESIAN_POINT('Ctrl Pts',(17.9543681146699,0.99502713087998,26.2149159219124));
#45412=CARTESIAN_POINT('Ctrl Pts',(17.9861247211715,1.00930328775722,26.7249060355728));
#45413=CARTESIAN_POINT('Ctrl Pts',(18.0178813276731,0.779844466238091,27.180583963405));
#45414=CARTESIAN_POINT('Ctrl Pts',(18.0496379341747,0.35736334799373,27.4709289170012));
#45415=CARTESIAN_POINT('Ctrl Pts',(18.0813945406763,-0.147393818954905,
27.5228873156073));
#45416=CARTESIAN_POINT('Ctrl Pts',(18.1237366826784,-0.783125367432545,
27.2642800146539));
#45417=CARTESIAN_POINT('Ctrl Pts',(18.1660788246805,-1.09047816706153,26.5908592590081));
#45418=CARTESIAN_POINT('Ctrl Pts',(18.2084209666827,-0.86932372855012,25.9412076475843));
#45419=CARTESIAN_POINT('Ctrl Pts',(18.2401775731842,-0.499383898262576,
25.5937943349109));
#45420=CARTESIAN_POINT('Ctrl Pts',(18.2719341796858,-0.00317682288826529,
25.46512447582));
#45421=CARTESIAN_POINT('Ctrl Pts',(18.3036907861874,0.491295670994858,25.5898019214257));
#45422=CARTESIAN_POINT('Ctrl Pts',(18.335447392689,0.867445371041332,25.9357290040588));
#45423=CARTESIAN_POINT('Ctrl Pts',(18.3672039991906,1.03128709694628,26.4194429443397));
#45424=CARTESIAN_POINT('Ctrl Pts',(18.3989606056922,0.944543650636288,26.9227295198934));
#45425=CARTESIAN_POINT('Ctrl Pts',(18.4307172121938,0.626670994684664,27.3228711066594));
#45426=CARTESIAN_POINT('Ctrl Pts',(18.4624738186954,0.157557720092282,27.5228140760235));
#45427=CARTESIAN_POINT('Ctrl Pts',(18.494230425197,-0.352613787923266,27.4727622200216));
#45428=CARTESIAN_POINT('Ctrl Pts',(18.5259870316986,-0.772006450303902,
27.1869950198973));
#45429=CARTESIAN_POINT('Ctrl Pts',(18.5683291737007,-1.09136884806166,26.5795887753102));
#45430=CARTESIAN_POINT('Ctrl Pts',(18.6106713157029,-0.892286124579294,
25.8665603164065));
#45431=CARTESIAN_POINT('Ctrl Pts',(18.653013457705,-0.304460587344251,25.5124475381155));
#45432=CARTESIAN_POINT('Ctrl Pts',(18.6847700642066,0.202308107498574,25.4852713570665));
#45433=CARTESIAN_POINT('Ctrl Pts',(18.7165266707082,0.66461794473409,25.7067433207557));
#45434=CARTESIAN_POINT('Ctrl Pts',(18.7482832772098,0.962302924353875,26.1207820489563));
#45435=CARTESIAN_POINT('Ctrl Pts',(18.7800398837114,1.02691384051011,26.6277156375282));
#45436=CARTESIAN_POINT('Ctrl Pts',(18.811796490213,0.840392506564997,27.1031438722984));
#45437=CARTESIAN_POINT('Ctrl Pts',(18.8435530967146,0.449670903237747,27.4320189904163));
#45438=CARTESIAN_POINT('Ctrl Pts',(18.8753097032162,-0.0512760300646483,
27.5330556333141));
#45439=CARTESIAN_POINT('Ctrl Pts',(18.9070663097177,-0.53881215429493,27.38354662265));
#45440=CARTESIAN_POINT('Ctrl Pts',(18.9388229162194,-0.896600742236581,
27.0164396345976));
#45441=CARTESIAN_POINT('Ctrl Pts',(18.970579522721,-1.03305018659491,26.5276302584141));
#45442=CARTESIAN_POINT('Ctrl Pts',(19.0129216647231,-0.885703716579554,
25.8573887059411));
#45443=CARTESIAN_POINT('Ctrl Pts',(19.0552638067252,-0.27390066770943,25.4405667680158));
#45444=CARTESIAN_POINT('Ctrl Pts',(19.0976059487273,0.403769437737008,25.5487238254014));
#45445=CARTESIAN_POINT('Ctrl Pts',(19.1293625552289,0.80873508663663,25.8545928829001));
#45446=CARTESIAN_POINT('Ctrl Pts',(19.1611191617305,1.01943935782009,26.3219085411192));
#45447=CARTESIAN_POINT('Ctrl Pts',(19.1928757682321,0.980157852742228,26.8303388510914));
#45448=CARTESIAN_POINT('Ctrl Pts',(19.2246323747337,0.702803149690609,27.259559775381));
#45449=CARTESIAN_POINT('Ctrl Pts',(19.2563889812353,0.253753217819898,27.5028217191771));
#45450=CARTESIAN_POINT('Ctrl Pts',(19.2881455877369,-0.25695418374839,27.5024160149589));
#45451=CARTESIAN_POINT('Ctrl Pts',(19.3199021942385,-0.70507685881597,27.2567693149135));
#45452=CARTESIAN_POINT('Ctrl Pts',(19.3516588007401,-0.981452793478104,
26.8282127148256));
#45453=CARTESIAN_POINT('Ctrl Pts',(19.3834154072417,-1.01837402149756,26.316923132266));
#45454=CARTESIAN_POINT('Ctrl Pts',(19.4151720137433,-0.807625565040175,
25.8552542625948));
#45455=CARTESIAN_POINT('Ctrl Pts',(19.4575141557454,-0.262956383022123,
25.4377974348384));
#45456=CARTESIAN_POINT('Ctrl Pts',(19.4998562977476,0.473465944610788,25.5134654856004));
#45457=CARTESIAN_POINT('Ctrl Pts',(19.5421984397497,0.921862468895972,26.0329607001015));
#45458=CARTESIAN_POINT('Ctrl Pts',(19.5739550462513,1.03432477236453,26.5278397635314));
#45459=CARTESIAN_POINT('Ctrl Pts',(19.6057116527529,0.894201810927097,27.0209378977708));
#45460=CARTESIAN_POINT('Ctrl Pts',(19.6374682592545,0.536451672577482,27.3843374784669));
#45461=CARTESIAN_POINT('Ctrl Pts',(19.6692248657561,0.0477390316638463,
27.5337235145085));
#45462=CARTESIAN_POINT('Ctrl Pts',(19.7009814722577,-0.452379697582753,
27.4302659325279));
#45463=CARTESIAN_POINT('Ctrl Pts',(19.7327380787593,-0.842578293657814,
27.1007704542076));
#45464=CARTESIAN_POINT('Ctrl Pts',(19.7644946852609,-1.02685355954554,26.6241166390178));
#45465=CARTESIAN_POINT('Ctrl Pts',(19.7962512917624,-0.961922530439277,
26.118321840509));
#45466=CARTESIAN_POINT('Ctrl Pts',(19.8280078982641,-0.660590012392387,
25.7036184189173));
#45467=CARTESIAN_POINT('Ctrl Pts',(19.8597645047656,-0.201886130050825,
25.4864921758063));
#45468=CARTESIAN_POINT('Ctrl Pts',(19.9021066467678,0.483618392455461,25.518402526854));
#45469=CARTESIAN_POINT('Ctrl Pts',(19.9444487887699,0.997875136828353,26.0509281125392));
#45470=CARTESIAN_POINT('Ctrl Pts',(19.9867909307721,1.00584597201986,26.7371286565982));
#45471=CARTESIAN_POINT('Ctrl Pts',(20.0185475372736,0.772845883424032,27.1879767638772));
#45472=CARTESIAN_POINT('Ctrl Pts',(20.0503041437752,0.34788027460314,27.474655060286));
#45473=CARTESIAN_POINT('Ctrl Pts',(20.0820607502768,-0.159872213864887,
27.5218972786275));
#45474=CARTESIAN_POINT('Ctrl Pts',(20.1138173567784,-0.629805628964096,
27.3211018142211));
#45475=CARTESIAN_POINT('Ctrl Pts',(20.14557396328,-0.945484809342076,26.9196433858772));
#45476=CARTESIAN_POINT('Ctrl Pts',(20.1773305697816,-1.03142817993489,26.4162191595395));
#45477=CARTESIAN_POINT('Ctrl Pts',(20.2090871762832,-0.865079916123635,
25.9330168330965));
#45478=CARTESIAN_POINT('Ctrl Pts',(20.2408437827848,-0.489418261207368,
25.5881650710814));
#45479=CARTESIAN_POINT('Ctrl Pts',(20.2726003892864,0.00826905202714611,
25.465333672173));
#45480=CARTESIAN_POINT('Ctrl Pts',(20.304356995788,0.49892246719443,25.5949958613701));
#45481=CARTESIAN_POINT('Ctrl Pts',(20.3466991377902,1.00245491067529,26.061246651442));
#45482=CARTESIAN_POINT('Ctrl Pts',(20.3890412797922,1.05238006533853,26.7998608792188));
#45483=CARTESIAN_POINT('Ctrl Pts',(20.4313834217944,0.616171706309765,27.3296315733818));
#45484=CARTESIAN_POINT('Ctrl Pts',(20.463140028296,0.14743010257547,27.5241421542027));
#45485=CARTESIAN_POINT('Ctrl Pts',(20.4948966347976,-0.362259777948479,
27.4694024062689));
#45486=CARTESIAN_POINT('Ctrl Pts',(20.5266532412992,-0.780911495880461,
27.1782406714686));
#45487=CARTESIAN_POINT('Ctrl Pts',(20.5584098478008,-1.01077175041952,26.7218192691043));
#45488=CARTESIAN_POINT('Ctrl Pts',(20.5901664543024,-0.993356517859664,
26.2114087242608));
#45489=CARTESIAN_POINT('Ctrl Pts',(20.6219230608039,-0.734573511031013,
25.7711206708353));
#45490=CARTESIAN_POINT('Ctrl Pts',(20.6536796673056,-0.295935925419432,
25.5089121628844));
#45491=CARTESIAN_POINT('Ctrl Pts',(20.6854362738071,0.213555451735285,25.4873958122577));
#45492=CARTESIAN_POINT('Ctrl Pts',(20.7171928803088,0.67323417955922,25.7142783402288));
#45493=CARTESIAN_POINT('Ctrl Pts',(20.7489494868103,0.964786043823933,26.1296704051102));
#45494=CARTESIAN_POINT('Ctrl Pts',(20.7912916288125,1.04923052736995,26.8107018655283));
#45495=CARTESIAN_POINT('Ctrl Pts',(20.8336337708146,0.611314093750934,27.4075876969138));
#45496=CARTESIAN_POINT('Ctrl Pts',(20.8759759128168,-0.0636608179687255,
27.5314569401891));
#45497=CARTESIAN_POINT('Ctrl Pts',(20.9077325193183,-0.547411231874149,
27.378034014363));
#45498=CARTESIAN_POINT('Ctrl Pts',(20.9394891258199,-0.901809936088342,
27.0076534360875));
#45499=CARTESIAN_POINT('Ctrl Pts',(20.9712457323215,-1.03421574978554,26.51519722764));
#45500=CARTESIAN_POINT('Ctrl Pts',(21.0030023388231,-0.915760529993523,
26.0180809494344));
#45501=CARTESIAN_POINT('Ctrl Pts',(21.0347589453247,-0.57345180235752,25.6390731004435));
#45502=CARTESIAN_POINT('Ctrl Pts',(21.0665155518263,-0.0918045968468163,
25.4692550094277));
#45503=CARTESIAN_POINT('Ctrl Pts',(21.0982721583279,0.412565734402345,25.5515155838763));
#45504=CARTESIAN_POINT('Ctrl Pts',(21.1300287648295,0.815964861986395,25.8634667989785));
#45505=CARTESIAN_POINT('Ctrl Pts',(21.1617853713311,1.02117005185408,26.3332231660069));
#45506=CARTESIAN_POINT('Ctrl Pts',(21.1935419778327,0.976327171856112,26.838734959377));
#45507=CARTESIAN_POINT('Ctrl Pts',(21.2358841198349,0.60191837674119,27.4138460573581));
#45508=CARTESIAN_POINT('Ctrl Pts',(21.2782262618369,-0.117622662984219,
27.5879270462491));
#45509=CARTESIAN_POINT('Ctrl Pts',(21.3205684038391,-0.713515152902132,
27.2475642084716));
#45510=CARTESIAN_POINT('Ctrl Pts',(21.3523250103406,-0.984473950176901,
26.8184553792661));
#45511=CARTESIAN_POINT('Ctrl Pts',(21.3840816168423,-1.01669340159119,26.3068479895003));
#45512=CARTESIAN_POINT('Ctrl Pts',(21.4158382233439,-0.800502768285593,
25.844997335273));
#45513=CARTESIAN_POINT('Ctrl Pts',(21.4475948298455,-0.389513214291506,
25.541280658647));
#45514=CARTESIAN_POINT('Ctrl Pts',(21.4793514363471,0.116494160805104,25.472152148173));
#45515=CARTESIAN_POINT('Ctrl Pts',(21.5111080428486,0.594195549276261,25.6527721860017));
#45516=CARTESIAN_POINT('Ctrl Pts',(21.5428646493503,0.926788179821187,26.040764937558));
#45517=CARTESIAN_POINT('Ctrl Pts',(21.5746212558519,1.03413244324324,26.5392843713313));
#45518=CARTESIAN_POINT('Ctrl Pts',(21.6063778623534,0.88823197146014,27.0307040154704));
#45519=CARTESIAN_POINT('Ctrl Pts',(21.6381344688551,0.528111077870776,27.3882875709132));
#45520=CARTESIAN_POINT('Ctrl Pts',(21.6804766108571,-0.128840070118087,
27.5866556884035));
#45521=CARTESIAN_POINT('Ctrl Pts',(21.7228187528594,-0.791170334647484,
27.2559562489864));
#45522=CARTESIAN_POINT('Ctrl Pts',(21.7651608948614,-1.0273717259971,26.6116398487566));
#45523=CARTESIAN_POINT('Ctrl Pts',(21.7969175013631,-0.957943088858718,
26.1089145545175));
#45524=CARTESIAN_POINT('Ctrl Pts',(21.8286741078646,-0.65281099082484,25.6969987657186));
#45525=CARTESIAN_POINT('Ctrl Pts',(21.8604307143662,-0.1898291330484,25.4832413889823));
#45526=CARTESIAN_POINT('Ctrl Pts',(21.8921873208678,0.320157771778428,25.5159459767056));
#45527=CARTESIAN_POINT('Ctrl Pts',(21.9239439273694,0.751582456070183,25.7892497571336));
#45528=CARTESIAN_POINT('Ctrl Pts',(21.955700533871,1.00038611624865,26.2352530679894));
#45529=CARTESIAN_POINT('Ctrl Pts',(21.9874571403726,1.00458155593204,26.7462703195953));
#45530=CARTESIAN_POINT('Ctrl Pts',(22.0192137468742,0.765322018551718,27.1966027418257));
#45531=CARTESIAN_POINT('Ctrl Pts',(22.0509703533758,0.337021128126196,27.4782737583913));
#45532=CARTESIAN_POINT('Ctrl Pts',(22.0827269598774,-0.168795095708431,
27.5195412374561));
#45533=CARTESIAN_POINT('Ctrl Pts',(22.1250691018795,-0.798927100233512,
27.2477538614546));
#45534=CARTESIAN_POINT('Ctrl Pts',(22.1674112438817,-1.09215204104248,26.5680019709608));
#45535=CARTESIAN_POINT('Ctrl Pts',(22.2097533858837,-0.857433947833973,
25.9231437403386));
#45536=CARTESIAN_POINT('Ctrl Pts',(22.2415099923854,-0.480312159776085,
25.5835377714648));
#45537=CARTESIAN_POINT('Ctrl Pts',(22.2732665988869,0.0184832960993065,
25.4652867354845));
#45538=CARTESIAN_POINT('Ctrl Pts',(22.3050232053886,0.510235965813027,25.6002820263975));
#45539=CARTESIAN_POINT('Ctrl Pts',(22.3367798118902,0.879064903268412,25.9540071287703));
#45540=CARTESIAN_POINT('Ctrl Pts',(22.3685364183917,1.03274691096626,26.4410431183259));
#45541=CARTESIAN_POINT('Ctrl Pts',(22.4002930248934,0.935489987070818,26.9424045701417));
#45542=CARTESIAN_POINT('Ctrl Pts',(22.4320496313949,0.609312582905039,27.3358058082749));
#45543=CARTESIAN_POINT('Ctrl Pts',(22.4638062378966,0.136117726577721,27.525887487257));
#45544=CARTESIAN_POINT('Ctrl Pts',(22.4955628443981,-0.372894606452285,
27.4651696222111));
#45545=CARTESIAN_POINT('Ctrl Pts',(22.5273194508997,-0.7862148363273,27.170687967946));
#45546=CARTESIAN_POINT('Ctrl Pts',(22.5696615929019,-1.09279546637427,26.5567310979945));
#45547=CARTESIAN_POINT('Ctrl Pts',(22.612003734904,-0.878834030206561,25.8480252334954));
#45548=CARTESIAN_POINT('Ctrl Pts',(22.6543458769061,-0.28372634610829,25.5062920551124));
#45549=CARTESIAN_POINT('Ctrl Pts',(22.6861024834077,0.223500105487194,25.4897275169502));
#45550=CARTESIAN_POINT('Ctrl Pts',(22.7178590899093,0.681073708837323,25.7208262227656));
#45551=CARTESIAN_POINT('Ctrl Pts',(22.7496156964109,0.970028462438422,26.1410042411229));
#45552=CARTESIAN_POINT('Ctrl Pts',(22.7813723029125,1.024016088893,26.6491789840438));
#45553=CARTESIAN_POINT('Ctrl Pts',(22.8131289094141,0.827585813813665,27.1205995623439));
#45554=CARTESIAN_POINT('Ctrl Pts',(22.8448855159157,0.430067065154834,27.4412256047629));
#45555=CARTESIAN_POINT('Ctrl Pts',(22.8766421224173,-0.0728846540605334,
27.5317562696853));
#45556=CARTESIAN_POINT('Ctrl Pts',(22.9083987289189,-0.557185066024646,
27.3720768166843));
#45557=CARTESIAN_POINT('Ctrl Pts',(22.9401553354205,-0.907212454062326,
26.9975624085023));
#45558=CARTESIAN_POINT('Ctrl Pts',(22.9719119419221,-1.03340217998071,26.5060044666528));
#45559=CARTESIAN_POINT('Ctrl Pts',(23.0142540839242,-0.872061123160507,
25.8389933840877));
#45560=CARTESIAN_POINT('Ctrl Pts',(23.0565962259264,-0.251668792754912,
25.4350665900813));
#45561=CARTESIAN_POINT('Ctrl Pts',(23.0989383679284,0.423589374350715,25.5573822826056));
#45562=CARTESIAN_POINT('Ctrl Pts',(23.1306949744301,0.822065082155542,25.8716594968801));
#45563=CARTESIAN_POINT('Ctrl Pts',(23.1624515809316,1.02294319380588,26.3432824379804));
#45564=CARTESIAN_POINT('Ctrl Pts',(23.1942081874333,0.973029829999189,26.8507793077765));
#45565=CARTESIAN_POINT('Ctrl Pts',(23.2259647939348,0.68675310912089,27.2741017289122));
#45566=CARTESIAN_POINT('Ctrl Pts',(23.2577214004365,0.232710524832593,27.5079126488139));
#45567=CARTESIAN_POINT('Ctrl Pts',(23.2894780069381,-0.27787653308415,27.49681891633));
#45568=CARTESIAN_POINT('Ctrl Pts',(23.3212346134396,-0.720760152325672,
27.2418476768528));
#45569=CARTESIAN_POINT('Ctrl Pts',(23.3529912199413,-0.98810669635931,26.8076009242656));
#45570=CARTESIAN_POINT('Ctrl Pts',(23.3847478264428,-1.01431953699964,26.2956506324423));
#45571=CARTESIAN_POINT('Ctrl Pts',(23.4165044329445,-0.793955402214,25.8384934327583));
#45572=CARTESIAN_POINT('Ctrl Pts',(23.4588465749466,-0.240668948257476,
25.4325269061225));
#45573=CARTESIAN_POINT('Ctrl Pts',(23.5011887169487,0.494008505367471,25.5235902778892));
#45574=CARTESIAN_POINT('Ctrl Pts',(23.5435308589508,0.931434794646534,26.0523557857735));
#45575=CARTESIAN_POINT('Ctrl Pts',(23.5752874654524,1.03351560643094,26.5494800810842));
#45576=CARTESIAN_POINT('Ctrl Pts',(23.607044071954,0.883103744901561,27.0395377166982));
#45577=CARTESIAN_POINT('Ctrl Pts',(23.6388006784556,0.517826709887917,27.3953706893567));
#45578=CARTESIAN_POINT('Ctrl Pts',(23.6705572849572,0.026094744315042,27.5344961981135));
#45579=CARTESIAN_POINT('Ctrl Pts',(23.7023138914588,-0.471749284087486,
27.4205947582786));
#45580=CARTESIAN_POINT('Ctrl Pts',(23.7340704979604,-0.854966718043896,
27.0830053435684));
#45581=CARTESIAN_POINT('Ctrl Pts',(23.765827104462,-1.02922618322529,26.6025993986139));
#45582=CARTESIAN_POINT('Ctrl Pts',(23.7975837109636,-0.953724069196557,
26.0982742579392));
#45583=CARTESIAN_POINT('Ctrl Pts',(23.8293403174652,-0.643778608069701,
25.6899679691813));
#45584=CARTESIAN_POINT('Ctrl Pts',(23.8610969239668,-0.180631157292743,
25.4824890643223));
#45585=CARTESIAN_POINT('Ctrl Pts',(23.9034390659689,0.504055406949821,25.5287387089293));
#45586=CARTESIAN_POINT('Ctrl Pts',(23.945781207971,1.00705479143988,26.0719100610318));
#45587=CARTESIAN_POINT('Ctrl Pts',(23.9881233499732,1.0006630320742,26.7581271304004));
#45588=CARTESIAN_POINT('Ctrl Pts',(24.0198799564748,0.758278596218176,27.2040002540325));
#45589=CARTESIAN_POINT('Ctrl Pts',(24.0516365629764,0.327406439929028,27.4817220559263));
#45590=CARTESIAN_POINT('Ctrl Pts',(24.083393169478,-0.181223530827346,27.5183276509586));
#45591=CARTESIAN_POINT('Ctrl Pts',(24.1151497759796,-0.646851762725688,
27.3077413674257));
#45592=CARTESIAN_POINT('Ctrl Pts',(24.1469063824811,-0.954060056708101,
26.8997643108148));
#45593=CARTESIAN_POINT('Ctrl Pts',(24.1786629889828,-1.02944890996991,26.3946517140441));
#45594=CARTESIAN_POINT('Ctrl Pts',(24.2104195954843,-0.853024589922902,
25.9150365636903));
#45595=CARTESIAN_POINT('Ctrl Pts',(24.2421762019859,-0.47022813118385,25.5781222008084));
#45596=CARTESIAN_POINT('Ctrl Pts',(24.2739328084876,0.029920803971738,25.4657333358122));
#45597=CARTESIAN_POINT('Ctrl Pts',(24.3056894149891,0.517753179655688,25.6056355529399));
#45598=CARTESIAN_POINT('Ctrl Pts',(24.3480315569913,1.01141761520222,26.0823221858101));
#45599=CARTESIAN_POINT('Ctrl Pts',(24.3903736989933,1.04587406972389,26.8218194821433));
#45600=CARTESIAN_POINT('Ctrl Pts',(24.4327158409956,0.598674172340223,27.3423451516935));
#45601=CARTESIAN_POINT('Ctrl Pts',(24.4644724474971,0.12596450061625,27.5270032773778));
#45602=CARTESIAN_POINT('Ctrl Pts',(24.4962290539988,-0.382468152772,27.4616086959436));
#45603=CARTESIAN_POINT('Ctrl Pts',(24.5279856605003,-0.794934727931843,
27.1617491603019));
#45604=CARTESIAN_POINT('Ctrl Pts',(24.5597422670019,-1.01519262315461,26.7006171913983));
#45605=CARTESIAN_POINT('Ctrl Pts',(24.5914988735035,-0.987099300322622,
26.1906829016855));
#45606=CARTESIAN_POINT('Ctrl Pts',(24.6232554800051,-0.719158594584726,
25.7559071056468));
#45607=CARTESIAN_POINT('Ctrl Pts',(24.6550120865067,-0.275129561181238,
25.5029358609414));
#45608=CARTESIAN_POINT('Ctrl Pts',(24.6867686930083,0.234700524814755,25.492086890823));
#45609=CARTESIAN_POINT('Ctrl Pts',(24.7185252995099,0.68953036364492,25.7285399136883));
#45610=CARTESIAN_POINT('Ctrl Pts',(24.7502819060115,0.972325021744744,26.1499426171358));
#45611=CARTESIAN_POINT('Ctrl Pts',(24.7926240480136,1.04249834070029,26.8325921803725));
#45612=CARTESIAN_POINT('Ctrl Pts',(24.8349661900157,0.59218615294308,27.4201825411679));
#45613=CARTESIAN_POINT('Ctrl Pts',(24.8773083320179,-0.0852332719656635,
27.5298987370411));
#45614=CARTESIAN_POINT('Ctrl Pts',(24.9090649385194,-0.56566689204097,27.3663854537151));
#45615=CARTESIAN_POINT('Ctrl Pts',(24.9408215450211,-0.912236628899084,
26.9886691159609));
#45616=CARTESIAN_POINT('Ctrl Pts',(24.9725781515226,-1.03430728862988,26.4935497659328));
#45617=CARTESIAN_POINT('Ctrl Pts',(25.0043347580243,-0.905474331192122,
25.9990214025088));
#45618=CARTESIAN_POINT('Ctrl Pts',(25.0360913645258,-0.555308674141558,
25.627260421185));
#45619=CARTESIAN_POINT('Ctrl Pts',(25.0678479710275,-0.0702129931772203,
25.4675594665158));
#45620=CARTESIAN_POINT('Ctrl Pts',(25.099604577529,0.432325318386934,25.5603575190988));
#45621=CARTESIAN_POINT('Ctrl Pts',(25.1313611840307,0.82910756018719,25.8806827746304));
#45622=CARTESIAN_POINT('Ctrl Pts',(25.1631177905322,1.02443671559781,26.3546308048603));
#45623=CARTESIAN_POINT('Ctrl Pts',(25.1948743970339,0.969024273802758,26.8590934084466));
#45624=CARTESIAN_POINT('Ctrl Pts',(25.2372165390359,0.582661518377644,27.426242896766));
#45625=CARTESIAN_POINT('Ctrl Pts',(25.2795586810381,-0.140365108464849,
27.5852271583099));
#45626=CARTESIAN_POINT('Ctrl Pts',(25.3219008230402,-0.729003953235837,
27.2324679893181));
#45627=CARTESIAN_POINT('Ctrl Pts',(25.3536574295418,-0.990922989234294,
26.7977824987574));
#45628=CARTESIAN_POINT('Ctrl Pts',(25.3854140360434,-1.01242843194554,26.285612868414));
#45629=CARTESIAN_POINT('Ctrl Pts',(25.417170642545,-0.786619507832964,25.8283878182122));
#45630=CARTESIAN_POINT('Ctrl Pts',(25.4489272490466,-0.369363765088924,
25.5333388760098));
#45631=CARTESIAN_POINT('Ctrl Pts',(25.4806838555482,0.137979512235093,25.4748152604466));
#45632=CARTESIAN_POINT('Ctrl Pts',(25.5124404620498,0.611796248789613,25.6653931047851));
#45633=CARTESIAN_POINT('Ctrl Pts',(25.5441970685514,0.936196099210013,26.0602613995694));
#45634=CARTESIAN_POINT('Ctrl Pts',(25.575953675053,1.03308380589826,26.560918157259));
#45635=CARTESIAN_POINT('Ctrl Pts',(25.6077102815546,0.876930827085415,27.0491767582768));
#45636=CARTESIAN_POINT('Ctrl Pts',(25.6394668880562,0.509405273945525,27.3991453641787));
#45637=CARTESIAN_POINT('Ctrl Pts',(25.6818090300583,-0.151553451361267,
27.5837213202816));
#45638=CARTESIAN_POINT('Ctrl Pts',(25.7241511720605,-0.806817757172094,
27.2392330192721));
#45639=CARTESIAN_POINT('Ctrl Pts',(25.7664933140625,-1.02948312020622,26.5901144967068));
#45640=CARTESIAN_POINT('Ctrl Pts',(25.7982499205642,-0.949548624829341,
26.0889523143866));
#45641=CARTESIAN_POINT('Ctrl Pts',(25.8300065270657,-0.635862749944225,
25.6835125654851));
#45642=CARTESIAN_POINT('Ctrl Pts',(25.8617631335674,-0.168508775453428,
25.4794913193942));
#45643=CARTESIAN_POINT('Ctrl Pts',(25.8935197400689,0.340682011144958,25.5228617818911));
#45644=CARTESIAN_POINT('Ctrl Pts',(25.9252763465706,0.766292448421236,25.8051345895338));
#45645=CARTESIAN_POINT('Ctrl Pts',(25.9570329530721,1.00570770483935,26.2562471941713));
#45646=CARTESIAN_POINT('Ctrl Pts',(25.9887895595738,0.999207484337658,26.7672403335045));
#45647=CARTESIAN_POINT('Ctrl Pts',(26.0205461660753,0.750576026028524,27.2124668751901));
#45648=CARTESIAN_POINT('Ctrl Pts',(26.0523027725769,0.316473618880258,27.4851127148182));
#45649=CARTESIAN_POINT('Ctrl Pts',(26.0840593790785,-0.190094577903723,
27.5157853616777));
#45650=CARTESIAN_POINT('Ctrl Pts',(26.1264015210806,-0.814402461431545,
27.2308701517941));
#45651=CARTESIAN_POINT('Ctrl Pts',(26.1687436630828,-1.0933334814934,26.545130338164));
#45652=CARTESIAN_POINT('Ctrl Pts',(26.2110858050849,-0.845176745039968,
25.9053257852602));
#45653=CARTESIAN_POINT('Ctrl Pts',(26.2428424115865,-0.461020723843732,
25.5736862003506));
#45654=CARTESIAN_POINT('Ctrl Pts',(26.2745990180881,0.0401212288996642,
25.4659007339855));
#45655=CARTESIAN_POINT('Ctrl Pts',(26.3063556245897,0.52897749149536,25.6111562525088));
#45656=CARTESIAN_POINT('Ctrl Pts',(26.3381122310913,0.890253680816816,25.9725259631335));
#45657=CARTESIAN_POINT('Ctrl Pts',(26.3698688375929,1.03384007386217,26.4626646873927));
#45658=CARTESIAN_POINT('Ctrl Pts',(26.4016254440945,0.925865194744989,26.9619004416844));
#45659=CARTESIAN_POINT('Ctrl Pts',(26.4227965150956,0.70328308920618,27.219502667261));
#45660=CARTESIAN_POINT('Ctrl Pts',(26.4333820505961,0.567943631320456,27.313938745633));
#45661=CARTESIAN_POINT('Ctrl Pts',(9.55924492783123,0.793913214729588,26.042198285305));
#45662=CARTESIAN_POINT('Ctrl Pts',(9.56983046333176,0.870035203292496,26.1742079539272));
#45663=CARTESIAN_POINT('Ctrl Pts',(9.59100153433282,0.955123975386584,26.4768302220545));
#45664=CARTESIAN_POINT('Ctrl Pts',(9.62275814083443,0.849667148176577,26.9365296811876));
#45665=CARTESIAN_POINT('Ctrl Pts',(9.65451474733602,0.537468143587547,27.2899993389655));
#45666=CARTESIAN_POINT('Ctrl Pts',(9.68627135383762,0.0937613626242288,
27.4504710862759));
#45667=CARTESIAN_POINT('Ctrl Pts',(9.71802796033921,-0.371876568579776,
27.3802506620641));
#45668=CARTESIAN_POINT('Ctrl Pts',(9.74978456684081,-0.748580824009798,
27.0936679080815));
#45669=CARTESIAN_POINT('Ctrl Pts',(9.7815411733424,-0.939721265234505,26.665804364338));
#45670=CARTESIAN_POINT('Ctrl Pts',(9.82388331534454,-0.89634841262424,26.0336291890481));
#45671=CARTESIAN_POINT('Ctrl Pts',(9.86622545734667,-0.394314069071067,
25.569696184457));
#45672=CARTESIAN_POINT('Ctrl Pts',(9.90856759934879,0.239316832616143,25.5762629832153));
#45673=CARTESIAN_POINT('Ctrl Pts',(9.94032420585039,0.650789571874067,25.8005057228205));
#45674=CARTESIAN_POINT('Ctrl Pts',(9.97208081235198,0.906814364531588,26.1986311613203));
#45675=CARTESIAN_POINT('Ctrl Pts',(10.0038374188536,0.940122666557803,26.6683225706626));
#45676=CARTESIAN_POINT('Ctrl Pts',(10.0355940253552,0.745222154778916,27.0980682396355));
#45677=CARTESIAN_POINT('Ctrl Pts',(10.0673506318568,0.368209093249168,27.3813418354716));
#45678=CARTESIAN_POINT('Ctrl Pts',(10.0991072383584,-0.0982720703761154,
27.4504652568396));
#45679=CARTESIAN_POINT('Ctrl Pts',(10.13086384486,-0.540965920742814,27.2870953841388));
#45680=CARTESIAN_POINT('Ctrl Pts',(10.1626204513616,-0.85169374061398,26.9333047730217));
#45681=CARTESIAN_POINT('Ctrl Pts',(10.1943770578631,-0.954986831558773,
26.4713710925651));
#45682=CARTESIAN_POINT('Ctrl Pts',(10.2261336643648,-0.825332603926062,
26.0210543415525));
#45683=CARTESIAN_POINT('Ctrl Pts',(10.2684758063669,-0.384694491533629,
25.5656782949712));
#45684=CARTESIAN_POINT('Ctrl Pts',(10.310817948369,0.298172024495185,25.5345776349681));
#45685=CARTESIAN_POINT('Ctrl Pts',(10.3531600903711,0.778379589008935,25.9480144315763));
#45686=CARTESIAN_POINT('Ctrl Pts',(10.3849166968727,0.948430841333095,26.3846813151855));
#45687=CARTESIAN_POINT('Ctrl Pts',(10.4166733033743,0.887555156211573,26.8540919408332));
#45688=CARTESIAN_POINT('Ctrl Pts',(10.4484299098759,0.610273299126541,27.2346630316351));
#45689=CARTESIAN_POINT('Ctrl Pts',(10.4801865163775,0.184262527222831,27.4375974170403));
#45690=CARTESIAN_POINT('Ctrl Pts',(10.5119431228791,-0.286570765530798,
27.4111633215117));
#45691=CARTESIAN_POINT('Ctrl Pts',(10.5436997293807,-0.687772514546559,
27.1633329206604));
#45692=CARTESIAN_POINT('Ctrl Pts',(10.5754563358823,-0.92093013211283,26.7530829140763));
#45693=CARTESIAN_POINT('Ctrl Pts',(10.6072129423839,-0.930454469678779,
26.2823081585637));
#45694=CARTESIAN_POINT('Ctrl Pts',(10.6389695488855,-0.711679597010942,
25.8625585431454));
#45695=CARTESIAN_POINT('Ctrl Pts',(10.6707261553871,-0.322293315397946,
25.6018408429898));
#45696=CARTESIAN_POINT('Ctrl Pts',(10.7130682973892,0.308115995869649,25.5377051219523));
#45697=CARTESIAN_POINT('Ctrl Pts',(10.7554104393913,0.850246395681263,25.9540806232981));
#45698=CARTESIAN_POINT('Ctrl Pts',(10.7977525813935,0.950900073946533,26.5796988195625));
#45699=CARTESIAN_POINT('Ctrl Pts',(10.8295091878951,0.799451144212613,27.023160900428));
#45700=CARTESIAN_POINT('Ctrl Pts',(10.8612657943967,0.450342041291193,27.3428091740228));
#45701=CARTESIAN_POINT('Ctrl Pts',(10.8930224008983,-0.00695681293825255,
27.4550470524467));
#45702=CARTESIAN_POINT('Ctrl Pts',(10.9247790073999,-0.463467182543916,
27.3356074234353));
#45703=CARTESIAN_POINT('Ctrl Pts',(10.9565356139015,-0.806403075589457,
27.0119135491492));
#45704=CARTESIAN_POINT('Ctrl Pts',(10.9882922204031,-0.953397519599223,
26.563833886121));
#45705=CARTESIAN_POINT('Ctrl Pts',(11.0200488269047,-0.867223863248237,
26.0998924636472));
#45706=CARTESIAN_POINT('Ctrl Pts',(11.0518054334063,-0.571059652597703,
25.7338236944761));
#45707=CARTESIAN_POINT('Ctrl Pts',(11.0835620399079,-0.133238974421134,
25.5539202806239));
#45708=CARTESIAN_POINT('Ctrl Pts',(11.1153186464094,0.332515466358953,25.6055748678044));
#45709=CARTESIAN_POINT('Ctrl Pts',(11.1576607884116,0.855833159021813,25.9628812951065));
#45710=CARTESIAN_POINT('Ctrl Pts',(11.2000029304137,1.00193559695058,26.6306597060727));
#45711=CARTESIAN_POINT('Ctrl Pts',(11.2423450724158,0.675637081015731,27.1738526450402));
#45712=CARTESIAN_POINT('Ctrl Pts',(11.2741016789174,0.274006008333107,27.4152814687936));
#45713=CARTESIAN_POINT('Ctrl Pts',(11.305858285419,-0.198939335039208,27.4346434608691));
#45714=CARTESIAN_POINT('Ctrl Pts',(11.3376148919206,-0.62091092787356,27.2256947631619));
#45715=CARTESIAN_POINT('Ctrl Pts',(11.3693714984222,-0.892947937991379,
26.8401258229424));
#45716=CARTESIAN_POINT('Ctrl Pts',(11.4011281049238,-0.946496248448144,
26.3716011923876));
#45717=CARTESIAN_POINT('Ctrl Pts',(11.4328847114254,-0.770062987601644,
25.9342751635987));
#45718=CARTESIAN_POINT('Ctrl Pts',(11.464641317927,-0.40513765195304,25.6351146014624));
#45719=CARTESIAN_POINT('Ctrl Pts',(11.4963979244286,0.0572499371661582,
25.5461353855679));
#45720=CARTESIAN_POINT('Ctrl Pts',(11.5281545309302,0.507944530381333,25.6907955673779));
#45721=CARTESIAN_POINT('Ctrl Pts',(11.5599111374318,0.830741094949436,26.030498045123));
#45722=CARTESIAN_POINT('Ctrl Pts',(11.6022532794339,1.00053431786251,26.640989283306));
#45723=CARTESIAN_POINT('Ctrl Pts',(11.644595421436,0.681808444057784,27.2457104966669));
#45724=CARTESIAN_POINT('Ctrl Pts',(11.6869375634382,0.0822132948446471,
27.4506859768724));
#45725=CARTESIAN_POINT('Ctrl Pts',(11.7186941699398,-0.380469891862701,
27.3763915341362));
#45726=CARTESIAN_POINT('Ctrl Pts',(11.7504507764414,-0.754539209241824,
27.0863495882901));
#45727=CARTESIAN_POINT('Ctrl Pts',(11.782207382943,-0.942475061715997,26.6546092742268));
#45728=CARTESIAN_POINT('Ctrl Pts',(11.8139639894446,-0.901935158882476,
26.1844773152895));
#45729=CARTESIAN_POINT('Ctrl Pts',(11.8457205959462,-0.640879726462179,
25.791752459706));
#45730=CARTESIAN_POINT('Ctrl Pts',(11.8774772024478,-0.224102042897375,
25.5711190228213));
#45731=CARTESIAN_POINT('Ctrl Pts',(11.9092338089494,0.247729853529148,25.5776154872809));
#45732=CARTESIAN_POINT('Ctrl Pts',(11.9409904154509,0.658600252589484,25.8076265709458));
#45733=CARTESIAN_POINT('Ctrl Pts',(11.9727470219526,0.909934481056709,26.2087291640008));
#45734=CARTESIAN_POINT('Ctrl Pts',(12.0045036284541,0.937766694451681,26.6765119804666));
#45735=CARTESIAN_POINT('Ctrl Pts',(12.0468457704563,0.674078991690957,27.2527047310789));
#45736=CARTESIAN_POINT('Ctrl Pts',(12.0891879124584,0.0406143730004874,
27.5096025811841));
#45737=CARTESIAN_POINT('Ctrl Pts',(12.1315300544605,-0.549925132422438,
27.2798366503321));
#45738=CARTESIAN_POINT('Ctrl Pts',(12.1632866609622,-0.85578066628253,26.9248045561627));
#45739=CARTESIAN_POINT('Ctrl Pts',(12.1950432674637,-0.954822893601219,
26.4619408378153));
#45740=CARTESIAN_POINT('Ctrl Pts',(12.2267998739653,-0.820223097137686,
26.0107175247821));
#45741=CARTESIAN_POINT('Ctrl Pts',(12.2585564804669,-0.486196719112702,
25.6774099771336));
#45742=CARTESIAN_POINT('Ctrl Pts',(12.2903130869685,-0.0334698188374221,
25.5454209444212));
#45743=CARTESIAN_POINT('Ctrl Pts',(12.3220696934701,0.427389645660999,25.6453774598239));
#45744=CARTESIAN_POINT('Ctrl Pts',(12.3538262999717,0.783940164013017,25.9544717341139));
#45745=CARTESIAN_POINT('Ctrl Pts',(12.3855829064733,0.949812500284005,26.395159777397));
#45746=CARTESIAN_POINT('Ctrl Pts',(12.4173395129749,0.883431851285648,26.8638236164045));
#45747=CARTESIAN_POINT('Ctrl Pts',(12.4490961194765,0.60319338861771,27.2394055642196));
#45748=CARTESIAN_POINT('Ctrl Pts',(12.4914382614786,0.0301965841333301,
27.5099678537134));
#45749=CARTESIAN_POINT('Ctrl Pts',(12.5337804034807,-0.619705204181141,
27.2980678913091));
#45750=CARTESIAN_POINT('Ctrl Pts',(12.5761225454829,-0.923101135526423,
26.7417584456868));
#45751=CARTESIAN_POINT('Ctrl Pts',(12.6078791519845,-0.928100155477381,
26.2731750429903));
#45752=CARTESIAN_POINT('Ctrl Pts',(12.6396357584861,-0.705475825344904,
25.8554543322424));
#45753=CARTESIAN_POINT('Ctrl Pts',(12.6713923649877,-0.311724079885715,
25.5972312767641));
#45754=CARTESIAN_POINT('Ctrl Pts',(12.7031489714893,0.158494124499654,25.557704288509));
#45755=CARTESIAN_POINT('Ctrl Pts',(12.7349055779909,0.5897011895471,25.7486053572393));
#45756=CARTESIAN_POINT('Ctrl Pts',(12.7666621844925,0.877621467780753,26.1220818148255));
#45757=CARTESIAN_POINT('Ctrl Pts',(12.7984187909941,0.950989231806714,26.5882198992358));
#45758=CARTESIAN_POINT('Ctrl Pts',(12.8301753974956,0.793753413987165,27.0320627554668));
#45759=CARTESIAN_POINT('Ctrl Pts',(12.8619320039973,0.440916858551541,27.3475917552481));
#45760=CARTESIAN_POINT('Ctrl Pts',(12.8936886104988,-0.0154266227514476,
27.4541094653034));
#45761=CARTESIAN_POINT('Ctrl Pts',(12.936030752501,-0.627905542014287,27.291632193342));
#45762=CARTESIAN_POINT('Ctrl Pts',(12.9783728945031,-0.988202581431092,
26.7107191431281));
#45763=CARTESIAN_POINT('Ctrl Pts',(13.0207150365052,-0.86158431644457,26.0898350110897));
#45764=CARTESIAN_POINT('Ctrl Pts',(13.0524716430068,-0.563372759635625,
25.7283585071938));
#45765=CARTESIAN_POINT('Ctrl Pts',(13.0842282495084,-0.123916753765488,
25.5524875219252));
#45766=CARTESIAN_POINT('Ctrl Pts',(13.11598485601,0.343567325343907,25.6088632189223));
#45767=CARTESIAN_POINT('Ctrl Pts',(13.1477414625116,0.728549312681536,25.8817302414103));
#45768=CARTESIAN_POINT('Ctrl Pts',(13.1794980690132,0.935179034674501,26.305625168224));
#45769=CARTESIAN_POINT('Ctrl Pts',(13.2112546755148,0.914577064838846,26.7767496844913));
#45770=CARTESIAN_POINT('Ctrl Pts',(13.2430112820164,0.670212837001825,27.180424883989));
#45771=CARTESIAN_POINT('Ctrl Pts',(13.274767888518,0.263911977775921,27.4184147897098));
#45772=CARTESIAN_POINT('Ctrl Pts',(13.3065244950196,-0.209228031077641,
27.4322248069704));
#45773=CARTESIAN_POINT('Ctrl Pts',(13.3382811015212,-0.626782162306477,
27.2195185706328));
#45774=CARTESIAN_POINT('Ctrl Pts',(13.3806232435233,-0.990323889191508,
26.7005130761929));
#45775=CARTESIAN_POINT('Ctrl Pts',(13.4229653855255,-0.891350548436152,
26.0241417237977));
#45776=CARTESIAN_POINT('Ctrl Pts',(13.4653075275276,-0.394343245000318,
25.6310602681465));
#45777=CARTESIAN_POINT('Ctrl Pts',(13.4970641340292,0.0666496135424663,
25.5469117098955));
#45778=CARTESIAN_POINT('Ctrl Pts',(13.5288207405308,0.515995320900319,25.6957089539351));
#45779=CARTESIAN_POINT('Ctrl Pts',(13.5605773470324,0.837071203165268,26.040135813022));
#45780=CARTESIAN_POINT('Ctrl Pts',(13.592333953534,0.955527079936532,26.4969024359207));
#45781=CARTESIAN_POINT('Ctrl Pts',(13.6240905600356,0.840276516062167,26.9541770345109));
#45782=CARTESIAN_POINT('Ctrl Pts',(13.6558471665372,0.520853866128242,27.3010947793704));
#45783=CARTESIAN_POINT('Ctrl Pts',(13.6876037730388,0.0738299518903651,
27.452214475755));
#45784=CARTESIAN_POINT('Ctrl Pts',(13.7193603795403,-0.390206894582817,
27.3722808248444));
#45785=CARTESIAN_POINT('Ctrl Pts',(13.751116986042,-0.76084642148672,27.0778686551721));
#45786=CARTESIAN_POINT('Ctrl Pts',(13.7828735925435,-0.942982927868766,
26.646102875465));
#45787=CARTESIAN_POINT('Ctrl Pts',(13.8252157345457,-0.886393891964172,
26.0149713745393));
#45788=CARTESIAN_POINT('Ctrl Pts',(13.8675578765478,-0.374757199409084,
25.561648285173));
#45789=CARTESIAN_POINT('Ctrl Pts',(13.9099000185499,0.258595981805174,25.5814734785183));
#45790=CARTESIAN_POINT('Ctrl Pts',(13.9416566250515,0.665286358978002,25.8142788319751));
#45791=CARTESIAN_POINT('Ctrl Pts',(13.9734132315531,0.912922684959164,26.2176749581455));
#45792=CARTESIAN_POINT('Ctrl Pts',(14.0051698380547,0.936394173098453,26.6879606932866));
#45793=CARTESIAN_POINT('Ctrl Pts',(14.0369264445563,0.732542489799628,27.1135332884477));
#45794=CARTESIAN_POINT('Ctrl Pts',(14.0686830510579,0.349683692101816,27.3888547224382));
#45795=CARTESIAN_POINT('Ctrl Pts',(14.1004396575595,-0.118141955808618,
27.4482004396081));
#45796=CARTESIAN_POINT('Ctrl Pts',(14.1321962640611,-0.55731981727521,27.2756016315776));
#45797=CARTESIAN_POINT('Ctrl Pts',(14.1639528705627,-0.860575439144756,
26.9153855696964));
#45798=CARTESIAN_POINT('Ctrl Pts',(14.1957094770643,-0.954178525076913,
26.4513913382035));
#45799=CARTESIAN_POINT('Ctrl Pts',(14.2274660835659,-0.815128438364575,
26.0038866244089));
#45800=CARTESIAN_POINT('Ctrl Pts',(14.269808225568,-0.365056692386834,25.5578320157364));
#45801=CARTESIAN_POINT('Ctrl Pts',(14.3121503675701,0.318311140684575,25.5410292408296));
#45802=CARTESIAN_POINT('Ctrl Pts',(14.3544925095723,0.789761100866001,25.9644253030342));
#45803=CARTESIAN_POINT('Ctrl Pts',(14.3862491160739,0.950636516610815,26.4045553929986));
#45804=CARTESIAN_POINT('Ctrl Pts',(14.4180057225755,0.879950308795002,26.8725892000887));
#45805=CARTESIAN_POINT('Ctrl Pts',(14.4497623290771,0.594764564687753,27.2472739673141));
#45806=CARTESIAN_POINT('Ctrl Pts',(14.4815189355787,0.164600072175658,27.4412483262322));
#45807=CARTESIAN_POINT('Ctrl Pts',(14.5132755420803,-0.305576886172813,
27.4049663909559));
#45808=CARTESIAN_POINT('Ctrl Pts',(14.5450321485819,-0.701504155152511,
27.1487938930808));
#45809=CARTESIAN_POINT('Ctrl Pts',(14.5767887550835,-0.926024969152664,
26.7337542002603));
#45810=CARTESIAN_POINT('Ctrl Pts',(14.608545361585,-0.925694816580148,26.2628832259669));
#45811=CARTESIAN_POINT('Ctrl Pts',(14.6403019680866,-0.698183312328932,
25.8478040769025));
#45812=CARTESIAN_POINT('Ctrl Pts',(14.6720585745883,-0.303425995824808,
25.5952925790462));
#45813=CARTESIAN_POINT('Ctrl Pts',(14.7144007165904,0.328187482238224,25.5443641510859));
#45814=CARTESIAN_POINT('Ctrl Pts',(14.7567428585925,0.861485213777406,25.9719941992074));
#45815=CARTESIAN_POINT('Ctrl Pts',(14.7990850005946,0.949023869712233,26.5995818617395));
#45816=CARTESIAN_POINT('Ctrl Pts',(14.8308416070962,0.788327306949261,27.0397772844774));
#45817=CARTESIAN_POINT('Ctrl Pts',(14.8625982135978,0.432605044989158,27.3520493724081));
#45818=CARTESIAN_POINT('Ctrl Pts',(14.8943548200994,-0.0269425750032053,
27.4546922893193));
#45819=CARTESIAN_POINT('Ctrl Pts',(14.926111426601,-0.480853321388377,27.3257249413122));
#45820=CARTESIAN_POINT('Ctrl Pts',(14.9578680331026,-0.816939819939113,
26.9949249768607));
#45821=CARTESIAN_POINT('Ctrl Pts',(14.9896246396042,-0.954524630017393,
26.5438671412952));
#45822=CARTESIAN_POINT('Ctrl Pts',(15.0213812461058,-0.858660451344394,
26.0818307771601));
#45823=CARTESIAN_POINT('Ctrl Pts',(15.0531378526074,-0.554899994784753,
25.7220403263928));
#45824=CARTESIAN_POINT('Ctrl Pts',(15.084894459109,-0.113410176167132,25.5513390533698));
#45825=CARTESIAN_POINT('Ctrl Pts',(15.1166510656106,0.351161226478998,25.6127296660606));
#45826=CARTESIAN_POINT('Ctrl Pts',(15.1589932076127,0.866886572506035,25.9809098636687));
#45827=CARTESIAN_POINT('Ctrl Pts',(15.2013353496149,0.998981702436636,26.65159966169));
#45828=CARTESIAN_POINT('Ctrl Pts',(15.243677491617,0.661386674545668,27.1878448365762));
#45829=CARTESIAN_POINT('Ctrl Pts',(15.2754340981186,0.254790927614128,27.4208154228319));
#45830=CARTESIAN_POINT('Ctrl Pts',(15.3071907046202,-0.218456042209027,
27.4302753439674));
#45831=CARTESIAN_POINT('Ctrl Pts',(15.3389473111218,-0.635962324857501,
27.2125413609015));
#45832=CARTESIAN_POINT('Ctrl Pts',(15.3707039176234,-0.89987054313192,26.821363658491));
#45833=CARTESIAN_POINT('Ctrl Pts',(15.402460524125,-0.943601812261104,26.3518209798243));
#45834=CARTESIAN_POINT('Ctrl Pts',(15.4342171306266,-0.758054806041372,
25.9182831389474));
#45835=CARTESIAN_POINT('Ctrl Pts',(15.4659737371282,-0.386948543494837,
25.626825278469));
#45836=CARTESIAN_POINT('Ctrl Pts',(15.4977303436297,0.0771999380983128,
25.547542427439));
#45837=CARTESIAN_POINT('Ctrl Pts',(15.5294869501314,0.524768364500619,25.7016030916023));
#45838=CARTESIAN_POINT('Ctrl Pts',(15.5612435566329,0.840384916331581,26.0479866762213));
#45839=CARTESIAN_POINT('Ctrl Pts',(15.6035856986351,0.997364552198828,26.6618976505233));
#45840=CARTESIAN_POINT('Ctrl Pts',(15.6459278406372,0.666052840252209,27.25981610487));
#45841=CARTESIAN_POINT('Ctrl Pts',(15.6882699826393,0.0622992719753226,
27.4521983266014));
#45842=CARTESIAN_POINT('Ctrl Pts',(15.7200265891409,-0.39872774090838,27.3682370922448));
#45843=CARTESIAN_POINT('Ctrl Pts',(15.7517831956425,-0.766645114785282,
27.0704301236322));
#45844=CARTESIAN_POINT('Ctrl Pts',(15.7835398021441,-0.945504317446849,
26.6348512340428));
#45845=CARTESIAN_POINT('Ctrl Pts',(15.8152964086457,-0.895134341830607,
26.1656706631617));
#45846=CARTESIAN_POINT('Ctrl Pts',(15.8470530151473,-0.625917113840984,
25.7784952053356));
#45847=CARTESIAN_POINT('Ctrl Pts',(15.8788096216489,-0.204613280560773,
25.566632440668));
#45848=CARTESIAN_POINT('Ctrl Pts',(15.9105662281505,0.266979318749092,25.5830020103654));
#45849=CARTESIAN_POINT('Ctrl Pts',(15.9423228346521,0.672946044002942,25.821561439899));
#45850=CARTESIAN_POINT('Ctrl Pts',(15.9740794411537,0.91583092558663,26.2278361238909));
#45851=CARTESIAN_POINT('Ctrl Pts',(16.0058360476553,0.933867254621135,26.6960989628159));
#45852=CARTESIAN_POINT('Ctrl Pts',(16.0481781896574,0.658178704973912,27.2666470449604));
#45853=CARTESIAN_POINT('Ctrl Pts',(16.0905203316595,0.0194764504986447,
27.5102314423456));
#45854=CARTESIAN_POINT('Ctrl Pts',(16.1328624736617,-0.566125161298197,
27.2681569853983));
#45855=CARTESIAN_POINT('Ctrl Pts',(16.1646190801633,-0.864483573584741,
26.9068016847578));
#45856=CARTESIAN_POINT('Ctrl Pts',(16.1963756866649,-0.953817267616392,
26.4419665788703));
#45857=CARTESIAN_POINT('Ctrl Pts',(16.2281322931665,-0.809803720332871,
25.993659004061));
#45858=CARTESIAN_POINT('Ctrl Pts',(16.2598888996681,-0.468875017752602,
25.6674149814447));
#45859=CARTESIAN_POINT('Ctrl Pts',(16.2916455061697,-0.0134849969651525,
25.5449295539179));
#45860=CARTESIAN_POINT('Ctrl Pts',(16.3234021126713,0.445181635637873,25.6545090735637));
#45861=CARTESIAN_POINT('Ctrl Pts',(16.3551587191728,0.795185319036783,25.970997563312));
#45862=CARTESIAN_POINT('Ctrl Pts',(16.3869153256744,0.951798579107647,26.4150604757497));
#45863=CARTESIAN_POINT('Ctrl Pts',(16.418671932176,0.875624241768845,26.8822324514563));
#45864=CARTESIAN_POINT('Ctrl Pts',(16.4504285386776,0.587586952789248,27.2518672924014));
#45865=CARTESIAN_POINT('Ctrl Pts',(16.4927706806798,0.00905329884619842,
27.5103786107236));
#45866=CARTESIAN_POINT('Ctrl Pts',(16.5351128226819,-0.636271494686479,
27.2849238716444));
#45867=CARTESIAN_POINT('Ctrl Pts',(16.577454964684,-0.927958497882414,26.7223867772124));
#45868=CARTESIAN_POINT('Ctrl Pts',(16.6092115711856,-0.923149879585831,
26.2538013819286));
#45869=CARTESIAN_POINT('Ctrl Pts',(16.6409681776872,-0.691832222007586,
25.8408312548647));
#45870=CARTESIAN_POINT('Ctrl Pts',(16.6727247841888,-0.292762605847151,
25.5909052160247));
#45871=CARTESIAN_POINT('Ctrl Pts',(16.7044813906904,0.178179836603969,25.5612276414258));
#45872=CARTESIAN_POINT('Ctrl Pts',(16.736237997192,0.605297270682226,25.7611112287851));
#45873=CARTESIAN_POINT('Ctrl Pts',(16.7679946036936,0.885338350632903,26.140531503058));
#45874=CARTESIAN_POINT('Ctrl Pts',(16.7997512101952,0.948934678345878,26.6081029410621));
#45875=CARTESIAN_POINT('Ctrl Pts',(16.8315078166968,0.782444526026321,27.0485579474062));
#45876=CARTESIAN_POINT('Ctrl Pts',(16.8632644231984,0.423081836349496,27.3566336553455));
#45877=CARTESIAN_POINT('Ctrl Pts',(16.8950210297,-0.0353909079102747,27.4535776508021));
#45878=CARTESIAN_POINT('Ctrl Pts',(16.9373631717021,-0.644335349815601,
27.2783179660028));
#45879=CARTESIAN_POINT('Ctrl Pts',(16.9797053137042,-0.992396093030616,
26.6899918255381));
#45880=CARTESIAN_POINT('Ctrl Pts',(17.0220474557064,-0.852811656678332,
26.0718935521386));
#45881=CARTESIAN_POINT('Ctrl Pts',(17.0538040622079,-0.547100409593038,
25.7167372078641));
#45882=CARTESIAN_POINT('Ctrl Pts',(17.0855606687096,-0.104060012346944,
25.5501017044901));
#45883=CARTESIAN_POINT('Ctrl Pts',(17.1173172752111,0.36214184608273,25.6162485910021));
#45884=CARTESIAN_POINT('Ctrl Pts',(17.1490738817128,0.741328937838052,25.8971127788516));
#45885=CARTESIAN_POINT('Ctrl Pts',(17.1808304882143,0.939042104386864,26.3252392260279));
#45886=CARTESIAN_POINT('Ctrl Pts',(17.212587094716,0.908584923009143,26.7958293990439));
#45887=CARTESIAN_POINT('Ctrl Pts',(17.2443437012175,0.655826073959799,27.1943021173535));
#45888=CARTESIAN_POINT('Ctrl Pts',(17.2761003077192,0.244633534093608,27.4237368086484));
#45889=CARTESIAN_POINT('Ctrl Pts',(17.3078569142207,-0.228691868279225,
27.4276418979317));
#45890=CARTESIAN_POINT('Ctrl Pts',(17.3396135207224,-0.641703015565117,
27.206243646366));
#45891=CARTESIAN_POINT('Ctrl Pts',(17.3819556627244,-0.994303347678889,
26.6797436015688));
#45892=CARTESIAN_POINT('Ctrl Pts',(17.4242978047266,-0.88119652697226,26.0055916982066));
#45893=CARTESIAN_POINT('Ctrl Pts',(17.4666399467287,-0.376071662495523,
25.6229977451693));
#45894=CARTESIAN_POINT('Ctrl Pts',(17.4983965532303,0.0865813322721645,
25.5485152861257));
#45895=CARTESIAN_POINT('Ctrl Pts',(17.5301531597319,0.532714518507328,25.706683914095));
#45896=CARTESIAN_POINT('Ctrl Pts',(17.5619097662335,0.846512025133718,26.0577547633947));
#45897=CARTESIAN_POINT('Ctrl Pts',(17.5936663727351,0.955382466040536,26.5169005346908));
#45898=CARTESIAN_POINT('Ctrl Pts',(17.6254229792367,0.83058774652791,26.9716627557347));
#45899=CARTESIAN_POINT('Ctrl Pts',(17.6571795857383,0.503973842045383,27.3118201059033));
#45900=CARTESIAN_POINT('Ctrl Pts',(17.6889361922399,0.0538868825730616,
27.4535504471568));
#45901=CARTESIAN_POINT('Ctrl Pts',(17.7206927987415,-0.408378664397602,
27.3639246296828));
#45902=CARTESIAN_POINT('Ctrl Pts',(17.7524494052431,-0.772769571707759,
27.0618169554814));
#45903=CARTESIAN_POINT('Ctrl Pts',(17.7842060117447,-0.945840995106025,
26.6263398149854));
#45904=CARTESIAN_POINT('Ctrl Pts',(17.8265481537468,-0.876033313989953,
25.9965186109302));
#45905=CARTESIAN_POINT('Ctrl Pts',(17.868890295749,-0.355067658577955,25.5540272619233));
#45906=CARTESIAN_POINT('Ctrl Pts',(17.911232437751,0.277799571538731,25.5870664787881));
#45907=CARTESIAN_POINT('Ctrl Pts',(17.9429890442527,0.679413189226427,25.8283943842124));
#45908=CARTESIAN_POINT('Ctrl Pts',(17.9747456507543,0.918783490271958,26.2367603996339));
#45909=CARTESIAN_POINT('Ctrl Pts',(18.0065022572559,0.931965741123502,26.7076726814112));
#45910=CARTESIAN_POINT('Ctrl Pts',(18.0382588637574,0.720089129555561,27.1284344314988));
#45911=CARTESIAN_POINT('Ctrl Pts',(18.070015470259,0.329980493973673,27.396531794444));
#45912=CARTESIAN_POINT('Ctrl Pts',(18.1017720767607,-0.136099813986084,
27.4445088971166));
#45913=CARTESIAN_POINT('Ctrl Pts',(18.1441142187627,-0.723118632728979,
27.2057172991734));
#45914=CARTESIAN_POINT('Ctrl Pts',(18.1864563607649,-1.00692062085995,26.5838971968947));
#45915=CARTESIAN_POINT('Ctrl Pts',(18.228798502767,-0.802712071566496,25.984024935646));
#45916=CARTESIAN_POINT('Ctrl Pts',(18.2605551092686,-0.46111876429496,25.6632320586692));
#45917=CARTESIAN_POINT('Ctrl Pts',(18.2923117157702,-0.00293339983474069,
25.5444214870179));
#45918=CARTESIAN_POINT('Ctrl Pts',(18.3240683222718,0.453650294894908,25.6595455626102));
#45919=CARTESIAN_POINT('Ctrl Pts',(18.3558249287734,0.800977642610365,25.9789660914556));
#45920=CARTESIAN_POINT('Ctrl Pts',(18.387581535275,0.952265047855294,26.4256156033654));
#45921=CARTESIAN_POINT('Ctrl Pts',(18.4193381417766,0.87216829080666,26.8903380035327));
#45922=CARTESIAN_POINT('Ctrl Pts',(18.4510947482782,0.5786525270315,27.259818867202));
#45923=CARTESIAN_POINT('Ctrl Pts',(18.4828513547798,0.14548490939909,27.4444412694929));
#45924=CARTESIAN_POINT('Ctrl Pts',(18.5146079612814,-0.325594867448101,
27.3982246211978));
#45925=CARTESIAN_POINT('Ctrl Pts',(18.546364567783,-0.712851699124399,27.1343542428059));
#45926=CARTESIAN_POINT('Ctrl Pts',(18.5887067097851,-1.00774305370889,26.5734903104616));
#45927=CARTESIAN_POINT('Ctrl Pts',(18.6310488517872,-0.823914981229908,
25.9150974327161));
#45928=CARTESIAN_POINT('Ctrl Pts',(18.6733909937894,-0.281131390701923,
25.5881184345652));
#45929=CARTESIAN_POINT('Ctrl Pts',(18.705147600291,0.186806312460487,25.5630246198324));
#45930=CARTESIAN_POINT('Ctrl Pts',(18.7369042067926,0.613691803981374,25.7675263640368));
#45931=CARTESIAN_POINT('Ctrl Pts',(18.7686608132942,0.888566765767323,26.1498395050539));
#45932=CARTESIAN_POINT('Ctrl Pts',(18.8004174197958,0.948226890816592,26.6179294670152));
#45933=CARTESIAN_POINT('Ctrl Pts',(18.8321740262974,0.775997695356658,27.0569281629903));
#45934=CARTESIAN_POINT('Ctrl Pts',(18.863930632799,0.415215011861205,27.3606033287324));
#45935=CARTESIAN_POINT('Ctrl Pts',(18.8956872393005,-0.0473470204057584,
27.4538980706808));
#45936=CARTESIAN_POINT('Ctrl Pts',(18.9274438458022,-0.497525842623222,
27.3158451408842));
#45937=CARTESIAN_POINT('Ctrl Pts',(18.9592004523037,-0.827898992667679,
26.9768676102035));
#45938=CARTESIAN_POINT('Ctrl Pts',(18.9909570588054,-0.953893041314731,
26.5255130985628));
#45939=CARTESIAN_POINT('Ctrl Pts',(19.0332992008074,-0.817836948170601,
25.9066285940149));
#45940=CARTESIAN_POINT('Ctrl Pts',(19.0756413428097,-0.252913115286982,
25.5217455058419));
#45941=CARTESIAN_POINT('Ctrl Pts',(19.1179834848117,0.372830731701806,25.6216150627598));
#45942=CARTESIAN_POINT('Ctrl Pts',(19.1497400913134,0.746766015262565,25.904047000034));
#45943=CARTESIAN_POINT('Ctrl Pts',(19.1814966978149,0.94132513800925,26.3355547430818));
#45944=CARTESIAN_POINT('Ctrl Pts',(19.2132533043165,0.905053565889767,26.8050267406374));
#45945=CARTESIAN_POINT('Ctrl Pts',(19.2450099108181,0.648951079631192,27.2013587467485));
#45946=CARTESIAN_POINT('Ctrl Pts',(19.2767665173197,0.234309457401578,27.425980820695));
#45947=CARTESIAN_POINT('Ctrl Pts',(19.3085231238213,-0.237265150323603,
27.4256062034349));
#45948=CARTESIAN_POINT('Ctrl Pts',(19.3402797303229,-0.651050566510682,
27.1987821044357));
#45949=CARTESIAN_POINT('Ctrl Pts',(19.3720363368245,-0.906249282199466,
26.8030635188936));
#45950=CARTESIAN_POINT('Ctrl Pts',(19.4037929433261,-0.940341432747018,
26.3309513396123));
#45951=CARTESIAN_POINT('Ctrl Pts',(19.4355495498277,-0.745741510409131,
25.9046577017179));
#45952=CARTESIAN_POINT('Ctrl Pts',(19.4778916918298,-0.242807432967905,
25.5191883719474));
#45953=CARTESIAN_POINT('Ctrl Pts',(19.520233833832,0.437186765681122,25.5890583821446));
#45954=CARTESIAN_POINT('Ctrl Pts',(19.5625759758341,0.85122504747574,26.0687474394035));
#45955=CARTESIAN_POINT('Ctrl Pts',(19.5943325823357,0.955069962351073,26.5257065504164));
#45956=CARTESIAN_POINT('Ctrl Pts',(19.6260891888373,0.825683878714483,26.9810211953773));
#45957=CARTESIAN_POINT('Ctrl Pts',(19.6578457953389,0.495346232074199,27.3165753976231));
#45958=CARTESIAN_POINT('Ctrl Pts',(19.6896024018405,0.0440810433938132,
27.454514775689));
#45959=CARTESIAN_POINT('Ctrl Pts',(19.7213590083421,-0.417716245692366,
27.3589845983528));
#45960=CARTESIAN_POINT('Ctrl Pts',(19.7531156148437,-0.778015997201674,
27.0547366073134));
#45961=CARTESIAN_POINT('Ctrl Pts',(19.7848722213452,-0.948171228861939,
26.6146062406326));
#45962=CARTESIAN_POINT('Ctrl Pts',(19.8166288278469,-0.888215519416682,
26.1475678093043));
#45963=CARTESIAN_POINT('Ctrl Pts',(19.8483854343484,-0.609972510687159,
25.7646409068179));
#45964=CARTESIAN_POINT('Ctrl Pts',(19.88014204085,-0.186416668901866,25.5641518937206));
#45965=CARTESIAN_POINT('Ctrl Pts',(19.9224841828522,0.446561285406313,25.5936171241666));
#45966=CARTESIAN_POINT('Ctrl Pts',(19.9648263248543,0.921413268661259,26.0853381045205));
#45967=CARTESIAN_POINT('Ctrl Pts',(20.0071684668564,0.928773341115951,26.718958747949));
#45968=CARTESIAN_POINT('Ctrl Pts',(20.038925073358,0.713626810946046,27.1352607609624));
#45969=CARTESIAN_POINT('Ctrl Pts',(20.0706816798596,0.321224058095783,27.3999724231729));
#45970=CARTESIAN_POINT('Ctrl Pts',(20.1024382863612,-0.147622055815055,
27.4435947214087));
#45971=CARTESIAN_POINT('Ctrl Pts',(20.1341948928628,-0.5815469709462,27.2581851462398));
#45972=CARTESIAN_POINT('Ctrl Pts',(20.1659514993644,-0.873037333522926,
26.8874883435638));
#45973=CARTESIAN_POINT('Ctrl Pts',(20.197708105866,-0.952395320404333,26.4226388400605));
#45974=CARTESIAN_POINT('Ctrl Pts',(20.2294647123676,-0.798793439930978,
25.9764617397393));
#45975=CARTESIAN_POINT('Ctrl Pts',(20.2612213188692,-0.451916741041312,
25.6580341354082));
#45976=CARTESIAN_POINT('Ctrl Pts',(20.2929779253708,0.00763543851914112,
25.5446146537662));
#45977=CARTESIAN_POINT('Ctrl Pts',(20.3247345318724,0.460692690237073,25.6643415185417));
#45978=CARTESIAN_POINT('Ctrl Pts',(20.3670766738745,0.925642118779168,26.0948659886288));
#45979=CARTESIAN_POINT('Ctrl Pts',(20.4094188158766,0.97174177418587,26.7768841337632));
#45980=CARTESIAN_POINT('Ctrl Pts',(20.4517609578788,0.568957743322508,27.2660613152904));
#45981=CARTESIAN_POINT('Ctrl Pts',(20.4835175643804,0.136133317385707,27.4456675840998));
#45982=CARTESIAN_POINT('Ctrl Pts',(20.515274170882,-0.33450173652478,27.395122252116));
#45983=CARTESIAN_POINT('Ctrl Pts',(20.5470307773836,-0.721074398387512,
27.1262706935691));
#45984=CARTESIAN_POINT('Ctrl Pts',(20.5787873838852,-0.933321683296651,
26.7048224374515));
#45985=CARTESIAN_POINT('Ctrl Pts',(20.6105439903868,-0.917240887448331,
26.233521939898));
#45986=CARTESIAN_POINT('Ctrl Pts',(20.6423005968884,-0.678287047037146,
25.8269708199366));
#45987=CARTESIAN_POINT('Ctrl Pts',(20.67405720339,-0.273259928313006,25.584853956348));
#45988=CARTESIAN_POINT('Ctrl Pts',(20.7058138098915,0.197191832486415,25.5649862893134));
#45989=CARTESIAN_POINT('Ctrl Pts',(20.7375704163932,0.621647822525948,25.7744840150153));
#45990=CARTESIAN_POINT('Ctrl Pts',(20.7693270228947,0.890859616989826,26.1580467937161));
#45991=CARTESIAN_POINT('Ctrl Pts',(20.8116691648969,0.968833568572465,26.7868944329102));
#45992=CARTESIAN_POINT('Ctrl Pts',(20.854011306899,0.564472343796524,27.3380440754021));
#45993=CARTESIAN_POINT('Ctrl Pts',(20.8963534489011,-0.0587828278361782,
27.4524218769131));
#45994=CARTESIAN_POINT('Ctrl Pts',(20.9281100554027,-0.505466018590451,
27.3107549344715));
#45995=CARTESIAN_POINT('Ctrl Pts',(20.9598666619043,-0.832709033680724,
26.9687546513878));
#45996=CARTESIAN_POINT('Ctrl Pts',(20.9916232684059,-0.954969293592875,
26.5140327448572));
#45997=CARTESIAN_POINT('Ctrl Pts',(21.0233798749075,-0.845590667720455,
26.0550078449463));
#45998=CARTESIAN_POINT('Ctrl Pts',(21.0551364814091,-0.529511238559754,
25.7050413530494));
#45999=CARTESIAN_POINT('Ctrl Pts',(21.0868930879107,-0.0847700985191855,
25.5482355197884));
#46000=CARTESIAN_POINT('Ctrl Pts',(21.1186496944123,0.380953014904775,25.6241929036207));
#46001=CARTESIAN_POINT('Ctrl Pts',(21.1504063009139,0.753441811352533,25.9122409550869));
#46002=CARTESIAN_POINT('Ctrl Pts',(21.1821629074155,0.94292321815782,26.3460023884001));
#46003=CARTESIAN_POINT('Ctrl Pts',(21.2139195139171,0.901516409720417,26.8127794997692));
#46004=CARTESIAN_POINT('Ctrl Pts',(21.2562616559192,0.555796570644303,27.343822890948));
#46005=CARTESIAN_POINT('Ctrl Pts',(21.2986037979214,-0.108609863467862,
27.5045649788765));
#46006=CARTESIAN_POINT('Ctrl Pts',(21.3409459399235,-0.658842278969386,
27.1902823363766));
#46007=CARTESIAN_POINT('Ctrl Pts',(21.3727025464251,-0.909038943717463,
26.7940538360991));
#46008=CARTESIAN_POINT('Ctrl Pts',(21.4044591529267,-0.938789589811806,
26.3216482014888));
#46009=CARTESIAN_POINT('Ctrl Pts',(21.4362157594283,-0.739164495713174,
25.8951867082226));
#46010=CARTESIAN_POINT('Ctrl Pts',(21.4679723659299,-0.359666886889135,
25.6147422263144));
#46011=CARTESIAN_POINT('Ctrl Pts',(21.4997289724315,0.107567832412902,25.5509106661896));
#46012=CARTESIAN_POINT('Ctrl Pts',(21.5314855789331,0.548665502402203,25.7176907504899));
#46013=CARTESIAN_POINT('Ctrl Pts',(21.5632421854347,0.855773327352228,26.0759536796221));
#46014=CARTESIAN_POINT('Ctrl Pts',(21.5949987919363,0.954892370388148,26.5362742187471));
#46015=CARTESIAN_POINT('Ctrl Pts',(21.6267553984379,0.82017147631701,26.9900389873832));
#46016=CARTESIAN_POINT('Ctrl Pts',(21.6585120049394,0.487644732810762,27.3202228154794));
#46017=CARTESIAN_POINT('Ctrl Pts',(21.7008541469416,-0.118967740312026,
27.5033910384256));
#46018=CARTESIAN_POINT('Ctrl Pts',(21.7431962889437,-0.730547156864122,
27.1980313394293));
#46019=CARTESIAN_POINT('Ctrl Pts',(21.7855384309458,-0.948649690972304,
26.6030854804968));
#46020=CARTESIAN_POINT('Ctrl Pts',(21.8172950374474,-0.88454100129426,26.1388813536399));
#46021=CARTESIAN_POINT('Ctrl Pts',(21.849051643949,-0.602789554197912,25.7585284824614));
#46022=CARTESIAN_POINT('Ctrl Pts',(21.8808082504506,-0.175283535498467,
25.5611501974135));
#46023=CARTESIAN_POINT('Ctrl Pts',(21.9125648569522,0.295625783321212,25.5913488063999));
#46024=CARTESIAN_POINT('Ctrl Pts',(21.9443214634538,0.693992687018111,25.8437107707054));
#46025=CARTESIAN_POINT('Ctrl Pts',(21.9760780699554,0.923731845074089,26.2555392182961));
#46026=CARTESIAN_POINT('Ctrl Pts',(22.007834676457,0.927605810512738,26.7273999338973));
#46027=CARTESIAN_POINT('Ctrl Pts',(22.0395912829586,0.706679459850598,27.1432257760666));
#46028=CARTESIAN_POINT('Ctrl Pts',(22.0713478894602,0.311196990298509,27.4033138396751));
#46029=CARTESIAN_POINT('Ctrl Pts',(22.1031044959618,-0.155861224646809,
27.4414192111503));
#46030=CARTESIAN_POINT('Ctrl Pts',(22.1454466379639,-0.737709562729427,
27.1904574572595));
#46031=CARTESIAN_POINT('Ctrl Pts',(22.1877887799661,-1.00846623477415,26.5627913413472));
#46032=CARTESIAN_POINT('Ctrl Pts',(22.2301309219682,-0.791733341554092,
25.9673451696054));
#46033=CARTESIAN_POINT('Ctrl Pts',(22.2618875284698,-0.443508391765042,
25.6537614011678));
#46034=CARTESIAN_POINT('Ctrl Pts',(22.2936441349714,0.0170670193553443,
25.5445713135867));
#46035=CARTESIAN_POINT('Ctrl Pts',(22.3254007414729,0.471139295586204,25.6692226328383));
#46036=CARTESIAN_POINT('Ctrl Pts',(22.3571573479746,0.811706831839087,25.9958436606161));
#46037=CARTESIAN_POINT('Ctrl Pts',(22.3889139544761,0.953613004085633,26.4455606708209));
#46038=CARTESIAN_POINT('Ctrl Pts',(22.4206705609778,0.863808361361245,26.9085054592507));
#46039=CARTESIAN_POINT('Ctrl Pts',(22.4524271674793,0.562624198088996,27.2717624513788));
#46040=CARTESIAN_POINT('Ctrl Pts',(22.484183773981,0.125687748636954,27.4472791815583));
#46041=CARTESIAN_POINT('Ctrl Pts',(22.5159403804825,-0.34432167464298,27.3912138038039));
#46042=CARTESIAN_POINT('Ctrl Pts',(22.5476969869841,-0.725971372042429,
27.1192967135759));
#46043=CARTESIAN_POINT('Ctrl Pts',(22.5900391289863,-1.00906035784248,26.5523840954732));
#46044=CARTESIAN_POINT('Ctrl Pts',(22.6323812709884,-0.811493649352943,
25.8979825946971));
#46045=CARTESIAN_POINT('Ctrl Pts',(22.6747234129905,-0.261985904172254,
25.5824346135091));
#46046=CARTESIAN_POINT('Ctrl Pts',(22.7064800194921,0.206374480275771,25.567139327868));
#46047=CARTESIAN_POINT('Ctrl Pts',(22.7382366259937,0.628886650341483,25.7805301681145));
#46048=CARTESIAN_POINT('Ctrl Pts',(22.7699932324953,0.895700336928616,26.1685121781128));
#46049=CARTESIAN_POINT('Ctrl Pts',(22.8017498389969,0.945551178504746,26.6377481913622));
#46050=CARTESIAN_POINT('Ctrl Pts',(22.8335064454985,0.764172311405064,27.0730463162821));
#46051=CARTESIAN_POINT('Ctrl Pts',(22.8652630520001,0.397113311698903,27.3691044891535));
#46052=CARTESIAN_POINT('Ctrl Pts',(22.8970196585017,-0.0672998903916815,
27.4526982703809));
#46053=CARTESIAN_POINT('Ctrl Pts',(22.9287762650033,-0.514490935776569,
27.3052542051893));
#46054=CARTESIAN_POINT('Ctrl Pts',(22.9605328715049,-0.837697585415996,
26.9594368456141));
#46055=CARTESIAN_POINT('Ctrl Pts',(22.9922894780065,-0.954218063318174,
26.5055443762862));
#46056=CARTESIAN_POINT('Ctrl Pts',(23.0346316200086,-0.805239714176764,
25.8896428079065));
#46057=CARTESIAN_POINT('Ctrl Pts',(23.0769737620108,-0.232384750750894,
25.5166667773099));
#46058=CARTESIAN_POINT('Ctrl Pts',(23.1193159040128,0.391131971913022,25.629610068407));
#46059=CARTESIAN_POINT('Ctrl Pts',(23.1510725105145,0.759074604071942,25.9198058900914));
#46060=CARTESIAN_POINT('Ctrl Pts',(23.1828291170161,0.944560493665858,26.3552908718259));
#46061=CARTESIAN_POINT('Ctrl Pts',(23.2145857235177,0.898471725645074,26.823900953765));
#46062=CARTESIAN_POINT('Ctrl Pts',(23.2463423300193,0.634130868366591,27.2147864276691));
#46063=CARTESIAN_POINT('Ctrl Pts',(23.2780989365208,0.214879154138892,27.4306816594514));
#46064=CARTESIAN_POINT('Ctrl Pts',(23.3098555430225,-0.25658433122915,27.420437980726));
#46065=CARTESIAN_POINT('Ctrl Pts',(23.3416121495241,-0.665532132593269,
27.1850038321932));
#46066=CARTESIAN_POINT('Ctrl Pts',(23.3733687560256,-0.912393331867455,
26.7840311002954));
#46067=CARTESIAN_POINT('Ctrl Pts',(23.4051253625272,-0.936597621847152,
26.3113088383897));
#46068=CARTESIAN_POINT('Ctrl Pts',(23.4368819690288,-0.733118819505304,
25.8891811651903));
#46069=CARTESIAN_POINT('Ctrl Pts',(23.479224111031,-0.222227765874648,25.5143216958347));
#46070=CARTESIAN_POINT('Ctrl Pts',(23.5215662530331,0.456155259187886,25.5984073654122));
#46071=CARTESIAN_POINT('Ctrl Pts',(23.5639083950352,0.860063896779621,26.0866563827427));
#46072=CARTESIAN_POINT('Ctrl Pts',(23.5956650015368,0.954322798502375,26.5456886854505));
#46073=CARTESIAN_POINT('Ctrl Pts',(23.6274216080384,0.815436198503803,26.9981958090358));
#46074=CARTESIAN_POINT('Ctrl Pts',(23.65917821454,0.478148401286439,27.3267631922024));
#46075=CARTESIAN_POINT('Ctrl Pts',(23.6909348210416,0.0240952427481605,
27.455228252656));
#46076=CARTESIAN_POINT('Ctrl Pts',(23.7226914275432,-0.43560164372991,27.3500544747853));
#46077=CARTESIAN_POINT('Ctrl Pts',(23.7544480340448,-0.789455162469809,
27.0383327426834));
#46078=CARTESIAN_POINT('Ctrl Pts',(23.7862046405464,-0.950362050999274,
26.5947377519997));
#46079=CARTESIAN_POINT('Ctrl Pts',(23.817961247048,-0.880645262685305,26.1290563664367));
#46080=CARTESIAN_POINT('Ctrl Pts',(23.8497178535496,-0.594449274927437,
25.7520364184949));
#46081=CARTESIAN_POINT('Ctrl Pts',(23.8814744600511,-0.166790351739,25.5604555193937));
#46082=CARTESIAN_POINT('Ctrl Pts',(23.9238166020534,0.465432320099869,25.6031612995448));
#46083=CARTESIAN_POINT('Ctrl Pts',(23.9661587440554,0.929889535128502,26.1047123178162));
#46084=CARTESIAN_POINT('Ctrl Pts',(24.0085008860576,0.923987542311717,26.7383482203077));
#46085=CARTESIAN_POINT('Ctrl Pts',(24.0402574925592,0.700175737535662,27.1500564562298));
#46086=CARTESIAN_POINT('Ctrl Pts',(24.0720140990608,0.302319024557154,27.4064979124974));
#46087=CARTESIAN_POINT('Ctrl Pts',(24.1037707055624,-0.167337334837971,
27.440298615336));
#46088=CARTESIAN_POINT('Ctrl Pts',(24.135527312064,-0.597286950075481,27.2458484394733));
#46089=CARTESIAN_POINT('Ctrl Pts',(24.1672839185655,-0.880955505259544,
26.869132496369));
#46090=CARTESIAN_POINT('Ctrl Pts',(24.1990405250672,-0.950567711377221,
26.4027239932854));
#46091=CARTESIAN_POINT('Ctrl Pts',(24.2307971315687,-0.787661849304617,
25.9598592028151));
#46092=CARTESIAN_POINT('Ctrl Pts',(24.2625537380703,-0.434197048688617,
25.6487607969077));
#46093=CARTESIAN_POINT('Ctrl Pts',(24.294310344572,0.0276281317882825,25.5449836933049));
#46094=CARTESIAN_POINT('Ctrl Pts',(24.3260669510735,0.478080505285049,25.674165947095));
#46095=CARTESIAN_POINT('Ctrl Pts',(24.3684090930757,0.933918058893733,26.1143266168117));
#46096=CARTESIAN_POINT('Ctrl Pts',(24.4107512350778,0.965734298436713,26.7971601656526));
#46097=CARTESIAN_POINT('Ctrl Pts',(24.45309337708,0.552800952384084,27.2778007196669));
#46098=CARTESIAN_POINT('Ctrl Pts',(24.4848499835815,0.116312510417921,27.4483094746125));
#46099=CARTESIAN_POINT('Ctrl Pts',(24.5166065900832,-0.353161650990287,
27.3879257323904));
#46100=CARTESIAN_POINT('Ctrl Pts',(24.5483631965847,-0.734023104698332,
27.1110428392531));
#46101=CARTESIAN_POINT('Ctrl Pts',(24.5801198030863,-0.937403808050388,
26.685244962274));
#46102=CARTESIAN_POINT('Ctrl Pts',(24.6118764095879,-0.911463127234907,
26.2143842269519));
#46103=CARTESIAN_POINT('Ctrl Pts',(24.6436330160895,-0.664053293709996,
25.8129229893904));
#46104=CARTESIAN_POINT('Ctrl Pts',(24.6753896225911,-0.254047845183442,
25.5793355866597));
#46105=CARTESIAN_POINT('Ctrl Pts',(24.7071462290927,0.216716670998938,25.5693179154607));
#46106=CARTESIAN_POINT('Ctrl Pts',(24.7389028355943,0.636695316637121,25.7876527998988));
#46107=CARTESIAN_POINT('Ctrl Pts',(24.7706594420959,0.897820923101191,26.1767656538782));
#46108=CARTESIAN_POINT('Ctrl Pts',(24.813001584098,0.962617233586659,26.8071074092719));
#46109=CARTESIAN_POINT('Ctrl Pts',(24.8553437261002,0.546810075430422,27.3496738436809));
#46110=CARTESIAN_POINT('Ctrl Pts',(24.8976858681022,-0.0787022993379347,
27.4509830705907));
#46111=CARTESIAN_POINT('Ctrl Pts',(24.9294424746039,-0.522322844544992,
27.2999989411156));
#46112=CARTESIAN_POINT('Ctrl Pts',(24.9611990811055,-0.842336784437806,
26.9512249988135));
#46113=CARTESIAN_POINT('Ctrl Pts',(24.9929556876071,-0.955053818302088,
26.4940440130873));
#46114=CARTESIAN_POINT('Ctrl Pts',(25.0247122941086,-0.836092645663481,
26.0374087298028));
#46115=CARTESIAN_POINT('Ctrl Pts',(25.0564689006103,-0.512758321830771,
25.6941338166197));
#46116=CARTESIAN_POINT('Ctrl Pts',(25.0882255071118,-0.0648329446824077,
25.5466698973183));
#46117=CARTESIAN_POINT('Ctrl Pts',(25.1199821136134,0.399198526988075,25.6323573283407));
#46118=CARTESIAN_POINT('Ctrl Pts',(25.151738720115,0.765577454441822,25.9281377620251));
#46119=CARTESIAN_POINT('Ctrl Pts',(25.1834953266166,0.945939574820729,26.3657696736668));
#46120=CARTESIAN_POINT('Ctrl Pts',(25.2152519331182,0.894773093931002,26.831577989089));
#46121=CARTESIAN_POINT('Ctrl Pts',(25.2575940751203,0.538015262989621,27.3552698264395));
#46122=CARTESIAN_POINT('Ctrl Pts',(25.2999362171226,-0.129609676224257,
27.5020719690006));
#46123=CARTESIAN_POINT('Ctrl Pts',(25.3422783591246,-0.673144254854347,
27.1763428602625));
#46124=CARTESIAN_POINT('Ctrl Pts',(25.3740349656263,-0.914993827187637,
26.7749650085504));
#46125=CARTESIAN_POINT('Ctrl Pts',(25.4057915721278,-0.934851422122379,
26.3020402148696));
#46126=CARTESIAN_POINT('Ctrl Pts',(25.4375481786294,-0.726345035721426,
25.8798498901769));
#46127=CARTESIAN_POINT('Ctrl Pts',(25.469304785131,-0.341061382887417,25.6074089802713));
#46128=CARTESIAN_POINT('Ctrl Pts',(25.5010613916326,0.127406875554477,25.5533697183237));
#46129=CARTESIAN_POINT('Ctrl Pts',(25.5328179981342,0.564917553857126,25.7293445953454));
#46130=CARTESIAN_POINT('Ctrl Pts',(25.5645746046358,0.864460367880076,26.0939562313707));
#46131=CARTESIAN_POINT('Ctrl Pts',(25.5963312111374,0.953924084549553,26.5562503226398));
#46132=CARTESIAN_POINT('Ctrl Pts',(25.628087817639,0.809736278571705,27.0070962620883));
#46133=CARTESIAN_POINT('Ctrl Pts',(25.6598444241406,0.470372255221548,27.3302486337547));
#46134=CARTESIAN_POINT('Ctrl Pts',(25.7021865661427,-0.139940715869016,
27.5006815153371));
#46135=CARTESIAN_POINT('Ctrl Pts',(25.7445287081448,-0.744995600564553,
27.1825895219264));
#46136=CARTESIAN_POINT('Ctrl Pts',(25.786870850147,-0.950599300264946,26.5832095017703));
#46137=CARTESIAN_POINT('Ctrl Pts',(25.8186274566486,-0.876789760428042,
26.1204487138737));
#46138=CARTESIAN_POINT('Ctrl Pts',(25.8503840631502,-0.587139966938427,
25.7460756580744));
#46139=CARTESIAN_POINT('Ctrl Pts',(25.8821406696517,-0.155596843591253,
25.5576874757268));
#46140=CARTESIAN_POINT('Ctrl Pts',(25.9138972761533,0.314577359308573,25.5977346901905));
#46141=CARTESIAN_POINT('Ctrl Pts',(25.945653882655,0.707575530836875,25.8583784328245));
#46142=CARTESIAN_POINT('Ctrl Pts',(25.9774104891565,0.928645668614596,26.2749246761696));
#46143=CARTESIAN_POINT('Ctrl Pts',(26.0091670956582,0.922643525462191,26.7467631270934));
#46144=CARTESIAN_POINT('Ctrl Pts',(26.0409237021597,0.693063374361549,27.157874325207));
#46145=CARTESIAN_POINT('Ctrl Pts',(26.0726803086614,0.292223927478923,27.4096287632192));
#46146=CARTESIAN_POINT('Ctrl Pts',(26.1044369151629,-0.175528640725272,
27.4379511281708));
#46147=CARTESIAN_POINT('Ctrl Pts',(26.146779057165,-0.751999129248255,27.1748674565358));
#46148=CARTESIAN_POINT('Ctrl Pts',(26.1891211991672,-1.00955714772251,26.541672240212));
#46149=CARTESIAN_POINT('Ctrl Pts',(26.2314633411693,-0.780415343064855,
25.9508925097247));
#46150=CARTESIAN_POINT('Ctrl Pts',(26.2632199476709,-0.425695156036877,
25.6446647035882));
#46151=CARTESIAN_POINT('Ctrl Pts',(26.2949765541725,0.0370469523678254,
25.5451382646459));
#46152=CARTESIAN_POINT('Ctrl Pts',(26.3267331606741,0.488444757764112,25.6792636247976));
#46153=CARTESIAN_POINT('Ctrl Pts',(26.3584897671757,0.822038272830759,26.0129434951272));
#46154=CARTESIAN_POINT('Ctrl Pts',(26.3902463736773,0.954622403718847,26.4655254939658));
#46155=CARTESIAN_POINT('Ctrl Pts',(26.4220029801789,0.854921065716908,26.926507465775));
#46156=CARTESIAN_POINT('Ctrl Pts',(26.44317405118,0.649394243932496,27.1643710019258));
#46157=CARTESIAN_POINT('Ctrl Pts',(26.4537595866805,0.524425129394093,27.2515709455267));
#46158=CARTESIAN_POINT('Ctrl Pts',(9.57962246391563,0.728031715487703,26.0801881597144));
#46159=CARTESIAN_POINT('Ctrl Pts',(9.59020799941616,0.797836853998554,26.2012432369256));
#46160=CARTESIAN_POINT('Ctrl Pts',(9.61137907041722,0.875864683195867,26.4787529255437));
#46161=CARTESIAN_POINT('Ctrl Pts',(9.64313567691882,0.779159006304305,26.9003050292651));
#46162=CARTESIAN_POINT('Ctrl Pts',(9.67489228342041,0.492867289945966,27.224442625857));
#46163=CARTESIAN_POINT('Ctrl Pts',(9.70664888992201,0.0859807399742794,
27.3715979059481));
#46164=CARTESIAN_POINT('Ctrl Pts',(9.73840549642361,-0.341017042102029,
27.3072046007951));
#46165=CARTESIAN_POINT('Ctrl Pts',(9.7701621029252,-0.686461153906695,27.0444034153001));
#46166=CARTESIAN_POINT('Ctrl Pts',(9.8019187094268,-0.861740140000044,26.6520453792238));
#46167=CARTESIAN_POINT('Ctrl Pts',(9.84426085142894,-0.821966507686613,
26.0723301549197));
#46168=CARTESIAN_POINT('Ctrl Pts',(9.88660299343105,-0.361592605867576,
25.6468958191038));
#46169=CARTESIAN_POINT('Ctrl Pts',(9.9289451354332,0.21945754392555,25.6529176835553));
#46170=CARTESIAN_POINT('Ctrl Pts',(9.96070174193477,0.596784937752111,25.8585520317075));
#46171=CARTESIAN_POINT('Ctrl Pts',(9.99245834843639,0.83156396088418,26.2236397271795));
#46172=CARTESIAN_POINT('Ctrl Pts',(10.024214954938,0.862108231736756,26.6543546166019));
#46173=CARTESIAN_POINT('Ctrl Pts',(10.0559715614396,0.683381197966278,27.048438593038));
#46174=CARTESIAN_POINT('Ctrl Pts',(10.0877281679412,0.33765390579586,27.3082052250863));
#46175=CARTESIAN_POINT('Ctrl Pts',(10.1194847744428,-0.0901171345344043,
27.3715925602575));
#46176=CARTESIAN_POINT('Ctrl Pts',(10.1512413809444,-0.496074810183009,
27.2217796506413));
#46177=CARTESIAN_POINT('Ctrl Pts',(10.182997987446,-0.781017425513611,26.8973477344617));
#46178=CARTESIAN_POINT('Ctrl Pts',(10.2147545939475,-0.875738920008686,
26.4737468123648));
#46179=CARTESIAN_POINT('Ctrl Pts',(10.2465112004492,-0.756843821637242,
26.0607988091448));
#46180=CARTESIAN_POINT('Ctrl Pts',(10.2888533424513,-0.352771292143462,
25.6432113471481));
#46181=CARTESIAN_POINT('Ctrl Pts',(10.3311954844534,0.273428740668571,25.6146915210074));
#46182=CARTESIAN_POINT('Ctrl Pts',(10.3735376264555,0.713787120522742,25.993819988321));
#46183=CARTESIAN_POINT('Ctrl Pts',(10.4052942329571,0.869726967162744,26.3942508345048));
#46184=CARTESIAN_POINT('Ctrl Pts',(10.4370508394587,0.813902944274307,26.8247082405763));
#46185=CARTESIAN_POINT('Ctrl Pts',(10.4688074459603,0.559630837018874,27.1736983051843));
#46186=CARTESIAN_POINT('Ctrl Pts',(10.5005640524619,0.168971823752622,27.3597925356327));
#46187=CARTESIAN_POINT('Ctrl Pts',(10.5323206589635,-0.262790191883949,
27.3355520272775));
#46188=CARTESIAN_POINT('Ctrl Pts',(10.5640772654651,-0.630698915625386,
27.1082873986829));
#46189=CARTESIAN_POINT('Ctrl Pts',(10.5958338719667,-0.844508356187008,
26.7320812711984));
#46190=CARTESIAN_POINT('Ctrl Pts',(10.6275904784683,-0.853242333262068,
26.3003729351923));
#46191=CARTESIAN_POINT('Ctrl Pts',(10.6593470849699,-0.652622110674877,
25.9154555072938));
#46192=CARTESIAN_POINT('Ctrl Pts',(10.6911036914715,-0.295548368443942,
25.6763730093826));
#46193=CARTESIAN_POINT('Ctrl Pts',(10.7334458334736,0.282547528974645,25.6175594789554));
#46194=CARTESIAN_POINT('Ctrl Pts',(10.7757879754757,0.779690185968125,25.9993827877349));
#46195=CARTESIAN_POINT('Ctrl Pts',(10.8181301174779,0.871991294827471,26.5730851524473));
#46196=CARTESIAN_POINT('Ctrl Pts',(10.8498867239795,0.733110089580741,26.9797473083307));
#46197=CARTESIAN_POINT('Ctrl Pts',(10.8816433304811,0.412971194829101,27.2728701291382));
#46198=CARTESIAN_POINT('Ctrl Pts',(10.9133999369827,-0.00637951398688148,
27.3757941435716));
#46199=CARTESIAN_POINT('Ctrl Pts',(10.9451565434843,-0.425007169196209,
27.2662660032243));
#46200=CARTESIAN_POINT('Ctrl Pts',(10.9769131499859,-0.739485127094044,
26.9694332988216));
#46201=CARTESIAN_POINT('Ctrl Pts',(11.0086697564875,-0.874281494321734,
26.5585367427531));
#46202=CARTESIAN_POINT('Ctrl Pts',(11.0404263629891,-0.795258808089696,
26.133094687598));
#46203=CARTESIAN_POINT('Ctrl Pts',(11.0721829694907,-0.523671266346352,
25.7974034948309));
#46204=CARTESIAN_POINT('Ctrl Pts',(11.1039395759923,-0.122182371218882,
25.6324290510517));
#46205=CARTESIAN_POINT('Ctrl Pts',(11.1356961824939,0.304922252090156,25.6797971726802));
#46206=CARTESIAN_POINT('Ctrl Pts',(11.178038324496,0.78481334152642,26.0074531511894));
#46207=CARTESIAN_POINT('Ctrl Pts',(11.2203804664981,0.918791724237265,26.6198171389421));
#46208=CARTESIAN_POINT('Ctrl Pts',(11.2627226085002,0.619570519816269,27.1179341621384));
#46209=CARTESIAN_POINT('Ctrl Pts',(11.2944792150018,0.251268099081413,27.3393284373114));
#46210=CARTESIAN_POINT('Ctrl Pts',(11.3262358215034,-0.182430702348097,
27.3570837083467));
#46211=CARTESIAN_POINT('Ctrl Pts',(11.357992428005,-0.569385720753886,27.1654742527812));
#46212=CARTESIAN_POINT('Ctrl Pts',(11.3897490345066,-0.818848215492295,
26.8119010765462));
#46213=CARTESIAN_POINT('Ctrl Pts',(11.4215056410082,-0.867952913083958,
26.3822561428148));
#46214=CARTESIAN_POINT('Ctrl Pts',(11.4532622475098,-0.706160657734097,
25.9812208494608));
#46215=CARTESIAN_POINT('Ctrl Pts',(11.4850188540114,-0.371518012659009,
25.706885603218));
#46216=CARTESIAN_POINT('Ctrl Pts',(11.516775460513,0.0524991512842034,25.6252901718929));
#46217=CARTESIAN_POINT('Ctrl Pts',(11.5485320670146,0.46579364213261,25.7579459815859));
#46218=CARTESIAN_POINT('Ctrl Pts',(11.5802886735162,0.761803498494695,26.0694588434954));
#46219=CARTESIAN_POINT('Ctrl Pts',(11.6226308155183,0.917506727842895,26.6292895342794));
#46220=CARTESIAN_POINT('Ctrl Pts',(11.6649729575205,0.625229763092544,27.183829015657));
#46221=CARTESIAN_POINT('Ctrl Pts',(11.7073150995226,0.0753909683970407,
27.3717949642245));
#46222=CARTESIAN_POINT('Ctrl Pts',(11.7390717060242,-0.348897263485596,
27.3036657158471));
#46223=CARTESIAN_POINT('Ctrl Pts',(11.7708283125258,-0.691925092963921,
27.0376923934737));
#46224=CARTESIAN_POINT('Ctrl Pts',(11.8025849190274,-0.86426541749805,26.6417792940806));
#46225=CARTESIAN_POINT('Ctrl Pts',(11.834341525529,-0.827089647580133,26.2106604133007));
#46226=CARTESIAN_POINT('Ctrl Pts',(11.8660981320305,-0.58769744352536,25.8505251428195));
#46227=CARTESIAN_POINT('Ctrl Pts',(11.8978547385322,-0.205505326914698,
25.6482005857156));
#46228=CARTESIAN_POINT('Ctrl Pts',(11.9296113450337,0.22717242501594,25.654157952437));
#46229=CARTESIAN_POINT('Ctrl Pts',(11.9613679515354,0.603947462792471,25.8650819687084));
#46230=CARTESIAN_POINT('Ctrl Pts',(11.9931245580369,0.834425159997837,26.2328997647731));
#46231=CARTESIAN_POINT('Ctrl Pts',(12.0248811645385,0.859947765854294,26.66186444256));
#46232=CARTESIAN_POINT('Ctrl Pts',(12.0672233065407,0.61814172580837,27.1902428457621));
#46233=CARTESIAN_POINT('Ctrl Pts',(12.1095654485428,0.0372440603084071,
27.4258224771968));
#46234=CARTESIAN_POINT('Ctrl Pts',(12.1519075905449,-0.504290557354765,
27.2151232701611));
#46235=CARTESIAN_POINT('Ctrl Pts',(12.1836641970465,-0.784765204805277,
26.8895528932284));
#46236=CARTESIAN_POINT('Ctrl Pts',(12.2154208035481,-0.875588586155747,
26.465099110808));
#46237=CARTESIAN_POINT('Ctrl Pts',(12.2471774100497,-0.752158318331058,
26.0513197750307));
#46238=CARTESIAN_POINT('Ctrl Pts',(12.2789340165513,-0.445850534936249,
25.7456711711312));
#46239=CARTESIAN_POINT('Ctrl Pts',(12.3106906230529,-0.0306923844737817,
25.624635017395));
#46240=CARTESIAN_POINT('Ctrl Pts',(12.3424472295545,0.39192346359699,25.7162968162322));
#46241=CARTESIAN_POINT('Ctrl Pts',(12.3742038360561,0.718886260937855,25.9997414429039));
#46242=CARTESIAN_POINT('Ctrl Pts',(12.4059604425577,0.870993971562706,26.4038597598608));
#46243=CARTESIAN_POINT('Ctrl Pts',(12.4377170490593,0.810121804594295,26.833632350075));
#46244=CARTESIAN_POINT('Ctrl Pts',(12.4694736555609,0.553138440497928,27.1780472869989));
#46245=CARTESIAN_POINT('Ctrl Pts',(12.511815797563,0.0276907734253708,27.4261574382243));
#46246=CARTESIAN_POINT('Ctrl Pts',(12.5541579395651,-0.568280051932768,
27.2318416234996));
#46247=CARTESIAN_POINT('Ctrl Pts',(12.5965000815673,-0.846499202680308,
26.721696544007));
#46248=CARTESIAN_POINT('Ctrl Pts',(12.6282566880689,-0.851083387706002,
26.2919977152372));
#46249=CARTESIAN_POINT('Ctrl Pts',(12.6600132945705,-0.646933148147585,
25.9089408269044));
#46250=CARTESIAN_POINT('Ctrl Pts',(12.6917699010721,-0.28585620245073,25.6721459599461));
#46251=CARTESIAN_POINT('Ctrl Pts',(12.7235265075737,0.145341766849772,25.6358990496622));
#46252=CARTESIAN_POINT('Ctrl Pts',(12.7552831140753,0.540765867963709,25.8109585271689));
#46253=CARTESIAN_POINT('Ctrl Pts',(12.7870397205769,0.804793585599763,26.153442694287));
#46254=CARTESIAN_POINT('Ctrl Pts',(12.8187963270785,0.872073054078602,26.5808991252308));
#46255=CARTESIAN_POINT('Ctrl Pts',(12.85055293358,0.727885175530364,26.9879104585021));
#46256=CARTESIAN_POINT('Ctrl Pts',(12.8823095400817,0.404328144390558,27.2772558362273));
#46257=CARTESIAN_POINT('Ctrl Pts',(12.9140661465832,-0.014146471449928,
27.3749343604572));
#46258=CARTESIAN_POINT('Ctrl Pts',(12.9564082885854,-0.575799899076613,
27.2259399806695));
#46259=CARTESIAN_POINT('Ctrl Pts',(12.9987504305875,-0.906198318985923,
26.6932329836706));
#46260=CARTESIAN_POINT('Ctrl Pts',(13.0410925725896,-0.790087249211633,
26.1238718351462));
#46261=CARTESIAN_POINT('Ctrl Pts',(13.0728491790912,-0.516622256749178,
25.7923918265544));
#46262=CARTESIAN_POINT('Ctrl Pts',(13.1046057855928,-0.113633738735928,
25.6311151873271));
#46263=CARTESIAN_POINT('Ctrl Pts',(13.1363623920944,0.315056991891516,25.6828126457333));
#46264=CARTESIAN_POINT('Ctrl Pts',(13.168118998596,0.668091922502613,25.9330362757174));
#46265=CARTESIAN_POINT('Ctrl Pts',(13.1998756050976,0.857574838496823,26.3217550235969));
#46266=CARTESIAN_POINT('Ctrl Pts',(13.2316322115992,0.838682487086633,26.7537840960733));
#46267=CARTESIAN_POINT('Ctrl Pts',(13.2633888181008,0.61459639720261,27.1239610153356));
#46268=CARTESIAN_POINT('Ctrl Pts',(13.2951454246024,0.242011703991384,27.3422017450729));
#46269=CARTESIAN_POINT('Ctrl Pts',(13.326902031104,-0.191865608944966,27.3548657622106));
#46270=CARTESIAN_POINT('Ctrl Pts',(13.3586586376056,-0.574769741068602,
27.1598105807844));
#46271=CARTESIAN_POINT('Ctrl Pts',(13.4010007796077,-0.908143593732887,
26.6838738493453));
#46272=CARTESIAN_POINT('Ctrl Pts',(13.4433429216098,-0.817383382514841,
26.0636299903754));
#46273=CARTESIAN_POINT('Ctrl Pts',(13.485685063612,-0.361619360683378,25.7031677116595));
#46274=CARTESIAN_POINT('Ctrl Pts',(13.5174416701136,0.061118811960344,25.6260020743044));
#46275=CARTESIAN_POINT('Ctrl Pts',(13.5491982766152,0.473176351884539,25.7624516393552));
#46276=CARTESIAN_POINT('Ctrl Pts',(13.5809548831168,0.767608313754213,26.0782968380857));
#46277=CARTESIAN_POINT('Ctrl Pts',(13.6127114896184,0.876234336819935,26.4971594818568));
#46278=CARTESIAN_POINT('Ctrl Pts',(13.64446809612,0.770547639367812,26.9164879478454));
#46279=CARTESIAN_POINT('Ctrl Pts',(13.6762247026215,0.477631719236381,27.2346173305503));
#46280=CARTESIAN_POINT('Ctrl Pts',(13.7079813091232,0.0677033024918876,
27.3731966233013));
#46281=CARTESIAN_POINT('Ctrl Pts',(13.7397379156247,-0.357826258069027,
27.2998961265745));
#46282=CARTESIAN_POINT('Ctrl Pts',(13.7714945221263,-0.697708912234596,
27.0299152357539));
#46283=CARTESIAN_POINT('Ctrl Pts',(13.8032511286279,-0.8647311392666,26.6339787839389));
#46284=CARTESIAN_POINT('Ctrl Pts',(13.8455932706301,-0.812838045508947,
26.0552206265075));
#46285=CARTESIAN_POINT('Ctrl Pts',(13.8879354126322,-0.343658628821443,
25.6395157606628));
#46286=CARTESIAN_POINT('Ctrl Pts',(13.9302775546343,0.237136846646333,25.6576957950208));
#46287=CARTESIAN_POINT('Ctrl Pts',(13.9620341611359,0.610078734339102,25.8711822034938));
#46288=CARTESIAN_POINT('Ctrl Pts',(13.9937907676375,0.837165393027052,26.2411032078405));
#46289=CARTESIAN_POINT('Ctrl Pts',(14.0255473741391,0.858689140784456,26.6723631039751));
#46290=CARTESIAN_POINT('Ctrl Pts',(14.0573039806407,0.67175373280332,27.0626203018292));
#46291=CARTESIAN_POINT('Ctrl Pts',(14.0890605871423,0.320665802654134,27.3150946682711));
#46292=CARTESIAN_POINT('Ctrl Pts',(14.1208171936439,-0.108338152284935,
27.3695156849218));
#46293=CARTESIAN_POINT('Ctrl Pts',(14.1525738001455,-0.511071607221392,
27.2112396870291));
#46294=CARTESIAN_POINT('Ctrl Pts',(14.1843304066471,-0.789162091829571,
26.8809155248763));
#46295=CARTESIAN_POINT('Ctrl Pts',(14.2160870131487,-0.874997689426164,
26.4554250429661));
#46296=CARTESIAN_POINT('Ctrl Pts',(14.2478436196503,-0.747486430903569,
26.0450557249749));
#46297=CARTESIAN_POINT('Ctrl Pts',(14.2901857616524,-0.334763101404237,
25.6360161776692));
#46298=CARTESIAN_POINT('Ctrl Pts',(14.3325279036546,0.291896647532627,25.6206077516431));
#46299=CARTESIAN_POINT('Ctrl Pts',(14.3748700456567,0.724224157529318,26.0088690323203));
#46300=CARTESIAN_POINT('Ctrl Pts',(14.4066266521583,0.871749608336183,26.4124756967386));
#46301=CARTESIAN_POINT('Ctrl Pts',(14.4383832586599,0.806929171816575,26.8416705371319));
#46302=CARTESIAN_POINT('Ctrl Pts',(14.4701398651615,0.545409067776301,27.1852627444276));
#46303=CARTESIAN_POINT('Ctrl Pts',(14.501896471663,0.150941023139775,27.3631404805124));
#46304=CARTESIAN_POINT('Ctrl Pts',(14.5336530781647,-0.28021912285405,27.3298693381627));
#46305=CARTESIAN_POINT('Ctrl Pts',(14.5654096846662,-0.64329106005797,27.0949548668723));
#46306=CARTESIAN_POINT('Ctrl Pts',(14.5971662911679,-0.84918040708807,26.7143565168844));
#46307=CARTESIAN_POINT('Ctrl Pts',(14.6289228976694,-0.848877651649225,
26.2825599466448));
#46308=CARTESIAN_POINT('Ctrl Pts',(14.6606795041711,-0.640245791566623,
25.9019254146205));
#46309=CARTESIAN_POINT('Ctrl Pts',(14.6924361106726,-0.278246720378839,
25.6703681416667));
#46310=CARTESIAN_POINT('Ctrl Pts',(14.7347782526748,0.300953418160253,25.6236659202058));
#46311=CARTESIAN_POINT('Ctrl Pts',(14.7771203946769,0.7899963704059,26.0158098368856));
#46312=CARTESIAN_POINT('Ctrl Pts',(14.819462536679,0.8702707841193,26.5913182351529));
#46313=CARTESIAN_POINT('Ctrl Pts',(14.8512191431806,0.722909344492497,26.9949848108186));
#46314=CARTESIAN_POINT('Ctrl Pts',(14.8829757496822,0.39670607213585,27.2813435458255));
#46315=CARTESIAN_POINT('Ctrl Pts',(14.9147323561838,-0.0247067925502357,
27.3754688198417));
#46316=CARTESIAN_POINT('Ctrl Pts',(14.9464889626854,-0.440950549724207,
27.2572036015918));
#46317=CARTESIAN_POINT('Ctrl Pts',(14.978245569187,-0.749147498146967,26.9538544934843));
#46318=CARTESIAN_POINT('Ctrl Pts',(15.0100021756886,-0.875315073453636,
26.5402269033167));
#46319=CARTESIAN_POINT('Ctrl Pts',(15.0417587821902,-0.787406015941745,
26.1165318185666));
#46320=CARTESIAN_POINT('Ctrl Pts',(15.0735153886918,-0.508852589467088,
25.786597948934));
#46321=CARTESIAN_POINT('Ctrl Pts',(15.1052719951934,-0.103999031099223,
25.6300620224257));
#46322=CARTESIAN_POINT('Ctrl Pts',(15.137028601695,0.322020726425784,25.6863582425199));
#46323=CARTESIAN_POINT('Ctrl Pts',(15.1793707436971,0.794949506829644,26.0239856505288));
#46324=CARTESIAN_POINT('Ctrl Pts',(15.2217128856992,0.916082953491975,26.6390194289751));
#46325=CARTESIAN_POINT('Ctrl Pts',(15.2640550277014,0.60650265839727,27.1307652361379));
#46326=CARTESIAN_POINT('Ctrl Pts',(15.295811634203,0.233647548220779,27.3444031658551));
#46327=CARTESIAN_POINT('Ctrl Pts',(15.3275682407046,-0.20032784971622,27.3530780719845));
#46328=CARTESIAN_POINT('Ctrl Pts',(15.3593248472062,-0.583188103890229,
27.1534123625965));
#46329=CARTESIAN_POINT('Ctrl Pts',(15.3910814537078,-0.825196360355749,
26.7946958574891));
#46330=CARTESIAN_POINT('Ctrl Pts',(15.4228380602093,-0.865298666620334,
26.3641173565872));
#46331=CARTESIAN_POINT('Ctrl Pts',(15.454594666711,-0.69514895411333,25.9665558949986));
#46332=CARTESIAN_POINT('Ctrl Pts',(15.4863512732125,-0.354838295545939,
25.6992841551916));
#46333=CARTESIAN_POINT('Ctrl Pts',(15.5181078797141,0.0707936362898035,
25.6265804528559));
#46334=CARTESIAN_POINT('Ctrl Pts',(15.5498644862157,0.481221379809349,25.7678566623194));
#46335=CARTESIAN_POINT('Ctrl Pts',(15.5816210927173,0.770647044230475,26.0854962111369));
#46336=CARTESIAN_POINT('Ctrl Pts',(15.6239632347195,0.914599999637588,26.6484628572205));
#46337=CARTESIAN_POINT('Ctrl Pts',(15.6663053767216,0.610781610505709,27.1967640946398));
#46338=CARTESIAN_POINT('Ctrl Pts',(15.7086475187237,0.0571294758776682,
27.373181814257));
#46339=CARTESIAN_POINT('Ctrl Pts',(15.7404041252253,-0.365640016868747,
27.2961879560505));
#46340=CARTESIAN_POINT('Ctrl Pts',(15.7721607317269,-0.703026411114089,
27.0230939777408));
#46341=CARTESIAN_POINT('Ctrl Pts',(15.8039173382285,-0.867043295741499,
26.6236608402964));
#46342=CARTESIAN_POINT('Ctrl Pts',(15.8356739447301,-0.820853184433873,
26.193414398299));
#46343=CARTESIAN_POINT('Ctrl Pts',(15.8674305512317,-0.573976477136738,
25.8383680185107));
#46344=CARTESIAN_POINT('Ctrl Pts',(15.8991871577333,-0.187633805426696,
25.6440863147334));
#46345=CARTESIAN_POINT('Ctrl Pts',(15.9309437642349,0.244824507039883,25.6590974843267));
#46346=CARTESIAN_POINT('Ctrl Pts',(15.9627003707365,0.617102793802202,25.8778604769393));
#46347=CARTESIAN_POINT('Ctrl Pts',(15.9944569772381,0.839832298393764,26.2504211670227));
#46348=CARTESIAN_POINT('Ctrl Pts',(16.0262135837397,0.856371914216354,26.6798260334447));
#46349=CARTESIAN_POINT('Ctrl Pts',(16.0685557257418,0.603560896568364,27.2030281811171));
#46350=CARTESIAN_POINT('Ctrl Pts',(16.1108978677439,0.0178602313264146,
27.426399153415));
#46351=CARTESIAN_POINT('Ctrl Pts',(16.1532400097461,-0.519146255174819,
27.2044128217892));
#46352=CARTESIAN_POINT('Ctrl Pts',(16.1849966162477,-0.792745916569997,
26.8730439586125));
#46353=CARTESIAN_POINT('Ctrl Pts',(16.2167532227493,-0.874666410284016,
26.4467823807984));
#46354=CARTESIAN_POINT('Ctrl Pts',(16.2485098292509,-0.742603575282594,
26.0356768258092));
#46355=CARTESIAN_POINT('Ctrl Pts',(16.2802664357524,-0.429966244660699,
25.7365055926741));
#46356=CARTESIAN_POINT('Ctrl Pts',(16.3120230422541,-0.0123659680828667,
25.6241844040729));
#46357=CARTESIAN_POINT('Ctrl Pts',(16.3437796487556,0.408239016411182,25.7246706589808));
#46358=CARTESIAN_POINT('Ctrl Pts',(16.3755362552572,0.729198256444399,26.0148959050765));
#46359=CARTESIAN_POINT('Ctrl Pts',(16.4072928617588,0.872815239109643,26.4221090335752));
#46360=CARTESIAN_POINT('Ctrl Pts',(16.4390494682604,0.802962095894506,26.8505135601548));
#46361=CARTESIAN_POINT('Ctrl Pts',(16.470806074762,0.538827077444582,27.1894749004682));
#46362=CARTESIAN_POINT('Ctrl Pts',(16.5131482167641,0.00830202667944394,
27.4265341092826));
#46363=CARTESIAN_POINT('Ctrl Pts',(16.5554903587663,-0.583471617801813,
27.2197883373124));
#46364=CARTESIAN_POINT('Ctrl Pts',(16.5978325007684,-0.850953485318723,
26.7039323995519));
#46365=CARTESIAN_POINT('Ctrl Pts',(16.62958910727,-0.846543901799235,26.2742317435461));
#46366=CARTESIAN_POINT('Ctrl Pts',(16.6613457137716,-0.634421735364911,
25.8955312200211));
#46367=CARTESIAN_POINT('Ctrl Pts',(16.6931023202732,-0.268468213163799,
25.6663448562902));
#46368=CARTESIAN_POINT('Ctrl Pts',(16.7248589267748,0.163393894573562,25.639130023301));
#46369=CARTESIAN_POINT('Ctrl Pts',(16.7566155332764,0.55506773558983,25.8224266208424));
#46370=CARTESIAN_POINT('Ctrl Pts',(16.788372139778,0.811870096428448,26.1703613674176));
#46371=CARTESIAN_POINT('Ctrl Pts',(16.8201287462796,0.870188994142449,26.5991322076148));
#46372=CARTESIAN_POINT('Ctrl Pts',(16.8518853527812,0.717514735853032,27.0030368257953));
#46373=CARTESIAN_POINT('Ctrl Pts',(16.8836419592828,0.387973130305122,27.2855474100631));
#46374=CARTESIAN_POINT('Ctrl Pts',(16.9153985657844,-0.0324540553306391,
27.3744466776518));
#46375=CARTESIAN_POINT('Ctrl Pts',(16.9577407077865,-0.590866308020062,
27.213730611194));
#46376=CARTESIAN_POINT('Ctrl Pts',(17.0000828497886,-0.910043839361548,
26.6742256862701));
#46377=CARTESIAN_POINT('Ctrl Pts',(17.0424249917908,-0.782042573269087,
26.1074192167792));
#46378=CARTESIAN_POINT('Ctrl Pts',(17.0741815982923,-0.501700239207807,
25.7817349004191));
#46379=CARTESIAN_POINT('Ctrl Pts',(17.105938204794,-0.0954247742663506,
25.6289273527781));
#46380=CARTESIAN_POINT('Ctrl Pts',(17.1376948112956,0.332090138521344,25.6895851556312));
#46381=CARTESIAN_POINT('Ctrl Pts',(17.1694514177971,0.679811052822366,25.9471423201995));
#46382=CARTESIAN_POINT('Ctrl Pts',(17.2012080242988,0.861117338127211,26.3397414431271));
#46383=CARTESIAN_POINT('Ctrl Pts',(17.2329646308003,0.833187592663935,26.7712805138921));
#46384=CARTESIAN_POINT('Ctrl Pts',(17.2647212373019,0.601403494523231,27.1366866707663));
#46385=CARTESIAN_POINT('Ctrl Pts',(17.2964778438035,0.224333048232079,27.3470821255804));
#46386=CARTESIAN_POINT('Ctrl Pts',(17.3282344503051,-0.209714273666674,
27.350663157861));
#46387=CARTESIAN_POINT('Ctrl Pts',(17.3599910568068,-0.588452413422316,
27.1476372528845));
#46388=CARTESIAN_POINT('Ctrl Pts',(17.4023331988088,-0.911792823819409,
26.6648278932385));
#46389=CARTESIAN_POINT('Ctrl Pts',(17.444675340811,-0.808071974758552,26.0466193062064));
#46390=CARTESIAN_POINT('Ctrl Pts',(17.4870174828131,-0.344864013488189,
25.6957742430468));
#46391=CARTESIAN_POINT('Ctrl Pts',(17.5187740893147,0.0793965318800745,
25.6274725805664));
#46392=CARTESIAN_POINT('Ctrl Pts',(17.5505306958163,0.48850813612692,25.7725158616459));
#46393=CARTESIAN_POINT('Ctrl Pts',(17.5822873023179,0.776265705627514,26.0944537106846));
#46394=CARTESIAN_POINT('Ctrl Pts',(17.6140439088195,0.876101723455108,26.5154980733855));
#46395=CARTESIAN_POINT('Ctrl Pts',(17.6458005153211,0.761662875423693,26.9325226470832));
#46396=CARTESIAN_POINT('Ctrl Pts',(17.6775571218227,0.462152454421897,27.2444526346239));
#46397=CARTESIAN_POINT('Ctrl Pts',(17.7093137283243,0.0494151738932063,
27.3744217314534));
#46398=CARTESIAN_POINT('Ctrl Pts',(17.7410703348259,-0.37449007535567,27.29223335565));
#46399=CARTESIAN_POINT('Ctrl Pts',(17.7728269413275,-0.708642640693063,
27.015195558281));
#46400=CARTESIAN_POINT('Ctrl Pts',(17.8045835478291,-0.867352034794116,
26.6158557264595));
#46401=CARTESIAN_POINT('Ctrl Pts',(17.8469256898312,-0.803337221972986,
26.0382991332051));
#46402=CARTESIAN_POINT('Ctrl Pts',(17.8892678318333,-0.325602990091037,
25.6325271546952));
#46403=CARTESIAN_POINT('Ctrl Pts',(17.9316099738355,0.254746860080869,25.6628246699476));
#46404=CARTESIAN_POINT('Ctrl Pts',(17.9633665803371,0.623033274293027,25.8841264013226));
#46405=CARTESIAN_POINT('Ctrl Pts',(17.9951231868387,0.842539849663937,26.2586048773553));
#46406=CARTESIAN_POINT('Ctrl Pts',(18.0268797933403,0.854628194489789,26.6904393272496));
#46407=CARTESIAN_POINT('Ctrl Pts',(18.0586363998418,0.660333792873029,27.0762848995925));
#46408=CARTESIAN_POINT('Ctrl Pts',(18.0903930063434,0.302597639953616,27.3221346718869));
#46409=CARTESIAN_POINT('Ctrl Pts',(18.122149612845,-0.124805809017264,27.366130478626));
#46410=CARTESIAN_POINT('Ctrl Pts',(18.1644917548472,-0.66311189802541,27.1471545836929));
#46411=CARTESIAN_POINT('Ctrl Pts',(18.2068338968493,-0.923363074658378,
26.5769351347813));
#46412=CARTESIAN_POINT('Ctrl Pts',(18.2491760388514,-0.73610041458287,26.0268422237077));
#46413=CARTESIAN_POINT('Ctrl Pts',(18.280932645353,-0.422853630327345,25.7326697824275));
#46414=CARTESIAN_POINT('Ctrl Pts',(18.3126892518546,-0.00268997678121585,
25.6237184982157));
#46415=CARTESIAN_POINT('Ctrl Pts',(18.3444458583562,0.416004918794958,25.7292892037947));
#46416=CARTESIAN_POINT('Ctrl Pts',(18.3762024648578,0.734509914179396,26.0222031788523));
#46417=CARTESIAN_POINT('Ctrl Pts',(18.4079590713594,0.873242998764314,26.4317882623911));
#46418=CARTESIAN_POINT('Ctrl Pts',(18.439715677861,0.799792930977031,26.857946487172));
#46419=CARTESIAN_POINT('Ctrl Pts',(18.4714722843626,0.530634059378337,27.1967666277446));
#46420=CARTESIAN_POINT('Ctrl Pts',(18.5032288908642,0.133412098705898,27.3660684629623));
#46421=CARTESIAN_POINT('Ctrl Pts',(18.5349854973658,-0.298575946972933,
27.323687022374));
#46422=CARTESIAN_POINT('Ctrl Pts',(18.5667421038674,-0.653696947944898,
27.0817134657145));
#46423=CARTESIAN_POINT('Ctrl Pts',(18.6090842458695,-0.924117259356119,
26.5673918456129));
#46424=CARTESIAN_POINT('Ctrl Pts',(18.6514263878717,-0.755543837880523,
25.9636345490257));
#46425=CARTESIAN_POINT('Ctrl Pts',(18.6937685298738,-0.257802194059594,
25.663789331015));
#46426=CARTESIAN_POINT('Ctrl Pts',(18.7255251363754,0.171304517422399,25.6407778825982));
#46427=CARTESIAN_POINT('Ctrl Pts',(18.757281742877,0.562765663228658,25.828309407318));
#46428=CARTESIAN_POINT('Ctrl Pts',(18.7890383493786,0.814830607180771,26.1788969611515));
#46429=CARTESIAN_POINT('Ctrl Pts',(18.8207949558802,0.869539941123068,26.6081432965023));
#46430=CARTESIAN_POINT('Ctrl Pts',(18.8525515623818,0.711602884148318,27.0107124536822));
#46431=CARTESIAN_POINT('Ctrl Pts',(18.8843081688833,0.380759120484664,27.2891876670486));
#46432=CARTESIAN_POINT('Ctrl Pts',(18.916064775385,-0.0434180107468701,
27.3747405080475));
#46433=CARTESIAN_POINT('Ctrl Pts',(18.9478213818865,-0.456239530951512,
27.2481436591185));
#46434=CARTESIAN_POINT('Ctrl Pts',(18.9795779883882,-0.759197243098779,
26.9372955858094));
#46435=CARTESIAN_POINT('Ctrl Pts',(19.0113345948897,-0.874735896034552,
26.5233959387116));
#46436=CARTESIAN_POINT('Ctrl Pts',(19.0536767368919,-0.749970179761652,
25.9558684820887));
#46437=CARTESIAN_POINT('Ctrl Pts',(19.096018878894,-0.231925562864532,25.602924243668));
#46438=CARTESIAN_POINT('Ctrl Pts',(19.1383610208961,0.341892025666602,25.6945063001182));
#46439=CARTESIAN_POINT('Ctrl Pts',(19.1701176273977,0.684796943888501,25.953501117168));
#46440=CARTESIAN_POINT('Ctrl Pts',(19.2018742338993,0.863210918198414,26.3492009450444));
#46441=CARTESIAN_POINT('Ctrl Pts',(19.2336308404009,0.829949279037307,26.7797146301835));
#46442=CARTESIAN_POINT('Ctrl Pts',(19.2653874469025,0.595099009571776,27.143157718116));
#46443=CARTESIAN_POINT('Ctrl Pts',(19.2971440534041,0.214865696983258,27.3491399222129));
#46444=CARTESIAN_POINT('Ctrl Pts',(19.3289006599057,-0.217576116898816,
27.3487963919108));
#46445=CARTESIAN_POINT('Ctrl Pts',(19.3606572664073,-0.597024274205395,
27.1407948939579));
#46446=CARTESIAN_POINT('Ctrl Pts',(19.3924138729089,-0.831045770920826,
26.7779143229616));
#46447=CARTESIAN_POINT('Ctrl Pts',(19.4241704794105,-0.862308843996473,
26.3449795469586));
#46448=CARTESIAN_POINT('Ctrl Pts',(19.4559270859121,-0.683857455778086,
25.954061140841));
#46449=CARTESIAN_POINT('Ctrl Pts',(19.4982692279142,-0.222658482913689,
25.6005793090563));
#46450=CARTESIAN_POINT('Ctrl Pts',(19.5406113699163,0.400907586751457,25.6646512786888));
#46451=CARTESIAN_POINT('Ctrl Pts',(19.5829535119185,0.780587626055508,26.1045341787056));
#46452=CARTESIAN_POINT('Ctrl Pts',(19.6147101184201,0.875815152337618,26.5235733373014));
#46453=CARTESIAN_POINT('Ctrl Pts',(19.6464667249217,0.757165946501871,26.9411044929839));
#46454=CARTESIAN_POINT('Ctrl Pts',(19.6782233314233,0.454240791570915,27.2488133167793));
#46455=CARTESIAN_POINT('Ctrl Pts',(19.7099799379249,0.0404230551237811,
27.3753060368695));
#46456=CARTESIAN_POINT('Ctrl Pts',(19.7417365444265,-0.38305279380198,27.2877032641777));
#46457=CARTESIAN_POINT('Ctrl Pts',(19.7734931509281,-0.713453700745531,
27.0087027604192));
#46458=CARTESIAN_POINT('Ctrl Pts',(19.8052497574296,-0.86948889817834,26.6050958422474));
#46459=CARTESIAN_POINT('Ctrl Pts',(19.8370063639313,-0.814508508394085,
26.1768137780997));
#46460=CARTESIAN_POINT('Ctrl Pts',(19.8687629704328,-0.559355008981932,
25.8256633947185));
#46461=CARTESIAN_POINT('Ctrl Pts',(19.9005195769344,-0.170947207752905,
25.641811611635));
#46462=CARTESIAN_POINT('Ctrl Pts',(19.9428617189366,0.409504178357161,25.6688317214792));
#46463=CARTESIAN_POINT('Ctrl Pts',(19.9852038609387,0.844951400494168,26.1197480965017));
#46464=CARTESIAN_POINT('Ctrl Pts',(20.0275460029408,0.851700710212036,26.7007888392998));
#46465=CARTESIAN_POINT('Ctrl Pts',(20.0593026094424,0.65440773846806,27.0825447580477));
#46466=CARTESIAN_POINT('Ctrl Pts',(20.091059215944,0.294567841588426,27.3252897860598));
#46467=CARTESIAN_POINT('Ctrl Pts',(20.1228158224456,-0.135371897765222,
27.3652921641899));
#46468=CARTESIAN_POINT('Ctrl Pts',(20.1545724289472,-0.533288312928303,
27.1952684782584));
#46469=CARTESIAN_POINT('Ctrl Pts',(20.1863290354488,-0.800589857703777,
26.8553333012505));
#46470=CARTESIAN_POINT('Ctrl Pts',(20.2180856419504,-0.873362460873776,
26.4290585205815));
#46471=CARTESIAN_POINT('Ctrl Pts',(20.249842248452,-0.73250696373832,26.0199066463822));
#46472=CARTESIAN_POINT('Ctrl Pts',(20.2815988549536,-0.414415220875257,
25.7279031997349));
#46473=CARTESIAN_POINT('Ctrl Pts',(20.3133554614552,0.0070018250111366,
25.6238956353595));
#46474=CARTESIAN_POINT('Ctrl Pts',(20.3451120679568,0.422462913279715,25.7336871757133));
#46475=CARTESIAN_POINT('Ctrl Pts',(20.3874542099589,0.848829326883048,26.1284853258155));
#46476=CARTESIAN_POINT('Ctrl Pts',(20.429796351961,0.891103483033206,26.7539073883077));
#46477=CARTESIAN_POINT('Ctrl Pts',(20.4721384939632,0.52174378033525,27.202491057199));
#46478=CARTESIAN_POINT('Ctrl Pts',(20.5038951004647,0.124836532195944,27.3671930139969));
#46479=CARTESIAN_POINT('Ctrl Pts',(20.5356517069664,-0.306743695101083,
27.320842097963));
#46480=CARTESIAN_POINT('Ctrl Pts',(20.5674083134679,-0.661237300894562,
27.0743007156697));
#46481=CARTESIAN_POINT('Ctrl Pts',(20.5991649199696,-0.855871616173788,
26.6878256057987));
#46482=CARTESIAN_POINT('Ctrl Pts',(20.6309215264711,-0.841125257036995,
26.2556351555354));
#46483=CARTESIAN_POINT('Ctrl Pts',(20.6626781329728,-0.622000583043283,
25.8828209690378));
#46484=CARTESIAN_POINT('Ctrl Pts',(20.6944347394743,-0.250583931206579,
25.6607957498117));
#46485=CARTESIAN_POINT('Ctrl Pts',(20.7261913459759,0.180828213237544,25.6425767663691));
#46486=CARTESIAN_POINT('Ctrl Pts',(20.7579479524775,0.570061465492677,25.8346896898018));
#46487=CARTESIAN_POINT('Ctrl Pts',(20.7897045589791,0.816933190155719,26.186423182322));
#46488=CARTESIAN_POINT('Ctrl Pts',(20.8320467009813,0.888436609774976,26.7630870002921));
#46489=CARTESIAN_POINT('Ctrl Pts',(20.8743888429834,0.517630593842114,27.2685004538904));
#46490=CARTESIAN_POINT('Ctrl Pts',(20.9167309849855,-0.0539048377036311,
27.3733868136372));
#46491=CARTESIAN_POINT('Ctrl Pts',(20.9484875914871,-0.463520805306752,
27.24347585458));
#46492=CARTESIAN_POINT('Ctrl Pts',(20.9802441979887,-0.763608131273106,
26.9298558666882));
#46493=CARTESIAN_POINT('Ctrl Pts',(21.0120008044903,-0.875722837400207,
26.5128682620743));
#46494=CARTESIAN_POINT('Ctrl Pts',(21.0437574109919,-0.775420805447384,
26.0919347404582));
#46495=CARTESIAN_POINT('Ctrl Pts',(21.0755140174935,-0.485570674761989,
25.7710096056552));
#46496=CARTESIAN_POINT('Ctrl Pts',(21.1072706239951,-0.0777356001915541,
25.6272160301493));
#46497=CARTESIAN_POINT('Ctrl Pts',(21.1390272304967,0.349340295407205,25.6968702233649));
#46498=CARTESIAN_POINT('Ctrl Pts',(21.1707838369983,0.690918760718671,25.9610151111955));
#46499=CARTESIAN_POINT('Ctrl Pts',(21.2025404434999,0.864676384461559,26.3587816107931));
#46500=CARTESIAN_POINT('Ctrl Pts',(21.2342970500015,0.826705647584722,26.7868240401616));
#46501=CARTESIAN_POINT('Ctrl Pts',(21.2766391920036,0.509674764547415,27.2737997245377));
#46502=CARTESIAN_POINT('Ctrl Pts',(21.3189813340057,-0.0995970639515039,
27.421202911504));
#46503=CARTESIAN_POINT('Ctrl Pts',(21.3613234760079,-0.604169405036641,
27.1330004642816));
#46504=CARTESIAN_POINT('Ctrl Pts',(21.3930800825095,-0.833603937258024,
26.7696522929322));
#46505=CARTESIAN_POINT('Ctrl Pts',(21.4248366890111,-0.860885778032424,
26.3364484134772));
#46506=CARTESIAN_POINT('Ctrl Pts',(21.4565932955127,-0.677826223140756,
25.9453760811723));
#46507=CARTESIAN_POINT('Ctrl Pts',(21.4883499020142,-0.329820559486764,
25.6882037939819));
#46508=CARTESIAN_POINT('Ctrl Pts',(21.5201065085159,0.0986415040206994,
25.6296691842062));
#46509=CARTESIAN_POINT('Ctrl Pts',(21.5518631150174,0.503135455528145,25.7826093149782));
#46510=CARTESIAN_POINT('Ctrl Pts',(21.5836197215191,0.784758474883268,26.1111424216863));
#46511=CARTESIAN_POINT('Ctrl Pts',(21.6153763280206,0.875652297533056,26.533264066163));
#46512=CARTESIAN_POINT('Ctrl Pts',(21.6471329345222,0.752110981173881,26.949373959296));
#46513=CARTESIAN_POINT('Ctrl Pts',(21.6788895410238,0.447178387750749,27.2521580600457));
#46514=CARTESIAN_POINT('Ctrl Pts',(21.721231683026,-0.109095410505965,27.4201263884477));
#46515=CARTESIAN_POINT('Ctrl Pts',(21.7635738250281,-0.669923979080759,
27.1401064298722));
#46516=CARTESIAN_POINT('Ctrl Pts',(21.8059159670302,-0.869927655947503,
26.5945311122369));
#46517=CARTESIAN_POINT('Ctrl Pts',(21.8376725735318,-0.811138913729804,
26.1688481527623));
#46518=CARTESIAN_POINT('Ctrl Pts',(21.8694291800334,-0.552768117570983,
25.8200581992041));
#46519=CARTESIAN_POINT('Ctrl Pts',(21.901185786535,-0.160737937948536,25.6390590058447));
#46520=CARTESIAN_POINT('Ctrl Pts',(21.9329423930366,0.271093794863995,25.6667516360942));
#46521=CARTESIAN_POINT('Ctrl Pts',(21.9646989995382,0.63640291796604,25.8981717842771));
#46522=CARTESIAN_POINT('Ctrl Pts',(21.9964556060398,0.847077573899532,26.2758253686028));
#46523=CARTESIAN_POINT('Ctrl Pts',(22.0282122125414,0.850630065093437,26.7085295481993));
#46524=CARTESIAN_POINT('Ctrl Pts',(22.059968819043,0.648036901149478,27.0898488103076));
#46525=CARTESIAN_POINT('Ctrl Pts',(22.0917254255446,0.285372852470821,27.3283539209591));
#46526=CARTESIAN_POINT('Ctrl Pts',(22.1234820320462,-0.142927353585185,
27.3632971848444));
#46527=CARTESIAN_POINT('Ctrl Pts',(22.1658241740483,-0.676492025225343,
27.1331610530644));
#46528=CARTESIAN_POINT('Ctrl Pts',(22.2081663160505,-0.924780428505825,
26.5575807117335));
#46529=CARTESIAN_POINT('Ctrl Pts',(22.2505084580525,-0.726032735274209,
26.0115465988722));
#46530=CARTESIAN_POINT('Ctrl Pts',(22.2822650645542,-0.406704623753999,
25.7239850308707));
#46531=CARTESIAN_POINT('Ctrl Pts',(22.3140216710558,0.0156507426113821,
25.6238558916889));
#46532=CARTESIAN_POINT('Ctrl Pts',(22.3457782775574,0.43204262535938,25.7381632392791));
#46533=CARTESIAN_POINT('Ctrl Pts',(22.377534884059,0.744348760409762,26.0376801924619));
#46534=CARTESIAN_POINT('Ctrl Pts',(22.4092914905605,0.874479097205011,26.4500782233159));
#46535=CARTESIAN_POINT('Ctrl Pts',(22.4410480970622,0.792126735651671,26.8746063483597));
#46536=CARTESIAN_POINT('Ctrl Pts',(22.4728047035637,0.515935813272952,27.2077190944827));
#46537=CARTESIAN_POINT('Ctrl Pts',(22.5045613100654,0.115257770696188,27.3686708758596));
#46538=CARTESIAN_POINT('Ctrl Pts',(22.5363179165669,-0.315748742833674,
27.3172579853967));
#46539=CARTESIAN_POINT('Ctrl Pts',(22.5680745230685,-0.665727907757558,
27.0679054592059));
#46540=CARTESIAN_POINT('Ctrl Pts',(22.6104166650707,-0.925325249310694,
26.5480370929518));
#46541=CARTESIAN_POINT('Ctrl Pts',(22.6527588070727,-0.744153268499322,
25.9479399558989));
#46542=CARTESIAN_POINT('Ctrl Pts',(22.6951009490749,-0.240245462236218,
25.6585771719059));
#46543=CARTESIAN_POINT('Ctrl Pts',(22.7268575555765,0.189248855064349,25.6445511387859));
#46544=CARTESIAN_POINT('Ctrl Pts',(22.7586141620781,0.576699591845642,25.8402341134632));
#46545=CARTESIAN_POINT('Ctrl Pts',(22.7903707685797,0.821372211418811,26.1960201151029));
#46546=CARTESIAN_POINT('Ctrl Pts',(22.8221273750813,0.867086268116494,26.6263173986805));
#46547=CARTESIAN_POINT('Ctrl Pts',(22.8538839815829,0.700758808996464,27.0254930702204));
#46548=CARTESIAN_POINT('Ctrl Pts',(22.8856405880845,0.364159558242971,27.2969833735442));
#46549=CARTESIAN_POINT('Ctrl Pts',(22.9173971945861,-0.0617151267228295,
27.3736402710765));
#46550=CARTESIAN_POINT('Ctrl Pts',(22.9491538010877,-0.471796805528492,
27.2384315936942));
#46551=CARTESIAN_POINT('Ctrl Pts',(22.9809104075893,-0.768182716769667,
26.9213112827258));
#46552=CARTESIAN_POINT('Ctrl Pts',(23.0126670140909,-0.87503394665564,26.5050842859195));
#46553=CARTESIAN_POINT('Ctrl Pts',(23.055009156093,-0.738418305193021,25.9402922317253));
#46554=CARTESIAN_POINT('Ctrl Pts',(23.0973512980951,-0.213100708746876,
25.5982669645384));
#46555=CARTESIAN_POINT('Ctrl Pts',(23.1396934400973,0.358674569475328,25.7018378542084));
#46556=CARTESIAN_POINT('Ctrl Pts',(23.1714500465988,0.696084125988342,25.9679522833028));
#46557=CARTESIAN_POINT('Ctrl Pts',(23.2032066531005,0.866177793525835,26.3672993056713));
#46558=CARTESIAN_POINT('Ctrl Pts',(23.234963259602,0.823913621290959,26.7970225997534));
#46559=CARTESIAN_POINT('Ctrl Pts',(23.2667198661037,0.581508627612291,27.155471126426));
#46560=CARTESIAN_POINT('Ctrl Pts',(23.2984764726053,0.197047783445193,27.3534506700888));
#46561=CARTESIAN_POINT('Ctrl Pts',(23.3302330791068,-0.235292129374152,
27.3440570451221));
#46562=CARTESIAN_POINT('Ctrl Pts',(23.3619896856085,-0.610304112860864,
27.1281599875336));
#46563=CARTESIAN_POINT('Ctrl Pts',(23.39374629211,-0.836679967375603,26.7604612763252));
#46564=CARTESIAN_POINT('Ctrl Pts',(23.4255028986117,-0.858875706694659,
26.3269670443371));
#46565=CARTESIAN_POINT('Ctrl Pts',(23.4572595051132,-0.672282236796609,
25.9398688976223));
#46566=CARTESIAN_POINT('Ctrl Pts',(23.4996016471154,-0.203786583491818,
25.596116485547));
#46567=CARTESIAN_POINT('Ctrl Pts',(23.5419437891175,0.418302013008299,25.6732244529351));
#46568=CARTESIAN_POINT('Ctrl Pts',(23.5842859311196,0.788692998912709,26.1209569797119));
#46569=CARTESIAN_POINT('Ctrl Pts',(23.6160425376212,0.875129990573807,26.5418972898167));
#46570=CARTESIAN_POINT('Ctrl Pts',(23.6477991441228,0.747768652106043,26.9568539013734));
#46571=CARTESIAN_POINT('Ctrl Pts',(23.6795557506244,0.438470092684962,27.2581556950481));
#46572=CARTESIAN_POINT('Ctrl Pts',(23.711312357126,0.0220957411812786,27.3759603071985));
#46573=CARTESIAN_POINT('Ctrl Pts',(23.7430689636276,-0.399454003372334,
27.279514191292));
#46574=CARTESIAN_POINT('Ctrl Pts',(23.7748255701292,-0.723943606895722,
26.9936601417984));
#46575=CARTESIAN_POINT('Ctrl Pts',(23.8065821766308,-0.87149791877326,26.5868761053855));
#46576=CARTESIAN_POINT('Ctrl Pts',(23.8383387831324,-0.807566456174055,
26.1598384749342));
#46577=CARTESIAN_POINT('Ctrl Pts',(23.870095389634,-0.545119941785172,25.8141048678086));
#46578=CARTESIAN_POINT('Ctrl Pts',(23.9018519961356,-0.152949546185258,
25.638421974465));
#46579=CARTESIAN_POINT('Ctrl Pts',(23.9441941381377,0.426809233249918,25.6775838901603));
#46580=CARTESIAN_POINT('Ctrl Pts',(23.9865362801398,0.852724278817119,26.1375145746006));
#46581=CARTESIAN_POINT('Ctrl Pts',(24.028878422142,0.847312052549233,26.718569310215));
#46582=CARTESIAN_POINT('Ctrl Pts',(24.0606350286435,0.642072878853147,27.096112658427));
#46583=CARTESIAN_POINT('Ctrl Pts',(24.0923916351452,0.27723160918528,27.3312737690684));
#46584=CARTESIAN_POINT('Ctrl Pts',(24.1241482416467,-0.153451138848596,
27.3622695797134));
#46585=CARTESIAN_POINT('Ctrl Pts',(24.1559048481484,-0.547722137425273,
27.1839555115209));
#46586=CARTESIAN_POINT('Ctrl Pts',(24.1876614546499,-0.807850953810988,
26.8385006819232));
#46587=CARTESIAN_POINT('Ctrl Pts',(24.2194180611516,-0.871686512784537,
26.4107962725267));
#46588=CARTESIAN_POINT('Ctrl Pts',(24.2511746676531,-0.722299108686334,
26.0046818419399));
#46589=CARTESIAN_POINT('Ctrl Pts',(24.2829312741547,-0.398165966193382,
25.719399393007));
#46590=CARTESIAN_POINT('Ctrl Pts',(24.3146878806563,0.0253354596048242,
25.6242340507976));
#46591=CARTESIAN_POINT('Ctrl Pts',(24.3464444871579,0.438407830914415,25.7426963412501));
#46592=CARTESIAN_POINT('Ctrl Pts',(24.3887866291601,0.856418502585246,26.1463310478134));
#46593=CARTESIAN_POINT('Ctrl Pts',(24.4311287711621,0.885594527149535,26.7725008491618));
#46594=CARTESIAN_POINT('Ctrl Pts',(24.4734709131644,0.506927732427945,27.2132562876404));
#46595=CARTESIAN_POINT('Ctrl Pts',(24.5052275196659,0.106660520219594,27.3696156718471));
#46596=CARTESIAN_POINT('Ctrl Pts',(24.5369841261675,-0.323855149208574,
27.3142427688372));
#46597=CARTESIAN_POINT('Ctrl Pts',(24.5687407326691,-0.67311148146482,27.0603365182043));
#46598=CARTESIAN_POINT('Ctrl Pts',(24.6004973391707,-0.859614992946161,
26.6698727331497));
#46599=CARTESIAN_POINT('Ctrl Pts',(24.6322539456723,-0.835826954147192,
26.2380855522183));
#46600=CARTESIAN_POINT('Ctrl Pts',(24.6640105521739,-0.608947992835266,
25.8699388731341));
#46601=CARTESIAN_POINT('Ctrl Pts',(24.6957671586755,-0.232966129185645,
25.655735312378));
#46602=CARTESIAN_POINT('Ctrl Pts',(24.7275237651771,0.198732817183121,25.6465489400985));
#46603=CARTESIAN_POINT('Ctrl Pts',(24.7592803716787,0.583860269629324,25.8467656861094));
#46604=CARTESIAN_POINT('Ctrl Pts',(24.7910369781803,0.823316824457635,26.2035886906205));
#46605=CARTESIAN_POINT('Ctrl Pts',(24.8333791201824,0.882736126473029,26.7816226381713));
#46606=CARTESIAN_POINT('Ctrl Pts',(24.8757212621845,0.501433997917763,27.2791651461939));
#46607=CARTESIAN_POINT('Ctrl Pts',(24.9180634041867,-0.0721713267102057,
27.3720674041403));
#46608=CARTESIAN_POINT('Ctrl Pts',(24.9498200106883,-0.478978797049014,
27.233612428516));
#46609=CARTESIAN_POINT('Ctrl Pts',(24.9815766171899,-0.77243693997653,26.913780881666));
#46610=CARTESIAN_POINT('Ctrl Pts',(25.0133332236915,-0.875800347974294,
26.4945382602418));
#46611=CARTESIAN_POINT('Ctrl Pts',(25.045089830193,-0.766710960134842,26.0757960570967));
#46612=CARTESIAN_POINT('Ctrl Pts',(25.0768464366946,-0.470207969519981,
25.7610072120543));
#46613=CARTESIAN_POINT('Ctrl Pts',(25.1086030431962,-0.0594528961875975,
25.6257803281209));
#46614=CARTESIAN_POINT('Ctrl Pts',(25.1403596496979,0.366071735589218,25.7043571375826));
#46615=CARTESIAN_POINT('Ctrl Pts',(25.1721162561994,0.70204734869645,25.9755927494199));
#46616=CARTESIAN_POINT('Ctrl Pts',(25.2038728627011,0.867442434043655,26.3769085424732));
#46617=CARTESIAN_POINT('Ctrl Pts',(25.2356294692026,0.820521914059242,26.8040625697314));
#46618=CARTESIAN_POINT('Ctrl Pts',(25.2779716112048,0.493369007601602,27.2842967561129));
#46619=CARTESIAN_POINT('Ctrl Pts',(25.3203137532069,-0.118854243983667,
27.4189167796913));
#46620=CARTESIAN_POINT('Ctrl Pts',(25.362655895209,-0.617284556472856,27.120217731207));
#46621=CARTESIAN_POINT('Ctrl Pts',(25.3944125017106,-0.839064665140981,
26.7521475183433));
#46622=CARTESIAN_POINT('Ctrl Pts',(25.4261691082122,-0.857274412299222,
26.3184675613251));
#46623=CARTESIAN_POINT('Ctrl Pts',(25.4579257147138,-0.666070563609887,
25.9313119621416));
#46624=CARTESIAN_POINT('Ctrl Pts',(25.4896823212154,-0.312759000685908,
25.6814790845327));
#46625=CARTESIAN_POINT('Ctrl Pts',(25.521438927717,0.116834238873859,25.6319241762008));
#46626=CARTESIAN_POINT('Ctrl Pts',(25.5531955342186,0.51803885892464,25.7932960859057));
#46627=CARTESIAN_POINT('Ctrl Pts',(25.5849521407202,0.792724636550138,26.1276510631719));
#46628=CARTESIAN_POINT('Ctrl Pts',(25.6167087472218,0.874764363200845,26.5515824880205));
#46629=CARTESIAN_POINT('Ctrl Pts',(25.6484653537234,0.742541730057994,26.9650157659));
#46630=CARTESIAN_POINT('Ctrl Pts',(25.680221960225,0.431339236497572,27.2613519033306));
#46631=CARTESIAN_POINT('Ctrl Pts',(25.7225641022271,-0.128327980376764,
27.4176417103926));
#46632=CARTESIAN_POINT('Ctrl Pts',(25.7649062442292,-0.683173443957012,
27.1259460245806));
#46633=CARTESIAN_POINT('Ctrl Pts',(25.8072483862314,-0.871715480323669,
26.5763045068337));
#46634=CARTESIAN_POINT('Ctrl Pts',(25.8390049927329,-0.804030896026743,
26.1519451133608));
#46635=CARTESIAN_POINT('Ctrl Pts',(25.8707615992346,-0.538417183932629,
25.8086387506637));
#46636=CARTESIAN_POINT('Ctrl Pts',(25.9025182057361,-0.142684911729077,
25.6358836320594));
#46637=CARTESIAN_POINT('Ctrl Pts',(25.9342748122378,0.288472707472188,25.67260759849));
#46638=CARTESIAN_POINT('Ctrl Pts',(25.9660314187393,0.648858613252514,25.9116222761151));
#46639=CARTESIAN_POINT('Ctrl Pts',(25.997788025241,0.85158363238984,26.2936021581678));
#46640=CARTESIAN_POINT('Ctrl Pts',(26.0295446317425,0.846079566586723,26.7262859206823));
#46641=CARTESIAN_POINT('Ctrl Pts',(26.0613012382441,0.635550722694575,27.1032817752238));
#46642=CARTESIAN_POINT('Ctrl Pts',(26.0930578447457,0.267974236077588,27.3341448116203));
#46643=CARTESIAN_POINT('Ctrl Pts',(26.1248144512473,-0.16096270354682,27.3601168946639));
#46644=CARTESIAN_POINT('Ctrl Pts',(26.1671565932494,-0.689595797064967,
27.1188647612773));
#46645=CARTESIAN_POINT('Ctrl Pts',(26.2094987352516,-0.925780813951623,
26.53821414226));
#46646=CARTESIAN_POINT('Ctrl Pts',(26.2518408772537,-0.715653941089743,
25.9964592341892));
#46647=CARTESIAN_POINT('Ctrl Pts',(26.2835974837553,-0.390369588230022,
25.7156432068259));
#46648=CARTESIAN_POINT('Ctrl Pts',(26.3153540902569,0.0339726758359866,
25.6243757953063));
#46649=CARTESIAN_POINT('Ctrl Pts',(26.3471106967585,0.447912024032863,25.7473709970866));
#46650=CARTESIAN_POINT('Ctrl Pts',(26.3788673032601,0.753822864844703,26.0533610271208));
#46651=CARTESIAN_POINT('Ctrl Pts',(26.4106239097617,0.87540473357552,26.4683863005388));
#46652=CARTESIAN_POINT('Ctrl Pts',(26.4423805162633,0.783976936688825,26.8911144898655));
#46653=CARTESIAN_POINT('Ctrl Pts',(26.4635515872644,0.595505398658813,27.1092393365905));
#46654=CARTESIAN_POINT('Ctrl Pts',(26.4741371227649,0.480906627467731,27.1892031454205));
#46655=CARTESIAN_POINT('Ctrl Pts',(9.60000000000002,0.662150216245817,26.1181780341239));
#46656=CARTESIAN_POINT('Ctrl Pts',(9.61058553550055,0.725638504704611,26.2282785199239));
#46657=CARTESIAN_POINT('Ctrl Pts',(9.63175660650163,0.796605391005151,26.480675629033));
#46658=CARTESIAN_POINT('Ctrl Pts',(9.6635132130032,0.708650864432033,26.8640803773426));
#46659=CARTESIAN_POINT('Ctrl Pts',(9.69526981950482,0.448266436304386,27.1588859127484));
#46660=CARTESIAN_POINT('Ctrl Pts',(9.7270264260064,0.0782001173243299,27.2927247256205));
#46661=CARTESIAN_POINT('Ctrl Pts',(9.75878303250801,-0.310157515624281,
27.2341585395261));
#46662=CARTESIAN_POINT('Ctrl Pts',(9.7905396390096,-0.624341483803593,26.9951389225185));
#46663=CARTESIAN_POINT('Ctrl Pts',(9.82229624551119,-0.783759014765585,
26.6382863941097));
#46664=CARTESIAN_POINT('Ctrl Pts',(9.86463838751332,-0.747584602748986,
26.1110311207911));
#46665=CARTESIAN_POINT('Ctrl Pts',(9.90698052951547,-0.328871142664085,
25.7240954537507));
#46666=CARTESIAN_POINT('Ctrl Pts',(9.94932267151757,0.199598255234956,25.7295723838951));
#46667=CARTESIAN_POINT('Ctrl Pts',(9.98107927801918,0.542780303630156,25.9165983405945));
#46668=CARTESIAN_POINT('Ctrl Pts',(10.0128358845208,0.756313557236772,26.2486482930385));
#46669=CARTESIAN_POINT('Ctrl Pts',(10.0445924910224,0.784093796915711,26.6403866625412));
#46670=CARTESIAN_POINT('Ctrl Pts',(10.076349097524,0.621540241153639,26.9988089464404));
#46671=CARTESIAN_POINT('Ctrl Pts',(10.1081057040256,0.307098718342552,27.235068614701));
#46672=CARTESIAN_POINT('Ctrl Pts',(10.1398623105272,-0.0819621986926931,
27.2927198636753));
#46673=CARTESIAN_POINT('Ctrl Pts',(10.1716189170288,-0.451183699623203,
27.1564639171439));
#46674=CARTESIAN_POINT('Ctrl Pts',(10.2033755235304,-0.710341110413239,
26.8613906959017));
#46675=CARTESIAN_POINT('Ctrl Pts',(10.235132130032,-0.796491008458601,26.4761225321646));
#46676=CARTESIAN_POINT('Ctrl Pts',(10.2668887365335,-0.688355039348421,
26.1005432767371));
#46677=CARTESIAN_POINT('Ctrl Pts',(10.3092308785357,-0.320848092753299,
25.720744399325));
#46678=CARTESIAN_POINT('Ctrl Pts',(10.3515730205378,0.24868545684196,25.6948054070466));
#46679=CARTESIAN_POINT('Ctrl Pts',(10.3939151625399,0.649194652036547,26.0396255450656));
#46680=CARTESIAN_POINT('Ctrl Pts',(10.4256717690415,0.791023092992396,26.403820353824));
#46681=CARTESIAN_POINT('Ctrl Pts',(10.4574283755431,0.740250732337037,26.7953245403195));
#46682=CARTESIAN_POINT('Ctrl Pts',(10.4891849820447,0.508988374911209,27.1127335787333));
#46683=CARTESIAN_POINT('Ctrl Pts',(10.5209415885463,0.153681120282412,27.2819876542253));
#46684=CARTESIAN_POINT('Ctrl Pts',(10.5526981950479,-0.239009618237098,
27.2599407330431));
#46685=CARTESIAN_POINT('Ctrl Pts',(10.5844548015495,-0.573625316704213,
27.0532418767055));
#46686=CARTESIAN_POINT('Ctrl Pts',(10.6162114080511,-0.768086580261186,
26.7110796283205));
#46687=CARTESIAN_POINT('Ctrl Pts',(10.6479680145527,-0.776030196845357,
26.3184377118209));
#46688=CARTESIAN_POINT('Ctrl Pts',(10.6797246210543,-0.593564624338813,
25.9683524714423));
#46689=CARTESIAN_POINT('Ctrl Pts',(10.7114812275559,-0.268803421489938,
25.7509051757754));
#46690=CARTESIAN_POINT('Ctrl Pts',(10.753823369558,0.25697906207964,25.6974138359586));
#46691=CARTESIAN_POINT('Ctrl Pts',(10.7961655115601,0.709133976254987,26.0446849521718));
#46692=CARTESIAN_POINT('Ctrl Pts',(10.8385076535623,0.793082515708411,26.5664714853321));
#46693=CARTESIAN_POINT('Ctrl Pts',(10.8702642600639,0.666769034948869,26.9363337162334));
#46694=CARTESIAN_POINT('Ctrl Pts',(10.9020208665655,0.375600348367009,27.2029310842536));
#46695=CARTESIAN_POINT('Ctrl Pts',(10.9337774730671,-0.00580221503551052,
27.2965412346965));
#46696=CARTESIAN_POINT('Ctrl Pts',(10.9655340795687,-0.386547155848502,
27.1969245830134));
#46697=CARTESIAN_POINT('Ctrl Pts',(10.9972906860703,-0.672567178598631,
26.9269530484939));
#46698=CARTESIAN_POINT('Ctrl Pts',(11.0290472925719,-0.795165469044244,
26.5532395993853));
#46699=CARTESIAN_POINT('Ctrl Pts',(11.0608038990735,-0.723293752931155,
26.1662969115487));
#46700=CARTESIAN_POINT('Ctrl Pts',(11.092560505575,-0.476282880095,25.8609832951857));
#46701=CARTESIAN_POINT('Ctrl Pts',(11.1243171120767,-0.111125768016633,
25.7109378214796));
#46702=CARTESIAN_POINT('Ctrl Pts',(11.1560737185782,0.277329037821362,25.7540194775561));
#46703=CARTESIAN_POINT('Ctrl Pts',(11.1984158605804,0.713793524031026,26.0520250072723));
#46704=CARTESIAN_POINT('Ctrl Pts',(11.2407580025825,0.835647851523945,26.6089745718114));
#46705=CARTESIAN_POINT('Ctrl Pts',(11.2831001445846,0.563503958616806,27.0620156792366));
#46706=CARTESIAN_POINT('Ctrl Pts',(11.3148567510862,0.228530189829721,27.2633754058293));
#46707=CARTESIAN_POINT('Ctrl Pts',(11.3466133575878,-0.165922069656989,
27.2795239558244));
#46708=CARTESIAN_POINT('Ctrl Pts',(11.3783699640894,-0.517860513634208,
27.1052537424003));
#46709=CARTESIAN_POINT('Ctrl Pts',(11.410126570591,-0.744748492993213,26.7836763301501));
#46710=CARTESIAN_POINT('Ctrl Pts',(11.4418831770926,-0.789409577719771,
26.3929110932419));
#46711=CARTESIAN_POINT('Ctrl Pts',(11.4736397835942,-0.64225832786655,26.028166535323));
#46712=CARTESIAN_POINT('Ctrl Pts',(11.5053963900958,-0.337898373364977,
25.7786566049734));
#46713=CARTESIAN_POINT('Ctrl Pts',(11.5371529965974,0.0477483654022483,
25.704444958218));
#46714=CARTESIAN_POINT('Ctrl Pts',(11.568909603099,0.423642753883886,25.8250963957939));
#46715=CARTESIAN_POINT('Ctrl Pts',(11.6006662096006,0.692865902039955,26.1084196418678));
#46716=CARTESIAN_POINT('Ctrl Pts',(11.6430083516027,0.834479137823284,26.6175897852527));
#46717=CARTESIAN_POINT('Ctrl Pts',(11.6853504936048,0.568651082127304,27.1219475346471));
#46718=CARTESIAN_POINT('Ctrl Pts',(11.727692635607,0.0685686419494346,27.2929039515766));
#46719=CARTESIAN_POINT('Ctrl Pts',(11.7594492421086,-0.31732463510849,27.2309398975579));
#46720=CARTESIAN_POINT('Ctrl Pts',(11.7912058486102,-0.629310976686018,
26.9890351986573));
#46721=CARTESIAN_POINT('Ctrl Pts',(11.8229624551117,-0.786055773280103,
26.6289493139345));
#46722=CARTESIAN_POINT('Ctrl Pts',(11.8547190616134,-0.752244136277789,
26.2368435113117));
#46723=CARTESIAN_POINT('Ctrl Pts',(11.8864756681149,-0.534515160588541,
25.9092978259331));
#46724=CARTESIAN_POINT('Ctrl Pts',(11.9182322746166,-0.186908610932021,
25.7252821486098));
#46725=CARTESIAN_POINT('Ctrl Pts',(11.9499888811181,0.206614996502733,25.7307004175932));
#46726=CARTESIAN_POINT('Ctrl Pts',(11.9817454876198,0.549294672995457,25.9225373664711));
#46727=CARTESIAN_POINT('Ctrl Pts',(12.0135020941213,0.758915838938966,26.2570703655453));
#46728=CARTESIAN_POINT('Ctrl Pts',(12.0452587006229,0.782128837256907,26.6472169046534));
#46729=CARTESIAN_POINT('Ctrl Pts',(12.0876008426251,0.562204459925782,27.1277809604453));
#46730=CARTESIAN_POINT('Ctrl Pts',(12.1299429846272,0.0338737476163272,
27.3420423732096));
#46731=CARTESIAN_POINT('Ctrl Pts',(12.1722851266293,-0.458655982287092,
27.15040988999));
#46732=CARTESIAN_POINT('Ctrl Pts',(12.2040417331309,-0.713749743328025,
26.8543012302941));
#46733=CARTESIAN_POINT('Ctrl Pts',(12.2357983396325,-0.796354278710274,
26.4682573838007));
#46734=CARTESIAN_POINT('Ctrl Pts',(12.2675549461341,-0.684093539524432,
26.0919220252794));
#46735=CARTESIAN_POINT('Ctrl Pts',(12.2993115526357,-0.405504350759794,
25.8139323651287));
#46736=CARTESIAN_POINT('Ctrl Pts',(12.3310681591373,-0.0279149501101425,
25.7038490903687));
#46737=CARTESIAN_POINT('Ctrl Pts',(12.3628247656389,0.356457281532983,25.7872161726406));
#46738=CARTESIAN_POINT('Ctrl Pts',(12.3945813721405,0.653832357862692,26.0450111516939));
#46739=CARTESIAN_POINT('Ctrl Pts',(12.4263379786421,0.792175442841407,26.4125597423245));
#46740=CARTESIAN_POINT('Ctrl Pts',(12.4580945851437,0.736811757902941,26.8034410837456));
#46741=CARTESIAN_POINT('Ctrl Pts',(12.4898511916453,0.503083492378146,27.1166890097782));
#46742=CARTESIAN_POINT('Ctrl Pts',(12.5321933336474,0.0251849627174119,
27.3423470227353));
#46743=CARTESIAN_POINT('Ctrl Pts',(12.5745354756495,-0.516854899684397,
27.16561535569));
#46744=CARTESIAN_POINT('Ctrl Pts',(12.6168776176517,-0.769897269834191,
26.7016346423272));
#46745=CARTESIAN_POINT('Ctrl Pts',(12.6486342241533,-0.774066619934626,
26.310820387484));
#46746=CARTESIAN_POINT('Ctrl Pts',(12.6803908306549,-0.588390470950266,
25.9624273215664));
#46747=CARTESIAN_POINT('Ctrl Pts',(12.7121474371564,-0.259988325015747,
25.7470606431281));
#46748=CARTESIAN_POINT('Ctrl Pts',(12.7439040436581,0.132189409199892,25.7140938108156));
#46749=CARTESIAN_POINT('Ctrl Pts',(12.7756606501597,0.491830546380316,25.8733116970985));
#46750=CARTESIAN_POINT('Ctrl Pts',(12.8074172566613,0.731965703418775,26.1848035737485));
#46751=CARTESIAN_POINT('Ctrl Pts',(12.8391738631629,0.793156876350488,26.5735783512257));
#46752=CARTESIAN_POINT('Ctrl Pts',(12.8709304696645,0.662016937073565,26.9437581615374));
#46753=CARTESIAN_POINT('Ctrl Pts',(12.902687076166,0.367739430229575,27.2069199172065));
#46754=CARTESIAN_POINT('Ctrl Pts',(12.9344436826677,-0.0128663201484088,
27.2957592556109));
#46755=CARTESIAN_POINT('Ctrl Pts',(12.9767858246698,-0.523694256138937,
27.1602477679971));
#46756=CARTESIAN_POINT('Ctrl Pts',(13.0191279666719,-0.824194056540756,
26.675746824213));
#46757=CARTESIAN_POINT('Ctrl Pts',(13.061470108674,-0.718590181978695,26.1579086592029));
#46758=CARTESIAN_POINT('Ctrl Pts',(13.0932267151756,-0.469871753862732,
25.8564251459149));
#46759=CARTESIAN_POINT('Ctrl Pts',(13.1249833216772,-0.103350723706369,
25.7097428527291));
#46760=CARTESIAN_POINT('Ctrl Pts',(13.1567399281788,0.286546658439126,25.7567620725444));
#46761=CARTESIAN_POINT('Ctrl Pts',(13.1884965346804,0.607634532323689,25.9843423100245));
#46762=CARTESIAN_POINT('Ctrl Pts',(13.220253141182,0.779970642319146,26.3378848789699));
#46763=CARTESIAN_POINT('Ctrl Pts',(13.2520097476836,0.762787909334418,26.7308185076554));
#46764=CARTESIAN_POINT('Ctrl Pts',(13.2837663541852,0.558979957403396,27.0674971466822));
#46765=CARTESIAN_POINT('Ctrl Pts',(13.3155229606868,0.220111430206846,27.265988700436));
#46766=CARTESIAN_POINT('Ctrl Pts',(13.3472795671884,-0.17450318681229,27.2775067174508));
#46767=CARTESIAN_POINT('Ctrl Pts',(13.37903617369,-0.522757319830727,27.1001025909359));
#46768=CARTESIAN_POINT('Ctrl Pts',(13.4213783156921,-0.825963298274264,
26.6672346224978));
#46769=CARTESIAN_POINT('Ctrl Pts',(13.4637204576942,-0.743416216593533,
26.1031182569532));
#46770=CARTESIAN_POINT('Ctrl Pts',(13.5060625996964,-0.328895476366436,
25.7752751551725));
#46771=CARTESIAN_POINT('Ctrl Pts',(13.537819206198,0.0555880103782207,25.7050924387132));
#46772=CARTESIAN_POINT('Ctrl Pts',(13.5695758126996,0.430357382868759,25.8291943247753));
#46773=CARTESIAN_POINT('Ctrl Pts',(13.6013324192012,0.698145424343159,26.1164578631495));
#46774=CARTESIAN_POINT('Ctrl Pts',(13.6330890257028,0.796941593703338,26.497416527793));
#46775=CARTESIAN_POINT('Ctrl Pts',(13.6648456322043,0.700818762673457,26.8787988611799));
#46776=CARTESIAN_POINT('Ctrl Pts',(13.696602238706,0.434409572344521,27.1681398817303));
#46777=CARTESIAN_POINT('Ctrl Pts',(13.7283588452075,0.0615766530934091,
27.2941787708476));
#46778=CARTESIAN_POINT('Ctrl Pts',(13.7601154517091,-0.325445621555236,
27.2275114283046));
#46779=CARTESIAN_POINT('Ctrl Pts',(13.7918720582108,-0.634571402982474,
26.9819618163357));
#46780=CARTESIAN_POINT('Ctrl Pts',(13.8236286647123,-0.786479350664432,
26.6218546924128));
#46781=CARTESIAN_POINT('Ctrl Pts',(13.8659708067145,-0.739282199053725,
26.0954698784758));
#46782=CARTESIAN_POINT('Ctrl Pts',(13.9083129487166,-0.3125600582338,25.7173832361526));
#46783=CARTESIAN_POINT('Ctrl Pts',(13.9506550907188,0.21567771148749,25.7339181115233));
#46784=CARTESIAN_POINT('Ctrl Pts',(13.9824116972203,0.554871109700202,25.9280855750125));
#46785=CARTESIAN_POINT('Ctrl Pts',(14.0141683037219,0.761408101094941,26.2645314575356));
#46786=CARTESIAN_POINT('Ctrl Pts',(14.0459249102235,0.780984108470458,26.6567655146636));
#46787=CARTESIAN_POINT('Ctrl Pts',(14.0776815167251,0.610964975807012,27.0117073152108));
#46788=CARTESIAN_POINT('Ctrl Pts',(14.1094381232267,0.291647913206453,27.241334614104));
#46789=CARTESIAN_POINT('Ctrl Pts',(14.1411947297283,-0.0985343487612529,
27.2908309302356));
#46790=CARTESIAN_POINT('Ctrl Pts',(14.1729513362299,-0.464823397167573,
27.1468777424806));
#46791=CARTESIAN_POINT('Ctrl Pts',(14.2047079427315,-0.717748744514388,
26.8464454800562));
#46792=CARTESIAN_POINT('Ctrl Pts',(14.2364645492331,-0.795816853775414,
26.4594587477287));
#46793=CARTESIAN_POINT('Ctrl Pts',(14.2682211557347,-0.679844423442565,
26.0862248255409));
#46794=CARTESIAN_POINT('Ctrl Pts',(14.3105632977368,-0.304469510421639,
25.714200339602));
#46795=CARTESIAN_POINT('Ctrl Pts',(14.352905439739,0.26548215438068,25.7001862624564));
#46796=CARTESIAN_POINT('Ctrl Pts',(14.3952475817411,0.658687214192637,26.0533127616064));
#46797=CARTESIAN_POINT('Ctrl Pts',(14.4270041882427,0.79286270006155,26.4203960004784));
#46798=CARTESIAN_POINT('Ctrl Pts',(14.4587607947443,0.73390803483815,26.8107518741751));
#46799=CARTESIAN_POINT('Ctrl Pts',(14.4905174012459,0.496053570864849,27.1232515215411));
#46800=CARTESIAN_POINT('Ctrl Pts',(14.5222740077474,0.137281974103891,27.2850326347925));
#46801=CARTESIAN_POINT('Ctrl Pts',(14.5540306142491,-0.254861359535286,
27.2547722853697));
#46802=CARTESIAN_POINT('Ctrl Pts',(14.5857872207506,-0.58507796496343,27.0411158406638));
#46803=CARTESIAN_POINT('Ctrl Pts',(14.6175438272522,-0.772335845023473,
26.6949588335086));
#46804=CARTESIAN_POINT('Ctrl Pts',(14.6493004337538,-0.772060486718305,
26.3022366673227));
#46805=CARTESIAN_POINT('Ctrl Pts',(14.6810570402554,-0.582308270804313,
25.9560467523384));
#46806=CARTESIAN_POINT('Ctrl Pts',(14.712813646757,-0.25306744493287,25.7454437042873));
#46807=CARTESIAN_POINT('Ctrl Pts',(14.7551557887592,0.273719354082281,25.7029676893257));
#46808=CARTESIAN_POINT('Ctrl Pts',(14.7974979307613,0.718507527034393,26.059625474564));
#46809=CARTESIAN_POINT('Ctrl Pts',(14.8398400727634,0.791517698526367,26.5830546085662));
#46810=CARTESIAN_POINT('Ctrl Pts',(14.871596679265,0.657491382035733,26.9501923371599));
#46811=CARTESIAN_POINT('Ctrl Pts',(14.9033532857666,0.360807099282544,27.2106377192428));
#46812=CARTESIAN_POINT('Ctrl Pts',(14.9351098922682,-0.0224710100972664,
27.2962453503641));
#46813=CARTESIAN_POINT('Ctrl Pts',(14.9668664987698,-0.401047778060038,
27.1886822618713));
#46814=CARTESIAN_POINT('Ctrl Pts',(14.9986231052714,-0.681355176354821,
26.912784010108));
#46815=CARTESIAN_POINT('Ctrl Pts',(15.030379711773,-0.796105516889878,26.5365866653381));
#46816=CARTESIAN_POINT('Ctrl Pts',(15.0621363182746,-0.716151580539097,
26.1512328599732));
#46817=CARTESIAN_POINT('Ctrl Pts',(15.0938929247762,-0.462805184149422,
25.8511555714751));
#46818=CARTESIAN_POINT('Ctrl Pts',(15.1256495312778,-0.0945878860313145,
25.7087849914816));
#46819=CARTESIAN_POINT('Ctrl Pts',(15.1574061377794,0.292880226372572,25.7599868189792));
#46820=CARTESIAN_POINT('Ctrl Pts',(15.1997482797815,0.723012441153252,26.067061437389));
#46821=CARTESIAN_POINT('Ctrl Pts',(15.2420904217837,0.833184204547314,26.6264391962602));
#46822=CARTESIAN_POINT('Ctrl Pts',(15.2844325637858,0.551618642248873,27.0736856356996));
#46823=CARTESIAN_POINT('Ctrl Pts',(15.3161891702874,0.21250416882743,27.2679909088782));
#46824=CARTESIAN_POINT('Ctrl Pts',(15.347945776789,-0.182199657223414,27.2758808000015));
#46825=CARTESIAN_POINT('Ctrl Pts',(15.3797023832906,-0.530413882922957,
27.0942833642916));
#46826=CARTESIAN_POINT('Ctrl Pts',(15.4114589897921,-0.750522177579577,
26.7680280564871));
#46827=CARTESIAN_POINT('Ctrl Pts',(15.4432155962938,-0.786995520979564,
26.3764137333501));
#46828=CARTESIAN_POINT('Ctrl Pts',(15.4749722027953,-0.632243102185288,
26.0148286510498));
#46829=CARTESIAN_POINT('Ctrl Pts',(15.5067288092969,-0.32272804759704,25.7717430319143));
#46830=CARTESIAN_POINT('Ctrl Pts',(15.5384854157985,0.0643873344812935,
25.7056184782728));
#46831=CARTESIAN_POINT('Ctrl Pts',(15.5702420223001,0.43767439511808,25.8341102330364));
#46832=CARTESIAN_POINT('Ctrl Pts',(15.6019986288018,0.700909172129369,26.1230057460524));
#46833=CARTESIAN_POINT('Ctrl Pts',(15.6443407708038,0.831835447076346,26.6350280639177));
#46834=CARTESIAN_POINT('Ctrl Pts',(15.686682912806,0.555510380759211,27.1337120844097));
#46835=CARTESIAN_POINT('Ctrl Pts',(15.7290250548081,0.0519596797800127,
27.2941653019125));
#46836=CARTESIAN_POINT('Ctrl Pts',(15.7607816613097,-0.332552292829113,
27.2241388198563));
#46837=CARTESIAN_POINT('Ctrl Pts',(15.7925382678113,-0.639407707442898,
26.9757578318493));
#46838=CARTESIAN_POINT('Ctrl Pts',(15.8242948743129,-0.788582274036148,
26.6124704465499));
#46839=CARTESIAN_POINT('Ctrl Pts',(15.8560514808145,-0.746572027037139,
26.2211581334363));
#46840=CARTESIAN_POINT('Ctrl Pts',(15.8878080873161,-0.522035840432493,
25.8982408316857));
#46841=CARTESIAN_POINT('Ctrl Pts',(15.9195646938177,-0.17065433029262,25.7215401887988));
#46842=CARTESIAN_POINT('Ctrl Pts',(15.9513213003193,0.222669695330672,25.7351929582878));
#46843=CARTESIAN_POINT('Ctrl Pts',(15.9830779068209,0.561259543601463,25.9341595139798));
#46844=CARTESIAN_POINT('Ctrl Pts',(16.0148345133225,0.763833671200898,26.2730062101543));
#46845=CARTESIAN_POINT('Ctrl Pts',(16.0465911198241,0.778876573811572,26.6635531040737));
#46846=CARTESIAN_POINT('Ctrl Pts',(16.0889332618262,0.548943088162816,27.1394093172736));
#46847=CARTESIAN_POINT('Ctrl Pts',(16.1312754038283,0.016244012154183,27.3425668644846));
#46848=CARTESIAN_POINT('Ctrl Pts',(16.1736175458305,-0.47216734905144,27.1406686581801));
#46849=CARTESIAN_POINT('Ctrl Pts',(16.2053741523321,-0.721008259555255,
26.8392862324673));
#46850=CARTESIAN_POINT('Ctrl Pts',(16.2371307588337,-0.795515552951639,
26.4515981827264));
#46851=CARTESIAN_POINT('Ctrl Pts',(16.2688873653352,-0.675403430232317,
26.0776946475575));
#46852=CARTESIAN_POINT('Ctrl Pts',(16.3006439718369,-0.391057471568795,
25.8055962039035));
#46853=CARTESIAN_POINT('Ctrl Pts',(16.3324005783384,-0.0112469392005812,
25.7034392542279));
#46854=CARTESIAN_POINT('Ctrl Pts',(16.3641571848401,0.371296397184491,25.7948322443979));
#46855=CARTESIAN_POINT('Ctrl Pts',(16.3959137913416,0.663211193852015,26.0587942468411));
#46856=CARTESIAN_POINT('Ctrl Pts',(16.4276703978433,0.79383189911164,26.4291575914007));
#46857=CARTESIAN_POINT('Ctrl Pts',(16.4594270043448,0.730299950020167,26.8187946688532));
#46858=CARTESIAN_POINT('Ctrl Pts',(16.4911836108465,0.490067202099917,27.127082508535));
#46859=CARTESIAN_POINT('Ctrl Pts',(16.5335257528485,0.00755075451268908,
27.3426896078416));
#46860=CARTESIAN_POINT('Ctrl Pts',(16.5758678948507,-0.530671740917147,
27.1546528029804));
#46861=CARTESIAN_POINT('Ctrl Pts',(16.6182100368528,-0.773948472755031,
26.6854780218913));
#46862=CARTESIAN_POINT('Ctrl Pts',(16.6499666433544,-0.76993792401264,26.2946621051637));
#46863=CARTESIAN_POINT('Ctrl Pts',(16.681723249856,-0.577011248722235,25.9502311851775));
#46864=CARTESIAN_POINT('Ctrl Pts',(16.7134798563576,-0.244173820480448,
25.7417844965558));
#46865=CARTESIAN_POINT('Ctrl Pts',(16.7452364628592,0.148607952543154,25.7170324051763));
#46866=CARTESIAN_POINT('Ctrl Pts',(16.7769930693608,0.504838200497434,25.8837420128997));
#46867=CARTESIAN_POINT('Ctrl Pts',(16.8087496758624,0.738401842223993,26.2001912317773));
#46868=CARTESIAN_POINT('Ctrl Pts',(16.840506282364,0.791443309939019,26.5901614741675));
#46869=CARTESIAN_POINT('Ctrl Pts',(16.8722628888656,0.652584945679744,26.9575157041844));
#46870=CARTESIAN_POINT('Ctrl Pts',(16.9040194953672,0.352864424260747,27.2144611647807));
#46871=CARTESIAN_POINT('Ctrl Pts',(16.9357761018688,-0.0295172027510032,
27.2953157045016));
#46872=CARTESIAN_POINT('Ctrl Pts',(16.9781182438709,-0.537397266224523,
27.1491432563852));
#46873=CARTESIAN_POINT('Ctrl Pts',(17.0204603858731,-0.82769158569248,26.658459547002));
#46874=CARTESIAN_POINT('Ctrl Pts',(17.0628025278752,-0.711273489859842,
26.1429448814199));
#46875=CARTESIAN_POINT('Ctrl Pts',(17.0945591343768,-0.456300068822577,
25.846732592974));
#46876=CARTESIAN_POINT('Ctrl Pts',(17.1263157408784,-0.0867895361857581,
25.7077530010661));
#46877=CARTESIAN_POINT('Ctrl Pts',(17.1580723473799,0.30203843095996,25.7629217202603));
#46878=CARTESIAN_POINT('Ctrl Pts',(17.1898289538815,0.618293167806677,25.9971718615475));
#46879=CARTESIAN_POINT('Ctrl Pts',(17.2215855603831,0.78319257186756,26.3542436602263));
#46880=CARTESIAN_POINT('Ctrl Pts',(17.2533421668847,0.757790262318726,26.7467316287404));
#46881=CARTESIAN_POINT('Ctrl Pts',(17.2850987733863,0.546980915086662,27.0790712241793));
#46882=CARTESIAN_POINT('Ctrl Pts',(17.316855379888,0.20403256237055,27.2704274425122));
#46883=CARTESIAN_POINT('Ctrl Pts',(17.3486119863895,-0.190736679054125,
27.2736844177905));
#46884=CARTESIAN_POINT('Ctrl Pts',(17.3803685928912,-0.535201811279513,
27.0890308594029));
#46885=CARTESIAN_POINT('Ctrl Pts',(17.4227107348932,-0.829282299959934,
26.6499121849083));
#46886=CARTESIAN_POINT('Ctrl Pts',(17.4650528768954,-0.73494742254484,26.0876469142062));
#46887=CARTESIAN_POINT('Ctrl Pts',(17.5073950188975,-0.313656364480858,
25.7685507409244));
#46888=CARTESIAN_POINT('Ctrl Pts',(17.5391516253991,0.072211731487986,25.7064298750071));
#46889=CARTESIAN_POINT('Ctrl Pts',(17.5709082319007,0.444301753746512,25.8383478091969));
#46890=CARTESIAN_POINT('Ctrl Pts',(17.6026648384023,0.70601938612131,26.1311526579745));
#46891=CARTESIAN_POINT('Ctrl Pts',(17.6344214449039,0.796820980869681,26.5140956120801));
#46892=CARTESIAN_POINT('Ctrl Pts',(17.6661780514055,0.692738004319475,26.8933825384317));
#46893=CARTESIAN_POINT('Ctrl Pts',(17.6979346579071,0.420331066798412,27.1770851633445));
#46894=CARTESIAN_POINT('Ctrl Pts',(17.7296912644087,0.0449434652133512,
27.2952930157502));
#46895=CARTESIAN_POINT('Ctrl Pts',(17.7614478709103,-0.34060148631374,27.2205420816171));
#46896=CARTESIAN_POINT('Ctrl Pts',(17.7932044774119,-0.644515709678365,
26.9685741610806));
#46897=CARTESIAN_POINT('Ctrl Pts',(17.8249610839135,-0.788863074482209,
26.6053716379335));
#46898=CARTESIAN_POINT('Ctrl Pts',(17.8673032259156,-0.730641129956017,
26.08007965548));
#46899=CARTESIAN_POINT('Ctrl Pts',(17.9096453679177,-0.29613832160412,25.711027047467));
#46900=CARTESIAN_POINT('Ctrl Pts',(17.9519875099199,0.231694148623007,25.7385828611072));
#46901=CARTESIAN_POINT('Ctrl Pts',(17.9837441164214,0.566653359359628,25.9398584184328));
#46902=CARTESIAN_POINT('Ctrl Pts',(18.0155007229231,0.766296209055916,26.2804493550768));
#46903=CARTESIAN_POINT('Ctrl Pts',(18.0472573294246,0.777290647856074,26.673205973088));
#46904=CARTESIAN_POINT('Ctrl Pts',(18.0790139359263,0.6005784561905,27.0241353676862));
#46905=CARTESIAN_POINT('Ctrl Pts',(18.1107705424278,0.275214785933559,27.2477375493297));
#46906=CARTESIAN_POINT('Ctrl Pts',(18.1425271489295,-0.113511804048443,
27.2877520601354));
#46907=CARTESIAN_POINT('Ctrl Pts',(18.1848692909315,-0.603105163321842,
27.0885918682123));
#46908=CARTESIAN_POINT('Ctrl Pts',(18.2272114329337,-0.839805528456801,
26.569973072668));
#46909=CARTESIAN_POINT('Ctrl Pts',(18.2695535749358,-0.669488757599245,
26.0696595117695));
#46910=CARTESIAN_POINT('Ctrl Pts',(18.3013101814374,-0.38458849635973,25.8021075061857));
#46911=CARTESIAN_POINT('Ctrl Pts',(18.333066787939,-0.00244655372769168,
25.7030155094137));
#46912=CARTESIAN_POINT('Ctrl Pts',(18.3648233944406,0.378359542695009,25.7990328449791));
#46913=CARTESIAN_POINT('Ctrl Pts',(18.3965800009422,0.668042185748427,26.0654402662492));
#46914=CARTESIAN_POINT('Ctrl Pts',(18.4283366074438,0.794220949673334,26.4379609214166));
#46915=CARTESIAN_POINT('Ctrl Pts',(18.4600932139454,0.7274175711474,26.8255549708114));
#46916=CARTESIAN_POINT('Ctrl Pts',(18.491849820447,0.482615591725175,27.1337143882872));
#46917=CARTESIAN_POINT('Ctrl Pts',(18.5236064269486,0.121339288012704,27.2876956564317));
#46918=CARTESIAN_POINT('Ctrl Pts',(18.5553630334502,-0.271557026497766,
27.2491494235501));
#46919=CARTESIAN_POINT('Ctrl Pts',(18.5871196399518,-0.594542196765398,
27.0290726886231));
#46920=CARTESIAN_POINT('Ctrl Pts',(18.6294617819539,-0.840491465003347,
26.5612933807642));
#46921=CARTESIAN_POINT('Ctrl Pts',(18.671803923956,-0.687172694531139,26.0121716653354));
#46922=CARTESIAN_POINT('Ctrl Pts',(18.7141460659582,-0.234472997417264,
25.7394602274647));
#46923=CARTESIAN_POINT('Ctrl Pts',(18.7459026724598,0.155802722384311,25.7185311453641));
#46924=CARTESIAN_POINT('Ctrl Pts',(18.7776592789614,0.511839522475942,25.8890924505991));
#46925=CARTESIAN_POINT('Ctrl Pts',(18.8094158854629,0.741094448594219,26.2079544172491));
#46926=CARTESIAN_POINT('Ctrl Pts',(18.8411724919646,0.790852991429545,26.5983571259894));
#46927=CARTESIAN_POINT('Ctrl Pts',(18.8729290984662,0.647208072939979,26.964496744374));
#46928=CARTESIAN_POINT('Ctrl Pts',(18.9046857049677,0.346303229108121,27.2177720053648));
#46929=CARTESIAN_POINT('Ctrl Pts',(18.9364423114694,-0.0394890010879801,
27.2955829454142));
#46930=CARTESIAN_POINT('Ctrl Pts',(18.9681989179709,-0.414953219279804,
27.1804421773526));
#46931=CARTESIAN_POINT('Ctrl Pts',(18.9999555244725,-0.690495493529877,
26.8977235614153));
#46932=CARTESIAN_POINT('Ctrl Pts',(19.0317121309741,-0.795578750754377,
26.5212787788603));
#46933=CARTESIAN_POINT('Ctrl Pts',(19.0740542729763,-0.682103411352699,
26.0051083701625));
#46934=CARTESIAN_POINT('Ctrl Pts',(19.1163964149784,-0.210938010442085,
25.6841029814942));
#46935=CARTESIAN_POINT('Ctrl Pts',(19.1587385569805,0.310953319631399,25.7673975374766));
#46936=CARTESIAN_POINT('Ctrl Pts',(19.1904951634821,0.622827872514436,26.002955234302));
#46937=CARTESIAN_POINT('Ctrl Pts',(19.2222517699837,0.78509669838758,26.3628471470069));
#46938=CARTESIAN_POINT('Ctrl Pts',(19.2540083764853,0.754844992184846,26.7544025197296));
#46939=CARTESIAN_POINT('Ctrl Pts',(19.2857649829869,0.54124693951236,27.0849566894835));
#46940=CARTESIAN_POINT('Ctrl Pts',(19.3175215894885,0.195421936564938,27.2722990237309));
#46941=CARTESIAN_POINT('Ctrl Pts',(19.3492781959901,-0.197887083474027,
27.2719865803867));
#46942=CARTESIAN_POINT('Ctrl Pts',(19.3810348024917,-0.542997981900108,
27.0828076834802));
#46943=CARTESIAN_POINT('Ctrl Pts',(19.4127914089933,-0.755842259642186,
26.7527651270297));
#46944=CARTESIAN_POINT('Ctrl Pts',(19.4445480154949,-0.784276255245929,
26.3590077543049));
#46945=CARTESIAN_POINT('Ctrl Pts',(19.4763046219965,-0.621973401147041,
26.0034645799642));
#46946=CARTESIAN_POINT('Ctrl Pts',(19.5186467639986,-0.202509532859472,
25.6819702461652));
#46947=CARTESIAN_POINT('Ctrl Pts',(19.5609889060007,0.364628407821791,25.7402441752329));
#46948=CARTESIAN_POINT('Ctrl Pts',(19.6033310480029,0.709950204635276,26.1403209180076));
#46949=CARTESIAN_POINT('Ctrl Pts',(19.6350876545045,0.796560342324164,26.5214401241865));
#46950=CARTESIAN_POINT('Ctrl Pts',(19.6668442610061,0.688648014289257,26.9011877905904));
#46951=CARTESIAN_POINT('Ctrl Pts',(19.6986008675076,0.413135351067633,27.1810512359355));
#46952=CARTESIAN_POINT('Ctrl Pts',(19.7303574740093,0.0367650668537481,
27.2960972980499));
#46953=CARTESIAN_POINT('Ctrl Pts',(19.7621140805108,-0.348389341911593,
27.2164219300026));
#46954=CARTESIAN_POINT('Ctrl Pts',(19.7938706870124,-0.64889140428939,26.962668913525));
#46955=CARTESIAN_POINT('Ctrl Pts',(19.8256272935141,-0.790806567494741,
26.5955854438622));
#46956=CARTESIAN_POINT('Ctrl Pts',(19.8573839000156,-0.74080149737149,26.2060597468949));
#46957=CARTESIAN_POINT('Ctrl Pts',(19.8891405065173,-0.508737507276705,
25.8866858826192));
#46958=CARTESIAN_POINT('Ctrl Pts',(19.9208971130188,-0.155477746603945,
25.7194713295494));
#46959=CARTESIAN_POINT('Ctrl Pts',(19.963239255021,0.372447071308012,25.7440463187918));
#46960=CARTESIAN_POINT('Ctrl Pts',(20.0055813970231,0.768489532327075,26.154158088483));
#46961=CARTESIAN_POINT('Ctrl Pts',(20.0479235390252,0.774628079308121,26.6826189306506));
#46962=CARTESIAN_POINT('Ctrl Pts',(20.0796801455268,0.595188665990073,27.0298287551329));
#46963=CARTESIAN_POINT('Ctrl Pts',(20.1114367520284,0.267911625081069,27.2506071489466));
#46964=CARTESIAN_POINT('Ctrl Pts',(20.14319335853,-0.12312173971539,27.2869896069711));
#46965=CARTESIAN_POINT('Ctrl Pts',(20.1749499650316,-0.485029654910406,
27.132351810277));
#46966=CARTESIAN_POINT('Ctrl Pts',(20.2067065715332,-0.728142381884628,
26.8231782589373));
#46967=CARTESIAN_POINT('Ctrl Pts',(20.2384631780348,-0.794329601343219,
26.4354782011024));
#46968=CARTESIAN_POINT('Ctrl Pts',(20.2702197845364,-0.666220487545662,
26.0633515530251));
#46969=CARTESIAN_POINT('Ctrl Pts',(20.301976391038,-0.376913700709203,25.7977722640617));
#46970=CARTESIAN_POINT('Ctrl Pts',(20.3337329975396,0.00636821150313297,
25.7031766169527));
#46971=CARTESIAN_POINT('Ctrl Pts',(20.3654896040411,0.384233136322356,25.8030328328849));
#46972=CARTESIAN_POINT('Ctrl Pts',(20.4078317460434,0.77201653498693,26.1621046630022));
#46973=CARTESIAN_POINT('Ctrl Pts',(20.4501738880454,0.81046519188054,26.7309306428521));
#46974=CARTESIAN_POINT('Ctrl Pts',(20.4925160300476,0.474529817347993,27.1389207991076));
#46975=CARTESIAN_POINT('Ctrl Pts',(20.5242726365491,0.113539747006181,27.2887184438939));
#46976=CARTESIAN_POINT('Ctrl Pts',(20.5560292430508,-0.278985653677384,
27.2465619438101));
#46977=CARTESIAN_POINT('Ctrl Pts',(20.5877858495523,-0.601400203401613,
27.0223307377703));
#46978=CARTESIAN_POINT('Ctrl Pts',(20.619542456054,-0.778421549050925,26.670828774146));
#46979=CARTESIAN_POINT('Ctrl Pts',(20.6512990625556,-0.76500962662566,26.2777483711726));
#46980=CARTESIAN_POINT('Ctrl Pts',(20.6830556690571,-0.565714119049419,
25.9386711181391));
#46981=CARTESIAN_POINT('Ctrl Pts',(20.7148122755588,-0.227907934100152,
25.7367375432753));
#46982=CARTESIAN_POINT('Ctrl Pts',(20.7465688820603,0.164464593988673,25.7201672434249));
#46983=CARTESIAN_POINT('Ctrl Pts',(20.778325488562,0.518475108459405,25.8948953645883));
#46984=CARTESIAN_POINT('Ctrl Pts',(20.8100820950635,0.743006763321614,26.2147995709279));
#46985=CARTESIAN_POINT('Ctrl Pts',(20.8524242370657,0.808039650977486,26.739279567674));
#46986=CARTESIAN_POINT('Ctrl Pts',(20.8947663790678,0.470788843887705,27.1989568323787));
#46987=CARTESIAN_POINT('Ctrl Pts',(20.9371085210699,-0.0490268475710841,
27.2943517503612));
#46988=CARTESIAN_POINT('Ctrl Pts',(20.9688651275715,-0.421575592023053,
27.1761967746885));
#46989=CARTESIAN_POINT('Ctrl Pts',(21.0006217340731,-0.694507228865489,
26.8909570819885));
#46990=CARTESIAN_POINT('Ctrl Pts',(21.0323783405747,-0.796476381207539,
26.5117037792914));
#46991=CARTESIAN_POINT('Ctrl Pts',(21.0641349470763,-0.705250943174314,
26.1288616359701));
#46992=CARTESIAN_POINT('Ctrl Pts',(21.0958915535779,-0.441630110964222,
25.8369778582611));
#46993=CARTESIAN_POINT('Ctrl Pts',(21.1276481600795,-0.0707011018639236,
25.70619654051));
#46994=CARTESIAN_POINT('Ctrl Pts',(21.1594047665811,0.317727575909635,25.7695475431092));
#46995=CARTESIAN_POINT('Ctrl Pts',(21.1911613730827,0.628395710084807,26.009789267304));
#46996=CARTESIAN_POINT('Ctrl Pts',(21.2229179795843,0.786429550765298,26.3715608331863));
#46997=CARTESIAN_POINT('Ctrl Pts',(21.2546745860859,0.751894885449026,26.7608685805538));
#46998=CARTESIAN_POINT('Ctrl Pts',(21.297016728088,0.463552958450529,27.2037765581276));
#46999=CARTESIAN_POINT('Ctrl Pts',(21.3393588700901,-0.0905842644351466,
27.3378408441313));
#47000=CARTESIAN_POINT('Ctrl Pts',(21.3817010120923,-0.549496531103895,
27.0757185921867));
#47001=CARTESIAN_POINT('Ctrl Pts',(21.4134576185938,-0.758168930798584,
26.7452507497653));
#47002=CARTESIAN_POINT('Ctrl Pts',(21.4452142250955,-0.782981966253044,
26.3512486254657));
#47003=CARTESIAN_POINT('Ctrl Pts',(21.476970831597,-0.616487950568337,25.9955654541219));
#47004=CARTESIAN_POINT('Ctrl Pts',(21.5087274380987,-0.299974232084392,
25.7616653616493));
#47005=CARTESIAN_POINT('Ctrl Pts',(21.5404840446002,0.0897151756284967,
25.7084277022228));
#47006=CARTESIAN_POINT('Ctrl Pts',(21.5722406511019,0.457605408654088,25.8475278794664));
#47007=CARTESIAN_POINT('Ctrl Pts',(21.6039972576034,0.713743622414307,26.1463311637505));
#47008=CARTESIAN_POINT('Ctrl Pts',(21.6357538641051,0.796412224677964,26.5302539135788));
#47009=CARTESIAN_POINT('Ctrl Pts',(21.6675104706066,0.684050486030751,26.9087089312087));
#47010=CARTESIAN_POINT('Ctrl Pts',(21.6992670771083,0.406712042690736,27.184093304612));
#47011=CARTESIAN_POINT('Ctrl Pts',(21.7416092191103,-0.0992230806999048,
27.3368617384697));
#47012=CARTESIAN_POINT('Ctrl Pts',(21.7839513611125,-0.609300801297396,
27.0821815203151));
#47013=CARTESIAN_POINT('Ctrl Pts',(21.8262935031146,-0.791205620922703,
26.5859767439771));
#47014=CARTESIAN_POINT('Ctrl Pts',(21.8580501096162,-0.737736826165347,
26.1988149518847));
#47015=CARTESIAN_POINT('Ctrl Pts',(21.8898067161178,-0.502746680944055,
25.8815879159468));
#47016=CARTESIAN_POINT('Ctrl Pts',(21.9215633226194,-0.146192340398604,
25.7169678142758));
#47017=CARTESIAN_POINT('Ctrl Pts',(21.953319929121,0.246561806406779,25.7421544657884));
#47018=CARTESIAN_POINT('Ctrl Pts',(21.9850765356226,0.578813148913968,25.9526327978489));
#47019=CARTESIAN_POINT('Ctrl Pts',(22.0168331421242,0.770423302724975,26.2961115189095));
#47020=CARTESIAN_POINT('Ctrl Pts',(22.0485897486258,0.773654319674137,26.6896591625013));
#47021=CARTESIAN_POINT('Ctrl Pts',(22.0803463551274,0.589394342448357,27.0364718445485));
#47022=CARTESIAN_POINT('Ctrl Pts',(22.112102961629,0.259548714643134,27.253394002243));
#47023=CARTESIAN_POINT('Ctrl Pts',(22.1438595681306,-0.129993482523563,
27.2851751585385));
#47024=CARTESIAN_POINT('Ctrl Pts',(22.1862017101327,-0.615274487721257,
27.0758646488693));
#47025=CARTESIAN_POINT('Ctrl Pts',(22.2285438521349,-0.841094622237496,
26.5523700821198));
#47026=CARTESIAN_POINT('Ctrl Pts',(22.2708859941369,-0.660332128994326,
26.055748028139));
#47027=CARTESIAN_POINT('Ctrl Pts',(22.3026426006386,-0.369900855742956,
25.7942086605736));
#47028=CARTESIAN_POINT('Ctrl Pts',(22.3343992071401,0.01423446586742,25.7031404697911));
#47029=CARTESIAN_POINT('Ctrl Pts',(22.3661558136418,0.392945955132557,25.8071038457199));
#47030=CARTESIAN_POINT('Ctrl Pts',(22.3979124201434,0.676990688980436,26.0795167243078));
#47031=CARTESIAN_POINT('Ctrl Pts',(22.4296690266449,0.79534519032439,26.4545957758109));
#47032=CARTESIAN_POINT('Ctrl Pts',(22.4614256331466,0.720445109942096,26.8407072374687));
#47033=CARTESIAN_POINT('Ctrl Pts',(22.4931822396481,0.469247428456909,27.1436757375867));
#47034=CARTESIAN_POINT('Ctrl Pts',(22.5249388461498,0.104827792755421,27.290062570161));
#47035=CARTESIAN_POINT('Ctrl Pts',(22.5566954526513,-0.287175811024369,
27.2433021669895));
#47036=CARTESIAN_POINT('Ctrl Pts',(22.5884520591529,-0.605484443472687,
27.0165142048358));
#47037=CARTESIAN_POINT('Ctrl Pts',(22.630794201155,-0.841590140778907,26.5436900904305));
#47038=CARTESIAN_POINT('Ctrl Pts',(22.6731363431572,-0.676812887645703,
25.9978973171006));
#47039=CARTESIAN_POINT('Ctrl Pts',(22.7154784851593,-0.218505020300182,
25.7347197303026));
#47040=CARTESIAN_POINT('Ctrl Pts',(22.7472350916609,0.172123229852927,25.7219629497037));
#47041=CARTESIAN_POINT('Ctrl Pts',(22.7789916981625,0.524512533349801,25.899938058812));
#47042=CARTESIAN_POINT('Ctrl Pts',(22.8107483046641,0.747044085909005,26.2235280520929));
#47043=CARTESIAN_POINT('Ctrl Pts',(22.8425049111657,0.788621357728243,26.6148866059988));
#47044=CARTESIAN_POINT('Ctrl Pts',(22.8742615176673,0.637345306587861,26.9779398241586));
#47045=CARTESIAN_POINT('Ctrl Pts',(22.9060181241689,0.331205804787041,27.2248622579349));
#47046=CARTESIAN_POINT('Ctrl Pts',(22.9377747306705,-0.0561303630539786,
27.2945822717721));
#47047=CARTESIAN_POINT('Ctrl Pts',(22.9695313371721,-0.429102675280415,
27.1716089821991));
#47048=CARTESIAN_POINT('Ctrl Pts',(23.0012879436737,-0.698667848123337,
26.8831857198376));
#47049=CARTESIAN_POINT('Ctrl Pts',(23.0330445501753,-0.795849829993106,
26.5046241955528));
#47050=CARTESIAN_POINT('Ctrl Pts',(23.0753866921774,-0.671596896209279,
25.9909416555441));
#47051=CARTESIAN_POINT('Ctrl Pts',(23.1177288341795,-0.193816666742857,
25.679867151767));
#47052=CARTESIAN_POINT('Ctrl Pts',(23.1600709761817,0.326217167037633,25.7740656400097));
#47053=CARTESIAN_POINT('Ctrl Pts',(23.1918275826833,0.633093647904743,26.0160986765141));
#47054=CARTESIAN_POINT('Ctrl Pts',(23.2235841891849,0.787795093385811,26.3793077395167));
#47055=CARTESIAN_POINT('Ctrl Pts',(23.2553407956864,0.749355516936845,26.7701442457419));
#47056=CARTESIAN_POINT('Ctrl Pts',(23.2870974021881,0.528886386857991,27.0961558251828));
#47057=CARTESIAN_POINT('Ctrl Pts',(23.3188540086896,0.179216412751493,27.2762196807263));
#47058=CARTESIAN_POINT('Ctrl Pts',(23.3506106151912,-0.213999927519153,
27.2676761095181));
#47059=CARTESIAN_POINT('Ctrl Pts',(23.3823672216928,-0.55507609312846,27.071316142874));
#47060=CARTESIAN_POINT('Ctrl Pts',(23.4141238281944,-0.760966602883749,
26.7368914523551));
#47061=CARTESIAN_POINT('Ctrl Pts',(23.445880434696,-0.781153791542167,26.3426252502845));
#47062=CARTESIAN_POINT('Ctrl Pts',(23.4776370411976,-0.611445654087914,
25.9905566300544));
#47063=CARTESIAN_POINT('Ctrl Pts',(23.5199791831997,-0.185345401108989,
25.6779112752593));
#47064=CARTESIAN_POINT('Ctrl Pts',(23.5623213252019,0.380448766828713,25.7480415404581));
#47065=CARTESIAN_POINT('Ctrl Pts',(23.604663467204,0.717322101045798,26.1552575766811));
#47066=CARTESIAN_POINT('Ctrl Pts',(23.6364200737056,0.795937182645239,26.538105894183));
#47067=CARTESIAN_POINT('Ctrl Pts',(23.6681766802072,0.680101105708285,26.915511993711));
#47068=CARTESIAN_POINT('Ctrl Pts',(23.6999332867088,0.398791784083484,27.1895481978939));
#47069=CARTESIAN_POINT('Ctrl Pts',(23.7316898932104,0.0200962396143968,
27.296692361741));
#47070=CARTESIAN_POINT('Ctrl Pts',(23.763446499712,-0.363306363014758,27.2089739077987));
#47071=CARTESIAN_POINT('Ctrl Pts',(23.7952031062136,-0.658432051321634,
26.9489875409133));
#47072=CARTESIAN_POINT('Ctrl Pts',(23.8269597127152,-0.792633786547248,
26.5790144587714));
#47073=CARTESIAN_POINT('Ctrl Pts',(23.8587163192167,-0.734487649662804,
26.1906205834317));
#47074=CARTESIAN_POINT('Ctrl Pts',(23.8904729257184,-0.495790608642908,
25.8761733171223));
#47075=CARTESIAN_POINT('Ctrl Pts',(23.9222295322199,-0.139108740631515,
25.7163884295363));
#47076=CARTESIAN_POINT('Ctrl Pts',(23.9645716742221,0.388186146399965,25.752006480776));
#47077=CARTESIAN_POINT('Ctrl Pts',(24.0069138162242,0.775559022505738,26.170316831385));
#47078=CARTESIAN_POINT('Ctrl Pts',(24.0492559582264,0.770636562786746,26.6987904001223));
#47079=CARTESIAN_POINT('Ctrl Pts',(24.0810125647279,0.583970020170633,27.0421688606243));
#47080=CARTESIAN_POINT('Ctrl Pts',(24.1127691712296,0.252144193813407,27.2560496256394));
#47081=CARTESIAN_POINT('Ctrl Pts',(24.1445257777311,-0.139564942859222,
27.2842405440908));
#47082=CARTESIAN_POINT('Ctrl Pts',(24.1762823842328,-0.498157324775064,
27.1220625835686));
#47083=CARTESIAN_POINT('Ctrl Pts',(24.2080389907343,-0.734746402362433,
26.8078688674774));
#47084=CARTESIAN_POINT('Ctrl Pts',(24.2397955972359,-0.79280531419185,26.418868551768));
#47085=CARTESIAN_POINT('Ctrl Pts',(24.2715522037375,-0.656936368068052,
26.0495044810648));
#47086=CARTESIAN_POINT('Ctrl Pts',(24.3033088102391,-0.362134883698147,
25.7900379891063));
#47087=CARTESIAN_POINT('Ctrl Pts',(24.3350654167407,0.0230427874213672,
25.7034844082904));
#47088=CARTESIAN_POINT('Ctrl Pts',(24.3668220232423,0.398735156543778,25.8112267354052));
#47089=CARTESIAN_POINT('Ctrl Pts',(24.4091641652445,0.778918946276761,26.178335478815));
#47090=CARTESIAN_POINT('Ctrl Pts',(24.4515063072465,0.805454755862356,26.7478415326711));
#47091=CARTESIAN_POINT('Ctrl Pts',(24.4938484492488,0.461054512471806,27.1487118556139));
#47092=CARTESIAN_POINT('Ctrl Pts',(24.5256050557503,0.0970085300212661,
27.2909218690818));
#47093=CARTESIAN_POINT('Ctrl Pts',(24.5573616622519,-0.294548647426862,
27.2405598052841));
#47094=CARTESIAN_POINT('Ctrl Pts',(24.5891182687535,-0.612199858231308,
27.0096301971554));
#47095=CARTESIAN_POINT('Ctrl Pts',(24.6208748752551,-0.781826177841934,
26.6545005040255));
#47096=CARTESIAN_POINT('Ctrl Pts',(24.6526314817566,-0.760190781059477,
26.2617868774846));
#47097=CARTESIAN_POINT('Ctrl Pts',(24.6843880882583,-0.553842691960536,
25.9269547568778));
#47098=CARTESIAN_POINT('Ctrl Pts',(24.7161446947598,-0.211884413187848,
25.7321350380964));
#47099=CARTESIAN_POINT('Ctrl Pts',(24.7479013012615,0.180748963367304,25.7237799647362));
#47100=CARTESIAN_POINT('Ctrl Pts',(24.7796579077631,0.531025222621527,25.90587857232));
#47101=CARTESIAN_POINT('Ctrl Pts',(24.8114145142647,0.74881272581408,26.2304117273629));
#47102=CARTESIAN_POINT('Ctrl Pts',(24.8537566562668,0.802855019359397,26.7561378670706));
#47103=CARTESIAN_POINT('Ctrl Pts',(24.8960987982689,0.456057920405105,27.2086564487069));
#47104=CARTESIAN_POINT('Ctrl Pts',(24.9384409402711,-0.0656403540824771,
27.2931517376899));
#47105=CARTESIAN_POINT('Ctrl Pts',(24.9701975467727,-0.435634749553036,
27.1672259159165));
#47106=CARTESIAN_POINT('Ctrl Pts',(25.0019541532743,-0.702537095515253,
26.8763367645186));
#47107=CARTESIAN_POINT('Ctrl Pts',(25.0337107597758,-0.796546877646502,
26.4950325073963));
#47108=CARTESIAN_POINT('Ctrl Pts',(25.0654673662775,-0.697329274606203,
26.1141833843906));
#47109=CARTESIAN_POINT('Ctrl Pts',(25.097223972779,-0.427657617209193,25.827880607489));
#47110=CARTESIAN_POINT('Ctrl Pts',(25.1289805792807,-0.0540728476927859,
25.7048907589234));
#47111=CARTESIAN_POINT('Ctrl Pts',(25.1607371857822,0.33294494419036,25.7763569468244));
#47112=CARTESIAN_POINT('Ctrl Pts',(25.1924937922838,0.638517242951082,26.0230477368148));
#47113=CARTESIAN_POINT('Ctrl Pts',(25.2242503987854,0.788945293266577,26.3880474112795));
#47114=CARTESIAN_POINT('Ctrl Pts',(25.256007005287,0.746270734187485,26.7765471503739));
#47115=CARTESIAN_POINT('Ctrl Pts',(25.2983491472892,0.44872275221358,27.2133236857863));
#47116=CARTESIAN_POINT('Ctrl Pts',(25.3406912892913,-0.108098811743075,
27.335761590382));
#47117=CARTESIAN_POINT('Ctrl Pts',(25.3830334312934,-0.561424858091366,
27.0640926021514));
#47118=CARTESIAN_POINT('Ctrl Pts',(25.4147900377951,-0.763135503094323,
26.7293300281363));
#47119=CARTESIAN_POINT('Ctrl Pts',(25.4465466442966,-0.779697402476066,
26.3348949077807));
#47120=CARTESIAN_POINT('Ctrl Pts',(25.4783032507982,-0.605796091498349,
25.9827740341064));
#47121=CARTESIAN_POINT('Ctrl Pts',(25.5100598572998,-0.284456618484401,
25.7555491887942));
#47122=CARTESIAN_POINT('Ctrl Pts',(25.5418164638014,0.106261602193242,25.710478634078));
#47123=CARTESIAN_POINT('Ctrl Pts',(25.5735730703029,0.471160163992154,25.857247576466));
#47124=CARTESIAN_POINT('Ctrl Pts',(25.6053296768046,0.720988905220201,26.1613458949732));
#47125=CARTESIAN_POINT('Ctrl Pts',(25.6370862833062,0.795604641852137,26.5469146534013));
#47126=CARTESIAN_POINT('Ctrl Pts',(25.6688428898078,0.675347181544284,26.9229352697116));
#47127=CARTESIAN_POINT('Ctrl Pts',(25.7005994963094,0.392306217773594,27.1924551729066));
#47128=CARTESIAN_POINT('Ctrl Pts',(25.7429416383115,-0.116715244884512,
27.3346019054481));
#47129=CARTESIAN_POINT('Ctrl Pts',(25.7852837803136,-0.621351287349472,
27.0693025272348));
#47130=CARTESIAN_POINT('Ctrl Pts',(25.8276259223158,-0.792831660382392,
26.5693995118972));
#47131=CARTESIAN_POINT('Ctrl Pts',(25.8593825288174,-0.731272031625445,
26.1834415128479));
#47132=CARTESIAN_POINT('Ctrl Pts',(25.8911391353189,-0.489694400926831,
25.8712018432531));
#47133=CARTESIAN_POINT('Ctrl Pts',(25.9228957418205,-0.129772979866902,
25.714079788392));
#47134=CARTESIAN_POINT('Ctrl Pts',(25.9546523483221,0.262368055635802,25.7474805067894));
#47135=CARTESIAN_POINT('Ctrl Pts',(25.9864089548237,0.590141695668152,25.9648661194057));
#47136=CARTESIAN_POINT('Ctrl Pts',(26.0181655613253,0.774521596165084,26.3122796401661));
#47137=CARTESIAN_POINT('Ctrl Pts',(26.0499221678269,0.769515607711255,26.7058087142711));
#47138=CARTESIAN_POINT('Ctrl Pts',(26.0816787743285,0.5780380710276,27.0486892252408));
#47139=CARTESIAN_POINT('Ctrl Pts',(26.1134353808301,0.243724544676253,27.2586608600213));
#47140=CARTESIAN_POINT('Ctrl Pts',(26.1451919873318,-0.146396766368369,
27.282282661157));
#47141=CARTESIAN_POINT('Ctrl Pts',(26.1875341293338,-0.627192464881676,
27.062862066019));
#47142=CARTESIAN_POINT('Ctrl Pts',(26.2298762713361,-0.842004480180732,
26.534756044308));
#47143=CARTESIAN_POINT('Ctrl Pts',(26.2722184133381,-0.650892539114633,
26.0420259586536));
#47144=CARTESIAN_POINT('Ctrl Pts',(26.3039750198397,-0.355044020423166,
25.7866217100636));
#47145=CARTESIAN_POINT('Ctrl Pts',(26.3357316263413,0.0308983993041465,
25.7036133259667));
#47146=CARTESIAN_POINT('Ctrl Pts',(26.3674882328429,0.407379290301616,25.8154783693755));
#47147=CARTESIAN_POINT('Ctrl Pts',(26.3992448393445,0.685607456858645,26.0937785591144));
#47148=CARTESIAN_POINT('Ctrl Pts',(26.4310014458461,0.796187063432195,26.4712471071119));
#47149=CARTESIAN_POINT('Ctrl Pts',(26.4627580523477,0.713032807660742,26.855721513956));
#47150=CARTESIAN_POINT('Ctrl Pts',(26.4839291233488,0.541616553385129,27.0541076712552));
#47151=CARTESIAN_POINT('Ctrl Pts',(26.4945146588493,0.437388125541368,27.1268353453143));
#47152=CARTESIAN_POINT('',(26.4075,0.887101818743898,26.8183655338816));
#47153=CARTESIAN_POINT('Ctrl Pts',(26.4428553390594,0.547713856063084,27.2849429494197));
#47154=CARTESIAN_POINT('Ctrl Pts',(26.4403015215003,0.582091546070041,27.2596651488676));
#47155=CARTESIAN_POINT('Ctrl Pts',(26.4377478434971,0.614688075782228,27.2320922094722));
#47156=CARTESIAN_POINT('Ctrl Pts',(26.4351883782295,0.645331373578053,27.2024576259984));
#47157=CARTESIAN_POINT('Ctrl Pts',(26.4334556727824,0.666076257160053,27.1823956213061));
#47158=CARTESIAN_POINT('Ctrl Pts',(26.4317203150251,0.68592535478861,27.1613878091695));
#47159=CARTESIAN_POINT('Ctrl Pts',(26.4299804660993,0.704814988397489,27.1394978057222));
#47160=CARTESIAN_POINT('Ctrl Pts',(26.429150320803,0.713827920644061,27.1290532877378));
#47161=CARTESIAN_POINT('Ctrl Pts',(26.4283191530511,0.722622287140125,27.1184078428865));
#47162=CARTESIAN_POINT('Ctrl Pts',(26.4274867630985,0.731190377254997,27.1075679654722));
#47163=CARTESIAN_POINT('Ctrl Pts',(26.4269700334783,0.736509261675482,27.1008388047929));
#47164=CARTESIAN_POINT('Ctrl Pts',(26.4264526784239,0.741742465290211,27.0940326563995));
#47165=CARTESIAN_POINT('Ctrl Pts',(26.4259351560647,0.746883024781805,27.0871577648099));
#47166=CARTESIAN_POINT('Ctrl Pts',(26.4233544388515,0.772517338217262,27.0528748961589));
#47167=CARTESIAN_POINT('Ctrl Pts',(26.4207778202209,0.795770458426538,27.0169961987609));
#47168=CARTESIAN_POINT('Ctrl Pts',(26.4181993932428,0.81646839864648,26.9797548648337));
#47169=CARTESIAN_POINT('Ctrl Pts',(26.4168907728525,0.826973154778107,26.9608538956183));
#47170=CARTESIAN_POINT('Ctrl Pts',(26.4155816866621,0.836819115669743,26.941601383311));
#47171=CARTESIAN_POINT('Ctrl Pts',(26.4142713624564,0.845979193354906,26.9220250507742));
#47172=CARTESIAN_POINT('Ctrl Pts',(26.4120192059813,0.861723333759698,26.8883776802318));
#47173=CARTESIAN_POINT('Ctrl Pts',(26.4097633921638,0.875442884267091,26.8537738979748));
#47174=CARTESIAN_POINT('Ctrl Pts',(26.4074999999956,0.887094662747573,26.8184069534176));
#47175=CARTESIAN_POINT('Ctrl Pts',(26.4075,0.702460755335681,26.1986212829383));
#47176=CARTESIAN_POINT('Ctrl Pts',(26.4075,0.724104732401363,26.224024074543));
#47177=CARTESIAN_POINT('Ctrl Pts',(26.4075,0.743985347108709,26.2508566613889));
#47178=CARTESIAN_POINT('Ctrl Pts',(26.4075,0.762051830778776,26.2788529213646));
#47179=CARTESIAN_POINT('Ctrl Pts',(26.4075,0.781091487998052,26.3083572346052));
#47180=CARTESIAN_POINT('Ctrl Pts',(26.4075,0.79811757528923,26.3391539940486));
#47181=CARTESIAN_POINT('Ctrl Pts',(26.4075,0.813068246637555,26.3709924441191));
#47182=CARTESIAN_POINT('Ctrl Pts',(26.4075,0.818689978394547,26.3829642961975));
#47183=CARTESIAN_POINT('Ctrl Pts',(26.4075,0.824018141973892,26.3950840167916));
#47184=CARTESIAN_POINT('Ctrl Pts',(26.4075,0.829048786022781,26.4073402559923));
#47185=CARTESIAN_POINT('Ctrl Pts',(26.4075,0.832452526428086,26.415632843617));
#47186=CARTESIAN_POINT('Ctrl Pts',(26.4075,0.835716738922779,26.4239799751948));
#47187=CARTESIAN_POINT('Ctrl Pts',(26.4075,0.838839667726155,26.4323745124417));
#47188=CARTESIAN_POINT('Ctrl Pts',(26.4075,0.843376079903281,26.4445685403514));
#47189=CARTESIAN_POINT('Ctrl Pts',(26.4075,0.847615144743271,26.4568644216205));
#47190=CARTESIAN_POINT('Ctrl Pts',(26.4075,0.851554819573637,26.4692493635078));
#47191=CARTESIAN_POINT('Ctrl Pts',(26.4075,0.862536111498967,26.5037706547816));
#47192=CARTESIAN_POINT('Ctrl Pts',(26.4075,0.871193227879546,26.5389805248123));
#47193=CARTESIAN_POINT('Ctrl Pts',(26.4075,0.87759612970566,26.5746307452721));
#47194=CARTESIAN_POINT('Ctrl Pts',(26.4075,0.881461513193471,26.5961525141895));
#47195=CARTESIAN_POINT('Ctrl Pts',(26.4075,0.884504926078275,26.6178357226439));
#47196=CARTESIAN_POINT('Ctrl Pts',(26.4075,0.886736695632634,26.6396330336608));
#47197=CARTESIAN_POINT('Ctrl Pts',(26.4075,0.887583223161862,26.6479009230596));
#47198=CARTESIAN_POINT('Ctrl Pts',(26.4075,0.888312931455761,26.6561852775869));
#47199=CARTESIAN_POINT('Ctrl Pts',(26.4075,0.888926212894426,26.6644836796199));
#47200=CARTESIAN_POINT('Ctrl Pts',(26.4075,0.889537315014905,26.6727525929756));
#47201=CARTESIAN_POINT('Ctrl Pts',(26.4075,0.890032032238849,26.6810245992922));
#47202=CARTESIAN_POINT('Ctrl Pts',(26.4075,0.890411592374961,26.6892991424034));
#47203=CARTESIAN_POINT('Ctrl Pts',(26.4075,0.892188989170611,26.72804701135));
#47204=CARTESIAN_POINT('Ctrl Pts',(26.4075,0.891442494227263,26.766834586409));
#47205=CARTESIAN_POINT('Ctrl Pts',(26.4075,0.888261545772562,26.8053932068493));
#47206=CARTESIAN_POINT('Ctrl Pts',(26.4075,0.887903437733349,26.8097340983027));
#47207=CARTESIAN_POINT('Ctrl Pts',(26.4075,0.887514442749773,26.8140721311828));
#47208=CARTESIAN_POINT('Ctrl Pts',(26.4075,0.887094662732194,26.8184069534123));
#47209=CARTESIAN_POINT('',(9.6,0.66215021624593,26.1181780341239));
#47210=CARTESIAN_POINT('Ctrl Pts',(9.60000000000002,0.662150216245817,26.1181780341239));
#47211=CARTESIAN_POINT('Ctrl Pts',(9.61058553550055,0.725638504704611,26.2282785199239));
#47212=CARTESIAN_POINT('Ctrl Pts',(9.63175660650163,0.796605391005151,26.480675629033));
#47213=CARTESIAN_POINT('Ctrl Pts',(9.6635132130032,0.708650864432033,26.8640803773426));
#47214=CARTESIAN_POINT('Ctrl Pts',(9.69526981950482,0.448266436304386,27.1588859127484));
#47215=CARTESIAN_POINT('Ctrl Pts',(9.7270264260064,0.0782001173243299,27.2927247256205));
#47216=CARTESIAN_POINT('Ctrl Pts',(9.75878303250801,-0.310157515624281,
27.2341585395261));
#47217=CARTESIAN_POINT('Ctrl Pts',(9.7905396390096,-0.624341483803593,26.9951389225185));
#47218=CARTESIAN_POINT('Ctrl Pts',(9.81537842347006,-0.749031686158336,
26.716022731786));
#47219=CARTESIAN_POINT('Ctrl Pts',(9.82963167242999,-0.764213466994258,
26.5441969818453));
#47220=CARTESIAN_POINT('Ctrl Pts',(9.83329938588939,-0.764354837691052,
26.4999637734947));
#47221=CARTESIAN_POINT('Ctrl Pts',(9.6,0.899181451069003,26.9202569089796));
#47222=CARTESIAN_POINT('Ctrl Pts',(9.6,0.907250892683643,26.8807649655044));
#47223=CARTESIAN_POINT('Ctrl Pts',(9.6,0.912814425070195,26.8408626129725));
#47224=CARTESIAN_POINT('Ctrl Pts',(9.6,0.915826552715021,26.8007896179812));
#47225=CARTESIAN_POINT('Ctrl Pts',(9.6,0.918777836392666,26.7615260840352));
#47226=CARTESIAN_POINT('Ctrl Pts',(9.6,0.919279144120976,26.722097769122));
#47227=CARTESIAN_POINT('Ctrl Pts',(9.6,0.917249439708845,26.6827606307352));
#47228=CARTESIAN_POINT('Ctrl Pts',(9.6,0.91650588615301,26.6683500254524));
#47229=CARTESIAN_POINT('Ctrl Pts',(9.6,0.915422334890081,26.6539520254147));
#47230=CARTESIAN_POINT('Ctrl Pts',(9.6,0.913993735787157,26.6395806368628));
#47231=CARTESIAN_POINT('Ctrl Pts',(9.6,0.912867742205004,26.6282533924016));
#47232=CARTESIAN_POINT('Ctrl Pts',(9.6,0.911526840337707,26.6169401702507));
#47233=CARTESIAN_POINT('Ctrl Pts',(9.6,0.909972044783114,26.6056708003737));
#47234=CARTESIAN_POINT('Ctrl Pts',(9.6,0.90487132111677,26.5687000607378));
#47235=CARTESIAN_POINT('Ctrl Pts',(9.6,0.897466999839062,26.5321448048616));
#47236=CARTESIAN_POINT('Ctrl Pts',(9.6,0.887699646549959,26.4962326846631));
#47237=CARTESIAN_POINT('Ctrl Pts',(9.6,0.886096693095341,26.4903390248936));
#47238=CARTESIAN_POINT('Ctrl Pts',(9.6,0.884430025516682,26.48446277673));
#47239=CARTESIAN_POINT('Ctrl Pts',(9.6,0.882699302581969,26.4786050578291));
#47240=CARTESIAN_POINT('Ctrl Pts',(9.6,0.872596303121075,26.4444109475464));
#47241=CARTESIAN_POINT('Ctrl Pts',(9.6,0.860311415881943,26.4108446276722));
#47242=CARTESIAN_POINT('Ctrl Pts',(9.6,0.845888980484608,26.378149615024));
#47243=CARTESIAN_POINT('Ctrl Pts',(9.6,0.840991978648279,26.3670483320183));
#47244=CARTESIAN_POINT('Ctrl Pts',(9.6,0.835845528233583,26.3560424349843));
#47245=CARTESIAN_POINT('Ctrl Pts',(9.6,0.83046648420776,26.3451721019));
#47246=CARTESIAN_POINT('Ctrl Pts',(9.6,0.815111322539747,26.3141413609181));
#47247=CARTESIAN_POINT('Ctrl Pts',(9.6,0.797847456292624,26.2841727552048));
#47248=CARTESIAN_POINT('Ctrl Pts',(9.6,0.77873876852075,26.2554703858443));
#47249=CARTESIAN_POINT('Ctrl Pts',(9.6,0.76024206322928,26.2276872500494));
#47250=CARTESIAN_POINT('Ctrl Pts',(9.6,0.740015758053793,26.2010902999295));
#47251=CARTESIAN_POINT('Ctrl Pts',(9.6,0.718109952543232,26.1759118525573));
#47252=CARTESIAN_POINT('Ctrl Pts',(9.6,0.700529207372861,26.1557046126626));
#47253=CARTESIAN_POINT('Ctrl Pts',(9.6,0.681866325015503,26.1364118903963));
#47254=CARTESIAN_POINT('Ctrl Pts',(9.6,0.662150216245888,26.1181780341239));
#47255=CARTESIAN_POINT('Ctrl Pts',(26.3575,0.966230510866419,26.2733743026085));
#47256=CARTESIAN_POINT('Ctrl Pts',(26.3510374103638,0.943190455260765,26.175271874718));
#47257=CARTESIAN_POINT('Ctrl Pts',(26.3445748207275,0.905342771426808,26.0806300603281));
#47258=CARTESIAN_POINT('Ctrl Pts',(26.3381122310913,0.85397204810411,25.9939874654059));
#47259=CARTESIAN_POINT('Ctrl Pts',(26.3275266955908,0.769828284376302,25.8520693929252));
#47260=CARTESIAN_POINT('Ctrl Pts',(26.3169411600902,0.6494028879358,25.731612822717));
#47261=CARTESIAN_POINT('Ctrl Pts',(26.3063556245897,0.507714145949595,25.6471752845257));
#47262=CARTESIAN_POINT('Ctrl Pts',(26.2957700890892,0.366025403963423,25.5627377463344));
#47263=CARTESIAN_POINT('Ctrl Pts',(26.2851845535887,0.203073316431535,25.51431924016));
#47264=CARTESIAN_POINT('Ctrl Pts',(26.2745990180881,0.038073613875047,25.5080742314669));
#47265=CARTESIAN_POINT('Ctrl Pts',(26.2640134825876,-0.12692608868146,25.5018292227739));
#47266=CARTESIAN_POINT('Ctrl Pts',(26.253427947087,-0.293973406262545,25.5377577115622));
#47267=CARTESIAN_POINT('Ctrl Pts',(26.2428424115865,-0.441523068585815,
25.610995220108));
#47268=CARTESIAN_POINT('Ctrl Pts',(26.232256876086,-0.589072730909101,25.6842327286538));
#47269=CARTESIAN_POINT('Ctrl Pts',(26.2216713405855,-0.717124737974537,
25.794779256957));
#47270=CARTESIAN_POINT('Ctrl Pts',(26.2110858050849,-0.812170333563929,
25.9300280902216));
#47271=CARTESIAN_POINT('Ctrl Pts',(26.2005002695844,-0.907215929153311,
26.0652769234861));
#47272=CARTESIAN_POINT('Ctrl Pts',(26.1899147340839,-0.969255113266671,
26.2252280617121));
#47273=CARTESIAN_POINT('Ctrl Pts',(26.1793291985833,-0.987370317670422,
26.3890071383319));
#47274=CARTESIAN_POINT('Ctrl Pts',(26.1769417249343,-0.991456041359965,
26.4259460565071));
#47275=CARTESIAN_POINT('Ctrl Pts',(26.1745542512852,-0.993307404832562,
26.4630796973216));
#47276=CARTESIAN_POINT('Ctrl Pts',(26.1721667776362,-0.993011273520018,
26.5001944908134));
#47277=CARTESIAN_POINT('Origin',(26.4251776695297,0.,26.5));
#47278=CARTESIAN_POINT('',(26.4075,-0.93691208277389,26.6024792620495));
#47279=CARTESIAN_POINT('Ctrl Pts',(26.4075000000007,-0.936837214195958,
26.6024576131701));
#47280=CARTESIAN_POINT('Ctrl Pts',(26.410745248043,-0.942820328546626,26.5601312037567));
#47281=CARTESIAN_POINT('Ctrl Pts',(26.4139775393434,-0.945947559415033,
26.5174819531867));
#47282=CARTESIAN_POINT('Ctrl Pts',(26.4172042771818,-0.946194674320254,
26.4748112889781));
#47283=CARTESIAN_POINT('Ctrl Pts',(26.4199365043253,-0.946403917861382,
26.4386800775753));
#47284=CARTESIAN_POINT('Ctrl Pts',(26.4226647497551,-0.94454742016796,26.4025327690601));
#47285=CARTESIAN_POINT('Ctrl Pts',(26.4253935079933,-0.940581316298395,
26.3665500875366));
#47286=CARTESIAN_POINT('Ctrl Pts',(26.4265821111055,-0.93885374537013,26.3508766113581));
#47287=CARTESIAN_POINT('Ctrl Pts',(26.4277708115146,-0.936725552147973,
26.3352343970121));
#47288=CARTESIAN_POINT('Ctrl Pts',(26.4289599806693,-0.934201239741837,
26.319637053445));
#47289=CARTESIAN_POINT('Ctrl Pts',(26.4296389953106,-0.93275985936615,26.3107309826767));
#47290=CARTESIAN_POINT('Ctrl Pts',(26.4303182652535,-0.931188922788708,
26.3018382283537));
#47291=CARTESIAN_POINT('Ctrl Pts',(26.4309964994545,-0.929492931583898,
26.2929790744995));
#47292=CARTESIAN_POINT('Ctrl Pts',(26.434148130317,-0.921611969201675,26.2518121993028));
#47293=CARTESIAN_POINT('Ctrl Pts',(26.4372840391634,-0.911022048127747,
26.2112836035419));
#47294=CARTESIAN_POINT('Ctrl Pts',(26.4404115024132,-0.897868176129323,
26.1716298451886));
#47295=CARTESIAN_POINT('Ctrl Pts',(26.4412266454206,-0.89443974678467,26.1612944771099));
#47296=CARTESIAN_POINT('Ctrl Pts',(26.4420412146901,-0.890836862988219,
26.1510185492494));
#47297=CARTESIAN_POINT('Ctrl Pts',(26.4428553390593,-0.887061520921181,
26.1408063078486));
#47298=CARTESIAN_POINT('Origin',(26.4075,0.,26.5));
#47299=CARTESIAN_POINT('Origin',(26.4075,9.00781732476477E-17,26.5));
#47300=CARTESIAN_POINT('Ctrl Pts',(26.4075,-0.936837214193549,26.6024576131701));
#47301=CARTESIAN_POINT('Ctrl Pts',(26.4075,-0.933888297224056,26.5812044318456));
#47302=CARTESIAN_POINT('Ctrl Pts',(26.4075,-0.930200091360513,26.5600464692594));
#47303=CARTESIAN_POINT('Ctrl Pts',(26.4075,-0.925762213721532,26.5390303476949));
#47304=CARTESIAN_POINT('Ctrl Pts',(26.4075,-0.923851791507024,26.5299833056703));
#47305=CARTESIAN_POINT('Ctrl Pts',(26.4075,-0.921801990307457,26.5209608466283));
#47306=CARTESIAN_POINT('Ctrl Pts',(26.4075,-0.91961313840563,26.5119721671209));
#47307=CARTESIAN_POINT('Ctrl Pts',(26.4075,-0.910761827123966,26.4756236136786));
#47308=CARTESIAN_POINT('Ctrl Pts',(26.4075,-0.899666778401924,26.4399338213958));
#47309=CARTESIAN_POINT('Ctrl Pts',(26.4075,-0.886299889617234,26.4051323253511));
#47310=CARTESIAN_POINT('Ctrl Pts',(26.4075,-0.882533408506134,26.3953260660486));
#47311=CARTESIAN_POINT('Ctrl Pts',(26.4075,-0.878586371075686,26.3855905978107));
#47312=CARTESIAN_POINT('Ctrl Pts',(26.4075,-0.874457770423122,26.3759317127677));
#47313=CARTESIAN_POINT('Ctrl Pts',(26.4075,-0.860409573041769,26.3430658739551));
#47314=CARTESIAN_POINT('Ctrl Pts',(26.4075,-0.844259571750178,26.3110832093572));
#47315=CARTESIAN_POINT('Ctrl Pts',(26.4075,-0.826080250833576,26.280221179434));
#47316=CARTESIAN_POINT('Ctrl Pts',(26.4075,-0.819767876265086,26.2695050094674));
#47317=CARTESIAN_POINT('Ctrl Pts',(26.4075,-0.813206985360593,26.2589189247773));
#47318=CARTESIAN_POINT('Ctrl Pts',(26.4075,-0.806420124795332,26.2485029477329));
#47319=CARTESIAN_POINT('Ctrl Pts',(26.4075,-0.787519580466189,26.2194957751282));
#47320=CARTESIAN_POINT('Ctrl Pts',(26.4075,-0.766849244348869,26.1917685090718));
#47321=CARTESIAN_POINT('Ctrl Pts',(26.4075,-0.744495822943584,26.1655159597568));
#47322=CARTESIAN_POINT('Ctrl Pts',(26.4075,-0.722855094261229,26.1401004188136));
#47323=CARTESIAN_POINT('Ctrl Pts',(26.4075,-0.699635820512491,26.116066939103));
#47324=CARTESIAN_POINT('Ctrl Pts',(26.4075,-0.674914432867557,26.0936401042275));
#47325=CARTESIAN_POINT('Ctrl Pts',(26.4075,-0.655118740238286,26.0756817785778));
#47326=CARTESIAN_POINT('Ctrl Pts',(26.4075,-0.634359630469717,26.0587545344762));
#47327=CARTESIAN_POINT('Ctrl Pts',(26.4075,-0.612682133358436,26.0429972363723));
#47328=CARTESIAN_POINT('Ctrl Pts',(9.53886739174678,-0.692454762064432,
26.8236314647775));
#47329=CARTESIAN_POINT('Ctrl Pts',(9.54947659464505,-0.746387612144165,
26.7082345923037));
#47330=CARTESIAN_POINT('Ctrl Pts',(9.57069500044159,-0.795395645701817,
26.4500764782137));
#47331=CARTESIAN_POINT('Ctrl Pts',(9.60252260913642,-0.67404341179918,26.0748447559888));
#47332=CARTESIAN_POINT('Ctrl Pts',(9.63435021783122,-0.387770113791111,
25.8037814721796));
#47333=CARTESIAN_POINT('Ctrl Pts',(9.66617782652605,-0.00653957363242062,
25.7030919772491));
#47334=CARTESIAN_POINT('Ctrl Pts',(9.69800543522088,0.376272204290504,25.7974986628543));
#47335=CARTESIAN_POINT('Ctrl Pts',(9.72983304391567,0.66698890097209,26.0638527475773));
#47336=CARTESIAN_POINT('Ctrl Pts',(9.76166065261051,0.794431941545588,26.4369759237776));
#47337=CARTESIAN_POINT('Ctrl Pts',(9.79348826130532,0.727413669545738,26.8255225525671));
#47338=CARTESIAN_POINT('Ctrl Pts',(9.82531587000014,0.482334658244354,27.1343885069846));
#47339=CARTESIAN_POINT('Ctrl Pts',(9.85714347869494,0.119188665110999,27.2879652485877));
#47340=CARTESIAN_POINT('Ctrl Pts',(9.88897108738978,-0.273133232602854,
27.2486612961868));
#47341=CARTESIAN_POINT('Ctrl Pts',(9.92079869608458,-0.598596265249733,
27.0260967569105));
#47342=CARTESIAN_POINT('Ctrl Pts',(9.95262630477941,-0.77753264721618,26.6747523236194));
#47343=CARTESIAN_POINT('Ctrl Pts',(9.98445391347422,-0.766141435875682,
26.2806312379679));
#47344=CARTESIAN_POINT('Ctrl Pts',(10.016281522169,-0.567211114828819,25.9402081539091));
#47345=CARTESIAN_POINT('Ctrl Pts',(10.0481091308639,-0.229436586427856,
25.7368131175217));
#47346=CARTESIAN_POINT('Ctrl Pts',(10.0799367395587,0.164500331356799,25.7202340098908));
#47347=CARTESIAN_POINT('Ctrl Pts',(10.1117643482535,0.518170209717155,25.8945291116224));
#47348=CARTESIAN_POINT('Ctrl Pts',(10.1435919569483,0.745000323495275,26.2170337856481));
#47349=CARTESIAN_POINT('Ctrl Pts',(10.1754195656431,0.789466300620247,26.608804051599));
#47350=CARTESIAN_POINT('Ctrl Pts',(10.207247174338,0.640683580453765,26.9739408306562));
#47351=CARTESIAN_POINT('Ctrl Pts',(10.2390747830327,0.335071789291362,27.2230644903377));
#47352=CARTESIAN_POINT('Ctrl Pts',(10.2709023917276,-0.0525602054491083,
27.2951935525961));
#47353=CARTESIAN_POINT('Ctrl Pts',(10.3027300004224,-0.427326304238472,
27.1726719786772));
#47354=CARTESIAN_POINT('Ctrl Pts',(10.3345576091172,-0.697489773146787,
26.8854910862812));
#47355=CARTESIAN_POINT('Ctrl Pts',(10.366385217812,-0.796918925171605,26.5039481547106));
#47356=CARTESIAN_POINT('Ctrl Pts',(10.3982128265068,-0.701275097630571,
26.121438778171));
#47357=CARTESIAN_POINT('Ctrl Pts',(10.4300404352017,-0.433970366467297,
25.8315951210098));
#47358=CARTESIAN_POINT('Ctrl Pts',(10.4618680438965,-0.0604366454286784,
25.7053662648007));
#47359=CARTESIAN_POINT('Ctrl Pts',(10.4936956525913,0.327890997713297,25.7736510102933));
#47360=CARTESIAN_POINT('Ctrl Pts',(10.5255232612861,0.635956180167181,26.0197343462881));
#47361=CARTESIAN_POINT('Ctrl Pts',(10.5573508699809,0.78834948304845,26.3833790164421));
#47362=CARTESIAN_POINT('Ctrl Pts',(10.5891784786757,0.747767468424727,26.775570634129));
#47363=CARTESIAN_POINT('Ctrl Pts',(10.6210060873706,0.524143963013505,27.1003069775249));
#47364=CARTESIAN_POINT('Ctrl Pts',(10.6528336960654,0.172218416622154,27.2780977947564));
#47365=CARTESIAN_POINT('Ctrl Pts',(10.6846613047602,-0.221863437780272,
27.2654227434594));
#47366=CARTESIAN_POINT('Ctrl Pts',(10.716488913455,-0.561636678720128,27.0653844730313));
#47367=CARTESIAN_POINT('Ctrl Pts',(10.7483165221498,-0.763930262821534,
26.7269491457883));
#47368=CARTESIAN_POINT('Ctrl Pts',(10.7801441308446,-0.779225963129924,
26.3329603052779));
#47369=CARTESIAN_POINT('Ctrl Pts',(10.8119717395395,-0.603779637374724,
25.9798601046639));
#47370=CARTESIAN_POINT('Ctrl Pts',(10.8437993482343,-0.280537733984753,
25.7540818134411));
#47371=CARTESIAN_POINT('Ctrl Pts',(10.8756269569291,0.111375310126204,25.7108923384462));
#47372=CARTESIAN_POINT('Ctrl Pts',(10.9074545656239,0.476025463481309,25.8608637709017));
#47373=CARTESIAN_POINT('Ctrl Pts',(10.9392821743187,0.724152213281463,26.1672855079379));
#47374=CARTESIAN_POINT('Ctrl Pts',(10.9711097830136,0.795018108239294,26.5551504197647));
#47375=CARTESIAN_POINT('Ctrl Pts',(11.0029373917084,0.671276313132874,26.9295153928038));
#47376=CARTESIAN_POINT('Ctrl Pts',(11.0347650004032,0.383216836026789,27.1987418821097));
#47377=CARTESIAN_POINT('Ctrl Pts',(11.066592609098,0.00135201979696231,
27.2969275583584));
#47378=CARTESIAN_POINT('Ctrl Pts',(11.0984202177928,-0.380843749208507,
27.2000381417591));
#47379=CARTESIAN_POINT('Ctrl Pts',(11.1302478264876,-0.669815072706669,
26.9317906085171));
#47380=CARTESIAN_POINT('Ctrl Pts',(11.1620754351825,-0.794826402440226,
26.5578476552035));
#47381=CARTESIAN_POINT('Ctrl Pts',(11.1939030438773,-0.725276968616409,
26.1697445230988));
#47382=CARTESIAN_POINT('Ctrl Pts',(11.2257306525721,-0.478191357872257,
25.8624826382875));
#47383=CARTESIAN_POINT('Ctrl Pts',(11.2575582612669,-0.114052167341973,
25.7112747852685));
#47384=CARTESIAN_POINT('Ctrl Pts',(11.2893858699617,0.278005165684963,25.7531342228479));
#47385=CARTESIAN_POINT('Ctrl Pts',(11.3212134786565,0.6020112901178,25.977814431644));
#47386=CARTESIAN_POINT('Ctrl Pts',(11.3530410873514,0.778654699980662,26.3303172977978));
#47387=CARTESIAN_POINT('Ctrl Pts',(11.3848686960462,0.764695919842463,26.7243557697161));
#47388=CARTESIAN_POINT('Ctrl Pts',(11.416696304741,0.563551835344745,27.0634755452618));
#47389=CARTESIAN_POINT('Ctrl Pts',(11.4485239134358,0.224459294363696,27.2646655389139));
#47390=CARTESIAN_POINT('Ctrl Pts',(11.4803515221306,-0.169577284164262,
27.2786776649706));
#47391=CARTESIAN_POINT('Ctrl Pts',(11.5121791308255,-0.522104061573776,
27.1020819795649));
#47392=CARTESIAN_POINT('Ctrl Pts',(11.5440067395203,-0.746828133179442,
26.7781062759456));
#47393=CARTESIAN_POINT('Ctrl Pts',(11.5758343482151,-0.788740648209462,
26.386054613561));
#47394=CARTESIAN_POINT('Ctrl Pts',(11.6076619569099,-0.637582094773173,
26.0218949554196));
#47395=CARTESIAN_POINT('Ctrl Pts',(11.6394895656047,-0.330353663928771,
25.7747677489538));
#47396=CARTESIAN_POINT('Ctrl Pts',(11.6713171742995,0.0577400488194873,
25.7051657732641));
#47397=CARTESIAN_POINT('Ctrl Pts',(11.7031447829944,0.431699923094752,25.8301264763938));
#47398=CARTESIAN_POINT('Ctrl Pts',(11.7349723916892,0.69998657563618,26.1190614811315));
#47399=CARTESIAN_POINT('Ctrl Pts',(11.766800000384,0.796927734095428,26.5012441294702));
#47400=CARTESIAN_POINT('Ctrl Pts',(11.7986276090788,0.698793756689006,26.883122234856));
#47401=CARTESIAN_POINT('Ctrl Pts',(11.8304552177736,0.42960626815974,27.1712181579684));
#47402=CARTESIAN_POINT('Ctrl Pts',(11.8622828264684,0.055258051066885,27.2950106345332));
#47403=CARTESIAN_POINT('Ctrl Pts',(11.8941104351633,-0.332616451231466,
27.2241972504773));
#47404=CARTESIAN_POINT('Ctrl Pts',(11.9259380438581,-0.639071777563019,
26.9761119871953));
#47405=CARTESIAN_POINT('Ctrl Pts',(11.9577656525529,-0.789092576016674,
26.6114821407401));
#47406=CARTESIAN_POINT('Ctrl Pts',(11.9895932612477,-0.745956159717636,
26.219563253107));
#47407=CARTESIAN_POINT('Ctrl Pts',(12.0214208699425,-0.520221631970104,
25.8962907861735));
#47408=CARTESIAN_POINT('Ctrl Pts',(12.0532484786374,-0.167145187013454,
25.720796658319));
#47409=CARTESIAN_POINT('Ctrl Pts',(12.0850760873322,0.226845720661642,25.7360390191599));
#47410=CARTESIAN_POINT('Ctrl Pts',(12.116903696027,0.565308431882582,25.9382867830725));
#47411=CARTESIAN_POINT('Ctrl Pts',(12.1487313047218,0.76539269994308,26.2780329391498));
#47412=CARTESIAN_POINT('Ctrl Pts',(12.1805589134166,0.778121103043664,26.6721130739564));
#47413=CARTESIAN_POINT('Ctrl Pts',(12.2123865221114,0.600377932120684,27.0240626869479));
#47414=CARTESIAN_POINT('Ctrl Pts',(12.2442141308062,0.275671866485382,27.2477301540376));
#47415=CARTESIAN_POINT('Ctrl Pts',(12.2760417395011,-0.116514253498911,
27.2883652643034));
#47416=CARTESIAN_POINT('Ctrl Pts',(12.3078693481959,-0.480179551758527,
27.1360211940663));
#47417=CARTESIAN_POINT('Ctrl Pts',(12.3396969568907,-0.726304592236129,
26.8279893298955));
#47418=CARTESIAN_POINT('Ctrl Pts',(12.3715245655855,-0.794641910002403,
26.4396709348958));
#47419=CARTESIAN_POINT('Ctrl Pts',(12.4033521742804,-0.668463625002977,
26.0661201280579));
#47420=CARTESIAN_POINT('Ctrl Pts',(12.4351797829751,-0.378656158975322,
25.7987761594907));
#47421=CARTESIAN_POINT('Ctrl Pts',(12.46700739167,0.00384026553403038,25.7030805476152));
#47422=CARTESIAN_POINT('Ctrl Pts',(12.4988350003648,0.385396654593795,25.8024580443755));
#47423=CARTESIAN_POINT('Ctrl Pts',(12.5306626090596,0.672614119883514,26.0725826314222));
#47424=CARTESIAN_POINT('Ctrl Pts',(12.5624902177544,0.79518642952386,26.4473321394994));
#47425=CARTESIAN_POINT('Ctrl Pts',(12.5943178264493,0.723109846747402,26.8349738956479));
#47426=CARTESIAN_POINT('Ctrl Pts',(12.626145435144,0.474027563748743,27.1406194112225));
#47427=CARTESIAN_POINT('Ctrl Pts',(12.6579730438389,0.108910931026614,27.2894515630053));
#47428=CARTESIAN_POINT('Ctrl Pts',(12.6898006525337,-0.282865351947728,
27.2450386257746));
#47429=CARTESIAN_POINT('Ctrl Pts',(12.7216282612285,-0.605400730631636,
27.0182521746981));
#47430=CARTESIAN_POINT('Ctrl Pts',(12.7534558699233,-0.779743714034942,
26.6646058979855));
#47431=CARTESIAN_POINT('Ctrl Pts',(12.7852834786181,-0.763217934251803,
26.2706667358078));
#47432=CARTESIAN_POINT('Ctrl Pts',(12.817111087313,-0.559868637292059,25.9328646808695));
#47433=CARTESIAN_POINT('Ctrl Pts',(12.8489386960078,-0.219472471696671,
25.7338882618077));
#47434=CARTESIAN_POINT('Ctrl Pts',(12.8807663047026,0.174647037187299,25.7224437167444));
#47435=CARTESIAN_POINT('Ctrl Pts',(12.9125939133974,0.526015750672588,25.9013324868735));
#47436=CARTESIAN_POINT('Ctrl Pts',(12.9444215220922,0.748624239560586,26.2267654685606));
#47437=CARTESIAN_POINT('Ctrl Pts',(12.976249130787,0.787981513819465,26.6190818840437));
#47438=CARTESIAN_POINT('Ctrl Pts',(13.0080767394819,0.634453543543031,26.9822489629997));
#47439=CARTESIAN_POINT('Ctrl Pts',(13.0399043481767,0.325621515054088,27.2273692254711));
#47440=CARTESIAN_POINT('Ctrl Pts',(13.0717319568715,-0.0629174411427496,
27.2944411600796));
#47441=CARTESIAN_POINT('Ctrl Pts',(13.1035595655663,-0.436055216210945,
27.1670466322858));
#47442=CARTESIAN_POINT('Ctrl Pts',(13.1353871742611,-0.702453663598643,
26.8763697805689));
#47443=CARTESIAN_POINT('Ctrl Pts',(13.167214782956,-0.796902713314313,26.4935636391573));
#47444=CARTESIAN_POINT('Ctrl Pts',(13.1990423916508,-0.696282751850487,
26.1123330157156));
#47445=CARTESIAN_POINT('Ctrl Pts',(13.2308700003456,-0.425223933001015,
25.8259970563627));
#47446=CARTESIAN_POINT('Ctrl Pts',(13.2626976090404,-0.0500771109931841,
25.7046462144535));
#47447=CARTESIAN_POINT('Ctrl Pts',(13.2945252177352,0.337327785132049,25.777985231033));
#47448=CARTESIAN_POINT('Ctrl Pts',(13.32635282643,0.64216024626656,26.0280618903463));
#47449=CARTESIAN_POINT('Ctrl Pts',(13.3581804351249,0.789802171887619,26.3936614345112));
#47450=CARTESIAN_POINT('Ctrl Pts',(13.3900080438197,0.744113185060425,26.7852909550754));
#47451=CARTESIAN_POINT('Ctrl Pts',(13.4218356525145,0.516277217440969,27.107085822582));
#47452=CARTESIAN_POINT('Ctrl Pts',(13.4536632612093,0.162064862066652,27.2802758113077));
#47453=CARTESIAN_POINT('Ctrl Pts',(13.4854908699041,-0.231818373908386,
27.2624667879633));
#47454=CARTESIAN_POINT('Ctrl Pts',(13.5173184785989,-0.568956187617919,
27.058018116014));
#47455=CARTESIAN_POINT('Ctrl Pts',(13.5491460872938,-0.766822646030525,
26.7169755533772));
#47456=CARTESIAN_POINT('Ctrl Pts',(13.5809736959886,-0.776983211600699,
26.3228208530349));
#47457=CARTESIAN_POINT('Ctrl Pts',(13.6128013046834,-0.59695074073402,25.9720367679793));
#47458=CARTESIAN_POINT('Ctrl Pts',(13.6446289133782,-0.270794296674234,
25.7504896197401));
#47459=CARTESIAN_POINT('Ctrl Pts',(13.676456522073,0.121648250824199,25.7124105991698));
#47460=CARTESIAN_POINT('Ctrl Pts',(13.7082841307678,0.484313256342262,25.86712084016));
#47461=CARTESIAN_POINT('Ctrl Pts',(13.7401117394627,0.728426139452693,26.176749755467));
#47462=CARTESIAN_POINT('Ctrl Pts',(13.7719393481575,0.794231979098091,26.5655051494659));
#47463=CARTESIAN_POINT('Ctrl Pts',(13.8037669568523,0.665622560492644,26.9382259328153));
#47464=CARTESIAN_POINT('Ctrl Pts',(13.8355945655471,0.374079407913512,27.2036760318525));
#47465=CARTESIAN_POINT('Ctrl Pts',(13.8674221742419,-0.00903238784518047,
27.2968775170617));
#47466=CARTESIAN_POINT('Ctrl Pts',(13.8992497829368,-0.389933199833693,
27.1950161587302));
#47467=CARTESIAN_POINT('Ctrl Pts',(13.9310773916315,-0.675384614490799,
26.9230259847075));
#47468=CARTESIAN_POINT('Ctrl Pts',(13.9629050003264,-0.795512700825137,
26.5474858300392));
#47469=CARTESIAN_POINT('Ctrl Pts',(13.9947326090212,-0.720912028757716,
26.160321905297));
#47470=CARTESIAN_POINT('Ctrl Pts',(14.026560217716,-0.469843647084554,25.856305733657));
#47471=CARTESIAN_POINT('Ctrl Pts',(14.0583878264108,-0.10376507142601,25.7098556010573));
#47472=CARTESIAN_POINT('Ctrl Pts',(14.0902154351057,0.287713530534183,25.7568201526036));
#47473=CARTESIAN_POINT('Ctrl Pts',(14.1220430438004,0.608764471794302,25.9857032188419));
#47474=CARTESIAN_POINT('Ctrl Pts',(14.1538706524953,0.780799627852441,26.3404778937761));
#47475=CARTESIAN_POINT('Ctrl Pts',(14.1856982611901,0.761707549946172,26.734301023437));
#47476=CARTESIAN_POINT('Ctrl Pts',(14.2175258698849,0.556161672732346,27.0707710180205));
#47477=CARTESIAN_POINT('Ctrl Pts',(14.2493534785797,0.214476332390549,27.2675254159133));
#47478=CARTESIAN_POINT('Ctrl Pts',(14.2811810872745,-0.17970937641759,27.2764018941606));
#47479=CARTESIAN_POINT('Ctrl Pts',(14.3130086959694,-0.529905110324446,
27.0952276331628));
#47480=CARTESIAN_POINT('Ctrl Pts',(14.3448363046642,-0.750388566731274,
26.7683511880868));
#47481=CARTESIAN_POINT('Ctrl Pts',(14.376663913359,-0.787188929496858,26.3757866733952));
#47482=CARTESIAN_POINT('Ctrl Pts',(14.4084915220538,-0.631298059665474,
26.0136275901214));
#47483=CARTESIAN_POINT('Ctrl Pts',(14.4403191307486,-0.3208755434976,25.7705246770357));
#47484=CARTESIAN_POINT('Ctrl Pts',(14.4721467394435,0.0680921626112602,
25.7059856307223));
#47485=CARTESIAN_POINT('Ctrl Pts',(14.5039743481383,0.440391998718261,25.8358085752634));
#47486=CARTESIAN_POINT('Ctrl Pts',(14.5358019568331,0.704890932298469,26.128214934684));
#47487=CARTESIAN_POINT('Ctrl Pts',(14.5676295655279,0.79684386389434,26.5116283189908));
#47488=CARTESIAN_POINT('Ctrl Pts',(14.5994571742227,0.693742189705464,26.8921952771914));
#47489=CARTESIAN_POINT('Ctrl Pts',(14.6312847829175,0.42082354702301,27.1767591177809));
#47490=CARTESIAN_POINT('Ctrl Pts',(14.6631123916124,0.0448940451386551,
27.2956631736732));
#47491=CARTESIAN_POINT('Ctrl Pts',(14.6949400003072,-0.342024799417935,
27.2198016378223));
#47492=CARTESIAN_POINT('Ctrl Pts',(14.726767609002,-0.645221455172022,26.967744198269));
#47493=CARTESIAN_POINT('Ctrl Pts',(14.7585952176968,-0.790478240538743,
26.6011904761496));
#47494=CARTESIAN_POINT('Ctrl Pts',(14.7904228263916,-0.742238622687695,
26.2098669473857));
#47495=CARTESIAN_POINT('Ctrl Pts',(14.8222504350865,-0.512310886867079,
25.8895633395461));
#47496=CARTESIAN_POINT('Ctrl Pts',(14.8540780437813,-0.156977657442333,
25.71868484189));
#47497=CARTESIAN_POINT('Ctrl Pts',(14.8859056524761,0.236781186430625,25.7390597717421));
#47498=CARTESIAN_POINT('Ctrl Pts',(14.9177332611709,0.572579791078355,25.9457006728515));
#47499=CARTESIAN_POINT('Ctrl Pts',(14.9495608698657,0.768220040382449,26.2880251647402));
#47500=CARTESIAN_POINT('Ctrl Pts',(14.9813884785605,0.775812337104691,26.6822376986926));
#47501=CARTESIAN_POINT('Ctrl Pts',(15.0132160872554,0.593498208699499,27.0318413649756));
#47502=CARTESIAN_POINT('Ctrl Pts',(15.0450436959502,0.265905231604842,27.2512587896549));
#47503=CARTESIAN_POINT('Ctrl Pts',(15.076871304645,-0.126777084163142,27.2867801040696));
#47504=CARTESIAN_POINT('Ctrl Pts',(15.1086989133398,-0.488426401756141,
27.129710259799));
#47505=CARTESIAN_POINT('Ctrl Pts',(15.1405265220346,-0.730516764871153,
26.8184974371495));
#47506=CARTESIAN_POINT('Ctrl Pts',(15.1723541307294,-0.793788332927985,
26.4293215468758));
#47507=CARTESIAN_POINT('Ctrl Pts',(15.2041817394243,-0.6627532402055,26.0574466090676));
#47508=CARTESIAN_POINT('Ctrl Pts',(15.2360093481191,-0.369486777125133,
25.7939016479567));
#47509=CARTESIAN_POINT('Ctrl Pts',(15.2678369568139,0.0142241267301174,
25.7031982458306));
#47510=CARTESIAN_POINT('Ctrl Pts',(15.2996645655087,0.394453192351198,25.8075391417037));
#47511=CARTESIAN_POINT('Ctrl Pts',(15.3314921742035,0.678126438920626,26.0813833566788));
#47512=CARTESIAN_POINT('Ctrl Pts',(15.3633197828983,0.795805202493795,26.4576982162029));
#47513=CARTESIAN_POINT('Ctrl Pts',(15.3951473915932,0.718683607945039,26.8443678743723));
#47514=CARTESIAN_POINT('Ctrl Pts',(15.426975000288,0.465639785487568,27.1467417965461));
#47515=CARTESIAN_POINT('Ctrl Pts',(15.4588026089828,0.0986148069826778,
27.2908036931327));
#47516=CARTESIAN_POINT('Ctrl Pts',(15.4906302176776,-0.292549495638406,
27.2412895209231));
#47517=CARTESIAN_POINT('Ctrl Pts',(15.5224578263724,-0.612102370814474,
27.0103195556432));
#47518=CARTESIAN_POINT('Ctrl Pts',(15.5542854350672,-0.781822396609454,
26.6544315427252));
#47519=CARTESIAN_POINT('Ctrl Pts',(15.5861130437621,-0.760164831041612,
26.2607411634315));
#47520=CARTESIAN_POINT('Ctrl Pts',(15.6179406524569,-0.552431099026793,
25.9256175124043));
#47521=CARTESIAN_POINT('Ctrl Pts',(15.6497682611517,-0.209471088532158,
25.7310934879338));
#47522=CARTESIAN_POINT('Ctrl Pts',(15.6815958698465,0.184764086958111,25.7247854533105));
#47523=CARTESIAN_POINT('Ctrl Pts',(15.7134234785413,0.533771975425466,25.9082375143023));
#47524=CARTESIAN_POINT('Ctrl Pts',(15.7452510872362,0.752121039795552,26.2365435468138));
#47525=CARTESIAN_POINT('Ctrl Pts',(15.7770786959309,0.78636292888696,26.6293394962914));
#47526=CARTESIAN_POINT('Ctrl Pts',(15.8089063046258,0.628115777091278,26.9904752101765));
#47527=CARTESIAN_POINT('Ctrl Pts',(15.8407339133206,0.316115950726511,27.2315504541211));
#47528=CARTESIAN_POINT('Ctrl Pts',(15.8725615220154,-0.073263993557323,
27.2935538724477));
#47529=CARTESIAN_POINT('Ctrl Pts',(15.9043891307102,-0.444710086519647,
27.1613080221623));
#47530=CARTESIAN_POINT('Ctrl Pts',(15.9362167394051,-0.707298278273243,
26.8671845677318));
#47531=CARTESIAN_POINT('Ctrl Pts',(15.9680443480998,-0.796751188333675,
26.483180216485));
#47532=CARTESIAN_POINT('Ctrl Pts',(15.9998719567947,-0.691172178101171,
26.1032930786494));
#47533=CARTESIAN_POINT('Ctrl Pts',(16.0316995654895,-0.416405297022751,
25.8205134366008));
#47534=CARTESIAN_POINT('Ctrl Pts',(16.0635271741844,-0.0397090735252242,
25.7040612142204));
#47535=CARTESIAN_POINT('Ctrl Pts',(16.0953547828791,0.346707294700135,25.782442049009));
#47536=CARTESIAN_POINT('Ctrl Pts',(16.127182391574,0.648255274330614,26.0364695689265));
#47537=CARTESIAN_POINT('Ctrl Pts',(16.1590100002688,0.791120753270836,26.4039619087403));
#47538=CARTESIAN_POINT('Ctrl Pts',(16.1908376089636,0.740332552174896,26.7949628339619));
#47539=CARTESIAN_POINT('Ctrl Pts',(16.2226652176584,0.508322808619745,27.1137615851986));
#47540=CARTESIAN_POINT('Ctrl Pts',(16.2544928263532,0.151883789093077,27.2823213379676));
#47541=CARTESIAN_POINT('Ctrl Pts',(16.2863204350481,-0.24173394755624,27.2593813665264));
#47542=CARTESIAN_POINT('Ctrl Pts',(16.3181480437429,-0.576179088441399,
27.0505570081939));
#47543=CARTESIAN_POINT('Ctrl Pts',(16.3499756524377,-0.769584823679254,
26.706965118779));
#47544=CARTESIAN_POINT('Ctrl Pts',(16.3818032611325,-0.774608529259432,
26.3127114855973));
#47545=CARTESIAN_POINT('Ctrl Pts',(16.4136308698273,-0.590020482577639,
25.9643030788146));
#47546=CARTESIAN_POINT('Ctrl Pts',(16.4454584785221,-0.261004878818793,
25.7470246919976));
#47547=CARTESIAN_POINT('Ctrl Pts',(16.477286087217,0.131900535795971,25.7140625916236));
#47548=CARTESIAN_POINT('Ctrl Pts',(16.5091136959118,0.492518813396506,25.8734853715362));
#47549=CARTESIAN_POINT('Ctrl Pts',(16.5409413046066,0.732576379744177,26.1862688904977));
#47550=CARTESIAN_POINT('Ctrl Pts',(16.5727689133014,0.793310990324887,26.5758487564716));
#47551=CARTESIAN_POINT('Ctrl Pts',(16.6045965219962,0.659855785944694,26.9468620625921));
#47552=CARTESIAN_POINT('Ctrl Pts',(16.636424130691,0.364878461567863,27.2084906982538));
#47553=CARTESIAN_POINT('Ctrl Pts',(16.6682517393859,-0.0194152617984515,
27.2966921669241));
#47554=CARTESIAN_POINT('Ctrl Pts',(16.7000793480807,-0.398956440272542,
27.1898761627955));
#47555=CARTESIAN_POINT('Ctrl Pts',(16.7319069567755,-0.680839476780989,
26.9141895315969));
#47556=CARTESIAN_POINT('Ctrl Pts',(16.7637345654703,-0.796063922115232,
26.5371159418362));
#47557=CARTESIAN_POINT('Ctrl Pts',(16.7955621741651,-0.716424678902143,
26.1509569644296));
#47558=CARTESIAN_POINT('Ctrl Pts',(16.8273897828599,-0.461416157419982,
25.8502381275293));
#47559=CARTESIAN_POINT('Ctrl Pts',(16.8592173915548,-0.0934603563117058,
25.7085705824253));
#47560=CARTESIAN_POINT('Ctrl Pts',(16.8910450002496,0.29737304194578,25.7606322733754));
#47561=CARTESIAN_POINT('Ctrl Pts',(16.9228726089444,0.615414286049196,25.9936793330608));
#47562=CARTESIAN_POINT('Ctrl Pts',(16.9547002176392,0.782811976792353,26.3506655763249));
#47563=CARTESIAN_POINT('Ctrl Pts',(16.986527826334,0.758589843209824,26.7442064932981));
#47564=CARTESIAN_POINT('Ctrl Pts',(17.0183554350289,0.548677074193156,27.0779695742253));
#47565=CARTESIAN_POINT('Ctrl Pts',(17.0501830437237,0.204456953247554,27.270254968634));
#47566=CARTESIAN_POINT('Ctrl Pts',(17.0820106524185,-0.189810955467986,
27.273994290092));
#47567=CARTESIAN_POINT('Ctrl Pts',(17.1138382611133,-0.537616179499631,
27.0882722200051));
#47568=CARTESIAN_POINT('Ctrl Pts',(17.1456658698081,-0.753821589603515,
26.7585505304068));
#47569=CARTESIAN_POINT('Ctrl Pts',(17.1774934785029,-0.785503538757171,
26.3655398322693));
#47570=CARTESIAN_POINT('Ctrl Pts',(17.2093210871977,-0.624906846574195,
26.0054427956063));
#47571=CARTESIAN_POINT('Ctrl Pts',(17.2411486958926,-0.311342909206791,
25.7664054968385));
#47572=CARTESIAN_POINT('Ctrl Pts',(17.2729763045874,0.0784326585839467,
25.7069402585764));
#47573=CARTESIAN_POINT('Ctrl Pts',(17.3048039132822,0.449009401771598,25.8416035517627));
#47574=CARTESIAN_POINT('Ctrl Pts',(17.336631521977,0.709675400200942,26.1374313304758));
#47575=CARTESIAN_POINT('Ctrl Pts',(17.3684591306719,0.796625066564042,26.5220108860288));
#47576=CARTESIAN_POINT('Ctrl Pts',(17.4002867393666,0.688572116174983,26.9012010606094));
#47577=CARTESIAN_POINT('Ctrl Pts',(17.4321143480615,0.411970711104484,27.1821864196729));
#47578=CARTESIAN_POINT('Ctrl Pts',(17.4639419567563,0.0345198850269114,
27.296178240544));
#47579=CARTESIAN_POINT('Ctrl Pts',(17.4957695654511,-0.351370292731717,
27.2152882780459));
#47580=CARTESIAN_POINT('Ctrl Pts',(17.5275971741459,-0.651270599572141,
26.9592885385028));
#47581=CARTESIAN_POINT('Ctrl Pts',(17.5594247828408,-0.791712642528938,
26.5908975818914));
#47582=CARTESIAN_POINT('Ctrl Pts',(17.5912523915355,-0.73842722970491,26.2001897847722));
#47583=CARTESIAN_POINT('Ctrl Pts',(17.6230800002304,-0.504252400540365,
25.882996417912));
#47584=CARTESIAN_POINT('Ctrl Pts',(17.6549076089252,-0.146898168000676,
25.7165983131021));
#47585=CARTESIAN_POINT('Ctrl Pts',(17.68673521762,0.246892880351082,25.7424124008351));
#47586=CARTESIAN_POINT('Ctrl Pts',(17.7185628263148,0.579346349872695,25.9528266796507));
#47587=CARTESIAN_POINT('Ctrl Pts',(17.7503904350096,0.771677592213418,26.2987691287884));
#47588=CARTESIAN_POINT('Ctrl Pts',(17.7822180437045,0.772008340680367,26.6910250850529));
#47589=CARTESIAN_POINT('Ctrl Pts',(17.8246548552975,0.527363192762192,27.1585233970218));
#47590=CARTESIAN_POINT('Ctrl Pts',(17.8777008697889,-0.155425403013523,
27.3905262878577));
#47591=CARTESIAN_POINT('Ctrl Pts',(17.9307468842803,-0.719256274148258,
26.9409483117146));
#47592=CARTESIAN_POINT('Ctrl Pts',(17.9731836958734,-0.791074584357761,
26.4182169749722));
#47593=CARTESIAN_POINT('Ctrl Pts',(18.0050113045682,-0.657888459085232,
26.0492639960516));
#47594=CARTESIAN_POINT('Ctrl Pts',(18.036838913263,-0.35974177500854,25.7889256783384));
#47595=CARTESIAN_POINT('Ctrl Pts',(18.0686665219578,0.0243332818644455,
25.7035686117623));
#47596=CARTESIAN_POINT('Ctrl Pts',(18.1004941306526,0.403587040260669,25.8126756400868));
#47597=CARTESIAN_POINT('Ctrl Pts',(18.1323217393475,0.683447187528216,26.0902880943639));
#47598=CARTESIAN_POINT('Ctrl Pts',(18.1641493480422,0.796329325103614,26.468054034611));
#47599=CARTESIAN_POINT('Ctrl Pts',(18.1959769567371,0.71411390092001,26.8537126167479));
#47600=CARTESIAN_POINT('Ctrl Pts',(18.2278045654319,0.457184295086093,27.1527494739896));
#47601=CARTESIAN_POINT('Ctrl Pts',(18.2596321741268,0.0882959257025597,
27.2920241365189));
#47602=CARTESIAN_POINT('Ctrl Pts',(18.2914597828215,-0.302180780501247,
27.237413173922));
#47603=CARTESIAN_POINT('Ctrl Pts',(18.3232873915164,-0.618701763158597,
27.0023010116041));
#47604=CARTESIAN_POINT('Ctrl Pts',(18.3551150002112,-0.783767433557126,
26.6442305803327));
#47605=CARTESIAN_POINT('Ctrl Pts',(18.386942608906,-0.756983125763724,26.2508564207311));
#47606=CARTESIAN_POINT('Ctrl Pts',(18.4187702176008,-0.544899508122728,
25.9184677654519));
#47607=CARTESIAN_POINT('Ctrl Pts',(18.4505978262956,-0.199434270097742,
25.7284293306239));
#47608=CARTESIAN_POINT('Ctrl Pts',(18.4824254349904,0.194849834271444,25.7272587900961));
#47609=CARTESIAN_POINT('Ctrl Pts',(18.5142530436853,0.541437529129979,25.9152430383213));
#47610=CARTESIAN_POINT('Ctrl Pts',(18.5460806523801,0.755490150492264,26.2463663511633));
#47611=CARTESIAN_POINT('Ctrl Pts',(18.5779082610749,0.784610810040825,26.639575151346));
#47612=CARTESIAN_POINT('Ctrl Pts',(18.6097358697697,0.621671362865706,26.9986181728724));
#47613=CARTESIAN_POINT('Ctrl Pts',(18.6415634784645,0.306556707364476,27.2356074676479));
#47614=CARTESIAN_POINT('Ctrl Pts',(18.6733910871593,-0.0835981042838541,
27.2925318396574));
#47615=CARTESIAN_POINT('Ctrl Pts',(18.7052186958542,-0.453289446413202,
27.1554571230883));
#47616=CARTESIAN_POINT('Ctrl Pts',(18.737046304549,-0.71202279411859,26.8579370072105));
#47617=CARTESIAN_POINT('Ctrl Pts',(18.7688739132438,-0.796464376192686,
26.472799649891));
#47618=CARTESIAN_POINT('Ctrl Pts',(18.8007015219386,-0.685944244027812,
26.0943205018872));
#47619=CARTESIAN_POINT('Ctrl Pts',(18.8325291306334,-0.407515955991956,
25.8151451928656));
#47620=CARTESIAN_POINT('Ctrl Pts',(18.8643567393282,-0.0293342934702721,
25.7036113634181));
#47621=CARTESIAN_POINT('Ctrl Pts',(18.8961843480231,0.356027933769703,25.7870207074674));
#47622=CARTESIAN_POINT('Ctrl Pts',(18.9280119567179,0.654240229440685,26.0449559544106));
#47623=CARTESIAN_POINT('Ctrl Pts',(18.9598395654127,0.792305003299414,26.4142786901237));
#47624=CARTESIAN_POINT('Ctrl Pts',(18.9916671741075,0.736426211717768,26.8045846285138));
#47625=CARTESIAN_POINT('Ctrl Pts',(19.0234947828023,0.500282087197375,27.1203331318392));
#47626=CARTESIAN_POINT('Ctrl Pts',(19.0553223914972,0.141676926436067,27.2842340274076));
#47627=CARTESIAN_POINT('Ctrl Pts',(19.087150000192,-0.25160847507182,27.2561670030497));
#47628=CARTESIAN_POINT('Ctrl Pts',(19.1189776088868,-0.5833041547505,27.0430024164579));
#47629=CARTESIAN_POINT('Ctrl Pts',(19.1508052175816,-0.772216326753395,
26.6969195417532));
#47630=CARTESIAN_POINT('Ctrl Pts',(19.1826328262764,-0.772102319324263,
26.3026339195236));
#47631=CARTESIAN_POINT('Ctrl Pts',(19.2144604349712,-0.582990039655113,
25.956660350341));
#47632=CARTESIAN_POINT('Ctrl Pts',(19.2462880436661,-0.251171142649758,
25.7436876185539));
#47633=CARTESIAN_POINT('Ctrl Pts',(19.2781156523609,0.142130424215859,25.7158480353013));
#47634=CARTESIAN_POINT('Ctrl Pts',(19.3099432610557,0.500640741350412,25.8799562843406));
#47635=CARTESIAN_POINT('Ctrl Pts',(19.3417708697505,0.736602229450057,26.1958412966923));
#47636=CARTESIAN_POINT('Ctrl Pts',(19.3735984784453,0.792255298302605,26.58617948445));
#47637=CARTESIAN_POINT('Ctrl Pts',(19.4054260871402,0.653976968680098,26.9554223157297));
#47638=CARTESIAN_POINT('Ctrl Pts',(19.437253695835,0.355615559299935,27.2131850637895));
#47639=CARTESIAN_POINT('Ctrl Pts',(19.4690813045298,-0.0297948390643188,
27.2963715394172));
#47640=CARTESIAN_POINT('Ctrl Pts',(19.5009089132246,-0.407911938387894,
27.1846190267216));
#47641=CARTESIAN_POINT('Ctrl Pts',(19.5327365219194,-0.686178733351599,
26.9052827496015));
#47642=CARTESIAN_POINT('Ctrl Pts',(19.5645641306142,-0.796479972707378,
26.526739751395));
#47643=CARTESIAN_POINT('Ctrl Pts',(19.5963917393091,-0.711815681008405,
26.1416512906412));
#47644=CARTESIAN_POINT('Ctrl Pts',(19.6282193480038,-0.452910319833234,
25.8442808501979));
#47645=CARTESIAN_POINT('Ctrl Pts',(19.6600469566987,-0.0831397717704243,
25.7074199475267));
#47646=CARTESIAN_POINT('Ctrl Pts',(19.6918745653935,0.306982059827983,25.7645699379462));
#47647=CARTESIAN_POINT('Ctrl Pts',(19.7237021740883,0.621959603598031,26.0017414198222));
#47648=CARTESIAN_POINT('Ctrl Pts',(19.7555297827831,0.784691405396808,26.3608786158601));
#47649=CARTESIAN_POINT('Ctrl Pts',(19.787357391478,0.755343328467109,26.7540704968485));
#47650=CARTESIAN_POINT('Ctrl Pts',(19.8191850001728,0.54109931163992,27.0850699925406));
#47651=CARTESIAN_POINT('Ctrl Pts',(19.8510126088676,0.194402856255303,27.2728537317685));
#47652=CARTESIAN_POINT('Ctrl Pts',(19.8828402175624,-0.199880302382556,
27.2714552650336));
#47653=CARTESIAN_POINT('Ctrl Pts',(19.9146678262572,-0.545235966749666,
27.0812169145776));
#47654=CARTESIAN_POINT('Ctrl Pts',(19.9464954349521,-0.75712660569227,26.7487059793843));
#47655=CARTESIAN_POINT('Ctrl Pts',(19.9783230436469,-0.783684787055667,
26.3553158067855));
#47656=CARTESIAN_POINT('Ctrl Pts',(20.0101506523417,-0.618409493726067,
25.9973420056359));
#47657=CARTESIAN_POINT('Ctrl Pts',(20.0419782610365,-0.301757468419426,
25.7624108247258));
#47658=CARTESIAN_POINT('Ctrl Pts',(20.0738058697313,0.0887599484803642,
25.7080296515813));
#47659=CARTESIAN_POINT('Ctrl Pts',(20.1056334784261,0.457550352668162,25.8475101257477));
#47660=CARTESIAN_POINT('Ctrl Pts',(20.137461087121,0.71433976430242,26.1467096627914));
#47661=CARTESIAN_POINT('Ctrl Pts',(20.1692886958158,0.796270251327002,26.5323890117207));
#47662=CARTESIAN_POINT('Ctrl Pts',(20.2011163045106,0.683286543729253,26.9101400497234));
#47663=CARTESIAN_POINT('Ctrl Pts',(20.2329439132054,0.403045242186098,27.1874953774243));
#47664=CARTESIAN_POINT('Ctrl Pts',(20.2647715219002,0.0241449255081358,
27.2965628561519));
#47665=CARTESIAN_POINT('Ctrl Pts',(20.296599130595,-0.360665681930769,27.210644515286));
#47666=CARTESIAN_POINT('Ctrl Pts',(20.3284267392899,-0.657191111310729,
26.9507717875409));
#47667=CARTESIAN_POINT('Ctrl Pts',(20.3602543479846,-0.792846690334467,
26.5805573513361));
#47668=CARTESIAN_POINT('Ctrl Pts',(20.3920819566795,-0.734426107592801,
26.1906237667262));
#47669=CARTESIAN_POINT('Ctrl Pts',(20.4239095653743,-0.496229785355027,
25.8764205252295));
#47670=CARTESIAN_POINT('Ctrl Pts',(20.4557371740691,-0.136564365409659,
25.7148595442031));
#47671=CARTESIAN_POINT('Ctrl Pts',(20.4875647827639,0.256529822285824,25.7454883622458));
#47672=CARTESIAN_POINT('Ctrl Pts',(20.5193923914588,0.586829621236875,25.9608095356299));
#47673=CARTESIAN_POINT('Ctrl Pts',(20.5512200001536,0.773482934822817,26.3081158923556));
#47674=CARTESIAN_POINT('Ctrl Pts',(20.5830476088484,0.77080002362345,26.7023924030459));
#47675=CARTESIAN_POINT('Ctrl Pts',(20.6148752175432,0.579437621297725,27.047126497488));
#47676=CARTESIAN_POINT('Ctrl Pts',(20.646702826238,0.2462381767104,27.2579327948828));
#47677=CARTESIAN_POINT('Ctrl Pts',(20.6785304349328,-0.147236426742641,
27.2832092925066));
#47678=CARTESIAN_POINT('Ctrl Pts',(20.7103580436277,-0.504669912886847,
27.1167687088815));
#47679=CARTESIAN_POINT('Ctrl Pts',(20.7421856523225,-0.738568293385044,
26.7993530311103));
#47680=CARTESIAN_POINT('Ctrl Pts',(20.7740132610173,-0.791676993697611,
26.40866052946));
#47681=CARTESIAN_POINT('Ctrl Pts',(20.8058408697121,-0.650995855233153,
26.0403264661764));
#47682=CARTESIAN_POINT('Ctrl Pts',(20.8376684784069,-0.350961365800501,
25.7845131161621));
#47683=CARTESIAN_POINT('Ctrl Pts',(20.8694960871017,0.034982840646634,25.7038394872333));
#47684=CARTESIAN_POINT('Ctrl Pts',(20.9013236957965,0.412363808420875,25.8180531906862));
#47685=CARTESIAN_POINT('Ctrl Pts',(20.9331513044914,0.688804725407329,26.0991965425734));
#47686=CARTESIAN_POINT('Ctrl Pts',(20.9649789131862,0.796637286020959,26.4784501566183));
#47687=CARTESIAN_POINT('Ctrl Pts',(20.996806521881,0.70946580780214,26.8629788269146));
#47688=CARTESIAN_POINT('Ctrl Pts',(21.0286341305758,0.448628471403418,27.1586560983357));
#47689=CARTESIAN_POINT('Ctrl Pts',(21.0604617392707,0.0779740759816852,
27.2931049140583));
#47690=CARTESIAN_POINT('Ctrl Pts',(21.0922893479654,-0.311767123444173,
27.2334143589867));
#47691=CARTESIAN_POINT('Ctrl Pts',(21.1241169566603,-0.625192728165132,
26.9941957242612));
#47692=CARTESIAN_POINT('Ctrl Pts',(21.1559445653551,-0.785581173842449,
26.6340058973812));
#47693=CARTESIAN_POINT('Ctrl Pts',(21.1877721740499,-0.753671939737323,
26.2410135747164));
#47694=CARTESIAN_POINT('Ctrl Pts',(21.2195997827447,-0.537275894906149,
25.9114169778345));
#47695=CARTESIAN_POINT('Ctrl Pts',(21.2514273914396,-0.189363322650899,
25.7258960707611));
#47696=CARTESIAN_POINT('Ctrl Pts',(21.2832550001344,0.204902355806668,25.7298633979523));
#47697=CARTESIAN_POINT('Ctrl Pts',(21.3150826088292,0.549011221810531,25.9223478213019));
#47698=CARTESIAN_POINT('Ctrl Pts',(21.346910217524,0.758730940462114,26.2562322391823));
#47699=CARTESIAN_POINT('Ctrl Pts',(21.3787378262188,0.782725486097683,26.6497870977146));
#47700=CARTESIAN_POINT('Ctrl Pts',(21.4105654349136,0.615121378538741,27.0066764755672));
#47701=CARTESIAN_POINT('Ctrl Pts',(21.4423930436085,0.296945416897534,27.2395395733916));
#47702=CARTESIAN_POINT('Ctrl Pts',(21.4742206523033,-0.0939180232535311,
27.2913752372527));
#47703=CARTESIAN_POINT('Ctrl Pts',(21.5060482609981,-0.461791836663578,
27.1494949274779));
#47704=CARTESIAN_POINT('Ctrl Pts',(21.5378758696929,-0.716626410222027,
26.848628669792));
#47705=CARTESIAN_POINT('Ctrl Pts',(21.5697034783877,-0.79604232490086,26.4624237016852));
#47706=CARTESIAN_POINT('Ctrl Pts',(21.6015310870826,-0.6805998376932,26.0854168091196));
#47707=CARTESIAN_POINT('Ctrl Pts',(21.6333586957773,-0.398557419114277,
25.8098932365948));
#47708=CARTESIAN_POINT('Ctrl Pts',(21.6651863044722,-0.0189545325561093,
25.7032967384752));
#47709=CARTESIAN_POINT('Ctrl Pts',(21.697013913167,0.36528811976181,25.791720428934));
#47710=CARTESIAN_POINT('Ctrl Pts',(21.7288415218618,0.660114095329825,26.053519605833));
#47711=CARTESIAN_POINT('Ctrl Pts',(21.7606691305566,0.793354720904365,26.4246100268778));
#47712=CARTESIAN_POINT('Ctrl Pts',(21.7924967392514,0.732394826972873,26.8141547049655));
#47713=CARTESIAN_POINT('Ctrl Pts',(21.8243243479463,0.492156418482947,27.126799346661));
#47714=CARTESIAN_POINT('Ctrl Pts',(21.856151956641,0.131446007206347,27.2860135548564));
#47715=CARTESIAN_POINT('Ctrl Pts',(21.8879795653359,-0.261440279771059,
27.2528242433277));
#47716=CARTESIAN_POINT('Ctrl Pts',(21.9198071740307,-0.590330176718207,
27.0353556235666));
#47717=CARTESIAN_POINT('Ctrl Pts',(21.9516347827255,-0.774716708426573,
26.6868405280267));
#47718=CARTESIAN_POINT('Ctrl Pts',(21.9834623914203,-0.769465007346789,
26.2925898659722));
#47719=CARTESIAN_POINT('Ctrl Pts',(22.0152900001152,-0.575860605727061,
25.9491098802844));
#47720=CARTESIAN_POINT('Ctrl Pts',(22.04711760881,-0.241294757923752,25.7404789660404));
#47721=CARTESIAN_POINT('Ctrl Pts',(22.0789452175048,0.152336179061179,25.7177666270366));
#47722=CARTESIAN_POINT('Ctrl Pts',(22.1107728261996,0.508677661110342,25.8865324798199));
#47723=CARTESIAN_POINT('Ctrl Pts',(22.1426004348944,0.740503004985982,26.2054653486679));
#47724=CARTESIAN_POINT('Ctrl Pts',(22.1744280435892,0.791065082286333,26.5964955792559));
#47725=CARTESIAN_POINT('Ctrl Pts',(22.2062556522841,0.647987106915214,26.9639052387075));
#47726=CARTESIAN_POINT('Ctrl Pts',(22.2380832609789,0.346292273938845,27.2177583313615));
#47727=CARTESIAN_POINT('Ctrl Pts',(22.2699108696737,-0.0401693572021401,
27.2959156889838));
#47728=CARTESIAN_POINT('Ctrl Pts',(22.3017384783685,-0.416798173548772,
27.1792456431623));
#47729=CARTESIAN_POINT('Ctrl Pts',(22.3335660870633,-0.691401477599888,
26.8963071510852));
#47730=CARTESIAN_POINT('Ctrl Pts',(22.3653936957582,-0.796760781963107,
26.5163590205743));
#47731=CARTESIAN_POINT('Ctrl Pts',(22.397221304453,-0.707085817666679,26.132406464035));
#47732=CARTESIAN_POINT('Ctrl Pts',(22.4290489131478,-0.444327578628173,
25.8384349131801));
#47733=CARTESIAN_POINT('Ctrl Pts',(22.4608765218426,-0.0728050701817948,
25.7064038917784));
#47734=CARTESIAN_POINT('Ctrl Pts',(22.4927041305374,0.316538952499552,25.768632477629));
#47735=CARTESIAN_POINT('Ctrl Pts',(22.5245317392322,0.628399313207805,26.0098881103375));
#47736=CARTESIAN_POINT('Ctrl Pts',(22.5563593479271,0.786437594250266,26.3711152779478));
#47737=CARTESIAN_POINT('Ctrl Pts',(22.5881869566219,0.751968557521462,26.7638913597064));
#47738=CARTESIAN_POINT('Ctrl Pts',(22.6200145653167,0.533429670730638,27.0920710663534));
#47739=CARTESIAN_POINT('Ctrl Pts',(22.6518421740115,0.184315750545256,27.2753212658824));
#47740=CARTESIAN_POINT('Ctrl Pts',(22.6836697827063,-0.209915711095263,
27.2687852466482));
#47741=CARTESIAN_POINT('Ctrl Pts',(22.7154973914012,-0.552763171263273,
27.0740629213976));
#47742=CARTESIAN_POINT('Ctrl Pts',(22.7473250000959,-0.760303066990549,
26.7388191942734));
#47743=CARTESIAN_POINT('Ctrl Pts',(22.7791526087908,-0.78173295832624,26.3451163562699));
#47744=CARTESIAN_POINT('Ctrl Pts',(22.8109802174856,-0.611807151357293,
25.9893265517215));
#47745=CARTESIAN_POINT('Ctrl Pts',(22.8428078261804,-0.292120759998493,
25.7585414220562));
#47746=CARTESIAN_POINT('Ctrl Pts',(22.8746354348752,0.0990721111926007,
25.7092534679099));
#47747=CARTESIAN_POINT('Ctrl Pts',(22.9064630435701,0.466013717526745,25.853527590453));
#47748=CARTESIAN_POINT('Ctrl Pts',(22.9382906522649,0.718882635243795,26.1560477969637));
#47749=CARTESIAN_POINT('Ctrl Pts',(22.9701182609597,0.795780606359475,26.5427619897895));
#47750=CARTESIAN_POINT('Ctrl Pts',(23.0019458696545,0.677884240092678,26.9190087329192));
#47751=CARTESIAN_POINT('Ctrl Pts',(23.0337734783493,0.394052677220659,27.1926888542512));
#47752=CARTESIAN_POINT('Ctrl Pts',(23.0656010870442,0.0137633349813457,
27.2968098467256));
#47753=CARTESIAN_POINT('Ctrl Pts',(23.0974286957389,-0.369895051057782,
27.2058845602728));
#47754=CARTESIAN_POINT('Ctrl Pts',(23.1292563044338,-0.663009057407268,
26.9421700476339));
#47755=CARTESIAN_POINT('Ctrl Pts',(23.1610839131286,-0.793829073448207,
26.5702193945928));
#47756=CARTESIAN_POINT('Ctrl Pts',(23.1929115218234,-0.730332456083478,
26.1810801592568));
#47757=CARTESIAN_POINT('Ctrl Pts',(23.2247391305182,-0.488062159497627,
25.8700073891742));
#47758=CARTESIAN_POINT('Ctrl Pts',(23.2565667392131,-0.126322069100469,
25.7131467124763));
#47759=CARTESIAN_POINT('Ctrl Pts',(23.2883943479078,0.266339639077475,25.7488951086002));
#47760=CARTESIAN_POINT('Ctrl Pts',(23.3202219566027,0.593805672595626,25.9685019431627));
#47761=CARTESIAN_POINT('Ctrl Pts',(23.3520495652975,0.775917595190683,26.3182109829992));
#47762=CARTESIAN_POINT('Ctrl Pts',(23.3838771739923,0.768097327165974,26.7124190604186));
#47763=CARTESIAN_POINT('Ctrl Pts',(23.4157047826871,0.572259144787906,27.0546303565756));
#47764=CARTESIAN_POINT('Ctrl Pts',(23.4475323913819,0.236341096138676,27.2610770312554));
#47765=CARTESIAN_POINT('Ctrl Pts',(23.4793600000768,-0.157429464686238,
27.281224247497));
#47766=CARTESIAN_POINT('Ctrl Pts',(23.5111876087716,-0.512663815891357,
27.1101402896911));
#47767=CARTESIAN_POINT('Ctrl Pts',(23.5430152174664,-0.742406282124077,
26.7897037685142));
#47768=CARTESIAN_POINT('Ctrl Pts',(23.5748428261612,-0.790419590044506,
26.39835240828));
#47769=CARTESIAN_POINT('Ctrl Pts',(23.6066704348561,-0.644950851448086,
26.0318827492551));
#47770=CARTESIAN_POINT('Ctrl Pts',(23.6384980435508,-0.341608481918587,
25.7800006900629));
#47771=CARTESIAN_POINT('Ctrl Pts',(23.6703256522457,0.0453541685624505,
25.7043629215386));
#47772=CARTESIAN_POINT('Ctrl Pts',(23.7021532609405,0.421214845532138,25.8234843570678));
#47773=CARTESIAN_POINT('Ctrl Pts',(23.7339808696353,0.693968879696766,26.1082059785538));
#47774=CARTESIAN_POINT('Ctrl Pts',(23.7658084783301,0.796850455291405,26.4888324966759));
#47775=CARTESIAN_POINT('Ctrl Pts',(23.797636087025,0.704675811632944,26.8721926406151));
#47776=CARTESIAN_POINT('Ctrl Pts',(23.8294636957197,0.440007824081036,27.1644459917676));
#47777=CARTESIAN_POINT('Ctrl Pts',(23.8612913044146,0.0676329737958395,
27.2940536141119));
#47778=CARTESIAN_POINT('Ctrl Pts',(23.8931189131094,-0.321297344429241,
27.229289639095));
#47779=CARTESIAN_POINT('Ctrl Pts',(23.9249465218042,-0.631579222606048,
26.9860072497412));
#47780=CARTESIAN_POINT('Ctrl Pts',(23.956774130499,-0.787260630265086,26.6237580755475));
#47781=CARTESIAN_POINT('Ctrl Pts',(23.9886017391939,-0.750233254128349,
26.2312149080983));
#47782=CARTESIAN_POINT('Ctrl Pts',(24.0204293478886,-0.529560802386153,
25.9044660229636));
#47783=CARTESIAN_POINT('Ctrl Pts',(24.0522569565835,-0.179260354208531,
25.7234943099773));
#47784=CARTESIAN_POINT('Ctrl Pts',(24.0840845652783,0.214920155430682,25.7325987437994));
#47785=CARTESIAN_POINT('Ctrl Pts',(24.1159121739731,0.556491655837079,25.9295507049594));
#47786=CARTESIAN_POINT('Ctrl Pts',(24.1477397826679,0.761842918540557,26.2661395101813));
#47787=CARTESIAN_POINT('Ctrl Pts',(24.1795673913627,0.780707245874303,26.6599736149119));
#47788=CARTESIAN_POINT('Ctrl Pts',(24.2113950000576,0.608466952871163,27.0146487428259));
#47789=CARTESIAN_POINT('Ctrl Pts',(24.2432226087524,0.287283702529686,27.2433461074691));
#47790=CARTESIAN_POINT('Ctrl Pts',(24.2750502174472,-0.104221993505796,
27.2900842596193));
#47791=CARTESIAN_POINT('Ctrl Pts',(24.306877826142,-0.470215816038203,27.1434224487661));
#47792=CARTESIAN_POINT('Ctrl Pts',(24.3387054348368,-0.721108343590642,
26.8392611354584));
#47793=CARTESIAN_POINT('Ctrl Pts',(24.3705330435317,-0.795485106812842,
26.4520541339887));
#47794=CARTESIAN_POINT('Ctrl Pts',(24.4023606522264,-0.675139866205197,
26.076583512025));
#47795=CARTESIAN_POINT('Ctrl Pts',(24.4341882609213,-0.389531207732191,
25.8047584596478));
#47796=CARTESIAN_POINT('Ctrl Pts',(24.4660158696161,-0.00857155315095306,
25.7031173927703));
#47797=CARTESIAN_POINT('Ctrl Pts',(24.4978434783109,0.37448628025374,25.7965404154251));
#47798=CARTESIAN_POINT('Ctrl Pts',(24.5296710870057,0.66587587465148,26.0621590690836));
#47799=CARTESIAN_POINT('Ctrl Pts',(24.5614986957005,0.79426972782966,26.4349541647604));
#47800=CARTESIAN_POINT('Ctrl Pts',(24.5933263043954,0.728239082472559,26.8236714383262));
#47801=CARTESIAN_POINT('Ctrl Pts',(24.6251539130902,0.483947182200952,27.1331591317105));
#47802=CARTESIAN_POINT('Ctrl Pts',(24.656981521785,0.121192768603945,27.2876596181516));
#47803=CARTESIAN_POINT('Ctrl Pts',(24.6888091304798,-0.271227692226556,
27.2493536549575));
#47804=CARTESIAN_POINT('Ctrl Pts',(24.7206367391747,-0.597255961333821,
27.0276179279363));
#47805=CARTESIAN_POINT('Ctrl Pts',(24.7524643478694,-0.777085544137324,
26.676729789004));
#47806=CARTESIAN_POINT('Ctrl Pts',(24.7842919565643,-0.766697041139229,
26.2825810304114));
#47807=CARTESIAN_POINT('Ctrl Pts',(24.8161195652591,-0.568633391362849,
25.9416529507056));
#47808=CARTESIAN_POINT('Ctrl Pts',(24.8479471739539,-0.231377401638892,
25.7373992792821));
#47809=CARTESIAN_POINT('Ctrl Pts',(24.8797747826487,0.16251606740706,25.7198180410551));
#47810=CARTESIAN_POINT('Ctrl Pts',(24.9116023913435,0.516628208017037,25.8932128413441));
#47811=CARTESIAN_POINT('Ctrl Pts',(24.9434300000383,0.744278044004932,26.2151394122719));
#47812=CARTESIAN_POINT('Ctrl Pts',(24.9752576087332,0.78974054437337,26.6067952892288));
#47813=CARTESIAN_POINT('Ctrl Pts',(25.007085217428,0.641887217721265,26.9723093911354));
#47814=CARTESIAN_POINT('Ctrl Pts',(25.0389128261228,0.336910188567394,27.2222097244347));
#47815=CARTESIAN_POINT('Ctrl Pts',(25.0707404348176,-0.0505370546315667,
27.2953246930265));
#47816=CARTESIAN_POINT('Ctrl Pts',(25.1025680435124,-0.425613636882587,
27.1737569245123));
#47817=CARTESIAN_POINT('Ctrl Pts',(25.1343956522073,-0.696506822711343,
26.8872642600927));
#47818=CARTESIAN_POINT('Ctrl Pts',(25.1662232609021,-0.796906302199207,
26.5059755120117));
#47819=CARTESIAN_POINT('Ctrl Pts',(25.1980508695969,-0.702235892006071,
26.1232240543678));
#47820=CARTESIAN_POINT('Ctrl Pts',(25.2298784782917,-0.435669391136255,
25.832701309116));
#47821=CARTESIAN_POINT('Ctrl Pts',(25.2617060869866,-0.0624580063800852,
25.705522587692));
#47822=CARTESIAN_POINT('Ctrl Pts',(25.2935336956813,0.326042097238796,25.7728192026347));
#47823=CARTESIAN_POINT('Ctrl Pts',(25.3253613043762,0.634732321372251,26.0181180212604));
#47824=CARTESIAN_POINT('Ctrl Pts',(25.357188913071,0.78805024694888,26.3813738245058));
#47825=CARTESIAN_POINT('Ctrl Pts',(25.3890165217658,0.748466103221927,26.7736674141299));
#47826=CARTESIAN_POINT('Ctrl Pts',(25.4208441304606,0.525669454106653,27.0989716072131));
#47827=CARTESIAN_POINT('Ctrl Pts',(25.4526717391554,0.174197348243338,27.2776571513812));
#47828=CARTESIAN_POINT('Ctrl Pts',(25.4844993478503,-0.219915476373876,
27.2659846894545));
#47829=CARTESIAN_POINT('Ctrl Pts',(25.5163269565451,-0.560196517256405,
27.0668114530277));
#47830=CARTESIAN_POINT('Ctrl Pts',(25.5481545652399,-0.763350429746691,
26.7288918579483));
#47831=CARTESIAN_POINT('Ctrl Pts',(25.5799821739347,-0.779648392280715,
26.3349432048161));
#47832=CARTESIAN_POINT('Ctrl Pts',(25.6118097826295,-0.605100924877577,
25.9813978095313));
#47833=CARTESIAN_POINT('Ctrl Pts',(25.6436373913244,-0.282434449814925,
25.7547979181797));
#47834=CARTESIAN_POINT('Ctrl Pts',(25.6754650000191,0.109367451560953,25.710611552006));
#47835=CARTESIAN_POINT('Ctrl Pts',(25.707292608714,0.474397953853924,25.8596548254688));
#47836=CARTESIAN_POINT('Ctrl Pts',(25.7391202174087,0.723303440713549,26.1654443336632));
#47837=CARTESIAN_POINT('Ctrl Pts',(25.7709478261036,0.795155838932149,26.553127707192));
#47838=CARTESIAN_POINT('Ctrl Pts',(25.8027754347984,0.672366832289694,26.9278062684317));
#47839=CARTESIAN_POINT('Ctrl Pts',(25.8346030434933,0.384993203039443,27.1977647143017));
#47840=CARTESIAN_POINT('Ctrl Pts',(25.8664306521881,0.00337940660061129,
27.2969215381445));
#47841=CARTESIAN_POINT('Ctrl Pts',(25.8982582608829,-0.379061610834525,
27.2010047503193));
#47842=CARTESIAN_POINT('Ctrl Pts',(25.9300858695777,-0.668714428418505,
26.9334932213543));
#47843=CARTESIAN_POINT('Ctrl Pts',(25.9619134782725,-0.794676659578473,
26.5598695268258));
#47844=CARTESIAN_POINT('Ctrl Pts',(25.9937410869674,-0.726114805888509,
26.1715906810597));
#47845=CARTESIAN_POINT('Ctrl Pts',(26.0255686956621,-0.479811640722421,
25.8637012684045));
#47846=CARTESIAN_POINT('Ctrl Pts',(26.057396304357,-0.116058362262509,25.7115674057289));
#47847=CARTESIAN_POINT('Ctrl Pts',(26.0892239130518,0.276104304993651,25.7524295460381));
#47848=CARTESIAN_POINT('Ctrl Pts',(26.1210515217466,0.600680758111244,25.9762843069252));
#47849=CARTESIAN_POINT('Ctrl Pts',(26.1528791304414,0.778220766932473,26.3283374916096));
#47850=CARTESIAN_POINT('Ctrl Pts',(26.1847067391362,0.765263715417021,26.7224086099901));
#47851=CARTESIAN_POINT('Ctrl Pts',(26.216534347831,0.564984430859093,27.0620420026143));
#47852=CARTESIAN_POINT('Ctrl Pts',(26.2483619565259,0.226402125810272,27.2640883311776));
#47853=CARTESIAN_POINT('Ctrl Pts',(26.2801895652207,-0.167592445455861,
27.2791135571752));
#47854=CARTESIAN_POINT('Ctrl Pts',(26.3120171739155,-0.520576980781025,
27.1033949839955));
#47855=CARTESIAN_POINT('Ctrl Pts',(26.3438447826103,-0.746106034620935,
26.7800308690168));
#47856=CARTESIAN_POINT('Ctrl Pts',(26.3756723913052,-0.789053050339413,
26.3880094871026));
#47857=CARTESIAN_POINT('Ctrl Pts',(26.3968907971017,-0.688841172942706,
26.1451000824837));
#47858=CARTESIAN_POINT('Ctrl Pts',(26.4075,-0.612682133358295,26.0429972363724));
#47859=CARTESIAN_POINT('Ctrl Pts',(9.55924498047908,-0.761351629614349,
26.8558316825899));
#47860=CARTESIAN_POINT('Ctrl Pts',(9.56985418337735,-0.820650612807892,
26.7289532181421));
#47861=CARTESIAN_POINT('Ctrl Pts',(9.59107258917389,-0.874534777171298,
26.4451092594775));
#47862=CARTESIAN_POINT('Ctrl Pts',(9.62290019786871,-0.74110841331227,26.0325432712716));
#47863=CARTESIAN_POINT('Ctrl Pts',(9.65472780656354,-0.426351906614665,
25.7345101228801));
#47864=CARTESIAN_POINT('Ctrl Pts',(9.68655541525833,-0.00719023871993623,
25.6238023694641));
#47865=CARTESIAN_POINT('Ctrl Pts',(9.71838302395318,0.413709994658858,25.7276021956329));
#47866=CARTESIAN_POINT('Ctrl Pts',(9.75021063264797,0.73335200291761,26.0204575958235));
#47867=CARTESIAN_POINT('Ctrl Pts',(9.78203824134281,0.873475187765602,26.4307052449264));
#47868=CARTESIAN_POINT('Ctrl Pts',(9.81386585003761,0.799788828170189,26.8579109271115));
#47869=CARTESIAN_POINT('Ctrl Pts',(9.84569345873243,0.530325298043976,27.1975079818376));
#47870=CARTESIAN_POINT('Ctrl Pts',(9.87752106742726,0.131047527412838,27.3663650810967));
#47871=CARTESIAN_POINT('Ctrl Pts',(9.90934867612206,-0.300309049971829,
27.3231505205938));
#47872=CARTESIAN_POINT('Ctrl Pts',(9.94117628481689,-0.658154535135611,
27.0784415750344));
#47873=CARTESIAN_POINT('Ctrl Pts',(9.97300389351169,-0.85489447176523,26.6921395788655));
#47874=CARTESIAN_POINT('Ctrl Pts',(10.0048315022065,-0.842369874069455,
26.2588048005306));
#47875=CARTESIAN_POINT('Ctrl Pts',(10.0366591109013,-0.62364667017783,25.8845107902855));
#47876=CARTESIAN_POINT('Ctrl Pts',(10.0684867195962,-0.252264737770291,
25.6608786472305));
#47877=CARTESIAN_POINT('Ctrl Pts',(10.100314328291,0.180867548628353,25.6426499754042));
#47878=CARTESIAN_POINT('Ctrl Pts',(10.1321419369858,0.569726363653874,25.8342868403763));
#47879=CARTESIAN_POINT('Ctrl Pts',(10.1639695456806,0.819125293709173,26.1888796204097));
#47880=CARTESIAN_POINT('Ctrl Pts',(10.1957971543754,0.868015482644472,26.6196296805679));
#47881=CARTESIAN_POINT('Ctrl Pts',(10.2276247630702,0.704429393468763,27.0210963134763));
#47882=CARTESIAN_POINT('Ctrl Pts',(10.2594523717651,0.368410280050912,27.2950069205873));
#47883=CARTESIAN_POINT('Ctrl Pts',(10.2912799804599,-0.0577897651425869,
27.3743125764966));
#47884=CARTESIAN_POINT('Ctrl Pts',(10.3231075891547,-0.469843801982232,
27.2396005273108));
#47885=CARTESIAN_POINT('Ctrl Pts',(10.3549351978495,-0.766887606984555,
26.9238461237048));
#47886=CARTESIAN_POINT('Ctrl Pts',(10.3867628065443,-0.876209617709942,
26.5043409825269));
#47887=CARTESIAN_POINT('Ctrl Pts',(10.4185904152391,-0.771049558237124,
26.0837732384293));
#47888=CARTESIAN_POINT('Ctrl Pts',(10.450418023934,-0.477148925554562,25.7650911341209));
#47889=CARTESIAN_POINT('Ctrl Pts',(10.4822456326288,-0.0664498838138394,
25.6263029408061));
#47890=CARTESIAN_POINT('Ctrl Pts',(10.5140732413236,0.360515024404849,25.7013817836515));
#47891=CARTESIAN_POINT('Ctrl Pts',(10.5459008500184,0.699231633110719,25.9719495653243));
#47892=CARTESIAN_POINT('Ctrl Pts',(10.5777284587132,0.866787545564904,26.3717756296248));
#47893=CARTESIAN_POINT('Ctrl Pts',(10.609556067408,0.822167760043173,26.8029889645678));
#47894=CARTESIAN_POINT('Ctrl Pts',(10.6413836761029,0.576294484860074,27.1600354573993));
#47895=CARTESIAN_POINT('Ctrl Pts',(10.6732112847977,0.189353556835892,27.3555158495422));
#47896=CARTESIAN_POINT('Ctrl Pts',(10.7050388934925,-0.243938086875568,
27.3415796742293));
#47897=CARTESIAN_POINT('Ctrl Pts',(10.7368665021873,-0.617517596846251,
27.121638283803));
#47898=CARTESIAN_POINT('Ctrl Pts',(10.7686941108822,-0.839938696900418,
26.7495298053411));
#47899=CARTESIAN_POINT('Ctrl Pts',(10.8005217195769,-0.856756266789251,
26.3163404300841));
#47900=CARTESIAN_POINT('Ctrl Pts',(10.8323493282718,-0.663853634961942,
25.9281079737816));
#47901=CARTESIAN_POINT('Ctrl Pts',(10.8641769369666,-0.308450273777893,
25.6798655190088));
#47902=CARTESIAN_POINT('Ctrl Pts',(10.8960045456614,0.122456770476399,25.6323788397758));
#47903=CARTESIAN_POINT('Ctrl Pts',(10.9278321543562,0.523388360098695,25.7972719140254));
#47904=CARTESIAN_POINT('Ctrl Pts',(10.9596597630511,0.796202868223438,26.1341815601461));
#47905=CARTESIAN_POINT('Ctrl Pts',(10.9914873717458,0.874119676029564,26.5606376968752));
#47906=CARTESIAN_POINT('Ctrl Pts',(11.0233149804407,0.738065997844413,26.9722506973317));
#47907=CARTESIAN_POINT('Ctrl Pts',(11.0551425891355,0.421345593371013,27.2682642964835));
#47908=CARTESIAN_POINT('Ctrl Pts',(11.0869701978303,0.00148654111727426,
27.3762191098691));
#47909=CARTESIAN_POINT('Ctrl Pts',(11.1187978065251,-0.418736392575163,
27.2696895295101));
#47910=CARTESIAN_POINT('Ctrl Pts',(11.1506254152199,-0.736459369020887,
26.9747522891842));
#47911=CARTESIAN_POINT('Ctrl Pts',(11.1824530239148,-0.873908896162748,
26.5636032979645));
#47912=CARTESIAN_POINT('Ctrl Pts',(11.2142806326096,-0.79743953284627,26.1368852388593));
#47913=CARTESIAN_POINT('Ctrl Pts',(11.2461082413044,-0.525769753533207,
25.7990518531489));
#47914=CARTESIAN_POINT('Ctrl Pts',(11.2779358499992,-0.125399965779644,
25.6327993387417));
#47915=CARTESIAN_POINT('Ctrl Pts',(11.309763458694,0.305665723641568,25.6788236464102));
#47916=CARTESIAN_POINT('Ctrl Pts',(11.3415910673888,0.661909343234156,25.9258587633311));
#47917=CARTESIAN_POINT('Ctrl Pts',(11.3734186760837,0.856128164921163,26.3134344524488));
#47918=CARTESIAN_POINT('Ctrl Pts',(11.4052462847785,0.840780534161899,26.7466783972681));
#47919=CARTESIAN_POINT('Ctrl Pts',(11.4370738934733,0.61962330496895,27.1195394242853));
#47920=CARTESIAN_POINT('Ctrl Pts',(11.4689015021681,0.246792222262105,27.3407471304354));
#47921=CARTESIAN_POINT('Ctrl Pts',(11.5007291108629,-0.186449640781078,
27.3561534148486));
#47922=CARTESIAN_POINT('Ctrl Pts',(11.5325567195578,-0.574051620242147,
27.1619870660381));
#47923=CARTESIAN_POINT('Ctrl Pts',(11.5643843282526,-0.821134964171277,
26.8057768940254));
#47924=CARTESIAN_POINT('Ctrl Pts',(11.5962119369474,-0.867217630314253,
26.3747174394559));
#47925=CARTESIAN_POINT('Ctrl Pts',(11.6280395456422,-0.701019320628618,
25.9743251476343));
#47926=CARTESIAN_POINT('Ctrl Pts',(11.659867154337,-0.363222717439855,25.7026096339684));
#47927=CARTESIAN_POINT('Ctrl Pts',(11.6916947630318,0.0634849851154085,
25.626082501051));
#47928=CARTESIAN_POINT('Ctrl Pts',(11.7235223717267,0.474652580874319,25.7634763644161));
#47929=CARTESIAN_POINT('Ctrl Pts',(11.7553499804215,0.769632832735413,26.0811594085096));
#47930=CARTESIAN_POINT('Ctrl Pts',(11.7871775891163,0.876219303091394,26.5013679160741));
#47931=CARTESIAN_POINT('Ctrl Pts',(11.8190051978111,0.76832133240493,26.9212415797091));
#47932=CARTESIAN_POINT('Ctrl Pts',(11.8508328065059,0.472350614473056,27.2380020564411));
#47933=CARTESIAN_POINT('Ctrl Pts',(11.8826604152007,0.0607560371216617,
27.3741114587154));
#47934=CARTESIAN_POINT('Ctrl Pts',(11.9144880238956,-0.365710644297763,
27.2962523864653));
#47935=CARTESIAN_POINT('Ctrl Pts',(11.9463156325904,-0.702657221733247,
27.0234834926246));
#47936=CARTESIAN_POINT('Ctrl Pts',(11.9781432412852,-0.867604573728051,
26.6225742303689));
#47937=CARTESIAN_POINT('Ctrl Pts',(12.00997084998,-0.820176232348615,26.1916607611821));
#47938=CARTESIAN_POINT('Ctrl Pts',(12.0417984586748,-0.571981895366318,
25.8362237954871));
#47939=CARTESIAN_POINT('Ctrl Pts',(12.0736260673696,-0.183775558327402,
25.6432686054161));
#47940=CARTESIAN_POINT('Ctrl Pts',(12.1054536760645,0.249416089770113,25.6600275287438));
#47941=CARTESIAN_POINT('Ctrl Pts',(12.1372812847593,0.621554676821614,25.882398249658));
#47942=CARTESIAN_POINT('Ctrl Pts',(12.1691088934541,0.841546641486399,26.2559479799154));
#47943=CARTESIAN_POINT('Ctrl Pts',(12.2009365021489,0.855541476923898,26.6892377329373));
#47944=CARTESIAN_POINT('Ctrl Pts',(12.2327641108438,0.660113471733214,27.0762051221055));
#47945=CARTESIAN_POINT('Ctrl Pts',(12.2645917195385,0.303100269195515,27.3221267330029));
#47946=CARTESIAN_POINT('Ctrl Pts',(12.2964193282334,-0.128107021042431,
27.3668048970004));
#47947=CARTESIAN_POINT('Ctrl Pts',(12.3282469369282,-0.527955765874044,
27.1993031156693));
#47948=CARTESIAN_POINT('Ctrl Pts',(12.360074545623,-0.798569401482301,26.860623140301));
#47949=CARTESIAN_POINT('Ctrl Pts',(12.3919021543178,-0.873706047361805,
26.4336684003829));
#47950=CARTESIAN_POINT('Ctrl Pts',(12.4237297630126,-0.734973456918116,
26.0229505728646));
#47951=CARTESIAN_POINT('Ctrl Pts',(12.4555573717074,-0.41633114463659,25.7290067987914));
#47952=CARTESIAN_POINT('Ctrl Pts',(12.4873849804023,0.00422235874845611,
25.623789802621));
#47953=CARTESIAN_POINT('Ctrl Pts',(12.5192125890971,0.423742296389348,25.7330550185607));
#47954=CARTESIAN_POINT('Ctrl Pts',(12.5510401977919,0.739536911766215,26.0300560730899));
#47955=CARTESIAN_POINT('Ctrl Pts',(12.5828678064867,0.874304744703109,26.4420918684986));
#47956=CARTESIAN_POINT('Ctrl Pts',(12.6146954151816,0.795056789803791,26.8683026463267));
#47957=CARTESIAN_POINT('Ctrl Pts',(12.6465230238764,0.521191676213231,27.2043588396197));
#47958=CARTESIAN_POINT('Ctrl Pts',(12.6783506325712,0.119747194131051,27.3679992786875));
#47959=CARTESIAN_POINT('Ctrl Pts',(12.710178241266,-0.311009481723835,27.3191674069336));
#47960=CARTESIAN_POINT('Ctrl Pts',(12.7420058499608,-0.665636021423207,
27.0698164838685));
#47961=CARTESIAN_POINT('Ctrl Pts',(12.7738334586556,-0.857325532128846,
26.6809836187735));
#47962=CARTESIAN_POINT('Ctrl Pts',(12.8056610673504,-0.839155494087598,
26.2478488646725));
#47963=CARTESIAN_POINT('Ctrl Pts',(12.8374886760453,-0.615573641376133,
25.8764366669317));
#47964=CARTESIAN_POINT('Ctrl Pts',(12.8693162847401,-0.241309227888843,
25.6576627784313));
#47965=CARTESIAN_POINT('Ctrl Pts',(12.9011438934349,0.192023816795586,25.6450795404907));
#47966=CARTESIAN_POINT('Ctrl Pts',(12.9329715021297,0.578352508954422,25.841767128069));
#47967=CARTESIAN_POINT('Ctrl Pts',(12.9647991108245,0.823109776960734,26.1995795723057));
#47968=CARTESIAN_POINT('Ctrl Pts',(12.9966267195193,0.866382964663031,26.6309301219966));
#47969=CARTESIAN_POINT('Ctrl Pts',(13.0284543282142,0.697579489309818,27.0302310764173));
#47970=CARTESIAN_POINT('Ctrl Pts',(13.060281936909,0.35801973602548,27.299739962063));
#47971=CARTESIAN_POINT('Ctrl Pts',(13.0921095456038,-0.0691775101703559,
27.3734853235121));
#47972=CARTESIAN_POINT('Ctrl Pts',(13.1239371542986,-0.479441210678199,
27.2334154782984));
#47973=CARTESIAN_POINT('Ctrl Pts',(13.1557647629934,-0.772345387466099,
26.9138172794413));
#47974=CARTESIAN_POINT('Ctrl Pts',(13.1875923716883,-0.876191792828601,
26.4929232433873));
#47975=CARTESIAN_POINT('Ctrl Pts',(13.2194199803831,-0.765560491220048,
26.0737614839233));
#47976=CARTESIAN_POINT('Ctrl Pts',(13.2512475890779,-0.467532252036404,
25.7589360812925));
#47977=CARTESIAN_POINT('Ctrl Pts',(13.2830751977727,-0.0550596113273092,
25.6255112479255));
#47978=CARTESIAN_POINT('Ctrl Pts',(13.3149028064675,0.370890739719697,25.7061472444499));
#47979=CARTESIAN_POINT('Ctrl Pts',(13.3467304151623,0.706052982451886,25.9811056713789));
#47980=CARTESIAN_POINT('Ctrl Pts',(13.3785580238572,0.868384771947934,26.3830811129317));
#47981=CARTESIAN_POINT('Ctrl Pts',(13.410385632552,0.818149888050798,26.8136764240213));
#47982=CARTESIAN_POINT('Ctrl Pts',(13.4422132412468,0.567645025155941,27.1674887742277));
#47983=CARTESIAN_POINT('Ctrl Pts',(13.4740408499416,0.17818975851907,27.3579105712504));
#47984=CARTESIAN_POINT('Ctrl Pts',(13.5058684586364,-0.254883504914502,
27.3383296113265));
#47985=CARTESIAN_POINT('Ctrl Pts',(13.5376960673312,-0.625565371708389,
27.1135389995947));
#47986=CARTESIAN_POINT('Ctrl Pts',(13.5695236760261,-0.843118862292117,
26.7385638747833));
#47987=CARTESIAN_POINT('Ctrl Pts',(13.6013512847209,-0.854290369195441,
26.3051921372114));
#47988=CARTESIAN_POINT('Ctrl Pts',(13.6331788934157,-0.656345286589309,
25.9195062420005));
#47989=CARTESIAN_POINT('Ctrl Pts',(13.6650065021105,-0.297737397961583,
25.6759159143877));
#47990=CARTESIAN_POINT('Ctrl Pts',(13.6968341108053,0.133751833446335,25.6340481622203));
#47991=CARTESIAN_POINT('Ctrl Pts',(13.7286617195001,0.532500759848507,25.8041515401575));
#47992=CARTESIAN_POINT('Ctrl Pts',(13.760489328195,0.800902035351146,26.1445874677579));
#47993=CARTESIAN_POINT('Ctrl Pts',(13.7923169368898,0.873255329742221,26.5720226865728));
#47994=CARTESIAN_POINT('Ctrl Pts',(13.8241445455846,0.731849716259112,26.9818279061198));
#47995=CARTESIAN_POINT('Ctrl Pts',(13.8559721542794,0.411299022583071,27.2736893771576));
#47996=CARTESIAN_POINT('Ctrl Pts',(13.8877997629742,-0.00993107937442886,
27.3761640896355));
#47997=CARTESIAN_POINT('Ctrl Pts',(13.9196273716691,-0.428730212279938,
27.2641678764399));
#47998=CARTESIAN_POINT('Ctrl Pts',(13.9514549803639,-0.742583061059497,
26.9651156154462));
#47999=CARTESIAN_POINT('Ctrl Pts',(13.9832825890587,-0.874663478876854,
26.5522105068295));
#48000=CARTESIAN_POINT('Ctrl Pts',(14.0151101977535,-0.792640296482183,
26.1265251029895));
#48001=CARTESIAN_POINT('Ctrl Pts',(14.0469378064483,-0.516591474228984,
25.7922603677493));
#48002=CARTESIAN_POINT('Ctrl Pts',(14.0787654151431,-0.11408933919623,25.6312389505819));
#48003=CARTESIAN_POINT('Ctrl Pts',(14.110593023838,0.31634003740729,25.6828763135011));
#48004=CARTESIAN_POINT('Ctrl Pts',(14.1424206325327,0.669334443264024,25.9345324577265));
#48005=CARTESIAN_POINT('Ctrl Pts',(14.1742482412276,0.858486505740013,26.3246059927858));
#48006=CARTESIAN_POINT('Ctrl Pts',(14.2060758499224,0.837494831737601,26.7576131695336));
#48007=CARTESIAN_POINT('Ctrl Pts',(14.2379034586172,0.61149784659057,27.127560771495));
#48008=CARTESIAN_POINT('Ctrl Pts',(14.269731067312,0.235815989902934,27.3438915553615));
#48009=CARTESIAN_POINT('Ctrl Pts',(14.3015586760069,-0.197589841370465,
27.3536512126692));
#48010=CARTESIAN_POINT('Ctrl Pts',(14.3333862847017,-0.582628846516562,
27.1544507357404));
#48011=CARTESIAN_POINT('Ctrl Pts',(14.3652138933965,-0.82504964861758,26.7950512084713));
#48012=CARTESIAN_POINT('Ctrl Pts',(14.3970415020913,-0.865511520925932,
26.363427874554));
#48013=CARTESIAN_POINT('Ctrl Pts',(14.4288691107861,-0.694110045637806,
25.9652352079194));
#48014=CARTESIAN_POINT('Ctrl Pts',(14.4606967194809,-0.352801556619993,
25.697944390986));
#48015=CARTESIAN_POINT('Ctrl Pts',(14.4925243281758,0.0748670986296862,
25.6269839315069));
#48016=CARTESIAN_POINT('Ctrl Pts',(14.5243519368706,0.484209488131278,25.7697238125832));
#48017=CARTESIAN_POINT('Ctrl Pts',(14.5561795455654,0.775025156020058,26.0912235992129));
#48018=CARTESIAN_POINT('Ctrl Pts',(14.5880071542602,0.876127088093716,26.5127852967419));
#48019=CARTESIAN_POINT('Ctrl Pts',(14.619834762955,0.762767151878309,26.9312173585558));
#48020=CARTESIAN_POINT('Ctrl Pts',(14.6516623716498,0.462694042786029,27.2440943227002));
#48021=CARTESIAN_POINT('Ctrl Pts',(14.6834899803447,0.0493608482442458,
27.3748289232558));
#48022=CARTESIAN_POINT('Ctrl Pts',(14.7153175890395,-0.376055090774514,
27.2914194254673));
#48023=CARTESIAN_POINT('Ctrl Pts',(14.7471451977343,-0.709418771116283,
27.0142831374761));
#48024=CARTESIAN_POINT('Ctrl Pts',(14.7789728064291,-0.869128107104919,
26.6112585805436));
#48025=CARTESIAN_POINT('Ctrl Pts',(14.8108004151239,-0.816088813168395,
26.1809997063861));
#48026=CARTESIAN_POINT('Ctrl Pts',(14.8426280238187,-0.56328405832972,25.8288269910552));
#48027=CARTESIAN_POINT('Ctrl Pts',(14.8744556325136,-0.172596394528967,
25.6409466705146));
#48028=CARTESIAN_POINT('Ctrl Pts',(14.9062832412084,0.260340100216139,25.6633488358199));
#48029=CARTESIAN_POINT('Ctrl Pts',(14.9381108499032,0.629549511251965,25.8905497959745));
#48030=CARTESIAN_POINT('Ctrl Pts',(14.969938458598,0.844655292576574,26.26693439759));
#48031=CARTESIAN_POINT('Ctrl Pts',(15.0017660672929,0.853002996713588,26.7003697230172));
#48032=CARTESIAN_POINT('Ctrl Pts',(15.0335936759876,0.652549239490231,27.0847577518469));
#48033=CARTESIAN_POINT('Ctrl Pts',(15.0654212846825,0.29236188773074,27.3260064557296));
#48034=CARTESIAN_POINT('Ctrl Pts',(15.0972488933773,-0.139390968065011,
27.3650620187745));
#48035=CARTESIAN_POINT('Ctrl Pts',(15.1290765020721,-0.537023149086413,
27.1923642651449));
#48036=CARTESIAN_POINT('Ctrl Pts',(15.1609041107669,-0.803200670809313,
26.8501868368683));
#48037=CARTESIAN_POINT('Ctrl Pts',(15.1927317194618,-0.872767542303841,
26.4222892838454));
#48038=CARTESIAN_POINT('Ctrl Pts',(15.2245593281565,-0.728694908470672,
26.0134140685621));
#48039=CARTESIAN_POINT('Ctrl Pts',(15.2563869368514,-0.406249440824799,
25.7236472901227));
#48040=CARTESIAN_POINT('Ctrl Pts',(15.2882145455462,0.015639378424601,25.6239192114041));
#48041=CARTESIAN_POINT('Ctrl Pts',(15.320042154241,0.433699928509178,25.7386416675996));
#48042=CARTESIAN_POINT('Ctrl Pts',(15.3518697629358,0.745597687591262,26.0397324402448));
#48043=CARTESIAN_POINT('Ctrl Pts',(15.3836973716307,0.874985083455662,26.4534893341863));
#48044=CARTESIAN_POINT('Ctrl Pts',(15.4155249803254,0.790190155461937,26.8786312936292));
#48045=CARTESIAN_POINT('Ctrl Pts',(15.4473525890203,0.511969342859715,27.2110903812289));
#48046=CARTESIAN_POINT('Ctrl Pts',(15.4791801977151,0.108426641151977,27.3694859411127));
#48047=CARTESIAN_POINT('Ctrl Pts',(15.5110078064099,-0.321657164409033,
27.3150452790421));
#48048=CARTESIAN_POINT('Ctrl Pts',(15.5428354151047,-0.673004451758036,
27.061094596497));
#48049=CARTESIAN_POINT('Ctrl Pts',(15.5746630237996,-0.85961103647116,26.6697969501533));
#48050=CARTESIAN_POINT('Ctrl Pts',(15.6064906324944,-0.835798617607276,
26.2369357319776));
#48051=CARTESIAN_POINT('Ctrl Pts',(15.6383182411892,-0.607396093630348,
25.8684684301265));
#48052=CARTESIAN_POINT('Ctrl Pts',(15.670145849884,-0.230312741493113,25.6545899341678));
#48053=CARTESIAN_POINT('Ctrl Pts',(15.7019734585788,0.203147478227175,25.6476542717921));
#48054=CARTESIAN_POINT('Ctrl Pts',(15.7338010672736,0.586880451397411,25.8493591819813));
#48055=CARTESIAN_POINT('Ctrl Pts',(15.7656286759684,0.826954496793968,26.2103305357195));
#48056=CARTESIAN_POINT('Ctrl Pts',(15.7974562846633,0.864603336095876,26.6422083313882));
#48057=CARTESIAN_POINT('Ctrl Pts',(15.8292838933581,0.690611136890996,27.0392758068989));
#48058=CARTESIAN_POINT('Ctrl Pts',(15.8611115020529,0.347568400735895,27.304337208585));
#48059=CARTESIAN_POINT('Ctrl Pts',(15.8929391107477,-0.0805535089695269,
27.372509753812));
#48060=CARTESIAN_POINT('Ctrl Pts',(15.9247667194425,-0.488957210819473,
27.2271058962022));
#48061=CARTESIAN_POINT('Ctrl Pts',(15.9565943281374,-0.777672024640725,
26.9037181695138));
#48062=CARTESIAN_POINT('Ctrl Pts',(15.9884219368322,-0.876025191633466,
26.4815067058666));
#48063=CARTESIAN_POINT('Ctrl Pts',(16.020249545527,-0.759941432957373,26.0638221042063));
#48064=CARTESIAN_POINT('Ctrl Pts',(16.0520771542218,-0.457836192104619,
25.7529068602219));
#48065=CARTESIAN_POINT('Ctrl Pts',(16.0839047629166,-0.0436599897858236,
25.6248680421809));
#48066=CARTESIAN_POINT('Ctrl Pts',(16.1157323716114,0.381203478234709,25.7110475004881));
#48067=CARTESIAN_POINT('Ctrl Pts',(16.1475599803063,0.712754444848184,25.9903498850648));
#48068=CARTESIAN_POINT('Ctrl Pts',(16.1793875890011,0.869834547644324,26.3944064489244));
#48069=CARTESIAN_POINT('Ctrl Pts',(16.2112151976959,0.813993095194338,26.8243106215965));
#48070=CARTESIAN_POINT('Ctrl Pts',(16.2430428063907,0.558899180011339,27.1748287522675));
#48071=CARTESIAN_POINT('Ctrl Pts',(16.2748704150855,0.166995703796211,27.3601596207786));
#48072=CARTESIAN_POINT('Ctrl Pts',(16.3066980237803,-0.265785644041754,
27.334937201067));
#48073=CARTESIAN_POINT('Ctrl Pts',(16.3385256324752,-0.633506926325045,
27.1053355372044));
#48074=CARTESIAN_POINT('Ctrl Pts',(16.37035324117,-0.84615586711807,26.7275574363672));
#48075=CARTESIAN_POINT('Ctrl Pts',(16.4021808498648,-0.851679414127489,
26.2940769224788));
#48076=CARTESIAN_POINT('Ctrl Pts',(16.4340084585596,-0.648725491578761,
25.9110030773592));
#48077=CARTESIAN_POINT('Ctrl Pts',(16.4658360672544,-0.286973966694253,
25.6721062382503));
#48078=CARTESIAN_POINT('Ctrl Pts',(16.4976636759493,0.145024185516322,25.6358645222422));
#48079=CARTESIAN_POINT('Ctrl Pts',(16.5294912846441,0.541522741611643,25.8111493205188));
#48080=CARTESIAN_POINT('Ctrl Pts',(16.5613188933389,0.805465210279413,26.1550537239889));
#48081=CARTESIAN_POINT('Ctrl Pts',(16.5931465020337,0.872242705753262,26.583395446905));
#48082=CARTESIAN_POINT('Ctrl Pts',(16.6249741107285,0.725509167474942,26.9913233011108));
#48083=CARTESIAN_POINT('Ctrl Pts',(16.6568017194234,0.401182613717069,27.2789830863088));
#48084=CARTESIAN_POINT('Ctrl Pts',(16.6886293281181,-0.0213470135804936,
27.3759602977967));
#48085=CARTESIAN_POINT('Ctrl Pts',(16.720456936813,-0.438651234112523,27.2585164685856));
#48086=CARTESIAN_POINT('Ctrl Pts',(16.7522845455078,-0.748580663388893,
26.9553999656387));
#48087=CARTESIAN_POINT('Ctrl Pts',(16.7841121542026,-0.875269544789723,
26.5408088504112));
#48088=CARTESIAN_POINT('Ctrl Pts',(16.8159397628974,-0.787706470747481,
26.1162283827109));
#48089=CARTESIAN_POINT('Ctrl Pts',(16.8477673715922,-0.507325478323994,
25.7855890556777));
#48090=CARTESIAN_POINT('Ctrl Pts',(16.8795949802871,-0.10275934036483,25.629826077015));
#48091=CARTESIAN_POINT('Ctrl Pts',(16.9114225889819,0.326960636986347,25.6870677271803));
#48092=CARTESIAN_POINT('Ctrl Pts',(16.9432501976767,0.676645891169302,25.9433021678813));
#48093=CARTESIAN_POINT('Ctrl Pts',(16.9750778063715,0.8606990764792,26.3358073147138));
#48094=CARTESIAN_POINT('Ctrl Pts',(17.0069054150664,0.834066923902435,26.7685041995821));
#48095=CARTESIAN_POINT('Ctrl Pts',(17.0387330237611,0.60326855623544,27.1354755592871));
#48096=CARTESIAN_POINT('Ctrl Pts',(17.070560632456,0.224799716990748,27.3468926891914));
#48097=CARTESIAN_POINT('Ctrl Pts',(17.1023882411507,-0.208696492798159,
27.3510040602751));
#48098=CARTESIAN_POINT('Ctrl Pts',(17.1342158498456,-0.591107140557163,
27.1468032828924));
#48099=CARTESIAN_POINT('Ctrl Pts',(17.1660434585404,-0.82882424545982,26.7842754190553));
#48100=CARTESIAN_POINT('Ctrl Pts',(17.1978710672352,-0.863658439603519,
26.3521615079739));
#48101=CARTESIAN_POINT('Ctrl Pts',(17.22969867593,-0.687082928822622,25.9562360544967));
#48102=CARTESIAN_POINT('Ctrl Pts',(17.2615262846249,-0.342320457998925,
25.6934153665245));
#48103=CARTESIAN_POINT('Ctrl Pts',(17.2933538933197,0.086236438391831,25.6280335415497));
#48104=CARTESIAN_POINT('Ctrl Pts',(17.3251815020145,0.493684293154122,25.7760953693158));
#48105=CARTESIAN_POINT('Ctrl Pts',(17.3570091107093,0.780285662025571,26.1013569946918));
#48106=CARTESIAN_POINT('Ctrl Pts',(17.3888367194041,0.875886521181471,26.5242008934958));
#48107=CARTESIAN_POINT('Ctrl Pts',(17.4206643280989,0.757082673810857,26.9411191864539));
#48108=CARTESIAN_POINT('Ctrl Pts',(17.4524919367938,0.452960380137535,27.2500616224666));
#48109=CARTESIAN_POINT('Ctrl Pts',(17.4843195454886,0.0379544948769752,
27.375395237509));
#48110=CARTESIAN_POINT('Ctrl Pts',(17.5161471541834,-0.386330428534896,
27.2864570019139));
#48111=CARTESIAN_POINT('Ctrl Pts',(17.5479747628782,-0.716069784581872,
27.0049861686412));
#48112=CARTESIAN_POINT('Ctrl Pts',(17.579802371573,-0.870485327848165,26.5999415787028));
#48113=CARTESIAN_POINT('Ctrl Pts',(17.6116299802679,-0.811898199690783,
26.1703596993712));
#48114=CARTESIAN_POINT('Ctrl Pts',(17.6434575889627,-0.554423780325743,
25.8216066833014));
#48115=CARTESIAN_POINT('Ctrl Pts',(17.6752851976575,-0.161514030550117,
25.6386525392877));
#48116=CARTESIAN_POINT('Ctrl Pts',(17.7071128063523,0.271457872908683,25.6670350399784));
#48117=CARTESIAN_POINT('Ctrl Pts',(17.7389404150471,0.636989319376892,25.8983848159446));
#48118=CARTESIAN_POINT('Ctrl Pts',(17.7707680237419,0.848456858924584,26.2787473491137));
#48119=CARTESIAN_POINT('Ctrl Pts',(17.8025956324368,0.848820515726568,26.7100314241014));
#48120=CARTESIAN_POINT('Ctrl Pts',(17.8450324440298,0.579834016898176,27.2240442104363));
#48121=CARTESIAN_POINT('Ctrl Pts',(17.8980784585212,-0.170889696122602,
27.4791305910779));
#48122=CARTESIAN_POINT('Ctrl Pts',(17.9511244730126,-0.790819799983081,
26.9848211523576));
#48123=CARTESIAN_POINT('Ctrl Pts',(17.9935612846056,-0.869783785083159,
26.4100798452247));
#48124=CARTESIAN_POINT('Ctrl Pts',(18.0253888933005,-0.723346098358382,
26.0044173136901));
#48125=CARTESIAN_POINT('Ctrl Pts',(18.0572165019953,-0.395534844509592,
25.7181762286391));
#48126=CARTESIAN_POINT('Ctrl Pts',(18.0890441106901,0.0267543597305262,
25.6243264274723));
#48127=CARTESIAN_POINT('Ctrl Pts',(18.1208717193849,0.443742562875346,25.7442892299081));
#48128=CARTESIAN_POINT('Ctrl Pts',(18.1526993280798,0.75144783238784,26.0495231687072));
#48129=CARTESIAN_POINT('Ctrl Pts',(18.1845269367746,0.875561354462757,26.4648755209135));
#48130=CARTESIAN_POINT('Ctrl Pts',(18.2163545454694,0.785165778302637,26.8889058057357));
#48131=CARTESIAN_POINT('Ctrl Pts',(18.2481821541642,0.50267256024079,27.2176958019182));
#48132=CARTESIAN_POINT('Ctrl Pts',(18.280009762859,0.097081066669982,27.370827814419));
#48133=CARTESIAN_POINT('Ctrl Pts',(18.3118373715538,-0.332246728994801,
27.3107832488446));
#48134=CARTESIAN_POINT('Ctrl Pts',(18.3436649802486,-0.680260460945816,
27.052278234901));
#48135=CARTESIAN_POINT('Ctrl Pts',(18.3754925889435,-0.861749597906357,
26.6585810270827));
#48136=CARTESIAN_POINT('Ctrl Pts',(18.4073201976383,-0.832300343595772,
26.2260674913711));
#48137=CARTESIAN_POINT('Ctrl Pts',(18.4391478063331,-0.599115135331636,
25.8606073079395));
#48138=CARTESIAN_POINT('Ctrl Pts',(18.4709754150279,-0.219277294139984,
25.6516607023674));
#48139=CARTESIAN_POINT('Ctrl Pts',(18.5028030237227,0.214236722714413,25.6503736970824));
#48140=CARTESIAN_POINT('Ctrl Pts',(18.5346306324176,0.59530870133453,25.8570617315489));
#48141=CARTESIAN_POINT('Ctrl Pts',(18.5664582411124,0.830658822419003,26.2211306753223));
#48142=CARTESIAN_POINT('Ctrl Pts',(18.5982858498072,0.862676887449892,26.6534623989214));
#48143=CARTESIAN_POINT('Ctrl Pts',(18.630113458502,0.683525525611608,27.0482289663804));
#48144=CARTESIAN_POINT('Ctrl Pts',(18.6619410671968,0.33705804553252,27.308797881006));
#48145=CARTESIAN_POINT('Ctrl Pts',(18.6937686758916,-0.0919158281754816,
27.3713860322737));
#48146=CARTESIAN_POINT('Ctrl Pts',(18.7255962845865,-0.498390187518964,
27.2206728527908));
#48147=CARTESIAN_POINT('Ctrl Pts',(18.7574238932813,-0.782866613565596,
26.893550508522));
#48148=CARTESIAN_POINT('Ctrl Pts',(18.7892515019761,-0.875709842670763,
26.4700933085941));
#48149=CARTESIAN_POINT('Ctrl Pts',(18.8210791106709,-0.754193337422004,
26.053956786912));
#48150=CARTESIAN_POINT('Ctrl Pts',(18.8529067193657,-0.448062392210722,
25.7470044946958));
#48151=CARTESIAN_POINT('Ctrl Pts',(18.8847343280605,-0.0322529547931279,
25.6243734327709));
#48152=CARTESIAN_POINT('Ctrl Pts',(18.9165619367554,0.39145148883905,25.7160817197175));
#48153=CARTESIAN_POINT('Ctrl Pts',(18.9483895454502,0.719334882410106,25.9996806367208));
#48154=CARTESIAN_POINT('Ctrl Pts',(18.980217154145,0.87113662647824,26.4057497145772));
#48155=CARTESIAN_POINT('Ctrl Pts',(19.0120447628398,0.809698087295199,26.834889751618));
#48156=CARTESIAN_POINT('Ctrl Pts',(19.0438723715346,0.550058434458596,27.1820541452));
#48157=CARTESIAN_POINT('Ctrl Pts',(19.0756999802295,0.155773293405102,27.3622626162404));
#48158=CARTESIAN_POINT('Ctrl Pts',(19.1075275889243,-0.276642653087724,
27.3314030194782));
#48159=CARTESIAN_POINT('Ctrl Pts',(19.1393551976191,-0.641340912229586,
27.09702928957));
#48160=CARTESIAN_POINT('Ctrl Pts',(19.1711828063139,-0.849049195698639,
26.716512358973));
#48161=CARTESIAN_POINT('Ctrl Pts',(19.2030104150088,-0.84892384492235,26.2829966732363));
#48162=CARTESIAN_POINT('Ctrl Pts',(19.2348380237035,-0.64099554376236,25.902599923685));
#48163=CARTESIAN_POINT('Ctrl Pts',(19.2666656323984,-0.276161807593532,
25.6684371374749));
#48164=CARTESIAN_POINT('Ctrl Pts',(19.2984932410932,0.156271912654531,25.6378276114259));
#48165=CARTESIAN_POINT('Ctrl Pts',(19.330320849788,0.550452773466548,25.8182640668944));
#48166=CARTESIAN_POINT('Ctrl Pts',(19.3621484584828,0.809891618186575,26.1655785516815));
#48167=CARTESIAN_POINT('Ctrl Pts',(19.3939760671776,0.871081976005171,26.594754046791));
#48168=CARTESIAN_POINT('Ctrl Pts',(19.4258036758724,0.719045428109123,27.0007352699978));
#48169=CARTESIAN_POINT('Ctrl Pts',(19.4576312845673,0.39099808452758,27.2841445250718));
#48170=CARTESIAN_POINT('Ctrl Pts',(19.4894588932621,-0.0327593230900933,
27.3756077689554));
#48171=CARTESIAN_POINT('Ctrl Pts',(19.5212865019569,-0.448497773493383,
27.2527362655511));
#48172=CARTESIAN_POINT('Ctrl Pts',(19.5531141106517,-0.754451157627163,
26.9456069894642));
#48173=CARTESIAN_POINT('Ctrl Pts',(19.5849417193465,-0.875726990985035,
26.5294002647037));
#48174=CARTESIAN_POINT('Ctrl Pts',(19.6167693280414,-0.782638893413152,
26.1059968263815));
#48175=CARTESIAN_POINT('Ctrl Pts',(19.6485969367361,-0.497973339148,25.7790390497384));
#48176=CARTESIAN_POINT('Ctrl Pts',(19.680424545431,-0.0914118931530433,
25.6285609579009));
#48177=CARTESIAN_POINT('Ctrl Pts',(19.7122521541258,0.337525719103477,25.6913971758347));
#48178=CARTESIAN_POINT('Ctrl Pts',(19.7440797628206,0.683842445305621,25.9521664045508));
#48179=CARTESIAN_POINT('Ctrl Pts',(19.7759073715154,0.86276550176665,26.3470365165613));
#48180=CARTESIAN_POINT('Ctrl Pts',(19.8077349802103,0.830497392107225,26.7793496375646));
#48181=CARTESIAN_POINT('Ctrl Pts',(19.839562588905,0.594936832367246,27.1432824448073));
#48182=CARTESIAN_POINT('Ctrl Pts',(19.8713901975999,0.213745271922699,27.3497500203207));
#48183=CARTESIAN_POINT('Ctrl Pts',(19.9032178062947,-0.219767705103356,
27.3482124109549));
#48184=CARTESIAN_POINT('Ctrl Pts',(19.9350454149895,-0.599485070434967,
27.1390459988373));
#48185=CARTESIAN_POINT('Ctrl Pts',(19.9668730236843,-0.832458099283822,
26.7734513690606));
#48186=CARTESIAN_POINT('Ctrl Pts',(19.9987006323791,-0.861658728362201,
26.3409202271136));
#48187=CARTESIAN_POINT('Ctrl Pts',(20.030528241074,-0.679939111709783,25.9473292637821));
#48188=CARTESIAN_POINT('Ctrl Pts',(20.0623558497688,-0.33178129881649,25.6890232382737));
#48189=CARTESIAN_POINT('Ctrl Pts',(20.0941834584636,0.0975912581185316,
25.6292313254123));
#48190=CARTESIAN_POINT('Ctrl Pts',(20.1260110671584,0.503075039293507,25.7825896271002));
#48191=CARTESIAN_POINT('Ctrl Pts',(20.1578386758532,0.78541411431491,26.1115584891656));
#48192=CARTESIAN_POINT('Ctrl Pts',(20.189666284548,0.875496403048518,26.5356116070047));
#48193=CARTESIAN_POINT('Ctrl Pts',(20.2214938932429,0.751271205083277,26.9509475742446));
#48194=CARTESIAN_POINT('Ctrl Pts',(20.2533215019377,0.443146857755472,27.2558988032573));
#48195=CARTESIAN_POINT('Ctrl Pts',(20.2851491106325,0.0265472625644233,
27.3758181210472));
#48196=CARTESIAN_POINT('Ctrl Pts',(20.3169767193273,-0.396550676993438,
27.2813512007288));
#48197=CARTESIAN_POINT('Ctrl Pts',(20.3488043280222,-0.722579366878462,
26.9956220302467));
#48198=CARTESIAN_POINT('Ctrl Pts',(20.3806319367169,-0.871732209510478,
26.5885725307662));
#48199=CARTESIAN_POINT('Ctrl Pts',(20.4124595454118,-0.807498979687936,
26.1598418954261));
#48200=CARTESIAN_POINT('Ctrl Pts',(20.4442871541066,-0.545602942518351,
25.8143765119107));
#48201=CARTESIAN_POINT('Ctrl Pts',(20.4761147628014,-0.150152050138101,
25.6367407688628));
#48202=CARTESIAN_POINT('Ctrl Pts',(20.5079423714962,0.282053657425552,25.6704170489714));
#48203=CARTESIAN_POINT('Ctrl Pts',(20.539769980191,0.645217150507662,25.9071619386416));
#48204=CARTESIAN_POINT('Ctrl Pts',(20.5715975888859,0.850441826915244,26.2890240835133));
#48205=CARTESIAN_POINT('Ctrl Pts',(20.6034251975807,0.847491975277755,26.7225297511439));
#48206=CARTESIAN_POINT('Ctrl Pts',(20.6352528062755,0.637089671994789,27.1015637024804));
#48207=CARTESIAN_POINT('Ctrl Pts',(20.6670804149703,0.270738028507132,27.3333445015265));
#48208=CARTESIAN_POINT('Ctrl Pts',(20.6989080236651,-0.161885944873748,
27.3611359237407));
#48209=CARTESIAN_POINT('Ctrl Pts',(20.7307356323599,-0.554882833714983,
27.1781350744157));
#48210=CARTESIAN_POINT('Ctrl Pts',(20.7625632410548,-0.812053298722016,
26.8291376282637));
#48211=CARTESIAN_POINT('Ctrl Pts',(20.7943908497496,-0.870446132080706,
26.3995725662476));
#48212=CARTESIAN_POINT('Ctrl Pts',(20.8262184584444,-0.715767704125924,
25.9945905303274));
#48213=CARTESIAN_POINT('Ctrl Pts',(20.8580460671392,-0.385880814780212,
25.7133246317007));
#48214=CARTESIAN_POINT('Ctrl Pts',(20.8898736758341,0.0384635129888852,
25.6246242541211));
#48215=CARTESIAN_POINT('Ctrl Pts',(20.9217012845288,0.453392589285155,25.7502018282994));
#48216=CARTESIAN_POINT('Ctrl Pts',(20.9535288932237,0.757338426861943,26.0593179768783));
#48217=CARTESIAN_POINT('Ctrl Pts',(20.9853565019185,0.875899956432333,26.4763060213094));
#48218=CARTESIAN_POINT('Ctrl Pts',(21.0171841106133,0.780055215903818,26.8990939719485));
#48219=CARTESIAN_POINT('Ctrl Pts',(21.0490117193081,0.493265461524222,27.2241901150745));
#48220=CARTESIAN_POINT('Ctrl Pts',(21.080839328003,0.0857322283975826,27.3720161256069));
#48221=CARTESIAN_POINT('Ctrl Pts',(21.1126669366977,-0.342786880094173,
27.3063865655749));
#48222=CARTESIAN_POINT('Ctrl Pts',(21.1444945453926,-0.687397254648788,
27.0433664993406));
#48223=CARTESIAN_POINT('Ctrl Pts',(21.1763221540874,-0.863743799112817,
26.6473390233391));
#48224=CARTESIAN_POINT('Ctrl Pts',(21.2081497627822,-0.828659705946547,
26.2152453160263));
#48225=CARTESIAN_POINT('Ctrl Pts',(21.239977371477,-0.590732998816771,25.8528549912012));
#48226=CARTESIAN_POINT('Ctrl Pts',(21.2718049801718,-0.208204322055058,
25.6488753918597));
#48227=CARTESIAN_POINT('Ctrl Pts',(21.3036325888667,0.22528943557288,25.6532374544635));
#48228=CARTESIAN_POINT('Ctrl Pts',(21.3354601975615,0.603635950391702,25.8648734160034));
#48229=CARTESIAN_POINT('Ctrl Pts',(21.3672878062563,0.834222059846133,26.2319781852714));
#48230=CARTESIAN_POINT('Ctrl Pts',(21.3991154149511,0.860603980257829,26.6646903988359));
#48231=CARTESIAN_POINT('Ctrl Pts',(21.4309430236459,0.676323840368784,27.0570890424817));
#48232=CARTESIAN_POINT('Ctrl Pts',(21.4627706323408,0.326490464716284,27.313121217749));
#48233=CARTESIAN_POINT('Ctrl Pts',(21.4945982410355,-0.103262543593578,
27.3701143519073));
#48234=CARTESIAN_POINT('Ctrl Pts',(21.5264258497304,-0.507738536360471,
27.2141174392205));
#48235=CARTESIAN_POINT('Ctrl Pts',(21.5582534584252,-0.787928273639996,
26.8833160235407));
#48236=CARTESIAN_POINT('Ctrl Pts',(21.59008106712,-0.875245798726787,26.4586849892235));
#48237=CARTESIAN_POINT('Ctrl Pts',(21.6219086758148,-0.748317181035922,
26.0441672073328));
#48238=CARTESIAN_POINT('Ctrl Pts',(21.6537362845097,-0.438212511721132,
25.741229986837));
#48239=CARTESIAN_POINT('Ctrl Pts',(21.6855638932045,-0.0208404433628588,
25.6240275037281));
#48240=CARTESIAN_POINT('Ctrl Pts',(21.7173915018993,0.401633031492615,25.7212490473082));
#48241=CARTESIAN_POINT('Ctrl Pts',(21.7492191105941,0.725793177755637,26.0090963420102));
#48242=CARTESIAN_POINT('Ctrl Pts',(21.7810467192889,0.872290787375023,26.4171089838099));
#48243=CARTESIAN_POINT('Ctrl Pts',(21.8128743279837,0.805265593631672,26.8454120177663));
#48244=CARTESIAN_POINT('Ctrl Pts',(21.8447019366786,0.541124289650361,27.18916372616));
#48245=CARTESIAN_POINT('Ctrl Pts',(21.8765295453734,0.144524432895027,27.3642192005508));
#48246=CARTESIAN_POINT('Ctrl Pts',(21.9083571540682,-0.287452688544044,
27.3277276666593));
#48247=CARTESIAN_POINT('Ctrl Pts',(21.940184762763,-0.649065999221366,27.0886216670826));
#48248=CARTESIAN_POINT('Ctrl Pts',(21.9720123714578,-0.851798356749761,
26.7054305180414));
#48249=CARTESIAN_POINT('Ctrl Pts',(22.0038399801527,-0.846024129472541,
26.271953270897));
#48250=CARTESIAN_POINT('Ctrl Pts',(22.0356675888474,-0.633156755675803,
25.894298207823));
#48251=CARTESIAN_POINT('Ctrl Pts',(22.0674951975423,-0.265302756551086,
25.6649092350704));
#48252=CARTESIAN_POINT('Ctrl Pts',(22.0993228062371,0.167493105010496,25.639937096441));
#48253=CARTESIAN_POINT('Ctrl Pts',(22.1311504149319,0.559289339104509,25.8254945712091));
#48254=CARTESIAN_POINT('Ctrl Pts',(22.1629780236267,0.814180507473988,26.1761601637325));
#48255=CARTESIAN_POINT('Ctrl Pts',(22.1948056323215,0.869773337588301,26.6060965575542));
#48256=CARTESIAN_POINT('Ctrl Pts',(22.2266332410164,0.712459595697104,27.01006221464));
#48257=CARTESIAN_POINT('Ctrl Pts',(22.2584608497112,0.380747164334811,27.2891728170403));
#48258=CARTESIAN_POINT('Ctrl Pts',(22.290288458406,-0.0441660701058053,
27.3751065629715));
#48259=CARTESIAN_POINT('Ctrl Pts',(22.3221160671008,-0.458268158493986,
27.2468282488062));
#48260=CARTESIAN_POINT('Ctrl Pts',(22.3539436757956,-0.760193546967717,
26.9357383497616));
#48261=CARTESIAN_POINT('Ctrl Pts',(22.3857712844904,-0.876035739796036,
26.5179866868646));
#48262=CARTESIAN_POINT('Ctrl Pts',(22.4175988931853,-0.777438424934401,
26.09583217132));
#48263=CARTESIAN_POINT('Ctrl Pts',(22.4494265018801,-0.488536644708137,
25.7726114620908));
#48264=CARTESIAN_POINT('Ctrl Pts',(22.4812541105749,-0.080048924296243,
25.6274438080998));
#48265=CARTESIAN_POINT('Ctrl Pts',(22.5130817192697,0.348033489730768,25.6958639242453));
#48266=CARTESIAN_POINT('Ctrl Pts',(22.5449093279645,0.690922883876116,25.9611236627568));
#48267=CARTESIAN_POINT('Ctrl Pts',(22.5767369366594,0.864685430406076,26.358291691324));
#48268=CARTESIAN_POINT('Ctrl Pts',(22.6085645453542,0.826786843057951,26.790147642504));
#48269=CARTESIAN_POINT('Ctrl Pts',(22.640392154049,0.586504088562538,27.1509801013885));
#48270=CARTESIAN_POINT('Ctrl Pts',(22.6722197627438,0.202654533882945,27.3524630655935));
#48271=CARTESIAN_POINT('Ctrl Pts',(22.7040473714386,-0.230801602472313,
27.3452767349221));
#48272=CARTESIAN_POINT('Ctrl Pts',(22.7358749801335,-0.607761205912453,
27.1311802079376));
#48273=CARTESIAN_POINT('Ctrl Pts',(22.7677025888282,-0.835950607557777,
26.7625808828307));
#48274=CARTESIAN_POINT('Ctrl Pts',(22.7995301975231,-0.859512699386321,
26.3297059663465));
#48275=CARTESIAN_POINT('Ctrl Pts',(22.8313578062179,-0.672679858980042,
25.9385162997673));
#48276=CARTESIAN_POINT('Ctrl Pts',(22.8631854149127,-0.321185771047252,
25.6847688433449));
#48277=CARTESIAN_POINT('Ctrl Pts',(22.8950130236075,0.108929445558247,25.630576907257));
#48278=CARTESIAN_POINT('Ctrl Pts',(22.9268406323023,0.51238047985094,25.7892058088504));
#48279=CARTESIAN_POINT('Ctrl Pts',(22.9586682409972,0.790408985292522,26.1218257355752));
#48280=CARTESIAN_POINT('Ctrl Pts',(22.990495849692,0.874958040090555,26.5470166607199));
#48281=CARTESIAN_POINT('Ctrl Pts',(23.0223234583868,0.745331390812788,26.9606986609199));
#48282=CARTESIAN_POINT('Ctrl Pts',(23.0541510670816,0.433259563500411,27.2616090131687));
#48283=CARTESIAN_POINT('Ctrl Pts',(23.0859786757764,0.0151327394813605,
27.3760896863336));
#48284=CARTESIAN_POINT('Ctrl Pts',(23.1178062844713,-0.406698336609806,
27.2761176465609));
#48285=CARTESIAN_POINT('Ctrl Pts',(23.1496338931661,-0.728976178604333,
26.9861644467994));
#48286=CARTESIAN_POINT('Ctrl Pts',(23.1814615018609,-0.872812336365727,
26.577205982878));
#48287=CARTESIAN_POINT('Ctrl Pts',(23.2132891105557,-0.802998023931051,
26.1493487318329));
#48288=CARTESIAN_POINT('Ctrl Pts',(23.2451167192505,-0.536622665975705,
25.807325290872));
#48289=CARTESIAN_POINT('Ctrl Pts',(23.2769443279453,-0.138890680568273,
25.6348575162694));
#48290=CARTESIAN_POINT('Ctrl Pts',(23.3087719366402,0.292839517253094,25.6741627548728));
#48291=CARTESIAN_POINT('Ctrl Pts',(23.340599545335,0.652887294986739,25.9156197142705));
#48292=CARTESIAN_POINT('Ctrl Pts',(23.3724271540298,0.853118727617184,26.30012360096));
#48293=CARTESIAN_POINT('Ctrl Pts',(23.4042547627246,0.844520369817035,26.7335540264445));
#48294=CARTESIAN_POINT('Ctrl Pts',(23.4360823714194,0.62919696175823,27.1098141697423));
#48295=CARTESIAN_POINT('Ctrl Pts',(23.4679099801142,0.25985622245349,27.3368015786055));
#48296=CARTESIAN_POINT('Ctrl Pts',(23.4997375888091,-0.173093155040001,
27.3589533735789));
#48297=CARTESIAN_POINT('Ctrl Pts',(23.5315651975039,-0.56367210257829,27.1708471503102));
#48298=CARTESIAN_POINT('Ctrl Pts',(23.5633928061987,-0.816273154142162,
26.818528297222));
#48299=CARTESIAN_POINT('Ctrl Pts',(23.5952204148935,-0.869063621088188,
26.3882388224586));
#48300=CARTESIAN_POINT('Ctrl Pts',(23.6270480235883,-0.709121243252345,
25.9853066926095));
#48301=CARTESIAN_POINT('Ctrl Pts',(23.6588756322832,-0.375597351115582,
25.7083632347223));
#48302=CARTESIAN_POINT('Ctrl Pts',(23.6907032409779,0.0498667523664727,
25.6251997683398));
#48303=CARTESIAN_POINT('Ctrl Pts',(23.7225308496728,0.463124274151249,25.7561733770587));
#48304=CARTESIAN_POINT('Ctrl Pts',(23.7543584583676,0.763016396744221,26.0692238207563));
#48305=CARTESIAN_POINT('Ctrl Pts',(23.7861860670624,0.876134335312124,26.487721368499));
#48306=CARTESIAN_POINT('Ctrl Pts',(23.8180136757572,0.774788631588053,26.909224528427));
#48307=CARTESIAN_POINT('Ctrl Pts',(23.8498412844521,0.483787089438719,27.2305560829921));
#48308=CARTESIAN_POINT('Ctrl Pts',(23.8816688931468,0.0743622221061536,
27.3730592180533));
#48309=CARTESIAN_POINT('Ctrl Pts',(23.9134965018417,-0.353265325293876,
27.3018514502384));
#48310=CARTESIAN_POINT('Ctrl Pts',(23.9453241105365,-0.694419183324126,
27.0343632997651));
#48311=CARTESIAN_POINT('Ctrl Pts',(23.9771517192313,-0.865590355674041,
26.6360715784741));
#48312=CARTESIAN_POINT('Ctrl Pts',(24.0089793279262,-0.824878882944739,
26.2044717157763));
#48313=CARTESIAN_POINT('Ctrl Pts',(24.0408069366209,-0.582250281122388,
25.8452124402241));
#48314=CARTESIAN_POINT('Ctrl Pts',(24.0726345453158,-0.197096142995666,
25.6462346641374));
#48315=CARTESIAN_POINT('Ctrl Pts',(24.1044621540105,0.236303971809375,25.6562449578157));
#48316=CARTESIAN_POINT('Ctrl Pts',(24.1362897627054,0.611860661879505,25.872792961815));
#48317=CARTESIAN_POINT('Ctrl Pts',(24.1681173714002,0.837643669041631,26.2428711956648));
#48318=CARTESIAN_POINT('Ctrl Pts',(24.1999449800951,0.858384932072728,26.675890439464));
#48319=CARTESIAN_POINT('Ctrl Pts',(24.2317725887899,0.669007322231117,27.0658545229169));
#48320=CARTESIAN_POINT('Ctrl Pts',(24.2636001974847,0.315867442994404,27.317306488877));
#48321=CARTESIAN_POINT('Ctrl Pts',(24.2954278061795,-0.114591723451727,
27.3686949264389));
#48322=CARTESIAN_POINT('Ctrl Pts',(24.3272554148743,-0.517000672713736,
27.2074407697595));
#48323=CARTESIAN_POINT('Ctrl Pts',(24.3590830235691,-0.792856143965913,
26.873016451755));
#48324=CARTESIAN_POINT('Ctrl Pts',(24.390910632264,-0.874633139355223,26.447283685201));
#48325=CARTESIAN_POINT('Ctrl Pts',(24.4227382409587,-0.742313961161101,
26.0344550275541));
#48326=CARTESIAN_POINT('Ctrl Pts',(24.4545658496536,-0.428288223346675,
25.7355843172417));
#48327=CARTESIAN_POINT('Ctrl Pts',(24.4863934583483,-0.00942439321280878,
25.6238303137423));
#48328=CARTESIAN_POINT('Ctrl Pts',(24.5182210670433,0.411746377322031,25.7265486058798));
#48329=CARTESIAN_POINT('Ctrl Pts',(24.550048675738,0.732128234305675,26.0185954021441));
#48330=CARTESIAN_POINT('Ctrl Pts',(24.5818762844329,0.873296834342774,26.4284823278396));
#48331=CARTESIAN_POINT('Ctrl Pts',(24.6137038931277,0.800696366844726,26.8558756333693));
#48332=CARTESIAN_POINT('Ctrl Pts',(24.6455315018225,0.532098262588963,27.1961562879513));
#48333=CARTESIAN_POINT('Ctrl Pts',(24.6773591105173,0.133251032311443,27.3660290414832));
#48334=CARTESIAN_POINT('Ctrl Pts',(24.7091867192121,-0.298213914881034,
27.3239117666811));
#48335=CARTESIAN_POINT('Ctrl Pts',(24.741014327907,-0.656680875589221,27.0801140973462));
#48336=CARTESIAN_POINT('Ctrl Pts',(24.7728419366017,-0.854402883467569,
26.6943137952556));
#48337=CARTESIAN_POINT('Ctrl Pts',(24.8046695452966,-0.842980760146056,
26.2609485906171));
#48338=CARTESIAN_POINT('Ctrl Pts',(24.8364971539914,-0.625210458335947,
25.8860993393946));
#48339=CARTESIAN_POINT('Ctrl Pts',(24.8683247626862,-0.254398657420573,
25.6615231300704));
#48340=CARTESIAN_POINT('Ctrl Pts',(24.900152371381,0.178685857239278,25.6421926190997));
#48341=CARTESIAN_POINT('Ctrl Pts',(24.9319799800758,0.568030938087369,25.8328396057319));
#48342=CARTESIAN_POINT('Ctrl Pts',(24.9638075887707,0.818331149893379,26.1867967633971));
#48343=CARTESIAN_POINT('Ctrl Pts',(24.9956351974655,0.868317012707937,26.6174210532499));
#48344=CARTESIAN_POINT('Ctrl Pts',(25.0274628061603,0.705752788505203,27.0193025513335));
#48345=CARTESIAN_POINT('Ctrl Pts',(25.0592904148551,0.370431593732857,27.2940671084165));
#48346=CARTESIAN_POINT('Ctrl Pts',(25.0911180235499,-0.0555653177760932,
27.3744567649488));
#48347=CARTESIAN_POINT('Ctrl Pts',(25.1229456322447,-0.467960730114108,
27.2407934215255));
#48348=CARTESIAN_POINT('Ctrl Pts',(25.1547732409396,-0.765806856361044,
26.9257957222128));
#48349=CARTESIAN_POINT('Ctrl Pts',(25.1866008496344,-0.876195738795198,
26.5065700549077));
#48350=CARTESIAN_POINT('Ctrl Pts',(25.2184284583292,-0.772105948348922,
26.0857361434682));
#48351=CARTESIAN_POINT('Ctrl Pts',(25.250256067024,-0.479016997335324,25.7663073841395));
#48352=CARTESIAN_POINT('Ctrl Pts',(25.2820836757188,-0.0686723632286731,
25.6264748172875));
#48353=CARTESIAN_POINT('Ctrl Pts',(25.3139112844136,0.358482164691299,25.7004672139914));
#48354=CARTESIAN_POINT('Ctrl Pts',(25.3457388931085,0.697886004574409,25.9701724215148));
#48355=CARTESIAN_POINT('Ctrl Pts',(25.3775665018033,0.866458536502466,26.3695709279865));
#48356=CARTESIAN_POINT('Ctrl Pts',(25.4093941104981,0.822935906600167,26.8008963807238));
#48357=CARTESIAN_POINT('Ctrl Pts',(25.4412217191929,0.577971757070994,27.1585672223336));
#48358=CARTESIAN_POINT('Ctrl Pts',(25.4730493278877,0.191529385348056,27.3550313636665));
#48359=CARTESIAN_POINT('Ctrl Pts',(25.5048769365825,-0.241796310008061,
27.3421975319184));
#48360=CARTESIAN_POINT('Ctrl Pts',(25.5367045452774,-0.615934144269444,
27.1232072434019));
#48361=CARTESIAN_POINT('Ctrl Pts',(25.5685321539722,-0.839301172428612,
26.7516658106803));
#48362=CARTESIAN_POINT('Ctrl Pts',(25.600359762667,-0.857220726187857,26.3185206213073));
#48363=CARTESIAN_POINT('Ctrl Pts',(25.6321873713618,-0.665306386027568,
25.9297986749954));
#48364=CARTESIAN_POINT('Ctrl Pts',(25.6640149800566,-0.310535706310569,
25.6806528737063));
#48365=CARTESIAN_POINT('Ctrl Pts',(25.6958425887515,0.120249136888709,25.6320701160504));
#48366=CARTESIAN_POINT('Ctrl Pts',(25.7276701974463,0.521598918860212,25.7959426826794));
#48367=CARTESIAN_POINT('Ctrl Pts',(25.7594978061411,0.795269645703851,26.1321571953627));
#48368=CARTESIAN_POINT('Ctrl Pts',(25.7913254148359,0.874271110452719,26.5584137313573));
#48369=CARTESIAN_POINT('Ctrl Pts',(25.8231530235307,0.739265019907162,26.9703715209621));
#48370=CARTESIAN_POINT('Ctrl Pts',(25.8549806322256,0.423298702792696,27.2671899038389));
#48371=CARTESIAN_POINT('Ctrl Pts',(25.8868082409203,0.00371564593592677,
27.3762124906646));
#48372=CARTESIAN_POINT('Ctrl Pts',(25.9186358496152,-0.416776937561546,
27.2707523122981));
#48373=CARTESIAN_POINT('Ctrl Pts',(25.95046345831,-0.735249214411046,26.9766243061436));
#48374=CARTESIAN_POINT('Ctrl Pts',(25.9822910670048,-0.873744254401199,
26.5658263388602));
#48375=CARTESIAN_POINT('Ctrl Pts',(26.0141186756997,-0.798360732045715,
26.1389150831885));
#48376=CARTESIAN_POINT('Ctrl Pts',(26.0459462843944,-0.527551248954989,
25.8003917327718));
#48377=CARTESIAN_POINT('Ctrl Pts',(26.0777738930893,-0.127605770195691,
25.6331210739316));
#48378=CARTESIAN_POINT('Ctrl Pts',(26.1096015017841,0.303575733848321,25.6780488566812));
#48379=CARTESIAN_POINT('Ctrl Pts',(26.1414291104789,0.6604464278685,25.9241763964648));
#48380=CARTESIAN_POINT('Ctrl Pts',(26.1732567191737,0.855651057026928,26.3112576623533));
#48381=CARTESIAN_POINT('Ctrl Pts',(26.2050843278685,0.841404823443538,26.7445375018455));
#48382=CARTESIAN_POINT('Ctrl Pts',(26.2369119365634,0.621198438810439,27.117963249074));
#48383=CARTESIAN_POINT('Ctrl Pts',(26.2687395452581,0.248928358756431,27.3401124925143));
#48384=CARTESIAN_POINT('Ctrl Pts',(26.300567153953,-0.184267317446832,27.3566326768286));
#48385=CARTESIAN_POINT('Ctrl Pts',(26.3323947626478,-0.572372600161979,
27.1634307098942));
#48386=CARTESIAN_POINT('Ctrl Pts',(26.3642223713426,-0.820341019289417,
26.8078929774887));
#48387=CARTESIAN_POINT('Ctrl Pts',(26.3960499800375,-0.867561115381817,
26.3768668161923));
#48388=CARTESIAN_POINT('Ctrl Pts',(26.417268385834,-0.757378500801713,26.1097887611524));
#48389=CARTESIAN_POINT('Ctrl Pts',(26.4278775887323,-0.673641898681181,
25.9975270329735));
#48390=CARTESIAN_POINT('Ctrl Pts',(9.57962256921138,-0.830248497164267,
26.8880319004024));
#48391=CARTESIAN_POINT('Ctrl Pts',(9.59023177210965,-0.894913613471617,
26.7496718439806));
#48392=CARTESIAN_POINT('Ctrl Pts',(9.6114501779062,-0.953673908640778,26.4401420407412));
#48393=CARTESIAN_POINT('Ctrl Pts',(9.643277786601,-0.80817341482536,25.9902417865545));
#48394=CARTESIAN_POINT('Ctrl Pts',(9.67510539529583,-0.464933699438219,
25.6652387735807));
#48395=CARTESIAN_POINT('Ctrl Pts',(9.70693300399065,-0.00784090380745088,
25.5445127616791));
#48396=CARTESIAN_POINT('Ctrl Pts',(9.73876061268547,0.45114778502721,25.6577057284115));
#48397=CARTESIAN_POINT('Ctrl Pts',(9.77058822138028,0.799715104863132,25.9770624440697));
#48398=CARTESIAN_POINT('Ctrl Pts',(9.8024158300751,0.952518433985614,26.4244345660751));
#48399=CARTESIAN_POINT('Ctrl Pts',(9.83424343876991,0.87216398679464,26.8902993016558));
#48400=CARTESIAN_POINT('Ctrl Pts',(9.86607104746474,0.578315937843598,27.2606274566905));
#48401=CARTESIAN_POINT('Ctrl Pts',(9.89789865615955,0.142906389714678,27.4447649136056));
#48402=CARTESIAN_POINT('Ctrl Pts',(9.92972626485437,-0.327484867340805,
27.3976397450008));
#48403=CARTESIAN_POINT('Ctrl Pts',(9.96155387354919,-0.717712805021489,
27.1307863931583));
#48404=CARTESIAN_POINT('Ctrl Pts',(9.993381482244,-0.932256296314281,26.7095268341116));
#48405=CARTESIAN_POINT('Ctrl Pts',(10.0252090909388,-0.918598312263225,
26.2369783630933));
#48406=CARTESIAN_POINT('Ctrl Pts',(10.0570366996336,-0.680082225526843,
25.8288134266618));
#48407=CARTESIAN_POINT('Ctrl Pts',(10.0888643083285,-0.275092889112725,
25.5849441769394));
#48408=CARTESIAN_POINT('Ctrl Pts',(10.1206919170233,0.197234765899907,25.5650659409174));
#48409=CARTESIAN_POINT('Ctrl Pts',(10.1525195257181,0.621282517590593,25.7740445691304));
#48410=CARTESIAN_POINT('Ctrl Pts',(10.1843471344129,0.893250263923072,26.1607254551713));
#48411=CARTESIAN_POINT('Ctrl Pts',(10.2161747431077,0.946564664668695,26.630455309537));
#48412=CARTESIAN_POINT('Ctrl Pts',(10.2480023518025,0.768175206483761,27.0682517962964));
#48413=CARTESIAN_POINT('Ctrl Pts',(10.2798299604974,0.401748770810461,27.366949350837));
#48414=CARTESIAN_POINT('Ctrl Pts',(10.3116575691922,-0.0630193248360654,
27.453431600397));
#48415=CARTESIAN_POINT('Ctrl Pts',(10.343485177887,-0.512361299725991,27.3065290759445));
#48416=CARTESIAN_POINT('Ctrl Pts',(10.3753127865818,-0.836285440822322,
26.9622011611285));
#48417=CARTESIAN_POINT('Ctrl Pts',(10.4071403952766,-0.95550031024828,26.5047338103433));
#48418=CARTESIAN_POINT('Ctrl Pts',(10.4389680039715,-0.840824018843678,
26.0461076986875));
#48419=CARTESIAN_POINT('Ctrl Pts',(10.4707956126662,-0.520327484641828,
25.6985871472319));
#48420=CARTESIAN_POINT('Ctrl Pts',(10.5026232213611,-0.0724631221990005,
25.5472396168115));
#48421=CARTESIAN_POINT('Ctrl Pts',(10.5344508300559,0.393139051096402,25.6291125570096));
#48422=CARTESIAN_POINT('Ctrl Pts',(10.5662784387507,0.762507086054255,25.9241647843606));
#48423=CARTESIAN_POINT('Ctrl Pts',(10.5981060474455,0.94522560808136,26.3601722428075));
#48424=CARTESIAN_POINT('Ctrl Pts',(10.6299336561403,0.896568051661617,26.8304072950067));
#48425=CARTESIAN_POINT('Ctrl Pts',(10.6617612648352,0.628445006706643,27.2197639372736));
#48426=CARTESIAN_POINT('Ctrl Pts',(10.69358887353,0.206488697049629,27.432933904328));
#48427=CARTESIAN_POINT('Ctrl Pts',(10.7254164822248,-0.266012735970864,
27.4177366049992));
#48428=CARTESIAN_POINT('Ctrl Pts',(10.7572440909196,-0.673398514972374,
27.1778920945748));
#48429=CARTESIAN_POINT('Ctrl Pts',(10.7890716996145,-0.915947130979303,
26.772110464894));
#48430=CARTESIAN_POINT('Ctrl Pts',(10.8208993083092,-0.934286570448576,
26.2997205548902));
#48431=CARTESIAN_POINT('Ctrl Pts',(10.8527269170041,-0.723927632549161,
25.8763558428994));
#48432=CARTESIAN_POINT('Ctrl Pts',(10.8845545256989,-0.336362813571031,
25.6056492245765));
#48433=CARTESIAN_POINT('Ctrl Pts',(10.9163821343937,0.133538230826593,25.5538653411054));
#48434=CARTESIAN_POINT('Ctrl Pts',(10.9482097430885,0.570751256716081,25.7336800571491));
#48435=CARTESIAN_POINT('Ctrl Pts',(10.9800373517833,0.868253523165414,26.1010776123544));
#48436=CARTESIAN_POINT('Ctrl Pts',(11.0118649604781,0.953221243819833,26.5661249739856));
#48437=CARTESIAN_POINT('Ctrl Pts',(11.043692569173,0.804855682555953,27.0149860018597));
#48438=CARTESIAN_POINT('Ctrl Pts',(11.0755201778678,0.459474350715236,27.3377867108572));
#48439=CARTESIAN_POINT('Ctrl Pts',(11.1073477865626,0.00162106243758639,
27.4555106613799));
#48440=CARTESIAN_POINT('Ctrl Pts',(11.1391753952574,-0.456629035941818,
27.3393409172612));
#48441=CARTESIAN_POINT('Ctrl Pts',(11.1710030039522,-0.803103665335106,
27.0177139698514));
#48442=CARTESIAN_POINT('Ctrl Pts',(11.2028306126471,-0.952991389885271,
26.5693589407255));
#48443=CARTESIAN_POINT('Ctrl Pts',(11.2346582213419,-0.869602097076131,
26.1040259546197));
#48444=CARTESIAN_POINT('Ctrl Pts',(11.2664858300367,-0.573348149194159,
25.7356210680104));
#48445=CARTESIAN_POINT('Ctrl Pts',(11.2983134387315,-0.136747764217315,
25.5543238922149));
#48446=CARTESIAN_POINT('Ctrl Pts',(11.3301410474263,0.333326281598174,25.6045130699726));
#48447=CARTESIAN_POINT('Ctrl Pts',(11.3619686561212,0.721807396350512,25.8739030950183));
#48448=CARTESIAN_POINT('Ctrl Pts',(11.393796264816,0.933601629861665,26.2965516070998));
#48449=CARTESIAN_POINT('Ctrl Pts',(11.4256238735108,0.916865148481333,26.7690010248202));
#48450=CARTESIAN_POINT('Ctrl Pts',(11.4574514822056,0.675694774593156,27.1756033033086));
#48451=CARTESIAN_POINT('Ctrl Pts',(11.4892790909004,0.269125150160512,27.4168287219569));
#48452=CARTESIAN_POINT('Ctrl Pts',(11.5211066995952,-0.203321997397894,
27.4336291647267));
#48453=CARTESIAN_POINT('Ctrl Pts',(11.5529343082901,-0.625999178910517,
27.2218921525113));
#48454=CARTESIAN_POINT('Ctrl Pts',(11.5847619169849,-0.895441795163115,
26.8334475121051));
#48455=CARTESIAN_POINT('Ctrl Pts',(11.6165895256797,-0.945694612419042,
26.3633802653508));
#48456=CARTESIAN_POINT('Ctrl Pts',(11.6484171343745,-0.764456546484064,
25.926755339849));
#48457=CARTESIAN_POINT('Ctrl Pts',(11.6802447430693,-0.396091770950939,
25.630451518983));
#48458=CARTESIAN_POINT('Ctrl Pts',(11.7120723517642,0.0692299214113307,
25.546999228838));
#48459=CARTESIAN_POINT('Ctrl Pts',(11.743899960459,0.517605238653885,25.6968262524384));
#48460=CARTESIAN_POINT('Ctrl Pts',(11.7757275691538,0.839279089834648,26.0432573358878));
#48461=CARTESIAN_POINT('Ctrl Pts',(11.8075551778486,0.955510872087357,26.501491702678));
#48462=CARTESIAN_POINT('Ctrl Pts',(11.8393827865434,0.837848908120856,26.9593609245623));
#48463=CARTESIAN_POINT('Ctrl Pts',(11.8712103952382,0.515094960786372,27.3047859549138));
#48464=CARTESIAN_POINT('Ctrl Pts',(11.903038003933,0.0662540231764387,27.4532122828976));
#48465=CARTESIAN_POINT('Ctrl Pts',(11.9348656126279,-0.398804837364059,
27.3683075224534));
#48466=CARTESIAN_POINT('Ctrl Pts',(11.9666932213227,-0.766242665903474,
27.0708549980539));
#48467=CARTESIAN_POINT('Ctrl Pts',(11.9985208300175,-0.946116571439429,
26.6336663199977));
#48468=CARTESIAN_POINT('Ctrl Pts',(12.0303484387123,-0.894396304979596,
26.1637582692573));
#48469=CARTESIAN_POINT('Ctrl Pts',(12.0621760474071,-0.623742158762532,
25.7761568048007));
#48470=CARTESIAN_POINT('Ctrl Pts',(12.094003656102,-0.200405929641351,25.5657405525131));
#48471=CARTESIAN_POINT('Ctrl Pts',(12.1258312647968,0.271986458878584,25.5840160383278));
#48472=CARTESIAN_POINT('Ctrl Pts',(12.1576588734916,0.677800921760648,25.8265097162434));
#48473=CARTESIAN_POINT('Ctrl Pts',(12.1894864821864,0.917700583029717,26.2338630206812));
#48474=CARTESIAN_POINT('Ctrl Pts',(12.2213140908812,0.932961850804134,26.7063623919181));
#48475=CARTESIAN_POINT('Ctrl Pts',(12.253141699576,0.719849011345744,27.1283475572632));
#48476=CARTESIAN_POINT('Ctrl Pts',(12.2849693082708,0.330528671905649,27.3965233119681));
#48477=CARTESIAN_POINT('Ctrl Pts',(12.3167969169657,-0.139699788585952,
27.4452445296975));
#48478=CARTESIAN_POINT('Ctrl Pts',(12.3486245256605,-0.575731979989561,
27.2625850372721));
#48479=CARTESIAN_POINT('Ctrl Pts',(12.3804521343553,-0.870834210728471,
26.8932569507065));
#48480=CARTESIAN_POINT('Ctrl Pts',(12.4122797430501,-0.952770184721209,
26.42766586587));
#48481=CARTESIAN_POINT('Ctrl Pts',(12.444107351745,-0.801483288833254,25.9797810176714));
#48482=CARTESIAN_POINT('Ctrl Pts',(12.4759349604397,-0.454006130297858,
25.659237438092));
#48483=CARTESIAN_POINT('Ctrl Pts',(12.5077625691346,0.00460445196288184,
25.5444990576268));
#48484=CARTESIAN_POINT('Ctrl Pts',(12.5395901778294,0.4620879381849,25.6636519927458));
#48485=CARTESIAN_POINT('Ctrl Pts',(12.5714177865242,0.806459703648916,25.9875295147577));
#48486=CARTESIAN_POINT('Ctrl Pts',(12.603245395219,0.95342305988236,26.4368515974978));
#48487=CARTESIAN_POINT('Ctrl Pts',(12.6350730039139,0.867003732860179,26.9016313970055));
#48488=CARTESIAN_POINT('Ctrl Pts',(12.6669006126086,0.568355788677721,27.2680982680169));
#48489=CARTESIAN_POINT('Ctrl Pts',(12.6987282213035,0.130583457235488,27.4465469943698));
#48490=CARTESIAN_POINT('Ctrl Pts',(12.7305558299983,-0.33915361149994,27.3932961880925));
#48491=CARTESIAN_POINT('Ctrl Pts',(12.7623834386931,-0.725871312214778,
27.1213807930388));
#48492=CARTESIAN_POINT('Ctrl Pts',(12.7942110473879,-0.934907350222748,
26.6973613395615));
#48493=CARTESIAN_POINT('Ctrl Pts',(12.8260386560827,-0.915093053923393,
26.2250309935371));
#48494=CARTESIAN_POINT('Ctrl Pts',(12.8578662647776,-0.671278645460207,
25.8200086529939));
#48495=CARTESIAN_POINT('Ctrl Pts',(12.8896938734724,-0.263145984081015,
25.5814372950549));
#48496=CARTESIAN_POINT('Ctrl Pts',(12.9215214821672,0.209400596403874,25.567715364237));
#48497=CARTESIAN_POINT('Ctrl Pts',(12.953349090862,0.630689267236257,25.7822017692645));
#48498=CARTESIAN_POINT('Ctrl Pts',(12.9851766995568,0.897595314360882,26.1723936760509));
#48499=CARTESIAN_POINT('Ctrl Pts',(13.0170043082516,0.944784415506595,26.6427783599496));
#48500=CARTESIAN_POINT('Ctrl Pts',(13.0488319169465,0.760705435076608,27.0782131898348));
#48501=CARTESIAN_POINT('Ctrl Pts',(13.0806595256413,0.39041795699687,27.3721106986549));
#48502=CARTESIAN_POINT('Ctrl Pts',(13.1124871343361,-0.075437579197961,
27.4525294869445));
#48503=CARTESIAN_POINT('Ctrl Pts',(13.1443147430309,-0.522827205145454,
27.2997843243111));
#48504=CARTESIAN_POINT('Ctrl Pts',(13.1761423517257,-0.842237111333554,
26.9512647783138));
#48505=CARTESIAN_POINT('Ctrl Pts',(13.2079699604206,-0.955480872342886,
26.4922828476173));
#48506=CARTESIAN_POINT('Ctrl Pts',(13.2397975691154,-0.83483823058961,26.035189952131));
#48507=CARTESIAN_POINT('Ctrl Pts',(13.2716251778102,-0.509840571071793,
25.6918751062223));
#48508=CARTESIAN_POINT('Ctrl Pts',(13.303452786505,-0.0600421116614344,
25.5463762813975));
#48509=CARTESIAN_POINT('Ctrl Pts',(13.3352803951998,0.404453694307345,25.6343092578668));
#48510=CARTESIAN_POINT('Ctrl Pts',(13.3671080038946,0.769945718637211,25.9341494524114));
#48511=CARTESIAN_POINT('Ctrl Pts',(13.3989356125895,0.946967372008249,26.3725007913522));
#48512=CARTESIAN_POINT('Ctrl Pts',(13.4307632212843,0.892186591041172,26.8420618929672));
#48513=CARTESIAN_POINT('Ctrl Pts',(13.4625908299791,0.619012832870912,27.2278917258736));
#48514=CARTESIAN_POINT('Ctrl Pts',(13.4944184386739,0.194314654971488,27.4355453311932));
#48515=CARTESIAN_POINT('Ctrl Pts',(13.5262460473687,-0.277948635920619,
27.4141924346897));
#48516=CARTESIAN_POINT('Ctrl Pts',(13.5580736560635,-0.682174555798859,
27.1690598831754));
#48517=CARTESIAN_POINT('Ctrl Pts',(13.5899012647584,-0.91941507855371,26.7601521961893));
#48518=CARTESIAN_POINT('Ctrl Pts',(13.6217288734532,-0.931597526790183,
26.2875634213878));
#48519=CARTESIAN_POINT('Ctrl Pts',(13.653556482148,-0.7157398324446,25.8669757160217));
#48520=CARTESIAN_POINT('Ctrl Pts',(13.6853840908428,-0.32468049924893,25.6013422090353));
#48521=CARTESIAN_POINT('Ctrl Pts',(13.7172116995376,0.145855416068471,25.5556857252707));
#48522=CARTESIAN_POINT('Ctrl Pts',(13.7490393082324,0.580688263354752,25.7411822401551));
#48523=CARTESIAN_POINT('Ctrl Pts',(13.7808669169273,0.873377931249599,26.1124251800488));
#48524=CARTESIAN_POINT('Ctrl Pts',(13.8126945256221,0.952278680386351,26.5785402236797));
#48525=CARTESIAN_POINT('Ctrl Pts',(13.8445221343169,0.798076872025581,27.0254298794244));
#48526=CARTESIAN_POINT('Ctrl Pts',(13.8763497430117,0.448518637252629,27.3437027224627));
#48527=CARTESIAN_POINT('Ctrl Pts',(13.9081773517065,-0.0108297709036782,
27.4554506622093));
#48528=CARTESIAN_POINT('Ctrl Pts',(13.9400049604013,-0.467527224726181,
27.3333195941497));
#48529=CARTESIAN_POINT('Ctrl Pts',(13.9718325690962,-0.809781507628197,
27.0072052461849));
#48530=CARTESIAN_POINT('Ctrl Pts',(14.003660177791,-0.95381425692857,26.5569351836198));
#48531=CARTESIAN_POINT('Ctrl Pts',(14.0354877864858,-0.86436856420665,26.0927283006821));
#48532=CARTESIAN_POINT('Ctrl Pts',(14.0673153951806,-0.563339301373415,
25.7282150018417));
#48533=CARTESIAN_POINT('Ctrl Pts',(14.0991430038754,-0.12441360696645,25.5526223001065));
#48534=CARTESIAN_POINT('Ctrl Pts',(14.1309706125703,0.344966544280397,25.6089324743987));
#48535=CARTESIAN_POINT('Ctrl Pts',(14.1627982212651,0.729904414733746,25.8833616966112));
#48536=CARTESIAN_POINT('Ctrl Pts',(14.1946258299599,0.936173383627583,26.3087340917955));
#48537=CARTESIAN_POINT('Ctrl Pts',(14.2264534386547,0.913282113529031,26.7809253156302));
#48538=CARTESIAN_POINT('Ctrl Pts',(14.2582810473495,0.666834020448794,27.1843505249696));
#48539=CARTESIAN_POINT('Ctrl Pts',(14.2901086560443,0.257155647415318,27.4202576948097));
#48540=CARTESIAN_POINT('Ctrl Pts',(14.3219362647392,-0.21547030632334,27.4309005311777));
#48541=CARTESIAN_POINT('Ctrl Pts',(14.353763873434,-0.635352582708677,27.2136738383179));
#48542=CARTESIAN_POINT('Ctrl Pts',(14.3855914821288,-0.899710730503885,
26.8217512288558));
#48543=CARTESIAN_POINT('Ctrl Pts',(14.4174190908236,-0.943834112355007,
26.3510690757127));
#48544=CARTESIAN_POINT('Ctrl Pts',(14.4492466995184,-0.756922031610138,
25.9168428257175));
#48545=CARTESIAN_POINT('Ctrl Pts',(14.4810743082132,-0.384727569742386,
25.6253641049361));
#48546=CARTESIAN_POINT('Ctrl Pts',(14.5129019169081,0.0816420346481125,
25.5479822322916));
#48547=CARTESIAN_POINT('Ctrl Pts',(14.5447295256029,0.528026977544294,25.7036390499029));
#48548=CARTESIAN_POINT('Ctrl Pts',(14.5765571342977,0.845159379741648,26.0542322637418));
#48549=CARTESIAN_POINT('Ctrl Pts',(14.6083847429925,0.955410312293092,26.513942274493));
#48550=CARTESIAN_POINT('Ctrl Pts',(14.6402123516873,0.831792114051153,26.9702394399201));
#48551=CARTESIAN_POINT('Ctrl Pts',(14.6720399603822,0.504564538549048,27.3114295276195));
#48552=CARTESIAN_POINT('Ctrl Pts',(14.703867569077,0.0538276513498363,27.4539946728385));
#48553=CARTESIAN_POINT('Ctrl Pts',(14.7356951777718,-0.410085382131093,
27.3630372131122));
#48554=CARTESIAN_POINT('Ctrl Pts',(14.7675227864666,-0.773616087060543,
27.0608220766831));
#48555=CARTESIAN_POINT('Ctrl Pts',(14.7993503951614,-0.947777973671093,
26.6213266849376));
#48556=CARTESIAN_POINT('Ctrl Pts',(14.8311780038562,-0.889939003649095,
26.1521324653865));
#48557=CARTESIAN_POINT('Ctrl Pts',(14.8630056125511,-0.614257229792361,
25.7680906425644));
#48558=CARTESIAN_POINT('Ctrl Pts',(14.8948332212458,-0.188215131615601,
25.5632084991393));
#48559=CARTESIAN_POINT('Ctrl Pts',(14.9266608299407,0.283899014001654,25.5876378998978));
#48560=CARTESIAN_POINT('Ctrl Pts',(14.9584884386355,0.686519231425576,25.8353989190974));
#48561=CARTESIAN_POINT('Ctrl Pts',(14.9903160473303,0.921090544770697,26.2458436304397));
#48562=CARTESIAN_POINT('Ctrl Pts',(15.0221436560251,0.930193656322486,26.7185017473418));
#48563=CARTESIAN_POINT('Ctrl Pts',(15.05397126472,0.711600270280961,27.1376741387183));
#48564=CARTESIAN_POINT('Ctrl Pts',(15.0857988734148,0.318818543856639,27.4007541218042));
#48565=CARTESIAN_POINT('Ctrl Pts',(15.1176264821096,-0.15200485196688,27.4433439334795));
#48566=CARTESIAN_POINT('Ctrl Pts',(15.1494540908044,-0.585619896416687,
27.2550182704908));
#48567=CARTESIAN_POINT('Ctrl Pts',(15.1812816994992,-0.875884576747471,
26.8818762365871));
#48568=CARTESIAN_POINT('Ctrl Pts',(15.213109308194,-0.951746751679696,26.4152570208149));
#48569=CARTESIAN_POINT('Ctrl Pts',(15.2449369168889,-0.794636576735844,
25.9693815280566));
#48570=CARTESIAN_POINT('Ctrl Pts',(15.2767645255837,-0.443012104524464,
25.6533929322887));
#48571=CARTESIAN_POINT('Ctrl Pts',(15.3085921342785,0.0170546301190841,
25.5446401769775));
#48572=CARTESIAN_POINT('Ctrl Pts',(15.3404197429733,0.472946664667159,25.6697441934957));
#48573=CARTESIAN_POINT('Ctrl Pts',(15.3722473516681,0.813068936261896,25.9980815238109));
#48574=CARTESIAN_POINT('Ctrl Pts',(15.404074960363,0.95416496441753,26.4492804521697));
#48575=CARTESIAN_POINT('Ctrl Pts',(15.4359025690577,0.861696702978835,26.9128947128862));
#48576=CARTESIAN_POINT('Ctrl Pts',(15.4677301777526,0.558298900231862,27.2754389659116));
#48577=CARTESIAN_POINT('Ctrl Pts',(15.4995577864474,0.118238475321277,27.4481681890929));
#48578=CARTESIAN_POINT('Ctrl Pts',(15.5313853951422,-0.35076483317966,27.388801037161));
#48579=CARTESIAN_POINT('Ctrl Pts',(15.563213003837,-0.733906532701598,27.1118696373509));
#48580=CARTESIAN_POINT('Ctrl Pts',(15.5950406125319,-0.937399676332867,
26.6851623575813));
#48581=CARTESIAN_POINT('Ctrl Pts',(15.6268682212267,-0.911432404172941,
26.2131303005238));
#48582=CARTESIAN_POINT('Ctrl Pts',(15.6586958299215,-0.662361088233901,
25.8113193478487));
#48583=CARTESIAN_POINT('Ctrl Pts',(15.6905234386163,-0.251154394454069,
25.5780863804019));
#48584=CARTESIAN_POINT('Ctrl Pts',(15.7223510473111,0.22153086949624,25.5705230902737));
#48585=CARTESIAN_POINT('Ctrl Pts',(15.7541786560059,0.639988927369355,25.7904808496604));
#48586=CARTESIAN_POINT('Ctrl Pts',(15.7860062647008,0.901787953792385,26.1841175246251));
#48587=CARTESIAN_POINT('Ctrl Pts',(15.8178338733956,0.94284374330479,26.6550771664851));
#48588=CARTESIAN_POINT('Ctrl Pts',(15.8496614820904,0.753106496690714,27.0880764036214));
#48589=CARTESIAN_POINT('Ctrl Pts',(15.8814890907852,0.379020850745279,27.3771239630487));
#48590=CARTESIAN_POINT('Ctrl Pts',(15.91331669948,-0.0878430243817305,27.4514656351763));
#48591=CARTESIAN_POINT('Ctrl Pts',(15.9451443081748,-0.5332043351193,27.292903770242));
#48592=CARTESIAN_POINT('Ctrl Pts',(15.9769719168697,-0.848045771008207,
26.9402517712959));
#48593=CARTESIAN_POINT('Ctrl Pts',(16.0087995255645,-0.955299194933258,
26.4798331952482));
#48594=CARTESIAN_POINT('Ctrl Pts',(16.0406271342593,-0.828710687813575,
26.0243511297632));
#48595=CARTESIAN_POINT('Ctrl Pts',(16.0724547429541,-0.499267087186487,
25.685300283843));
#48596=CARTESIAN_POINT('Ctrl Pts',(16.1042823516489,-0.0476109060464227,
25.5456748701415));
#48597=CARTESIAN_POINT('Ctrl Pts',(16.1361099603437,0.415699661769282,25.6396529519671));
#48598=CARTESIAN_POINT('Ctrl Pts',(16.1679375690386,0.777253615365754,25.944230201203));
#48599=CARTESIAN_POINT('Ctrl Pts',(16.1997651777333,0.948548342017812,26.3848509891085));
#48600=CARTESIAN_POINT('Ctrl Pts',(16.2315927864282,0.887653638213781,26.8536584092311));
#48601=CARTESIAN_POINT('Ctrl Pts',(16.263420395123,0.609475551402932,27.2358959193365));
#48602=CARTESIAN_POINT('Ctrl Pts',(16.2952480038179,0.182107618499345,27.4379979035896));
#48603=CARTESIAN_POINT('Ctrl Pts',(16.3270756125126,-0.289837340527268,
27.4104930356077));
#48604=CARTESIAN_POINT('Ctrl Pts',(16.3589032212075,-0.690834764208691,
27.1601140662149));
#48605=CARTESIAN_POINT('Ctrl Pts',(16.3907308299023,-0.922726910556888,
26.7481497539554));
#48606=CARTESIAN_POINT('Ctrl Pts',(16.4225584385971,-0.928750298995543,
26.2754423593602));
#48607=CARTESIAN_POINT('Ctrl Pts',(16.4543860472919,-0.707430500579885,
25.8577030759039));
#48608=CARTESIAN_POINT('Ctrl Pts',(16.4862136559868,-0.312943054569711,
25.597187784503));
#48609=CARTESIAN_POINT('Ctrl Pts',(16.5180412646815,0.158147835236672,25.5576664528608));
#48610=CARTESIAN_POINT('Ctrl Pts',(16.5498688733764,0.59052666982678,25.7488132695013));
#48611=CARTESIAN_POINT('Ctrl Pts',(16.5816964820712,0.87835404081465,26.1238385574802));
#48612=CARTESIAN_POINT('Ctrl Pts',(16.613524090766,0.951174421181637,26.5909421373384));
#48613=CARTESIAN_POINT('Ctrl Pts',(16.6453516994608,0.79116254900519,27.0357845396294));
#48614=CARTESIAN_POINT('Ctrl Pts',(16.6771793081556,0.437486765866275,27.3494754743637));
#48615=CARTESIAN_POINT('Ctrl Pts',(16.7090069168505,-0.0232787653625354,
27.4552284286692));
#48616=CARTESIAN_POINT('Ctrl Pts',(16.7408345255453,-0.478346027952504,
27.3271567743758));
#48617=CARTESIAN_POINT('Ctrl Pts',(16.7726621342401,-0.816321849996796,
26.9966103996805));
#48618=CARTESIAN_POINT('Ctrl Pts',(16.8044897429349,-0.954475167464214,
26.5445017589863));
#48619=CARTESIAN_POINT('Ctrl Pts',(16.8363173516297,-0.858988262592818,
26.081499800992));
#48620=CARTESIAN_POINT('Ctrl Pts',(16.8681449603245,-0.553234799228007,
25.7209399838263));
#48621=CARTESIAN_POINT('Ctrl Pts',(16.8999725690194,-0.112058324417954,
25.5510815716047));
#48622=CARTESIAN_POINT('Ctrl Pts',(16.9318001777142,0.356548232026913,25.6135031809852));
#48623=CARTESIAN_POINT('Ctrl Pts',(16.963627786409,0.737877496289409,25.8929250027018));
#48624=CARTESIAN_POINT('Ctrl Pts',(16.9954553951038,0.938586176166046,26.3209490531028));
#48625=CARTESIAN_POINT('Ctrl Pts',(17.0272830037986,0.909544004595047,26.7928019058661));
#48626=CARTESIAN_POINT('Ctrl Pts',(17.0591106124935,0.657860038277722,27.1929815443489));
#48627=CARTESIAN_POINT('Ctrl Pts',(17.0909382211882,0.245142480733944,27.4235304097486));
#48628=CARTESIAN_POINT('Ctrl Pts',(17.1227658298831,-0.227582030128332,
27.4280138304583));
#48629=CARTESIAN_POINT('Ctrl Pts',(17.1545934385779,-0.644598101614693,
27.2053343457797));
#48630=CARTESIAN_POINT('Ctrl Pts',(17.1864210472727,-0.903826901316126,
26.810000307704));
#48631=CARTESIAN_POINT('Ctrl Pts',(17.2182486559675,-0.941813340449867,
26.3387831836783));
#48632=CARTESIAN_POINT('Ctrl Pts',(17.2500762646624,-0.749259011071048,
25.9070293133871));
#48633=CARTESIAN_POINT('Ctrl Pts',(17.2819038733572,-0.37329800679106,25.6204252362105));
#48634=CARTESIAN_POINT('Ctrl Pts',(17.313731482052,0.0940402181997153,25.5491268245229));
#48635=CARTESIAN_POINT('Ctrl Pts',(17.3455590907468,0.538359184536647,25.710587186869));
#48636=CARTESIAN_POINT('Ctrl Pts',(17.3773866994416,0.8508959238502,26.0652826589078));
#48637=CARTESIAN_POINT('Ctrl Pts',(17.4092143081364,0.955147975798902,26.5263909009626));
#48638=CARTESIAN_POINT('Ctrl Pts',(17.4410419168313,0.82559323144673,26.9810373122984));
#48639=CARTESIAN_POINT('Ctrl Pts',(17.4728695255261,0.493950049170587,27.3179368252602));
#48640=CARTESIAN_POINT('Ctrl Pts',(17.5046971342209,0.0413891047270388,
27.454612234474));
#48641=CARTESIAN_POINT('Ctrl Pts',(17.5365247429157,-0.421290564338076,
27.357625725782));
#48642=CARTESIAN_POINT('Ctrl Pts',(17.5683523516105,-0.780868969591605,
27.0506837987796));
#48643=CARTESIAN_POINT('Ctrl Pts',(17.6001799603053,-0.949258013167391,
26.6089855755142));
#48644=CARTESIAN_POINT('Ctrl Pts',(17.6320075690002,-0.885369169676656,
26.1405296139703));
#48645=CARTESIAN_POINT('Ctrl Pts',(17.663835177695,-0.604595160111121,25.7602169486908));
#48646=CARTESIAN_POINT('Ctrl Pts',(17.6956627863898,-0.176129893099558,
25.5607067654733));
#48647=CARTESIAN_POINT('Ctrl Pts',(17.7274903950846,0.296022865466284,25.5916576791216));
#48648=CARTESIAN_POINT('Ctrl Pts',(17.7593180037794,0.69463228888109,25.8439429522386));
#48649=CARTESIAN_POINT('Ctrl Pts',(17.7911456124743,0.925236125635749,26.2587255694389));
#48650=CARTESIAN_POINT('Ctrl Pts',(17.822973221169,0.925632690772768,26.7290377631501));
#48651=CARTESIAN_POINT('Ctrl Pts',(17.8654100327622,0.632304841034162,27.2895650238507));
#48652=CARTESIAN_POINT('Ctrl Pts',(17.9184560472535,-0.186353989231682,
27.5677348942982));
#48653=CARTESIAN_POINT('Ctrl Pts',(17.9715020617449,-0.862383325817902,
27.0286939930005));
#48654=CARTESIAN_POINT('Ctrl Pts',(18.013938873338,-0.948492985808557,26.4019427154772));
#48655=CARTESIAN_POINT('Ctrl Pts',(18.0457664820328,-0.788803737631534,
25.9595706313286));
#48656=CARTESIAN_POINT('Ctrl Pts',(18.0775940907276,-0.431327914010642,
25.6474267789399));
#48657=CARTESIAN_POINT('Ctrl Pts',(18.1094216994224,0.0291754375966058,
25.5450842431823));
#48658=CARTESIAN_POINT('Ctrl Pts',(18.1412493081172,0.483898085490023,25.6759028197294));
#48659=CARTESIAN_POINT('Ctrl Pts',(18.1730769168121,0.819448477247464,26.0087582430504));
#48660=CARTESIAN_POINT('Ctrl Pts',(18.2049045255069,0.954793383821898,26.461697007216));
#48661=CARTESIAN_POINT('Ctrl Pts',(18.2367321342017,0.856217655685264,26.9240989947235));
#48662=CARTESIAN_POINT('Ctrl Pts',(18.2685597428965,0.548160825395486,27.2826421298468));
#48663=CARTESIAN_POINT('Ctrl Pts',(18.3003873515913,0.105866207637405,27.449631492319));
#48664=CARTESIAN_POINT('Ctrl Pts',(18.3322149602861,-0.362312677488355,
27.3841533237673));
#48665=CARTESIAN_POINT('Ctrl Pts',(18.364042568981,-0.741819158733036,27.1022554581978));
#48666=CARTESIAN_POINT('Ctrl Pts',(18.3958701776758,-0.939731762255589,
26.6729314738328));
#48667=CARTESIAN_POINT('Ctrl Pts',(18.4276977863706,-0.907617561427819,
26.2012785620111));
#48668=CARTESIAN_POINT('Ctrl Pts',(18.4595253950654,-0.653330762540545,
25.8027468504271));
#48669=CARTESIAN_POINT('Ctrl Pts',(18.4913530037602,-0.239120318182226,
25.5748920741108));
#48670=CARTESIAN_POINT('Ctrl Pts',(18.5231806124551,0.233623611157383,25.5734886040687));
#48671=CARTESIAN_POINT('Ctrl Pts',(18.5550082211498,0.64917987353908,25.7988804247766));
#48672=CARTESIAN_POINT('Ctrl Pts',(18.5868358298447,0.905827494345743,26.1958949994812));
#48673=CARTESIAN_POINT('Ctrl Pts',(18.6186634385395,0.940742964858958,26.6673496464969));
#48674=CARTESIAN_POINT('Ctrl Pts',(18.6504910472343,0.745379688357512,27.0978397598884));
#48675=CARTESIAN_POINT('Ctrl Pts',(18.6823186559291,0.367559383700563,27.3819882943641));
#48676=CARTESIAN_POINT('Ctrl Pts',(18.7141462646239,-0.100233552067108,
27.4502402248901));
#48677=CARTESIAN_POINT('Ctrl Pts',(18.7459738733188,-0.543490928624728,
27.2858885824934));
#48678=CARTESIAN_POINT('Ctrl Pts',(18.7778014820136,-0.853710433012601,
26.9291640098336));
#48679=CARTESIAN_POINT('Ctrl Pts',(18.8096290907084,-0.95495530914884,26.4673869672972));
#48680=CARTESIAN_POINT('Ctrl Pts',(18.8414566994032,-0.822442430816195,
26.0135930719367));
#48681=CARTESIAN_POINT('Ctrl Pts',(18.873284308098,-0.488608828429489,25.678863796526));
#48682=CARTESIAN_POINT('Ctrl Pts',(18.9051119167929,-0.0351716161159826,
25.5451355021236));
#48683=CARTESIAN_POINT('Ctrl Pts',(18.9369395254877,0.426875043908396,25.6451427319677));
#48684=CARTESIAN_POINT('Ctrl Pts',(18.9687671341825,0.784429535379528,25.954405319031));
#48685=CARTESIAN_POINT('Ctrl Pts',(19.0005947428773,0.949968249657067,26.3972207390307));
#48686=CARTESIAN_POINT('Ctrl Pts',(19.0324223515721,0.88296996287263,26.8651948747223));
#48687=CARTESIAN_POINT('Ctrl Pts',(19.0642499602669,0.599834781719817,27.2437751585608));
#48688=CARTESIAN_POINT('Ctrl Pts',(19.0960775689618,0.169869660374138,27.4402912050732));
#48689=CARTESIAN_POINT('Ctrl Pts',(19.1279051776566,-0.301676831103628,
27.4066390359068));
#48690=CARTESIAN_POINT('Ctrl Pts',(19.1597327863514,-0.699377669708671,
27.1510561626821));
#48691=CARTESIAN_POINT('Ctrl Pts',(19.1915603950462,-0.925882064643884,
26.7361051761929));
#48692=CARTESIAN_POINT('Ctrl Pts',(19.223388003741,-0.925745370520436,26.263359426949));
#48693=CARTESIAN_POINT('Ctrl Pts',(19.2552156124358,-0.699001047869608,
25.848539497029));
#48694=CARTESIAN_POINT('Ctrl Pts',(19.2870432211307,-0.301152472537305,
25.5931866563957));
#48695=CARTESIAN_POINT('Ctrl Pts',(19.3188708298255,0.170413401093204,25.5598071875504));
#48696=CARTESIAN_POINT('Ctrl Pts',(19.3506984385203,0.600264805582684,25.7565718494482));
#48697=CARTESIAN_POINT('Ctrl Pts',(19.3825260472151,0.883181006923094,26.1353158066706));
#48698=CARTESIAN_POINT('Ctrl Pts',(19.4143536559099,0.949908653707736,26.6033286091321));
#48699=CARTESIAN_POINT('Ctrl Pts',(19.4461812646048,0.784113887538146,27.0460482242658));
#48700=CARTESIAN_POINT('Ctrl Pts',(19.4780088732995,0.426380609755225,27.3551039863542));
#48701=CARTESIAN_POINT('Ctrl Pts',(19.5098364819944,-0.0357238071158677,
27.4548439984936));
#48702=CARTESIAN_POINT('Ctrl Pts',(19.5416640906892,-0.489083608598873,
27.3208535043806));
#48703=CARTESIAN_POINT('Ctrl Pts',(19.573491699384,-0.822723581902726,26.9859312293269));
#48704=CARTESIAN_POINT('Ctrl Pts',(19.6053193080788,-0.954974009262693,
26.5320607780124));
#48705=CARTESIAN_POINT('Ctrl Pts',(19.6371469167737,-0.853462105817896,
26.070342362122));
#48706=CARTESIAN_POINT('Ctrl Pts',(19.6689745254685,-0.543036358462768,
25.7137972492788));
#48707=CARTESIAN_POINT('Ctrl Pts',(19.7008021341633,-0.0996840145356615,
25.5497019682752));
#48708=CARTESIAN_POINT('Ctrl Pts',(19.7326297428581,0.368069378378971,25.6182244137232));
#48709=CARTESIAN_POINT('Ctrl Pts',(19.7644573515529,0.745725287013211,25.9025913892794));
#48710=CARTESIAN_POINT('Ctrl Pts',(19.7962849602477,0.940839598136492,26.3331944172625));
#48711=CARTESIAN_POINT('Ctrl Pts',(19.8281125689426,0.905651455747343,26.8046287782806));
#48712=CARTESIAN_POINT('Ctrl Pts',(19.8599401776374,0.648774353094571,27.2014948970739));
#48713=CARTESIAN_POINT('Ctrl Pts',(19.8917677863322,0.233087687590096,27.426646308873));
#48714=CARTESIAN_POINT('Ctrl Pts',(19.923595395027,-0.239655107824156,27.4249695568762));
#48715=CARTESIAN_POINT('Ctrl Pts',(19.9554230037218,-0.653734174120269,
27.1968750830969));
#48716=CARTESIAN_POINT('Ctrl Pts',(19.9872506124167,-0.907789592875371,
26.7981967587369));
#48717=CARTESIAN_POINT('Ctrl Pts',(20.0190782211114,-0.939632669668737,
26.3265246474417));
#48718=CARTESIAN_POINT('Ctrl Pts',(20.0509058298063,-0.741468729693499,
25.8973165219282));
#48719=CARTESIAN_POINT('Ctrl Pts',(20.0827334385011,-0.361805129213555,
25.6156356518217));
#48720=CARTESIAN_POINT('Ctrl Pts',(20.1145610471959,0.106422567756699,25.5504329992433));
#48721=CARTESIAN_POINT('Ctrl Pts',(20.1463886558907,0.548599725918852,25.7176691284529));
#48722=CARTESIAN_POINT('Ctrl Pts',(20.1782162645855,0.856488464327402,26.0764073155399));
#48723=CARTESIAN_POINT('Ctrl Pts',(20.2100438732804,0.954722554770033,26.5388342022888));
#48724=CARTESIAN_POINT('Ctrl Pts',(20.2418714819751,0.8192558664373,26.9917550987657));
#48725=CARTESIAN_POINT('Ctrl Pts',(20.27369909067,0.483248473324846,27.3243022290903));
#48726=CARTESIAN_POINT('Ctrl Pts',(20.3055266993648,0.0289495996207101,
27.4550733859426));
#48727=CARTESIAN_POINT('Ctrl Pts',(20.3373543080596,-0.432435672056107,
27.3520578861717));
#48728=CARTESIAN_POINT('Ctrl Pts',(20.3691819167544,-0.787967622446194,
27.0404722729526));
#48729=CARTESIAN_POINT('Ctrl Pts',(20.4010095254493,-0.950617728686493,
26.5965877101963));
#48730=CARTESIAN_POINT('Ctrl Pts',(20.4328371341441,-0.880571851783068,
26.1290600241261));
#48731=CARTESIAN_POINT('Ctrl Pts',(20.4646647428389,-0.594976099681679,
25.7523324985921));
#48732=CARTESIAN_POINT('Ctrl Pts',(20.4964923515337,-0.163739734866541,
25.5586219935223));
#48733=CARTESIAN_POINT('Ctrl Pts',(20.5283199602285,0.307577492565278,25.5953457356972));
#48734=CARTESIAN_POINT('Ctrl Pts',(20.5601475689234,0.703604679778453,25.8535143416533));
#48735=CARTESIAN_POINT('Ctrl Pts',(20.5919751776182,0.927400719007669,26.269932274671));
#48736=CARTESIAN_POINT('Ctrl Pts',(20.623802786313,0.924183926932062,26.7426670992418));
#48737=CARTESIAN_POINT('Ctrl Pts',(20.6556303950078,0.694741722691852,27.1560009074729));
#48738=CARTESIAN_POINT('Ctrl Pts',(20.6874580037026,0.295237880303865,27.4087562081701));
#48739=CARTESIAN_POINT('Ctrl Pts',(20.7192856123974,-0.176535463004856,
27.4390625549747));
#48740=CARTESIAN_POINT('Ctrl Pts',(20.7511132210923,-0.605095754543117,
27.2395014399499));
#48741=CARTESIAN_POINT('Ctrl Pts',(20.782940829787,-0.885538304058988,26.8589222254171));
#48742=CARTESIAN_POINT('Ctrl Pts',(20.8147684384819,-0.949215270463799,
26.3904846030352));
#48743=CARTESIAN_POINT('Ctrl Pts',(20.8465960471767,-0.780539553018697,
25.9488545944785));
#48744=CARTESIAN_POINT('Ctrl Pts',(20.8784236558715,-0.420800263759921,
25.6421361472392));
#48745=CARTESIAN_POINT('Ctrl Pts',(20.9102512645663,0.041944185331135,25.545409021009));
#48746=CARTESIAN_POINT('Ctrl Pts',(20.9420788732612,0.494421370149437,25.6823504659124));
#48747=CARTESIAN_POINT('Ctrl Pts',(20.9739064819559,0.825872128316555,26.0194394111832));
#48748=CARTESIAN_POINT('Ctrl Pts',(21.0057340906508,0.955162626843708,26.4741618860005));
#48749=CARTESIAN_POINT('Ctrl Pts',(21.0375616993456,0.850644624005495,26.9352091169824));
#48750=CARTESIAN_POINT('Ctrl Pts',(21.0693893080404,0.537902451645026,27.2897241318133));
#48751=CARTESIAN_POINT('Ctrl Pts',(21.1012169167353,0.0934903808134796,
27.4509273371553));
#48752=CARTESIAN_POINT('Ctrl Pts',(21.1330445254301,-0.373806636744173,
27.379358772163));
#48753=CARTESIAN_POINT('Ctrl Pts',(21.1648721341249,-0.749601781132445,
27.09253727442));
#48754=CARTESIAN_POINT('Ctrl Pts',(21.1966997428197,-0.941906424383186,
26.660672149297));
#48755=CARTESIAN_POINT('Ctrl Pts',(21.2285273515145,-0.90364747215577,26.1894770573363));
#48756=CARTESIAN_POINT('Ctrl Pts',(21.2603549602093,-0.644190102727395,
25.7942930045677));
#48757=CARTESIAN_POINT('Ctrl Pts',(21.2921825689042,-0.227045321459216,
25.5718547129584));
#48758=CARTESIAN_POINT('Ctrl Pts',(21.324010177599,0.245676515339092,25.5766115109745));
#48759=CARTESIAN_POINT('Ctrl Pts',(21.3558377862938,0.658260678972873,25.8073990107051));
#48760=CARTESIAN_POINT('Ctrl Pts',(21.3876653949886,0.909713179230154,26.2077241313605));
#48761=CARTESIAN_POINT('Ctrl Pts',(21.4194930036834,0.938482474417972,26.6795936999572));
#48762=CARTESIAN_POINT('Ctrl Pts',(21.4513206123782,0.737526302198827,27.1075016093962));
#48763=CARTESIAN_POINT('Ctrl Pts',(21.4831482210731,0.356035512535034,27.3867028621065));
#48764=CARTESIAN_POINT('Ctrl Pts',(21.5149758297678,-0.112607063933625,
27.4488534665618));
#48765=CARTESIAN_POINT('Ctrl Pts',(21.5468034384627,-0.553685236057366,
27.2787399509632));
#48766=CARTESIAN_POINT('Ctrl Pts',(21.5786310471575,-0.859230137057964,
26.9180033772894));
#48767=CARTESIAN_POINT('Ctrl Pts',(21.6104586558523,-0.954449272552715,
26.4549462767619));
#48768=CARTESIAN_POINT('Ctrl Pts',(21.6422862645472,-0.816034524378642,
26.002917605546));
#48769=CARTESIAN_POINT('Ctrl Pts',(21.6741138732419,-0.477867604327989,
25.6725667370791));
#48770=CARTESIAN_POINT('Ctrl Pts',(21.7059414819368,-0.0227263541696066,
25.544758268981));
#48771=CARTESIAN_POINT('Ctrl Pts',(21.7377690906316,0.437977943223417,25.6507776656824));
#48772=CARTESIAN_POINT('Ctrl Pts',(21.7695966993264,0.791472260181452,25.9646730781875));
#48773=CARTESIAN_POINT('Ctrl Pts',(21.8014243080212,0.951226853845677,26.4096079407421));
#48774=CARTESIAN_POINT('Ctrl Pts',(21.833251916716,0.878136360290474,26.8766693305671));
#48775=CARTESIAN_POINT('Ctrl Pts',(21.8650795254109,0.590092160817773,27.251528105659));
#48776=CARTESIAN_POINT('Ctrl Pts',(21.8969071341057,0.157602858583708,27.4424248462452));
#48777=CARTESIAN_POINT('Ctrl Pts',(21.9287347428005,-0.313465097317032,
27.4026310899908));
#48778=CARTESIAN_POINT('Ctrl Pts',(21.9605623514953,-0.707801821724523,
27.1418877105986));
#48779=CARTESIAN_POINT('Ctrl Pts',(21.9923899601901,-0.928880005072949,
26.7240205080561));
#48780=CARTESIAN_POINT('Ctrl Pts',(22.0242175688849,-0.922583251598293,
26.2513166758218));
#48781=CARTESIAN_POINT('Ctrl Pts',(22.0560451775798,-0.690452905624547,
25.8394865353616));
#48782=CARTESIAN_POINT('Ctrl Pts',(22.0878727862746,-0.289310755178418,
25.5893395041004));
#48783=CARTESIAN_POINT('Ctrl Pts',(22.1197003949694,0.182650030959813,25.5621075658454));
#48784=CARTESIAN_POINT('Ctrl Pts',(22.1515280036642,0.609901017098679,25.7644566625983));
#48785=CARTESIAN_POINT('Ctrl Pts',(22.183355612359,0.887858009961992,26.1468549787971));
#48786=CARTESIAN_POINT('Ctrl Pts',(22.2151832210538,0.94848159289027,26.6156975358526));
#48787=CARTESIAN_POINT('Ctrl Pts',(22.2470108297487,0.776932084478994,27.0562191905725));
#48788=CARTESIAN_POINT('Ctrl Pts',(22.2788384384435,0.415202054730778,27.3605873027191));
#48789=CARTESIAN_POINT('Ctrl Pts',(22.3106660471383,-0.0481627830094708,
27.4542974369591));
#48790=CARTESIAN_POINT('Ctrl Pts',(22.3424936558331,-0.4997381434392,27.31441085445));
#48791=CARTESIAN_POINT('Ctrl Pts',(22.3743212645279,-0.828985616335545,
26.975169548438));
#48792=CARTESIAN_POINT('Ctrl Pts',(22.4061488732227,-0.955310697628965,
26.5196143531548));
#48793=CARTESIAN_POINT('Ctrl Pts',(22.4379764819176,-0.847791032202123,
26.0592578786051));
#48794=CARTESIAN_POINT('Ctrl Pts',(22.4698040906124,-0.532745710788099,
25.7067880110015));
#48795=CARTESIAN_POINT('Ctrl Pts',(22.5016316993072,-0.0872927784106915,
25.5484837244212));
#48796=CARTESIAN_POINT('Ctrl Pts',(22.533459308002,0.379528026961983,25.6230953708616));
#48797=CARTESIAN_POINT('Ctrl Pts',(22.5652869166968,0.753446454544427,25.9123592151761));
#48798=CARTESIAN_POINT('Ctrl Pts',(22.5971145253917,0.942933266561886,26.3454681047002));
#48799=CARTESIAN_POINT('Ctrl Pts',(22.6289421340865,0.90160512859444,26.8164039253015));
#48800=CARTESIAN_POINT('Ctrl Pts',(22.6607697427813,0.639578506394438,27.2098891364236));
#48801=CARTESIAN_POINT('Ctrl Pts',(22.6925973514761,0.220993317220635,27.4296048653045));
#48802=CARTESIAN_POINT('Ctrl Pts',(22.7244249601709,-0.251687493849366,
27.421768223196));
#48803=CARTESIAN_POINT('Ctrl Pts',(22.7562525688658,-0.662759240561632,
27.1882974944776));
#48804=CARTESIAN_POINT('Ctrl Pts',(22.7880801775606,-0.911598148125007,
26.786342571388));
#48805=CARTESIAN_POINT('Ctrl Pts',(22.8199077862554,-0.937292440446401,
26.314295576423));
#48806=CARTESIAN_POINT('Ctrl Pts',(22.8517353949502,-0.733552566602793,
25.8877060478133));
#48807=CARTESIAN_POINT('Ctrl Pts',(22.883563003645,-0.350250782096009,25.6109962646337));
#48808=CARTESIAN_POINT('Ctrl Pts',(22.9153906123398,0.118786779923891,25.5519003466042));
#48809=CARTESIAN_POINT('Ctrl Pts',(22.9472182210346,0.558747242175138,25.7248840272477));
#48810=CARTESIAN_POINT('Ctrl Pts',(22.9790458297295,0.861935335341246,26.0876036741868));
#48811=CARTESIAN_POINT('Ctrl Pts',(23.0108734384243,0.954135473821638,26.5512713316502));
#48812=CARTESIAN_POINT('Ctrl Pts',(23.0427010471191,0.812778541532895,27.0023885889206));
#48813=CARTESIAN_POINT('Ctrl Pts',(23.0745286558139,0.472466449780163,27.3305291720862));
#48814=CARTESIAN_POINT('Ctrl Pts',(23.1063562645087,0.0165021439813753,
27.4553695259417));
#48815=CARTESIAN_POINT('Ctrl Pts',(23.1381838732036,-0.443501622161829,
27.3463507328489));
#48816=CARTESIAN_POINT('Ctrl Pts',(23.1700114818984,-0.794943299801397,
27.0301588459649));
#48817=CARTESIAN_POINT('Ctrl Pts',(23.2018390905932,-0.951795599283248,
26.5841925711631));
#48818=CARTESIAN_POINT('Ctrl Pts',(23.233666699288,-0.875663591778624,26.1176173044091));
#48819=CARTESIAN_POINT('Ctrl Pts',(23.2654943079828,-0.585183172453782,
25.7446431925699));
#48820=CARTESIAN_POINT('Ctrl Pts',(23.2973219166776,-0.151459292036076,
25.5565683200624));
#48821=CARTESIAN_POINT('Ctrl Pts',(23.3291495253724,0.319339395428713,25.5994304011453));
#48822=CARTESIAN_POINT('Ctrl Pts',(23.3609771340673,0.711968917377853,25.8627374853784));
#48823=CARTESIAN_POINT('Ctrl Pts',(23.3928047427621,0.930319860043684,26.2820362189208));
#48824=CARTESIAN_POINT('Ctrl Pts',(23.4246323514569,0.920943412468097,26.7546889924705));
#48825=CARTESIAN_POINT('Ctrl Pts',(23.4564599601517,0.686134778728554,27.1649979829091));
#48826=CARTESIAN_POINT('Ctrl Pts',(23.4882875688465,0.283371348768303,27.4125261259554));
#48827=CARTESIAN_POINT('Ctrl Pts',(23.5201151775414,-0.188756845393764,
27.4366824996609));
#48828=CARTESIAN_POINT('Ctrl Pts',(23.5519427862362,-0.614680389265223,
27.2315540109293));
#48829=CARTESIAN_POINT('Ctrl Pts',(23.583770394931,-0.890140026160248,26.8473528259298));
#48830=CARTESIAN_POINT('Ctrl Pts',(23.6155980036258,-0.947707652131871,
26.3781252366373));
#48831=CARTESIAN_POINT('Ctrl Pts',(23.6474256123206,-0.773291635056603,
25.9387306359639));
#48832=CARTESIAN_POINT('Ctrl Pts',(23.6792532210155,-0.409586220312577,
25.6367257793817));
#48833=CARTESIAN_POINT('Ctrl Pts',(23.7110808297102,0.0543793361704953,
25.546036615141));
#48834=CARTESIAN_POINT('Ctrl Pts',(23.7429084384051,0.505033702770359,25.6888623970496));
#48835=CARTESIAN_POINT('Ctrl Pts',(23.7747360470999,0.832063913791676,26.0302416629588));
#48836=CARTESIAN_POINT('Ctrl Pts',(23.8065636557947,0.95541821533284,26.4866102403221));
#48837=CARTESIAN_POINT('Ctrl Pts',(23.8383912644896,0.844901451543165,26.9462564162388));
#48838=CARTESIAN_POINT('Ctrl Pts',(23.8702188731843,0.527566354796399,27.2966661742165));
#48839=CARTESIAN_POINT('Ctrl Pts',(23.9020464818792,0.0810914704164689,
27.4520648219947));
#48840=CARTESIAN_POINT('Ctrl Pts',(23.933874090574,-0.385233306158512,27.3744132613817));
#48841=CARTESIAN_POINT('Ctrl Pts',(23.9657016992688,-0.757259144042203,
27.082719349789));
#48842=CARTESIAN_POINT('Ctrl Pts',(23.9975293079636,-0.943920081082997,
26.6483850814007));
#48843=CARTESIAN_POINT('Ctrl Pts',(24.0293569166584,-0.899524511761129,
26.1777285234543));
#48844=CARTESIAN_POINT('Ctrl Pts',(24.0611845253532,-0.634939759858623,
25.7859588574846));
#48845=CARTESIAN_POINT('Ctrl Pts',(24.0930121340481,-0.214931931782802,
25.5689750182975));
#48846=CARTESIAN_POINT('Ctrl Pts',(24.1248397427429,0.257687788188069,25.579891171832));
#48847=CARTESIAN_POINT('Ctrl Pts',(24.1566673514377,0.667229667921932,25.8160352186707));
#48848=CARTESIAN_POINT('Ctrl Pts',(24.1884949601325,0.913444419542706,26.2196028811483));
#48849=CARTESIAN_POINT('Ctrl Pts',(24.2203225688273,0.936062618271151,26.6918072640162));
#48850=CARTESIAN_POINT('Ctrl Pts',(24.2521501775222,0.729547691591071,27.1170603030079));
#48851=CARTESIAN_POINT('Ctrl Pts',(24.283977786217,0.344451183459123,27.391266870285));
#48852=CARTESIAN_POINT('Ctrl Pts',(24.3158053949118,-0.124961453397658,
27.4473055932585));
#48853=CARTESIAN_POINT('Ctrl Pts',(24.3476330036066,-0.563785529389269,
27.2714590907529));
#48854=CARTESIAN_POINT('Ctrl Pts',(24.3794606123014,-0.864603944341185,
26.9067717680514));
#48855=CARTESIAN_POINT('Ctrl Pts',(24.4112882209962,-0.953781171897604,
26.4425132364135));
#48856=CARTESIAN_POINT('Ctrl Pts',(24.4431158296911,-0.809488056117004,
25.9923265430831));
#48857=CARTESIAN_POINT('Ctrl Pts',(24.4749434383859,-0.467045238961159,
25.6664101748356));
#48858=CARTESIAN_POINT('Ctrl Pts',(24.5067710470807,-0.0102772332746646,
25.5445432347142));
#48859=CARTESIAN_POINT('Ctrl Pts',(24.5385986557755,0.449006474390322,25.6565567963345));
#48860=CARTESIAN_POINT('Ctrl Pts',(24.5704262644703,0.79838059395987,25.9750317352046));
#48861=CARTESIAN_POINT('Ctrl Pts',(24.6022538731651,0.952323940855888,26.4220104909188));
#48862=CARTESIAN_POINT('Ctrl Pts',(24.63408148186,0.873153651216892,26.8880798284125));
#48863=CARTESIAN_POINT('Ctrl Pts',(24.6659090905548,0.580249342976974,27.2591534441921));
#48864=CARTESIAN_POINT('Ctrl Pts',(24.6977366992496,0.145309296018941,27.4443984648148));
#48865=CARTESIAN_POINT('Ctrl Pts',(24.7295643079444,-0.325200137535511,
27.3984698784049));
#48866=CARTESIAN_POINT('Ctrl Pts',(24.7613919166392,-0.716105789844623,
27.1326102667559));
#48867=CARTESIAN_POINT('Ctrl Pts',(24.7932195253341,-0.931720222797812,
26.7118978015073));
#48868=CARTESIAN_POINT('Ctrl Pts',(24.8250471340289,-0.919264479152886,
26.2393161508229));
#48869=CARTESIAN_POINT('Ctrl Pts',(24.8568747427237,-0.681787525309043,
25.8305457280837));
#48870=CARTESIAN_POINT('Ctrl Pts',(24.8887023514185,-0.277419913202257,
25.5856469808586));
#48871=CARTESIAN_POINT('Ctrl Pts',(24.9205299601133,0.194855647071497,25.5645671971444));
#48872=CARTESIAN_POINT('Ctrl Pts',(24.9523575688081,0.6194336681577,25.7724663701197));
#48873=CARTESIAN_POINT('Ctrl Pts',(24.984185177503,0.892384255781827,26.1584541145223));
#48874=CARTESIAN_POINT('Ctrl Pts',(25.0160127861977,0.946893481042504,26.628046817271));
#48875=CARTESIAN_POINT('Ctrl Pts',(25.0478403948926,0.769618359289142,27.0662957115316));
#48876=CARTESIAN_POINT('Ctrl Pts',(25.0796680035874,0.403952998898319,27.3659244923982));
#48877=CARTESIAN_POINT('Ctrl Pts',(25.1114956122822,-0.0605935809206184,
27.4535888368711));
#48878=CARTESIAN_POINT('Ctrl Pts',(25.1433232209771,-0.510307823345631,
27.3078299185387));
#48879=CARTESIAN_POINT('Ctrl Pts',(25.1751508296718,-0.835106890010742,
26.964327184333));
#48880=CARTESIAN_POINT('Ctrl Pts',(25.2069784383667,-0.955485175391192,
26.5071645978036));
#48881=CARTESIAN_POINT('Ctrl Pts',(25.2388060470615,-0.841976004691772,
26.0482482325687));
#48882=CARTESIAN_POINT('Ctrl Pts',(25.2706336557563,-0.522364603534392,
25.699913459163));
#48883=CARTESIAN_POINT('Ctrl Pts',(25.3024612644511,-0.0748867200772622,
25.547427046883));
#48884=CARTESIAN_POINT('Ctrl Pts',(25.3342888731459,0.390922232143804,25.6281152253481));
#48885=CARTESIAN_POINT('Ctrl Pts',(25.3661164818408,0.761039687776565,25.9222268217692));
#48886=CARTESIAN_POINT('Ctrl Pts',(25.3979440905356,0.944866826056054,26.3577680314671));
#48887=CARTESIAN_POINT('Ctrl Pts',(25.4297716992304,0.897405709978404,26.8281253473178));
#48888=CARTESIAN_POINT('Ctrl Pts',(25.4615993079252,0.630274060035337,27.218162837454));
#48889=CARTESIAN_POINT('Ctrl Pts',(25.49342691662,0.208861422452774,27.4324055759519));
#48890=CARTESIAN_POINT('Ctrl Pts',(25.5252545253149,-0.263677143642244,
27.4184103743823));
#48891=CARTESIAN_POINT('Ctrl Pts',(25.5570821340096,-0.671671771282482,
27.1796030337761));
#48892=CARTESIAN_POINT('Ctrl Pts',(25.5889097427045,-0.915251915110534,
26.7744397634122));
#48893=CARTESIAN_POINT('Ctrl Pts',(25.6207373513993,-0.934793060094999,
26.3020980377986));
#48894=CARTESIAN_POINT('Ctrl Pts',(25.6525649600941,-0.725511847177558,
25.8781995404594));
#48895=CARTESIAN_POINT('Ctrl Pts',(25.6843925687889,-0.338636962806214,
25.6065078292329));
#48896=CARTESIAN_POINT('Ctrl Pts',(25.7162201774838,0.131130822216466,25.5535286800947));
#48897=CARTESIAN_POINT('Ctrl Pts',(25.7480477861786,0.568799883866499,25.7322305398899));
#48898=CARTESIAN_POINT('Ctrl Pts',(25.7798753948734,0.867235850694155,26.0988700570622));
#48899=CARTESIAN_POINT('Ctrl Pts',(25.8117030035682,0.953386381973287,26.5636997555226));
#48900=CARTESIAN_POINT('Ctrl Pts',(25.843530612263,0.80616320752463,27.0129367734926));
#48901=CARTESIAN_POINT('Ctrl Pts',(25.8753582209578,0.461604202545949,27.3366150933761));
#48902=CARTESIAN_POINT('Ctrl Pts',(25.9071858296527,0.00405188527124226,
27.4555034431848));
#48903=CARTESIAN_POINT('Ctrl Pts',(25.9390134383475,-0.454492264288568,
27.3404998742768));
#48904=CARTESIAN_POINT('Ctrl Pts',(25.9708410470423,-0.801784000403587,
27.019755390933));
#48905=CARTESIAN_POINT('Ctrl Pts',(26.0026686557371,-0.952811849223926,
26.5717831508947));
#48906=CARTESIAN_POINT('Ctrl Pts',(26.034496264432,-0.870606658202922,26.1062394853173));
#48907=CARTESIAN_POINT('Ctrl Pts',(26.0663238731267,-0.575290857187556,
25.7370821971392));
#48908=CARTESIAN_POINT('Ctrl Pts',(26.0981514818216,-0.139153178128873,
25.5546747421343));
#48909=CARTESIAN_POINT('Ctrl Pts',(26.1299790905164,0.331047162702991,25.6036681673243));
#48910=CARTESIAN_POINT('Ctrl Pts',(26.1618066992112,0.720212097625758,25.8720684860043));
#48911=CARTESIAN_POINT('Ctrl Pts',(26.193634307906,0.933081347121382,26.2941778330969));
#48912=CARTESIAN_POINT('Ctrl Pts',(26.2254619166008,0.917545931470056,26.7666663937008));
#48913=CARTESIAN_POINT('Ctrl Pts',(26.2572895252956,0.677412446761784,27.1738844955338));
#48914=CARTESIAN_POINT('Ctrl Pts',(26.2891171339905,0.271454591702591,27.416136653851));
#48915=CARTESIAN_POINT('Ctrl Pts',(26.3209447426853,-0.200942189437803,
27.434151796482));
#48916=CARTESIAN_POINT('Ctrl Pts',(26.3527723513801,-0.624168219542933,
27.223466435793));
#48917=CARTESIAN_POINT('Ctrl Pts',(26.3845999600749,-0.894576003957899,
26.8357550859606));
#48918=CARTESIAN_POINT('Ctrl Pts',(26.4164275687697,-0.946069180424221,
26.365724145282));
#48919=CARTESIAN_POINT('Ctrl Pts',(26.4376459745663,-0.82591582866072,26.0744774398212));
#48920=CARTESIAN_POINT('Ctrl Pts',(26.4482551774646,-0.734601664004067,
25.9520568295746));
#48921=CARTESIAN_POINT('Ctrl Pts',(9.60000015794368,-0.899145364714185,
26.9202321182148));
#48922=CARTESIAN_POINT('Ctrl Pts',(9.61060936084195,-0.969176614135344,
26.770390469819));
#48923=CARTESIAN_POINT('Ctrl Pts',(9.63182776663849,-1.03281304011026,26.4351748220049));
#48924=CARTESIAN_POINT('Ctrl Pts',(9.66365537533331,-0.87523841633845,25.9479403018373));
#48925=CARTESIAN_POINT('Ctrl Pts',(9.69548298402813,-0.503515492261773,
25.5959674242812));
#48926=CARTESIAN_POINT('Ctrl Pts',(9.72731059272294,-0.00849156889496621,
25.4652231538941));
#48927=CARTESIAN_POINT('Ctrl Pts',(9.75913820141777,0.488585575395564,25.58780926119));
#48928=CARTESIAN_POINT('Ctrl Pts',(9.79096581011257,0.866078206808652,25.933667292316));
#48929=CARTESIAN_POINT('Ctrl Pts',(9.82279341880741,1.03156168020563,26.4181638872238));
#48930=CARTESIAN_POINT('Ctrl Pts',(9.85462102750221,0.944539145419091,26.9226876762002));
#48931=CARTESIAN_POINT('Ctrl Pts',(9.88644863619703,0.62630657764322,27.3237469315434));
#48932=CARTESIAN_POINT('Ctrl Pts',(9.91827624489185,0.154765252016519,27.5231647461145));
#48933=CARTESIAN_POINT('Ctrl Pts',(9.95010385358666,-0.354660684709781,
27.4721289694078));
#48934=CARTESIAN_POINT('Ctrl Pts',(9.9819314622815,-0.777271074907365,27.1831312112822));
#48935=CARTESIAN_POINT('Ctrl Pts',(10.0137590709763,-1.00961812086333,26.7269140893577));
#48936=CARTESIAN_POINT('Ctrl Pts',(10.0455866796711,-0.994826750456996,
26.2151519256561));
#48937=CARTESIAN_POINT('Ctrl Pts',(10.0774142883659,-0.736517780875856,
25.7731160630381));
#48938=CARTESIAN_POINT('Ctrl Pts',(10.1092418970608,-0.297921040455159,
25.5090097066483));
#48939=CARTESIAN_POINT('Ctrl Pts',(10.1410695057556,0.21360198317146,25.4874819064308));
#48940=CARTESIAN_POINT('Ctrl Pts',(10.1728971144504,0.672838671527312,25.7138022978844));
#48941=CARTESIAN_POINT('Ctrl Pts',(10.2047247231452,0.967375234136969,26.1325712899329));
#48942=CARTESIAN_POINT('Ctrl Pts',(10.23655233184,1.02511384669292,26.641280938506));
#48943=CARTESIAN_POINT('Ctrl Pts',(10.2683799405348,0.831921019498759,27.1154072791165));
#48944=CARTESIAN_POINT('Ctrl Pts',(10.3002075492297,0.435087261570011,27.4388917810866));
#48945=CARTESIAN_POINT('Ctrl Pts',(10.3320351579245,-0.0682488845295447,
27.5325506242975));
#48946=CARTESIAN_POINT('Ctrl Pts',(10.3638627666193,-0.554878797469749,
27.3734576245781));
#48947=CARTESIAN_POINT('Ctrl Pts',(10.3956903753141,-0.90568327466009,27.0005561985521));
#48948=CARTESIAN_POINT('Ctrl Pts',(10.4275179840089,-1.03479100278662,26.5051266381597));
#48949=CARTESIAN_POINT('Ctrl Pts',(10.4593455927037,-0.910598479450232,
26.0084421589457));
#48950=CARTESIAN_POINT('Ctrl Pts',(10.4911732013986,-0.563506043729093,
25.6320831603431));
#48951=CARTESIAN_POINT('Ctrl Pts',(10.5230008100934,-0.0784763605841615,
25.4681762928169));
#48952=CARTESIAN_POINT('Ctrl Pts',(10.5548284187882,0.425763077787955,25.5568433303679));
#48953=CARTESIAN_POINT('Ctrl Pts',(10.586656027483,0.825782538997791,25.8763800033968));
#48954=CARTESIAN_POINT('Ctrl Pts',(10.6184836361778,1.02366367059781,26.3485688559903));
#48955=CARTESIAN_POINT('Ctrl Pts',(10.6503112448726,0.970968343280062,26.8578256254456));
#48956=CARTESIAN_POINT('Ctrl Pts',(10.6821388535675,0.680595528553212,27.2794924171479));
#48957=CARTESIAN_POINT('Ctrl Pts',(10.7139664622623,0.223623837263367,27.5103519591139));
#48958=CARTESIAN_POINT('Ctrl Pts',(10.7457940709571,-0.28808738506616,27.493893535769));
#48959=CARTESIAN_POINT('Ctrl Pts',(10.7776216796519,-0.729279433098497,
27.2341459053465));
#48960=CARTESIAN_POINT('Ctrl Pts',(10.8094492883467,-0.991955565058188,
26.7946911244468));
#48961=CARTESIAN_POINT('Ctrl Pts',(10.8412768970415,-1.0118168741079,26.2831006796964));
#48962=CARTESIAN_POINT('Ctrl Pts',(10.8731045057364,-0.784001630136379,
25.8246037120171));
#48963=CARTESIAN_POINT('Ctrl Pts',(10.9049321144312,-0.36427535336417,25.5314329301442));
#48964=CARTESIAN_POINT('Ctrl Pts',(10.936759723126,0.144619691176789,25.4753518424349));
#48965=CARTESIAN_POINT('Ctrl Pts',(10.9685873318208,0.618114153333466,25.6700882002728));
#48966=CARTESIAN_POINT('Ctrl Pts',(11.0004149405156,0.94030417810739,26.0679736645627));
#48967=CARTESIAN_POINT('Ctrl Pts',(11.0322425492105,1.0323228116101,26.571612251096));
#48968=CARTESIAN_POINT('Ctrl Pts',(11.0640701579053,0.871645367267493,27.0577213063876));
#48969=CARTESIAN_POINT('Ctrl Pts',(11.0958977666001,0.497603108059459,27.4073091252309));
#48970=CARTESIAN_POINT('Ctrl Pts',(11.1277253752949,0.00175558375789874,
27.5348022128906));
#48971=CARTESIAN_POINT('Ctrl Pts',(11.1595529839897,-0.494521679308475,
27.4089923050123));
#48972=CARTESIAN_POINT('Ctrl Pts',(11.1913805926845,-0.869747961649325,
27.0606756505186));
#48973=CARTESIAN_POINT('Ctrl Pts',(11.2232082013794,-1.03207388360779,26.5751145834865));
#48974=CARTESIAN_POINT('Ctrl Pts',(11.2550358100742,-0.941764661305992,
26.0711666703802));
#48975=CARTESIAN_POINT('Ctrl Pts',(11.286863418769,-0.62092654485511,25.6721902828718));
#48976=CARTESIAN_POINT('Ctrl Pts',(11.3186910274638,-0.148095562654985,
25.4758484456881));
#48977=CARTESIAN_POINT('Ctrl Pts',(11.3505186361586,0.360986839554778,25.5302024935349));
#48978=CARTESIAN_POINT('Ctrl Pts',(11.3823462448535,0.781705449466869,25.8219474267054));
#48979=CARTESIAN_POINT('Ctrl Pts',(11.4141738535483,1.01107509480216,26.2796687617508));
#48980=CARTESIAN_POINT('Ctrl Pts',(11.4460014622431,0.992949762800771,26.7913236523723));
#48981=CARTESIAN_POINT('Ctrl Pts',(11.4778290709379,0.73176624421736,27.2316671823319));
#48982=CARTESIAN_POINT('Ctrl Pts',(11.5096566796327,0.291458078058921,27.4929103134785));
#48983=CARTESIAN_POINT('Ctrl Pts',(11.5414842883276,-0.22019435401471,27.5111049146046));
#48984=CARTESIAN_POINT('Ctrl Pts',(11.5733118970223,-0.677946737578888,
27.2817972389845));
#48985=CARTESIAN_POINT('Ctrl Pts',(11.6051395057172,-0.96974862615495,26.8611181301848));
#48986=CARTESIAN_POINT('Ctrl Pts',(11.636967114412,-1.02417159452383,26.3520430912457));
#48987=CARTESIAN_POINT('Ctrl Pts',(11.6687947231068,-0.82789377233951,25.8791855320637));
#48988=CARTESIAN_POINT('Ctrl Pts',(11.7006223318016,-0.428960824462024,
25.5582934039976));
#48989=CARTESIAN_POINT('Ctrl Pts',(11.7324499404964,0.0749748577072528,
25.467915956625));
#48990=CARTESIAN_POINT('Ctrl Pts',(11.7642775491913,0.560557896433451,25.6301761404608));
#48991=CARTESIAN_POINT('Ctrl Pts',(11.7961051578861,0.908925346933881,26.0053552632659));
#48992=CARTESIAN_POINT('Ctrl Pts',(11.8279327665809,1.03480244108332,26.5016154892819));
#48993=CARTESIAN_POINT('Ctrl Pts',(11.8597603752757,0.907376483836781,26.9974802694154));
#48994=CARTESIAN_POINT('Ctrl Pts',(11.8915879839705,0.557839307099688,27.3715698533865));
#48995=CARTESIAN_POINT('Ctrl Pts',(11.9234155926653,0.0717520092312157,
27.5323131070799));
#48996=CARTESIAN_POINT('Ctrl Pts',(11.9552432013602,-0.431899030430357,
27.4403626584414));
#48997=CARTESIAN_POINT('Ctrl Pts',(11.987070810055,-0.829828110073699,27.1182265034833));
#48998=CARTESIAN_POINT('Ctrl Pts',(12.0188984187498,-1.02462856915081,26.6447584096265));
#48999=CARTESIAN_POINT('Ctrl Pts',(12.0507260274446,-0.968616377610574,
26.1358557773324));
#49000=CARTESIAN_POINT('Ctrl Pts',(12.0825536361394,-0.675502422158747,
25.7160898141143));
#49001=CARTESIAN_POINT('Ctrl Pts',(12.1143812448342,-0.217036300955299,
25.4882124996101));
#49002=CARTESIAN_POINT('Ctrl Pts',(12.1462088535291,0.294556827987056,25.5080045479117));
#49003=CARTESIAN_POINT('Ctrl Pts',(12.1780364622239,0.73404716669968,25.770621182829));
#49004=CARTESIAN_POINT('Ctrl Pts',(12.2098640709187,0.993854524573037,26.2117780614468));
#49005=CARTESIAN_POINT('Ctrl Pts',(12.2416916796135,1.01038222468437,26.7234870508989));
#49006=CARTESIAN_POINT('Ctrl Pts',(12.2735192883083,0.779584550958275,27.1804899924208));
#49007=CARTESIAN_POINT('Ctrl Pts',(12.3053468970032,0.357957074615781,27.4709198909334));
#49008=CARTESIAN_POINT('Ctrl Pts',(12.337174505698,-0.151292556129472,27.5236841623946));
#49009=CARTESIAN_POINT('Ctrl Pts',(12.3690021143928,-0.623508194105078,
27.325866958875));
#49010=CARTESIAN_POINT('Ctrl Pts',(12.4008297230876,-0.943099019974642,
26.9258907611119));
#49011=CARTESIAN_POINT('Ctrl Pts',(12.4326573317824,-1.03183432208061,26.4216633313571));
#49012=CARTESIAN_POINT('Ctrl Pts',(12.4644849404772,-0.867993120748392,
25.9366114624781));
#49013=CARTESIAN_POINT('Ctrl Pts',(12.496312549172,-0.491681115959126,25.5894680773928));
#49014=CARTESIAN_POINT('Ctrl Pts',(12.5281401578669,0.00498654517730746,
25.4652083126325));
#49015=CARTESIAN_POINT('Ctrl Pts',(12.5599677665617,0.500433579980453,25.594248966931));
#49016=CARTESIAN_POINT('Ctrl Pts',(12.5917953752565,0.873382495531615,25.9450029564253));
#49017=CARTESIAN_POINT('Ctrl Pts',(12.6236229839513,1.03254137506161,26.431611326497));
#49018=CARTESIAN_POINT('Ctrl Pts',(12.6554505926462,0.938950675916567,26.9349601476841));
#49019=CARTESIAN_POINT('Ctrl Pts',(12.6872782013409,0.615519901142211,27.3318376964141));
#49020=CARTESIAN_POINT('Ctrl Pts',(12.7191058100358,0.141419720339925,27.525094710052));
#49021=CARTESIAN_POINT('Ctrl Pts',(12.7509334187306,-0.367297741276047,
27.4674249692514));
#49022=CARTESIAN_POINT('Ctrl Pts',(12.7827610274254,-0.786106603006349,
27.1729451022093));
#49023=CARTESIAN_POINT('Ctrl Pts',(12.8145886361202,-1.01248916831665,26.7137390603495));
#49024=CARTESIAN_POINT('Ctrl Pts',(12.846416244815,-0.991030613759187,26.2022131224017));
#49025=CARTESIAN_POINT('Ctrl Pts',(12.8782438535099,-0.726983649544281,
25.7635806390562));
#49026=CARTESIAN_POINT('Ctrl Pts',(12.9100714622047,-0.284982740273187,
25.5052118116785));
#49027=CARTESIAN_POINT('Ctrl Pts',(12.9418990708995,0.22677737601216,25.4903511879833));
#49028=CARTESIAN_POINT('Ctrl Pts',(12.9737266795943,0.683026025518092,25.7226364104599));
#49029=CARTESIAN_POINT('Ctrl Pts',(13.0055542882891,0.97208085176103,26.1452077797962));
#49030=CARTESIAN_POINT('Ctrl Pts',(13.037381896984,1.02318586635016,26.6546265979024));
#49031=CARTESIAN_POINT('Ctrl Pts',(13.0692095056788,0.823831380843395,27.1261953032524));
#49032=CARTESIAN_POINT('Ctrl Pts',(13.1010371143736,0.422816177968262,27.4444814352468));
#49033=CARTESIAN_POINT('Ctrl Pts',(13.1328647230684,-0.0816976482255668,
27.531573650377));
#49034=CARTESIAN_POINT('Ctrl Pts',(13.1646923317632,-0.566213199612709,
27.3661531703238));
#49035=CARTESIAN_POINT('Ctrl Pts',(13.196519940458,-0.91212883520101,26.9887122771861));
#49036=CARTESIAN_POINT('Ctrl Pts',(13.2283475491529,-1.03476995185717,26.4916424518474));
#49037=CARTESIAN_POINT('Ctrl Pts',(13.2601751578477,-0.904115969959171,
25.9966184203386));
#49038=CARTESIAN_POINT('Ctrl Pts',(13.2920027665425,-0.552148890107181,
25.6248141311521));
#49039=CARTESIAN_POINT('Ctrl Pts',(13.3238303752373,-0.0650246119955593,
25.4672413148695));
#49040=CARTESIAN_POINT('Ctrl Pts',(13.3556579839321,0.438016648894992,25.5624712712837));
#49041=CARTESIAN_POINT('Ctrl Pts',(13.3874855926269,0.833838454822538,25.887193233444));
#49042=CARTESIAN_POINT('Ctrl Pts',(13.4193132013218,1.02554997206856,26.3619204697727));
#49043=CARTESIAN_POINT('Ctrl Pts',(13.4511408100166,0.966223294031546,26.8704473619132));
#49044=CARTESIAN_POINT('Ctrl Pts',(13.4829684187114,0.670380640585883,27.2882946775193));
#49045=CARTESIAN_POINT('Ctrl Pts',(13.5147960274062,0.210439551423907,27.5131800911359));
#49046=CARTESIAN_POINT('Ctrl Pts',(13.546623636101,-0.301013766926736,27.4900552580529));
#49047=CARTESIAN_POINT('Ctrl Pts',(13.5784512447958,-0.738783739889328,
27.224580766756));
#49048=CARTESIAN_POINT('Ctrl Pts',(13.6102788534907,-0.995711294815304,
26.7817405175953));
#49049=CARTESIAN_POINT('Ctrl Pts',(13.6421064621855,-1.00890468438493,26.2699347055643));
#49050=CARTESIAN_POINT('Ctrl Pts',(13.6739340708803,-0.77513437829989,25.8144451900429));
#49051=CARTESIAN_POINT('Ctrl Pts',(13.7057616795751,-0.351623600536278,
25.526768503683));
#49052=CARTESIAN_POINT('Ctrl Pts',(13.7375892882699,0.157958998690607,25.4773232883211));
#49053=CARTESIAN_POINT('Ctrl Pts',(13.7694168969648,0.628875766860997,25.6782129401527));
#49054=CARTESIAN_POINT('Ctrl Pts',(13.8012445056596,0.94585382714805,26.0802628923397));
#49055=CARTESIAN_POINT('Ctrl Pts',(13.8330721143544,1.03130203103048,26.5850577607866));
#49056=CARTESIAN_POINT('Ctrl Pts',(13.8648997230492,0.864304027792048,27.0690318527289));
#49057=CARTESIAN_POINT('Ctrl Pts',(13.896727331744,0.485738251922189,27.4137160677679));
#49058=CARTESIAN_POINT('Ctrl Pts',(13.9285549404388,-0.0117284624329275,
27.5347372347831));
#49059=CARTESIAN_POINT('Ctrl Pts',(13.9603825491336,-0.506324237172425,
27.4024713118595));
#49060=CARTESIAN_POINT('Ctrl Pts',(13.9922101578285,-0.876979954196896,
27.0492948769235));
#49061=CARTESIAN_POINT('Ctrl Pts',(14.0240377665233,-1.03296503498029,26.5616598604102));
#49062=CARTESIAN_POINT('Ctrl Pts',(14.0558653752181,-0.936096831931118,
26.0589314983745));
#49063=CARTESIAN_POINT('Ctrl Pts',(14.0876929839129,-0.610087128517846,
25.6641696359342));
#49064=CARTESIAN_POINT('Ctrl Pts',(14.1195205926077,-0.13473787473667,25.474005649631));
#49065=CARTESIAN_POINT('Ctrl Pts',(14.1513482013026,0.373593051153504,25.5349886352962));
#49066=CARTESIAN_POINT('Ctrl Pts',(14.1831758099974,0.790474386203466,25.8321909354959));
#49067=CARTESIAN_POINT('Ctrl Pts',(14.2150034186922,1.01386026151516,26.2928621908052));
#49068=CARTESIAN_POINT('Ctrl Pts',(14.246831027387,0.989069395320457,26.8042374617269));
#49069=CARTESIAN_POINT('Ctrl Pts',(14.2786586360818,0.72217019430702,27.2411402784441));
#49070=CARTESIAN_POINT('Ctrl Pts',(14.3104862447766,0.278495304927702,27.4966238342578));
#49071=CARTESIAN_POINT('Ctrl Pts',(14.3423138534715,-0.233350771276214,
27.5081498496863));
#49072=CARTESIAN_POINT('Ctrl Pts',(14.3741414621663,-0.688076318900794,
27.2728969408954));
#49073=CARTESIAN_POINT('Ctrl Pts',(14.4059690708611,-0.97437181239019,26.8484512492403));
#49074=CARTESIAN_POINT('Ctrl Pts',(14.4377966795559,-1.02215670378408,26.3387102768714));
#49075=CARTESIAN_POINT('Ctrl Pts',(14.4696242882507,-0.819734017582471,
25.8684504435156));
#49076=CARTESIAN_POINT('Ctrl Pts',(14.5014518969455,-0.416653582864778,
25.5527838188863));
#49077=CARTESIAN_POINT('Ctrl Pts',(14.5332795056404,0.0884169706665388,
25.4689805330763));
#49078=CARTESIAN_POINT('Ctrl Pts',(14.5651071143352,0.57184446695731,25.6375542872227));
#49079=CARTESIAN_POINT('Ctrl Pts',(14.59693472303,0.915293603463237,26.0172409282707));
#49080=CARTESIAN_POINT('Ctrl Pts',(14.6287623317248,1.03469353649247,26.5150992522442));
#49081=CARTESIAN_POINT('Ctrl Pts',(14.6605899404196,0.900817076223997,27.0092615212843));
#49082=CARTESIAN_POINT('Ctrl Pts',(14.6924175491145,0.546435034312068,27.3787647325388));
#49083=CARTESIAN_POINT('Ctrl Pts',(14.7242451578093,0.0582944544554268,
27.5331604224211));
#49084=CARTESIAN_POINT('Ctrl Pts',(14.7560727665041,-0.444115673487672,
27.4346550007571));
#49085=CARTESIAN_POINT('Ctrl Pts',(14.7879003751989,-0.837813403004803,
27.1073610158902));
#49086=CARTESIAN_POINT('Ctrl Pts',(14.8197279838937,-1.02642784023727,26.6313947893315));
#49087=CARTESIAN_POINT('Ctrl Pts',(14.8515555925885,-0.963789194129796,
26.1232652243869));
#49088=CARTESIAN_POINT('Ctrl Pts',(14.8833832012833,-0.665230401255004,
25.7073542940735));
#49089=CARTESIAN_POINT('Ctrl Pts',(14.9152108099782,-0.203833868702235,
25.4854703277639));
#49090=CARTESIAN_POINT('Ctrl Pts',(14.947038418673,0.307457927787168,25.5119269639756));
#49091=CARTESIAN_POINT('Ctrl Pts',(14.9788660273678,0.743488951599186,25.7802480422204));
#49092=CARTESIAN_POINT('Ctrl Pts',(15.0106936360626,0.997525796964821,26.2247528632895));
#49093=CARTESIAN_POINT('Ctrl Pts',(15.0425212447574,1.00738431593138,26.7366337716664));
#49094=CARTESIAN_POINT('Ctrl Pts',(15.0743488534523,0.770651301071694,27.1905905255896));
#49095=CARTESIAN_POINT('Ctrl Pts',(15.1061764621471,0.345275199982537,27.4755017878787));
#49096=CARTESIAN_POINT('Ctrl Pts',(15.1380040708419,-0.164618735868749,
27.5216258481844));
#49097=CARTESIAN_POINT('Ctrl Pts',(15.1698316795367,-0.634216643746959,
27.3176722758367));
#49098=CARTESIAN_POINT('Ctrl Pts',(15.2016592882315,-0.94856848268563,26.9135656363059));
#49099=CARTESIAN_POINT('Ctrl Pts',(15.2334868969263,-1.03072596105555,26.4082247577844));
#49100=CARTESIAN_POINT('Ctrl Pts',(15.2653145056211,-0.860578245001017,
25.9253489875511));
#49101=CARTESIAN_POINT('Ctrl Pts',(15.297142114316,-0.47977476822413,25.5831385744546));
#49102=CARTESIAN_POINT('Ctrl Pts',(15.3289697230108,0.0184698818135679,
25.465361142551));
#49103=CARTESIAN_POINT('Ctrl Pts',(15.3607973317056,0.512193400825138,25.6008467193916));
#49104=CARTESIAN_POINT('Ctrl Pts',(15.3926249404004,0.880540184932533,25.9564306073769));
#49105=CARTESIAN_POINT('Ctrl Pts',(15.4244525490953,1.03334484537939,26.445071570153));
#49106=CARTESIAN_POINT('Ctrl Pts',(15.4562801577901,0.933203250495736,26.9471581321432));
#49107=CARTESIAN_POINT('Ctrl Pts',(15.4881077664849,0.604628457604007,27.3397875505942));
#49108=CARTESIAN_POINT('Ctrl Pts',(15.5199353751797,0.128050309490577,27.526850437073));
#49109=CARTESIAN_POINT('Ctrl Pts',(15.5517629838745,-0.379872501950287,
27.4625567952799));
#49110=CARTESIAN_POINT('Ctrl Pts',(15.5835905925693,-0.79480861364516,27.1626446782048));
#49111=CARTESIAN_POINT('Ctrl Pts',(15.6154182012641,-1.01518831619457,26.7005277650094));
#49112=CARTESIAN_POINT('Ctrl Pts',(15.647245809959,-0.987066190738606,26.18932486907));
#49113=CARTESIAN_POINT('Ctrl Pts',(15.6790734186538,-0.717326082837455,
25.7541702655708));
#49114=CARTESIAN_POINT('Ctrl Pts',(15.7109010273486,-0.271996047415024,
25.501582826636));
#49115=CARTESIAN_POINT('Ctrl Pts',(15.7427286360434,0.239914260765304,25.4933919087554));
#49116=CARTESIAN_POINT('Ctrl Pts',(15.7745562447382,0.693097403341301,25.7316025173394));
#49117=CARTESIAN_POINT('Ctrl Pts',(15.8063838534331,0.976621410790803,26.1579045135308));
#49118=CARTESIAN_POINT('Ctrl Pts',(15.8382114621279,1.0210841505137,26.6679460015818));
#49119=CARTESIAN_POINT('Ctrl Pts',(15.8700390708227,0.815601856490434,27.1368770003439));
#49120=CARTESIAN_POINT('Ctrl Pts',(15.9018666795175,0.410473300754662,27.4499107175125));
#49121=CARTESIAN_POINT('Ctrl Pts',(15.9336942882123,-0.0951325397939341,
27.5304215165407));
#49122=CARTESIAN_POINT('Ctrl Pts',(15.9655218969071,-0.577451459419126,
27.3587016442818));
#49123=CARTESIAN_POINT('Ctrl Pts',(15.997349505602,-0.918419517375691,26.9767853730779));
#49124=CARTESIAN_POINT('Ctrl Pts',(16.0291771142968,-1.03457319823305,26.4781596846298));
#49125=CARTESIAN_POINT('Ctrl Pts',(16.0610047229916,-0.89747994266978,25.9848801553201));
#49126=CARTESIAN_POINT('Ctrl Pts',(16.0928323316864,-0.540697982268354,
25.617693707464));
#49127=CARTESIAN_POINT('Ctrl Pts',(16.1246599403813,-0.0515618223070227,
25.4664816981021));
#49128=CARTESIAN_POINT('Ctrl Pts',(16.156487549076,0.450195845303856,25.5682584034461));
#49129=CARTESIAN_POINT('Ctrl Pts',(16.1883151577709,0.841752785883323,25.8981105173412));
#49130=CARTESIAN_POINT('Ctrl Pts',(16.2201427664656,1.0272621363913,26.3752955292926));
#49131=CARTESIAN_POINT('Ctrl Pts',(16.2519703751605,0.961314181233222,26.8830061968657));
#49132=CARTESIAN_POINT('Ctrl Pts',(16.2837979838553,0.660051922794526,27.2969630864054));
#49133=CARTESIAN_POINT('Ctrl Pts',(16.3156255925501,0.197219533202479,27.5158361864007));
#49134=CARTESIAN_POINT('Ctrl Pts',(16.3474532012449,-0.313889037012783,
27.4860488701483));
#49135=CARTESIAN_POINT('Ctrl Pts',(16.3792808099398,-0.748162602092337,
27.2148925952254));
#49136=CARTESIAN_POINT('Ctrl Pts',(16.4111084186346,-0.999297953995706,
26.7687420715437));
#49137=CARTESIAN_POINT('Ctrl Pts',(16.4429360273294,-1.0058211838636,26.2568077962417));
#49138=CARTESIAN_POINT('Ctrl Pts',(16.4747636360242,-0.766135509581008,
25.8044030744485));
#49139=CARTESIAN_POINT('Ctrl Pts',(16.506591244719,-0.33891214244517,25.5222693307557));
#49140=CARTESIAN_POINT('Ctrl Pts',(16.5384188534138,0.171271484957023,25.4794683834794));
#49141=CARTESIAN_POINT('Ctrl Pts',(16.5702464621087,0.639530598041916,25.6864772184838));
#49142=CARTESIAN_POINT('Ctrl Pts',(16.6020740708035,0.951242871349886,26.0926233909713));
#49143=CARTESIAN_POINT('Ctrl Pts',(16.6339016794983,1.03010613661001,26.5984888277719));
#49144=CARTESIAN_POINT('Ctrl Pts',(16.6657292881931,0.856815930535437,27.080245778148));
#49145=CARTESIAN_POINT('Ctrl Pts',(16.6975568968879,0.473790918015481,27.4199678624187));
#49146=CARTESIAN_POINT('Ctrl Pts',(16.7293845055828,-0.0252105171445776,
27.5344965595417));
#49147=CARTESIAN_POINT('Ctrl Pts',(16.7612121142776,-0.518040821792485,
27.3957970801659));
#49148=CARTESIAN_POINT('Ctrl Pts',(16.7930397229724,-0.884063036604701,
27.0378208337223));
#49149=CARTESIAN_POINT('Ctrl Pts',(16.8248673316672,-1.0336807901387,26.5481946675613));
#49150=CARTESIAN_POINT('Ctrl Pts',(16.856694940362,-0.930270054438158,26.0467712192733));
#49151=CARTESIAN_POINT('Ctrl Pts',(16.8885225490569,-0.599144120132018,
25.6562909119748));
#49152=CARTESIAN_POINT('Ctrl Pts',(16.9203501577516,-0.121357308471081,
25.4723370661945));
#49153=CARTESIAN_POINT('Ctrl Pts',(16.9521777664465,0.386135827067481,25.5399386347901));
#49154=CARTESIAN_POINT('Ctrl Pts',(16.9840053751413,0.799109101409514,25.8425478375223));
#49155=CARTESIAN_POINT('Ctrl Pts',(17.0158329838361,1.0164732758529,26.3060907914917));
#49156=CARTESIAN_POINT('Ctrl Pts',(17.0476605925309,0.985021085287657,26.8170996121502));
#49157=CARTESIAN_POINT('Ctrl Pts',(17.0794882012258,0.712451520320007,27.2504875294108));
#49158=CARTESIAN_POINT('Ctrl Pts',(17.1113158099206,0.265485244477138,27.5001681303059));
#49159=CARTESIAN_POINT('Ctrl Pts',(17.1431434186154,-0.246467567458505,
27.5050236006414));
#49160=CARTESIAN_POINT('Ctrl Pts',(17.1749710273102,-0.698089062672224,
27.2638654086669));
#49161=CARTESIAN_POINT('Ctrl Pts',(17.206798636005,-0.97882955717243,26.8357251963527));
#49162=CARTESIAN_POINT('Ctrl Pts',(17.2386262446998,-1.01996824129622,26.3254048593828));
#49163=CARTESIAN_POINT('Ctrl Pts',(17.2704538533946,-0.811435093319473,
25.8578225722776));
#49164=CARTESIAN_POINT('Ctrl Pts',(17.3022814620895,-0.404275555583194,
25.5474351058964));
#49165=CARTESIAN_POINT('Ctrl Pts',(17.3341090707843,0.101843998007599,25.4702201074962));
#49166=CARTESIAN_POINT('Ctrl Pts',(17.3659366794791,0.583034075919173,25.6450790044221));
#49167=CARTESIAN_POINT('Ctrl Pts',(17.3977642881739,0.921506185674827,26.0292083231239));
#49168=CARTESIAN_POINT('Ctrl Pts',(17.4295918968687,1.03440943041633,26.5285809084295));
#49169=CARTESIAN_POINT('Ctrl Pts',(17.4614195055636,0.894103789082602,27.0209554381429));
#49170=CARTESIAN_POINT('Ctrl Pts',(17.4932471142584,0.534939718203638,27.3858120280539));
#49171=CARTESIAN_POINT('Ctrl Pts',(17.5250747229532,0.0448237145771032,
27.5338292314391));
#49172=CARTESIAN_POINT('Ctrl Pts',(17.556902331648,-0.456250700141257,27.4287944496501));
#49173=CARTESIAN_POINT('Ctrl Pts',(17.5887299403428,-0.845668154601334,
27.096381428918));
#49174=CARTESIAN_POINT('Ctrl Pts',(17.6205575490376,-1.02803069848662,26.6180295723256));
#49175=CARTESIAN_POINT('Ctrl Pts',(17.6523851577325,-0.958840139662527,
26.1106995285693));
#49176=CARTESIAN_POINT('Ctrl Pts',(17.6842127664273,-0.654766539896501,
25.6988272140803));
#49177=CARTESIAN_POINT('Ctrl Pts',(17.7160403751221,-0.190745755648998,
25.4827609916589));
#49178=CARTESIAN_POINT('Ctrl Pts',(17.7478679838169,0.320587858023884,25.5162803182649));
#49179=CARTESIAN_POINT('Ctrl Pts',(17.7796955925117,0.752275258385287,25.7895010885325));
#49180=CARTESIAN_POINT('Ctrl Pts',(17.8115232012066,1.00201539234692,26.2387037897642));
#49181=CARTESIAN_POINT('Ctrl Pts',(17.8433508099014,1.00244486581897,26.7480441021986));
#49182=CARTESIAN_POINT('Ctrl Pts',(17.8857876214945,0.684775665170146,27.3550858372652));
#49183=CARTESIAN_POINT('Ctrl Pts',(17.9388336359858,-0.201818282340762,
27.6563391975183));
#49184=CARTESIAN_POINT('Ctrl Pts',(17.9918796504772,-0.933946851652724,
27.0725668336436));
#49185=CARTESIAN_POINT('Ctrl Pts',(18.0343164620703,-1.02720218653396,26.3938055857297));
#49186=CARTESIAN_POINT('Ctrl Pts',(18.0661440707651,-0.854261376904684,
25.9147239489671));
#49187=CARTESIAN_POINT('Ctrl Pts',(18.0979716794599,-0.467120983511694,
25.5766773292406));
#49188=CARTESIAN_POINT('Ctrl Pts',(18.1297992881547,0.0315965154626858,
25.4658420588924));
#49189=CARTESIAN_POINT('Ctrl Pts',(18.1616268968495,0.524053608104702,25.6075164095507));
#49190=CARTESIAN_POINT('Ctrl Pts',(18.1934545055444,0.887449122107085,25.9679933173937));
#49191=CARTESIAN_POINT('Ctrl Pts',(18.2252821142392,1.03402541318104,26.4585184935185));
#49192=CARTESIAN_POINT('Ctrl Pts',(18.257109722934,0.927269533067888,26.9592921837113));
#49193=CARTESIAN_POINT('Ctrl Pts',(18.2889373316288,0.593649090550186,27.3475884577754));
#49194=CARTESIAN_POINT('Ctrl Pts',(18.3207649403236,0.114651348604825,27.528435170219));
#49195=CARTESIAN_POINT('Ctrl Pts',(18.3525925490184,-0.392378625981908,
27.45752339869));
#49196=CARTESIAN_POINT('Ctrl Pts',(18.3844201577133,-0.803377856520256,
27.1522326814947));
#49197=CARTESIAN_POINT('Ctrl Pts',(18.416247766408,-1.01771392660482,26.6872819205827));
#49198=CARTESIAN_POINT('Ctrl Pts',(18.4480753751029,-0.982934779259867,
26.1764896326511));
#49199=CARTESIAN_POINT('Ctrl Pts',(18.4799029837977,-0.707546389749453,
25.7448863929147));
#49200=CARTESIAN_POINT('Ctrl Pts',(18.5117305924926,-0.258963342224468,
25.4981234458543));
#49201=CARTESIAN_POINT('Ctrl Pts',(18.5435582011873,0.253010499600352,25.496603511055));
#49202=CARTESIAN_POINT('Ctrl Pts',(18.5753858098822,0.703051045743631,25.7406991180043));
#49203=CARTESIAN_POINT('Ctrl Pts',(18.607213418577,0.980996166272481,26.1706593236401));
#49204=CARTESIAN_POINT('Ctrl Pts',(18.6390410272718,1.01880904226803,26.6812368940723));
#49205=CARTESIAN_POINT('Ctrl Pts',(18.6708686359666,0.807233851103414,27.1474505533964));
#49206=CARTESIAN_POINT('Ctrl Pts',(18.7026962446614,0.398060721868608,27.4551787077222));
#49207=CARTESIAN_POINT('Ctrl Pts',(18.7345238533562,-0.108551275958736,
27.5290944175065));
#49208=CARTESIAN_POINT('Ctrl Pts',(18.7663514620511,-0.58859166973049,27.351104312196));
#49209=CARTESIAN_POINT('Ctrl Pts',(18.7981790707459,-0.924554252459608,
26.9647775111451));
#49210=CARTESIAN_POINT('Ctrl Pts',(18.8300066794407,-1.03420077562692,26.4646806260004));
#49211=CARTESIAN_POINT('Ctrl Pts',(18.8618342881355,-0.890691524210388,
25.9732293569615));
#49212=CARTESIAN_POINT('Ctrl Pts',(18.8936618968303,-0.529155264648254,
25.6107230983562));
#49213=CARTESIAN_POINT('Ctrl Pts',(18.9254895055251,-0.038090277438839,
25.4658975714764));
#49214=CARTESIAN_POINT('Ctrl Pts',(18.95731711422,0.462298598977743,25.5742037442178));
#49215=CARTESIAN_POINT('Ctrl Pts',(18.9891447229147,0.849524188348949,25.9091300013411));
#49216=CARTESIAN_POINT('Ctrl Pts',(19.0209723316096,1.02879987283589,26.3886917634842));
#49217=CARTESIAN_POINT('Ctrl Pts',(19.0527999403044,0.956241838450062,26.8954999978265));
#49218=CARTESIAN_POINT('Ctrl Pts',(19.0846275489993,0.649611128981037,27.3054961719217));
#49219=CARTESIAN_POINT('Ctrl Pts',(19.116455157694,0.183966027343174,27.518319793906));
#49220=CARTESIAN_POINT('Ctrl Pts',(19.1482827663889,-0.326711009119531,
27.4818750523353));
#49221=CARTESIAN_POINT('Ctrl Pts',(19.1801103750837,-0.757414427187756,
27.2050830357943));
#49222=CARTESIAN_POINT('Ctrl Pts',(19.2119379837785,-1.00271493358913,26.7556979934127));
#49223=CARTESIAN_POINT('Ctrl Pts',(19.2437655924733,-1.00256689611852,26.2437221806618));
#49224=CARTESIAN_POINT('Ctrl Pts',(19.2755932011681,-0.757006551976856,
25.7944790703729));
#49225=CARTESIAN_POINT('Ctrl Pts',(19.307420809863,-0.326143137481079,25.5179361753167));
#49226=CARTESIAN_POINT('Ctrl Pts',(19.3392484185578,0.184554889531876,25.481786763675));
#49227=CARTESIAN_POINT('Ctrl Pts',(19.3710760272526,0.650076837698819,25.694879632002));
#49228=CARTESIAN_POINT('Ctrl Pts',(19.4029036359474,0.956470395659613,26.1050530616598));
#49229=CARTESIAN_POINT('Ctrl Pts',(19.4347312446422,1.0287353314103,26.6119031714732));
#49230=CARTESIAN_POINT('Ctrl Pts',(19.466558853337,0.849182346967171,27.0913611785339));
#49231=CARTESIAN_POINT('Ctrl Pts',(19.4983864620319,0.46176313498287,27.4260634476365));
#49232=CARTESIAN_POINT('Ctrl Pts',(19.5302140707267,-0.038688291141642,
27.5340802280318));
#49233=CARTESIAN_POINT('Ctrl Pts',(19.5620416794215,-0.529669443704362,
27.3889707432101));
#49234=CARTESIAN_POINT('Ctrl Pts',(19.5938692881163,-0.890996006178292,
27.0262554691896));
#49235=CARTESIAN_POINT('Ctrl Pts',(19.6256968968112,-1.03422102754035,26.5347212913211));
#49236=CARTESIAN_POINT('Ctrl Pts',(19.6575245055059,-0.924285318222643,
26.0346878978624));
#49237=CARTESIAN_POINT('Ctrl Pts',(19.6893521142008,-0.588099377777535,
25.6485554488193));
#49238=CARTESIAN_POINT('Ctrl Pts',(19.7211797228956,-0.10795613591828,25.4708429786494));
#49239=CARTESIAN_POINT('Ctrl Pts',(19.7530073315904,0.398613037654465,25.5450516516117));
#49240=CARTESIAN_POINT('Ctrl Pts',(19.7848349402852,0.8076081287208,25.853016374008));
#49241=CARTESIAN_POINT('Ctrl Pts',(19.8166625489801,1.01891369450633,26.3193523179637));
#49242=CARTESIAN_POINT('Ctrl Pts',(19.8484901576748,0.980805519387458,26.8299079189967));
#49243=CARTESIAN_POINT('Ctrl Pts',(19.8803177663697,0.702611873821896,27.2597073493406));
#49244=CARTESIAN_POINT('Ctrl Pts',(19.9121453750645,0.252430103257493,27.5035425974252));
#49245=CARTESIAN_POINT('Ctrl Pts',(19.9439729837593,-0.259542510544956,
27.5017267027975));
#49246=CARTESIAN_POINT('Ctrl Pts',(19.9758005924541,-0.70798327780557,27.2547041673565));
#49247=CARTESIAN_POINT('Ctrl Pts',(20.0076282011489,-0.983121086466923,
26.8229421484132));
#49248=CARTESIAN_POINT('Ctrl Pts',(20.0394558098438,-1.01760661097527,26.3121290677698));
#49249=CARTESIAN_POINT('Ctrl Pts',(20.0712834185386,-0.802998347677216,
25.8473037800743));
#49250=CARTESIAN_POINT('Ctrl Pts',(20.1031110272334,-0.391828959610619,
25.5422480653697));
#49251=CARTESIAN_POINT('Ctrl Pts',(20.1349386359282,0.115253877394866,25.4716346730743));
#49252=CARTESIAN_POINT('Ctrl Pts',(20.1667662446231,0.594124412544197,25.6527486298054));
#49253=CARTESIAN_POINT('Ctrl Pts',(20.1985938533178,0.927562814339893,26.0412561419142));
#49254=CARTESIAN_POINT('Ctrl Pts',(20.2304214620127,1.03394870649155,26.5420567975728));
#49255=CARTESIAN_POINT('Ctrl Pts',(20.2622490707075,0.887240527791323,27.0325626232869));
#49256=CARTESIAN_POINT('Ctrl Pts',(20.2940766794023,0.523350088894221,27.3927056549233));
#49257=CARTESIAN_POINT('Ctrl Pts',(20.3259042880971,0.0313519366769965,
27.534328650838));
#49258=CARTESIAN_POINT('Ctrl Pts',(20.3577318967919,-0.468320667118775,
27.4227645716146));
#49259=CARTESIAN_POINT('Ctrl Pts',(20.3895595054867,-0.853355878013929,
27.0853225156584));
#49260=CARTESIAN_POINT('Ctrl Pts',(20.4213871141815,-1.0295032478625,26.6046028896263));
#49261=CARTESIAN_POINT('Ctrl Pts',(20.4532147228764,-0.953644723878202,
26.098278152826));
#49262=CARTESIAN_POINT('Ctrl Pts',(20.4850423315712,-0.644349256845004,
25.6902884852733));
#49263=CARTESIAN_POINT('Ctrl Pts',(20.516869940266,-0.177327419594983,25.4805032181819));
#49264=CARTESIAN_POINT('Ctrl Pts',(20.5486975489608,0.333101327705005,25.5202744224229));
#49265=CARTESIAN_POINT('Ctrl Pts',(20.5805251576557,0.761992209049242,25.7998667446651));
#49266=CARTESIAN_POINT('Ctrl Pts',(20.6123527663505,1.0043596111001,26.2508404658286));
#49267=CARTESIAN_POINT('Ctrl Pts',(20.6441803750453,1.00087587858637,26.7628044473398));
#49268=CARTESIAN_POINT('Ctrl Pts',(20.6760079837401,0.752393773388913,27.2104381124652));
#49269=CARTESIAN_POINT('Ctrl Pts',(20.7078355924349,0.319737732100598,27.4841679148137));
#49270=CARTESIAN_POINT('Ctrl Pts',(20.7396632011297,-0.191184981135965,
27.5169891862088));
#49271=CARTESIAN_POINT('Ctrl Pts',(20.7714908098246,-0.655308675371252,
27.300867805484));
#49272=CARTESIAN_POINT('Ctrl Pts',(20.8033184185194,-0.959023309395961,
26.8887068225705));
#49273=CARTESIAN_POINT('Ctrl Pts',(20.8351460272142,-1.02798440884689,26.3813966398228));
#49274=CARTESIAN_POINT('Ctrl Pts',(20.866973635909,-0.84531140191147,25.9031186586296));
#49275=CARTESIAN_POINT('Ctrl Pts',(20.8988012446038,-0.45571971273963,25.5709476627777));
#49276=CARTESIAN_POINT('Ctrl Pts',(20.9306288532986,0.0454248576733852,
25.4661937878969));
#49277=CARTESIAN_POINT('Ctrl Pts',(20.9624564619935,0.535450151013717,25.6144991035256));
#49278=CARTESIAN_POINT('Ctrl Pts',(20.9942840706883,0.894405829771168,25.9795608454882));
#49279=CARTESIAN_POINT('Ctrl Pts',(21.0261116793831,1.03442529725508,26.4720177506916));
#49280=CARTESIAN_POINT('Ctrl Pts',(21.0579392880779,0.921234032107172,26.9713242620163));
#49281=CARTESIAN_POINT('Ctrl Pts',(21.0897668967727,0.582539441765831,27.3552581485521));
#49282=CARTESIAN_POINT('Ctrl Pts',(21.1215945054676,0.101248533229376,27.5298385487039));
#49283=CARTESIAN_POINT('Ctrl Pts',(21.1534221141624,-0.404826393394172,
27.4523309787512));
#49284=CARTESIAN_POINT('Ctrl Pts',(21.1852497228572,-0.811806307616102,
27.1417080494994));
#49285=CARTESIAN_POINT('Ctrl Pts',(21.217077331552,-1.02006904965355,26.6740052752549));
#49286=CARTESIAN_POINT('Ctrl Pts',(21.2489049402468,-0.978635238364995,
26.1637087986463));
#49287=CARTESIAN_POINT('Ctrl Pts',(21.2807325489416,-0.697647206638017,
25.7357310179343));
#49288=CARTESIAN_POINT('Ctrl Pts',(21.3125601576365,-0.245886320863374,
25.4948340340571));
#49289=CARTESIAN_POINT('Ctrl Pts',(21.3443877663313,0.266063595105304,25.4999855674855));
#49290=CARTESIAN_POINT('Ctrl Pts',(21.3762153750261,0.712885407554046,25.7499246054068));
#49291=CARTESIAN_POINT('Ctrl Pts',(21.4080429837209,0.985204298614172,26.1834700774496));
#49292=CARTESIAN_POINT('Ctrl Pts',(21.4398705924157,1.01636096857812,26.6944970010786));
#49293=CARTESIAN_POINT('Ctrl Pts',(21.4716982011106,0.79872876402887,27.1579141763107));
#49294=CARTESIAN_POINT('Ctrl Pts',(21.5035258098053,0.385580560353784,27.460284506464));
#49295=CARTESIAN_POINT('Ctrl Pts',(21.5353534185002,-0.121951584273673,
27.5275925812163));
#49296=CARTESIAN_POINT('Ctrl Pts',(21.567181027195,-0.599631935754259,27.3433624627058));
#49297=CARTESIAN_POINT('Ctrl Pts',(21.5990086358898,-0.930532000475933,
26.9526907310382));
#49298=CARTESIAN_POINT('Ctrl Pts',(21.6308362445846,-1.03365274637864,26.4512075643002));
#49299=CARTESIAN_POINT('Ctrl Pts',(21.6626638532794,-0.883751867721363,
25.9616680037592));
#49300=CARTESIAN_POINT('Ctrl Pts',(21.6944914619742,-0.517522696934846,
25.6039034873213));
#49301=CARTESIAN_POINT('Ctrl Pts',(21.7263190706691,-0.024612264976355,
25.4654890342339));
#49302=CARTESIAN_POINT('Ctrl Pts',(21.7581466793639,0.47432285495422,25.5803062840566));
#49303=CARTESIAN_POINT('Ctrl Pts',(21.7899742880587,0.857151342607267,25.9202498143647));
#49304=CARTESIAN_POINT('Ctrl Pts',(21.8218018967535,1.03016292031633,26.4021068976742));
#49305=CARTESIAN_POINT('Ctrl Pts',(21.8536295054483,0.951007126949275,26.9079266433678));
#49306=CARTESIAN_POINT('Ctrl Pts',(21.8854571141432,0.639060031985187,27.313892485158));
#49307=CARTESIAN_POINT('Ctrl Pts',(21.917284722838,0.170681284272388,27.5206304919396));
#49308=CARTESIAN_POINT('Ctrl Pts',(21.9491123315328,-0.339477506090018,
27.4775345133224));
#49309=CARTESIAN_POINT('Ctrl Pts',(21.9809399402276,-0.766537644227681,
27.1951537541145));
#49310=CARTESIAN_POINT('Ctrl Pts',(22.0127675489225,-1.00596165339614,26.7426104980707));
#49311=CARTESIAN_POINT('Ctrl Pts',(22.0445951576172,-0.999142373724045,
26.2306800807465));
#49312=CARTESIAN_POINT('Ctrl Pts',(22.0764227663121,-0.74774905557329,25.7846748629002));
#49313=CARTESIAN_POINT('Ctrl Pts',(22.1082503750069,-0.313318753805751,
25.5137697731304));
#49314=CARTESIAN_POINT('Ctrl Pts',(22.1400779837017,0.19780695690913,25.4842780352498));
#49315=CARTESIAN_POINT('Ctrl Pts',(22.1719055923965,0.660512695092847,25.7034187539875));
#49316=CARTESIAN_POINT('Ctrl Pts',(22.2037332010913,0.961535512449999,26.1175497938618));
#49317=CARTESIAN_POINT('Ctrl Pts',(22.2355608097862,1.02718984819223,26.625298514151));
#49318=CARTESIAN_POINT('Ctrl Pts',(22.267388418481,0.841404573260887,27.102376166505));
#49319=CARTESIAN_POINT('Ctrl Pts',(22.2992160271758,0.449656945126742,27.4320017883979));
#49320=CARTESIAN_POINT('Ctrl Pts',(22.3310436358706,-0.0521594959131353,
27.5334883109468));
#49321=CARTESIAN_POINT('Ctrl Pts',(22.3628712445654,-0.541208128384414,
27.3819934600938));
#49322=CARTESIAN_POINT('Ctrl Pts',(22.3946988532602,-0.897777685703373,
27.0146007471144));
#49323=CARTESIAN_POINT('Ctrl Pts',(22.426526461955,-1.03458565546189,26.521242019445));
#49324=CARTESIAN_POINT('Ctrl Pts',(22.4583540706499,-0.918143639469846,
26.0226835858901));
#49325=CARTESIAN_POINT('Ctrl Pts',(22.4901816793447,-0.576954776868062,
25.6409645599122));
#49326=CARTESIAN_POINT('Ctrl Pts',(22.5220092880395,-0.0945366325251403,
25.4695236407426));
#49327=CARTESIAN_POINT('Ctrl Pts',(22.5538368967343,0.4110225641932,25.5503268174779));
#49328=CARTESIAN_POINT('Ctrl Pts',(22.5856645054292,0.815970025212737,25.8635947675954));
#49329=CARTESIAN_POINT('Ctrl Pts',(22.6174921141239,1.0211811027177,26.3326445180763));
#49330=CARTESIAN_POINT('Ctrl Pts',(22.6493197228188,0.976423414130928,26.8426602080991));
#49331=CARTESIAN_POINT('Ctrl Pts',(22.6811473315136,0.692652924226338,27.2687981714588));
#49332=CARTESIAN_POINT('Ctrl Pts',(22.7129749402084,0.239332100558325,27.5067466650155));
#49333=CARTESIAN_POINT('Ctrl Pts',(22.7448025489032,-0.272573385226417,
27.4982597114699));
#49334=CARTESIAN_POINT('Ctrl Pts',(22.7766301575981,-0.717757275210811,
27.2454147810176));
#49335=CARTESIAN_POINT('Ctrl Pts',(22.8084577662928,-0.987245688692236,
26.8101042599453));
#49336=CARTESIAN_POINT('Ctrl Pts',(22.8402853749877,-1.01507218150648,26.2988851864996));
#49337=CARTESIAN_POINT('Ctrl Pts',(22.8721129836825,-0.794425274225543,
25.8368957958591));
#49338=CARTESIAN_POINT('Ctrl Pts',(22.9039405923773,-0.379315793144767,
25.5372236859226));
#49339=CARTESIAN_POINT('Ctrl Pts',(22.9357682010721,0.128644114289536,25.4732237859512));
#49340=CARTESIAN_POINT('Ctrl Pts',(22.967595809767,0.605114004499334,25.6605622456451));
#49341=CARTESIAN_POINT('Ctrl Pts',(22.9994234184617,0.933461685389972,26.0533816127984));
#49342=CARTESIAN_POINT('Ctrl Pts',(23.0312510271566,1.03331290755272,26.5555260025805));
#49343=CARTESIAN_POINT('Ctrl Pts',(23.0630786358514,0.880225692253004,27.0440785169214));
#49344=CARTESIAN_POINT('Ctrl Pts',(23.0949062445462,0.511673336059915,27.3994493310037));
#49345=CARTESIAN_POINT('Ctrl Pts',(23.126733853241,0.0178715484813904,27.5346493655498));
#49346=CARTESIAN_POINT('Ctrl Pts',(23.1585614619359,-0.480304907713853,
27.4165838191369));
#49347=CARTESIAN_POINT('Ctrl Pts',(23.1903890706307,-0.860910420998461,
27.0741532451305));
#49348=CARTESIAN_POINT('Ctrl Pts',(23.2222166793255,-1.03077886220077,26.5911791594484));
#49349=CARTESIAN_POINT('Ctrl Pts',(23.2540442880203,-0.948329159626196,
26.0858858769852));
#49350=CARTESIAN_POINT('Ctrl Pts',(23.2858718967151,-0.63374367893186,25.6819610942678));
#49351=CARTESIAN_POINT('Ctrl Pts',(23.31769950541,-0.16402790350388,25.4782791238554));
#49352=CARTESIAN_POINT('Ctrl Pts',(23.3495271141047,0.345839273604333,25.5246980474179));
#49353=CARTESIAN_POINT('Ctrl Pts',(23.3813547227996,0.771050539768965,25.8098552564863));
#49354=CARTESIAN_POINT('Ctrl Pts',(23.4131823314944,1.00752099247019,26.2639488368816));
#49355=CARTESIAN_POINT('Ctrl Pts',(23.4450099401892,0.997366455119157,26.7758239584965));
#49356=CARTESIAN_POINT('Ctrl Pts',(23.476837548884,0.743072595698879,27.2201817960758));
#49357=CARTESIAN_POINT('Ctrl Pts',(23.5086651575788,0.306886475083116,27.4882506733054));
#49358=CARTESIAN_POINT('Ctrl Pts',(23.5404927662737,-0.204420535747526,
27.5144116257429));
#49359=CARTESIAN_POINT('Ctrl Pts',(23.5723203749685,-0.665688675952158,
27.2922608715484));
#49360=CARTESIAN_POINT('Ctrl Pts',(23.6041479836633,-0.964006898178333,
26.8761773546377));
#49361=CARTESIAN_POINT('Ctrl Pts',(23.6359755923581,-1.02635168317555,26.3680116508159));
#49362=CARTESIAN_POINT('Ctrl Pts',(23.6678032010529,-0.837462026860863,
25.8921545793183));
#49363=CARTESIAN_POINT('Ctrl Pts',(23.6996308097477,-0.44357508950957,25.5650883240412));
#49364=CARTESIAN_POINT('Ctrl Pts',(23.7314584184426,0.0588919199745167,
25.4668734619421));
#49365=CARTESIAN_POINT('Ctrl Pts',(23.7632860271374,0.54694313138947,25.6215514170406));
#49366=CARTESIAN_POINT('Ctrl Pts',(23.7951136358322,0.90111143083913,25.9912595051613));
#49367=CARTESIAN_POINT('Ctrl Pts',(23.826941244527,1.03470209535356,26.4854991121453));
#49368=CARTESIAN_POINT('Ctrl Pts',(23.8587688532218,0.915014271498275,26.9832883040506));
#49369=CARTESIAN_POINT('Ctrl Pts',(23.8905964619167,0.571345620154082,27.362776265441));
#49370=CARTESIAN_POINT('Ctrl Pts',(23.9224240706114,0.0878207187267834,
27.531070425936));
#49371=CARTESIAN_POINT('Ctrl Pts',(23.9542516793063,-0.417201287023148,
27.4469750725251));
#49372=CARTESIAN_POINT('Ctrl Pts',(23.9860792880011,-0.820099104760281,
27.1310753998129));
#49373=CARTESIAN_POINT('Ctrl Pts',(24.0179068966959,-1.02224980649195,26.6606985843273));
#49374=CARTESIAN_POINT('Ctrl Pts',(24.0497345053907,-0.974170140577519,
26.1509853311323));
#49375=CARTESIAN_POINT('Ctrl Pts',(24.0815621140856,-0.687629238594858,
25.7267052747451));
#49376=CARTESIAN_POINT('Ctrl Pts',(24.1133897227804,-0.232767720569937,
25.4917153724576));
#49377=CARTESIAN_POINT('Ctrl Pts',(24.1452173314752,0.279071604566762,25.5035373858483));
#49378=CARTESIAN_POINT('Ctrl Pts',(24.17704494017,0.722598673964357,25.7592774755263));
#49379=CARTESIAN_POINT('Ctrl Pts',(24.2088725488648,0.989245170043781,26.1963345666319));
#49380=CARTESIAN_POINT('Ctrl Pts',(24.2407001575596,1.01374030446957,26.7077240885684));
#49381=CARTESIAN_POINT('Ctrl Pts',(24.2725277662545,0.790088060951025,27.1682660830988));
#49382=CARTESIAN_POINT('Ctrl Pts',(24.3043553749492,0.373034923923842,27.465227251693));
#49383=CARTESIAN_POINT('Ctrl Pts',(24.3361829836441,-0.13533118334359,27.525916260078));
#49384=CARTESIAN_POINT('Ctrl Pts',(24.3680105923389,-0.610570386064801,
27.3354774117463));
#49385=CARTESIAN_POINT('Ctrl Pts',(24.3998382010337,-0.936351744716457,
26.9405270843479));
#49386=CARTESIAN_POINT('Ctrl Pts',(24.4316658097286,-1.03292920443998,26.4377427876258));
#49387=CARTESIAN_POINT('Ctrl Pts',(24.4634934184233,-0.876662151072909,
25.9501980586121));
#49388=CARTESIAN_POINT('Ctrl Pts',(24.4953210271182,-0.505802254575641,
25.5972360324294));
#49389=CARTESIAN_POINT('Ctrl Pts',(24.527148635813,-0.0111300733365206,
25.4652561556863));
#49390=CARTESIAN_POINT('Ctrl Pts',(24.5589762445079,0.486266571458613,25.5865649867891));
#49391=CARTESIAN_POINT('Ctrl Pts',(24.5908038532026,0.864632953614065,25.9314680682651));
#49392=CARTESIAN_POINT('Ctrl Pts',(24.6226314618975,1.031351047369,26.4155386539979));
#49393=CARTESIAN_POINT('Ctrl Pts',(24.6544590705922,0.945610935589058,26.9202840234556));
#49394=CARTESIAN_POINT('Ctrl Pts',(24.6862866792871,0.628400423364985,27.3221506004329));
#49395=CARTESIAN_POINT('Ctrl Pts',(24.7181142879819,0.157367559726439,27.5227678881464));
#49396=CARTESIAN_POINT('Ctrl Pts',(24.7499418966767,-0.352186360189988,
27.4730279901286));
#49397=CARTESIAN_POINT('Ctrl Pts',(24.7817695053715,-0.775530704100024,
27.1851064361658));
#49398=CARTESIAN_POINT('Ctrl Pts',(24.8135971140664,-1.00903756212806,26.7294818077589));
#49399=CARTESIAN_POINT('Ctrl Pts',(24.8454247227612,-0.995548198159715,
26.2176837110286));
#49400=CARTESIAN_POINT('Ctrl Pts',(24.877252331456,-0.73836459228214,25.7749921167727));
#49401=CARTESIAN_POINT('Ctrl Pts',(24.9090799401508,-0.300441168983939,
25.5097708316469));
#49402=CARTESIAN_POINT('Ctrl Pts',(24.9409075488456,0.211025436903717,25.486941775189));
#49403=CARTESIAN_POINT('Ctrl Pts',(24.9727351575404,0.670836398228031,25.7120931345076));
#49404=CARTESIAN_POINT('Ctrl Pts',(25.0045627662353,0.966437361670276,26.1301114656476));
#49405=CARTESIAN_POINT('Ctrl Pts',(25.0363903749301,1.02546994937707,26.6386725812921));
#49406=CARTESIAN_POINT('Ctrl Pts',(25.0682179836249,0.833483930073081,27.1132888717298));
#49407=CARTESIAN_POINT('Ctrl Pts',(25.1000455923197,0.437474404063782,27.4377818763799));
#49408=CARTESIAN_POINT('Ctrl Pts',(25.1318732010145,-0.0656218440651441,
27.5327209087934));
#49409=CARTESIAN_POINT('Ctrl Pts',(25.1637008097093,-0.552654916577154,
27.3748664155519));
#49410=CARTESIAN_POINT('Ctrl Pts',(25.1955284184042,-0.90440692366044,27.0028586464532));
#49411=CARTESIAN_POINT('Ctrl Pts',(25.227356027099,-1.03477461198718,26.5077591406996));
#49412=CARTESIAN_POINT('Ctrl Pts',(25.2591836357938,-0.911846061034622,
26.0107603216692));
#49413=CARTESIAN_POINT('Ctrl Pts',(25.2910112444886,-0.56571220973346,25.6335195341866));
#49414=CARTESIAN_POINT('Ctrl Pts',(25.3228388531834,-0.0811010769258508,
25.4683792764785));
#49415=CARTESIAN_POINT('Ctrl Pts',(25.3546664618783,0.423362299596309,25.5557632367048));
#49416=CARTESIAN_POINT('Ctrl Pts',(25.386494070573,0.824193370978722,25.8742812220235));
#49417=CARTESIAN_POINT('Ctrl Pts',(25.4183216792679,1.02327511560964,26.3459651349479));
#49418=CARTESIAN_POINT('Ctrl Pts',(25.4501492879627,0.971875513356643,26.8553543139117));
#49419=CARTESIAN_POINT('Ctrl Pts',(25.4819768966576,0.682576362999678,27.2777584525745));
#49420=CARTESIAN_POINT('Ctrl Pts',(25.5138045053523,0.226193459557492,27.5097797882372));
#49421=CARTESIAN_POINT('Ctrl Pts',(25.5456321140472,-0.285557977276429,
27.4946232168462));
#49422=CARTESIAN_POINT('Ctrl Pts',(25.5774597227419,-0.727409398295521,
27.2359988241503));
#49423=CARTESIAN_POINT('Ctrl Pts',(25.6092873314368,-0.991202657792454,
26.7972137161442));
#49424=CARTESIAN_POINT('Ctrl Pts',(25.6411149401316,-1.01236539400214,26.2856754542898));
#49425=CARTESIAN_POINT('Ctrl Pts',(25.6729425488264,-0.785717308327549,
25.8266004059235));
#49426=CARTESIAN_POINT('Ctrl Pts',(25.7047701575212,-0.366738219301859,
25.5323627847595));
#49427=CARTESIAN_POINT('Ctrl Pts',(25.7365977662161,0.142012507544223,25.4749872441391));
#49428=CARTESIAN_POINT('Ctrl Pts',(25.7684253749109,0.616000848872784,25.6685183971005));
#49429=CARTESIAN_POINT('Ctrl Pts',(25.8002529836057,0.93920205568446,26.0655829187618));
#49430=CARTESIAN_POINT('Ctrl Pts',(25.8320805923005,1.03250165349385,26.568985779688));
#49431=CARTESIAN_POINT('Ctrl Pts',(25.8639082009953,0.873061395142099,27.055502026023));
#49432=CARTESIAN_POINT('Ctrl Pts',(25.8957358096901,0.499909702299201,27.4060402829133));
#49433=CARTESIAN_POINT('Ctrl Pts',(25.927563418385,0.00438812460655832,
27.5347943957049));
#49434=CARTESIAN_POINT('Ctrl Pts',(25.9593910270797,-0.49220759101559,27.4102474362556));
#49435=CARTESIAN_POINT('Ctrl Pts',(25.9912186357746,-0.868318786396127,
27.0628864757224));
#49436=CARTESIAN_POINT('Ctrl Pts',(26.0230462444694,-1.03187944404665,26.5777399629291));
#49437=CARTESIAN_POINT('Ctrl Pts',(26.0548738531642,-0.942852584360126,
26.0735638874461));
#49438=CARTESIAN_POINT('Ctrl Pts',(26.086701461859,-0.623030465420126,25.6737726615066));
#49439=CARTESIAN_POINT('Ctrl Pts',(26.1185290705539,-0.150700586062053,
25.4762284103369));
#49440=CARTESIAN_POINT('Ctrl Pts',(26.1503566792486,0.35851859155766,25.5292874779674));
#49441=CARTESIAN_POINT('Ctrl Pts',(26.1821842879435,0.779977767383015,25.8199605755439));
#49442=CARTESIAN_POINT('Ctrl Pts',(26.2140118966383,1.01051163721584,26.2770980038405));
#49443=CARTESIAN_POINT('Ctrl Pts',(26.2458395053331,0.993687039496576,26.7887952855562));
#49444=CARTESIAN_POINT('Ctrl Pts',(26.2776671140279,0.733626454713128,27.2298057419935));
#49445=CARTESIAN_POINT('Ctrl Pts',(26.3094947227228,0.29398082464875,27.4921608151878));
#49446=CARTESIAN_POINT('Ctrl Pts',(26.3413223314176,-0.217617061428775,
27.5116709161353));
#49447=CARTESIAN_POINT('Ctrl Pts',(26.3731499401124,-0.675963838923886,
27.2835021616918));
#49448=CARTESIAN_POINT('Ctrl Pts',(26.4049775488072,-0.968810988626381,
26.8636171944324));
#49449=CARTESIAN_POINT('Ctrl Pts',(26.436805157502,-1.02457724546662,26.3545814743717));
#49450=CARTESIAN_POINT('Ctrl Pts',(26.4580235632986,-0.894453156519727,
26.0391661184899));
#49451=CARTESIAN_POINT('Ctrl Pts',(26.4686327661969,-0.795561429326952,
25.9065866261757));
#49452=CARTESIAN_POINT('Ctrl Pts',(26.0278332223638,-0.992541444115404,
26.5000219547962));
#49453=CARTESIAN_POINT('Ctrl Pts',(26.036846713316,-0.9924061168657,26.3595200944171));
#49454=CARTESIAN_POINT('Ctrl Pts',(26.0458602042683,-0.962278587565093,
26.2189620518872));
#49455=CARTESIAN_POINT('Ctrl Pts',(26.0548736952205,-0.904386170695536,
26.0909616053013));
#49456=CARTESIAN_POINT('Ctrl Pts',(26.0654828981188,-0.836244714727549,
25.9403004778764));
#49457=CARTESIAN_POINT('Ctrl Pts',(26.0760921010171,-0.729637405062499,
25.8070368150429));
#49458=CARTESIAN_POINT('Ctrl Pts',(26.0867013039153,-0.597612150423695,
25.7074809613184));
#49459=CARTESIAN_POINT('Ctrl Pts',(26.0973105068136,-0.465586895784892,
25.6079251075939));
#49460=CARTESIAN_POINT('Ctrl Pts',(26.1079197097119,-0.308143696172334,
25.5420770629784));
#49461=CARTESIAN_POINT('Ctrl Pts',(26.1185289126102,-0.144552283834306,
25.5179962133571));
#49462=CARTESIAN_POINT('Ctrl Pts',(26.1291381155085,0.0190391285036842,
25.4939153637357));
#49463=CARTESIAN_POINT('Ctrl Pts',(26.1397473184067,0.188778753567142,25.5116017091084));
#49464=CARTESIAN_POINT('Ctrl Pts',(26.150356521305,0.343891720351772,25.5688903692854));
#49465=CARTESIAN_POINT('Ctrl Pts',(26.1609657242032,0.499004687136437,25.6261790294623));
#49466=CARTESIAN_POINT('Ctrl Pts',(26.1715749271015,0.639490995642267,25.7230700044435));
#49467=CARTESIAN_POINT('Ctrl Pts',(26.1821841299998,0.748156438714674,25.8477050180672));
#49468=CARTESIAN_POINT('Ctrl Pts',(26.1927933328981,0.856821881787082,25.972340031691));
#49469=CARTESIAN_POINT('Ctrl Pts',(26.2034025357963,0.933666459426068,26.1247190839574));
#49470=CARTESIAN_POINT('Ctrl Pts',(26.2140117386946,0.969284650291061,26.2861914397263));
#49471=CARTESIAN_POINT('Ctrl Pts',(26.2246209415929,1.00490284115605,26.4476637954953));
#49472=CARTESIAN_POINT('Ctrl Pts',(26.2352301444912,0.999294645247054,26.6182294547669));
#49473=CARTESIAN_POINT('Ctrl Pts',(26.2458393473894,0.953147142237316,26.777013983489));
#49474=CARTESIAN_POINT('Ctrl Pts',(26.2564485502877,0.906999639227578,26.935798512211));
#49475=CARTESIAN_POINT('Ctrl Pts',(26.267057753186,0.820312829117102,27.0828019103836));
#49476=CARTESIAN_POINT('Ctrl Pts',(26.2776669560843,0.703695195902629,27.2000294290331));
#49477=CARTESIAN_POINT('Ctrl Pts',(26.2882761589825,0.587077562688156,27.3172569476826));
#49478=CARTESIAN_POINT('Ctrl Pts',(26.2988853618808,0.440529106369687,27.4047085868092));
#49479=CARTESIAN_POINT('Ctrl Pts',(26.3094945647791,0.281988614504523,27.4516860879325));
#49480=CARTESIAN_POINT('Ctrl Pts',(26.3201037676774,0.123448122639396,27.4986635890558));
#49481=CARTESIAN_POINT('Ctrl Pts',(26.3307129705756,-0.0470844047724203,
27.5051669521759));
#49482=CARTESIAN_POINT('Ctrl Pts',(26.3413221734739,-0.208741752691548,
27.4703905305806));
#49483=CARTESIAN_POINT('Ctrl Pts',(26.3467147823159,-0.290911436137823,
27.4527138360742));
#49484=CARTESIAN_POINT('Ctrl Pts',(26.352107391158,-0.370788090973951,27.4243719231966));
#49485=CARTESIAN_POINT('Ctrl Pts',(26.3575,-0.445914873067339,27.3865896766146));
#49486=CARTESIAN_POINT('',(9.6,-0.662189971174158,26.1181378955904));
#49487=CARTESIAN_POINT('Ctrl Pts',(9.6,-0.662189971174161,26.1181378955904));
#49488=CARTESIAN_POINT('Ctrl Pts',(9.6,-0.686801732918713,26.1409234509207));
#49489=CARTESIAN_POINT('Ctrl Pts',(9.6,-0.709791921105586,26.1653652554484));
#49490=CARTESIAN_POINT('Ctrl Pts',(9.6,-0.731095598422574,26.1911933292668));
#49491=CARTESIAN_POINT('Ctrl Pts',(9.6,-0.746587075514762,26.2099748291899));
#49492=CARTESIAN_POINT('Ctrl Pts',(9.6,-0.76118721574113,26.2294905658139));
#49493=CARTESIAN_POINT('Ctrl Pts',(9.6,-0.774872528490492,26.2496541439083));
#49494=CARTESIAN_POINT('Ctrl Pts',(9.6,-0.787306841273407,26.2679745317168));
#49495=CARTESIAN_POINT('Ctrl Pts',(9.6,-0.798986056598059,26.2868299650152));
#49496=CARTESIAN_POINT('Ctrl Pts',(9.6,-0.809890960914313,26.3061651627819));
#49497=CARTESIAN_POINT('Ctrl Pts',(9.6,-0.81424407823496,26.3138835601062));
#49498=CARTESIAN_POINT('Ctrl Pts',(9.6,-0.81847261504564,26.321676705201));
#49499=CARTESIAN_POINT('Ctrl Pts',(9.6,-0.822570170079064,26.3295304891797));
#49500=CARTESIAN_POINT('Ctrl Pts',(9.6,-0.839363102383987,26.3617175035373));
#49501=CARTESIAN_POINT('Ctrl Pts',(9.6,-0.853982926877251,26.3949649073311));
#49502=CARTESIAN_POINT('Ctrl Pts',(9.6,-0.866370885724305,26.4290078753479));
#49503=CARTESIAN_POINT('Ctrl Pts',(9.6,-0.868330245916886,26.4343923327224));
#49504=CARTESIAN_POINT('Ctrl Pts',(9.6,-0.8702337540175,26.4397967967659));
#49505=CARTESIAN_POINT('Ctrl Pts',(9.6,-0.872081151097179,26.4452203335801));
#49506=CARTESIAN_POINT('Ctrl Pts',(9.6,-0.88031761925099,26.4694007270337));
#49507=CARTESIAN_POINT('Ctrl Pts',(9.6,-0.887439277333979,26.4939594120755));
#49508=CARTESIAN_POINT('Ctrl Pts',(9.6,-0.893464100126309,26.5188184610355));
#49509=CARTESIAN_POINT('Ctrl Pts',(9.6,-0.896486584530233,26.531289547799));
#49510=CARTESIAN_POINT('Ctrl Pts',(9.6,-0.899232918726265,26.5438363937201));
#49511=CARTESIAN_POINT('Ctrl Pts',(9.6,-0.901704670785838,26.5564500650579));
#49512=CARTESIAN_POINT('Ctrl Pts',(9.6,-0.903275800885989,26.5644677457292));
#49513=CARTESIAN_POINT('Ctrl Pts',(9.6,-0.904735366145582,26.5725097265233));
#49514=CARTESIAN_POINT('Ctrl Pts',(9.6,-0.90608264699377,26.580564871723));
#49515=CARTESIAN_POINT('Ctrl Pts',(9.6,-0.912493287483545,26.6188929159742));
#49516=CARTESIAN_POINT('Ctrl Pts',(9.6,-0.916374828360992,26.6575700845772));
#49517=CARTESIAN_POINT('Ctrl Pts',(9.6,-0.917813576717061,26.6963221410477));
#49518=CARTESIAN_POINT('Ctrl Pts',(9.6,-0.919296030516451,26.7362513844811));
#49519=CARTESIAN_POINT('Ctrl Pts',(9.6,-0.918185813702954,26.776260957008));
#49520=CARTESIAN_POINT('Ctrl Pts',(9.6,-0.914542375176316,26.816094610719));
#49521=CARTESIAN_POINT('Ctrl Pts',(9.6,-0.911350401534987,26.8509924062365));
#49522=CARTESIAN_POINT('Ctrl Pts',(9.6,-0.90621378911242,26.8857563520486));
#49523=CARTESIAN_POINT('Ctrl Pts',(9.6,-0.899144830704795,26.9202318686355));
#49524=CARTESIAN_POINT('Ctrl Pts',(9.59999999999996,-0.662189971174005,
26.1181378955905));
#49525=CARTESIAN_POINT('Ctrl Pts',(9.60084086971211,-0.657153163178387,
26.1093900202931));
#49526=CARTESIAN_POINT('Ctrl Pts',(9.61229094232253,-0.586182178363583,
25.9916516862185));
#49527=CARTESIAN_POINT('Ctrl Pts',(9.63435021783122,-0.387770113791111,
25.8037814721796));
#49528=CARTESIAN_POINT('Ctrl Pts',(9.66617782652605,-0.00653957363242062,
25.7030919772491));
#49529=CARTESIAN_POINT('Ctrl Pts',(9.69800543522088,0.376272204290504,25.7974986628543));
#49530=CARTESIAN_POINT('Ctrl Pts',(9.72983304391567,0.66698890097209,26.0638527475773));
#49531=CARTESIAN_POINT('Ctrl Pts',(9.76166065261051,0.794431941545588,26.4369759237776));
#49532=CARTESIAN_POINT('Ctrl Pts',(9.79348826130532,0.727413669545738,26.8255225525671));
#49533=CARTESIAN_POINT('Ctrl Pts',(9.82531587000014,0.482334658244354,27.1343885069846));
#49534=CARTESIAN_POINT('Ctrl Pts',(9.85714347869494,0.119188665110999,27.2879652485877));
#49535=CARTESIAN_POINT('Ctrl Pts',(9.88897108738978,-0.273133232602854,
27.2486612961868));
#49536=CARTESIAN_POINT('Ctrl Pts',(9.92079869608458,-0.598596265249733,
27.0260967569105));
#49537=CARTESIAN_POINT('Ctrl Pts',(9.94670853832486,-0.744262673060946,
26.740078447277));
#49538=CARTESIAN_POINT('Ctrl Pts',(9.96200917766685,-0.764304859829967,
26.5563460400826));
#49539=CARTESIAN_POINT('Ctrl Pts',(9.96670061411058,-0.764287395473808,
26.5000068045578));
#49540=CARTESIAN_POINT('Origin',(8.83329938588935,0.,26.5));
#49541=CARTESIAN_POINT('Origin',(9.6,0.,26.5));
#49542=CARTESIAN_POINT('Origin',(18.,0.,26.5));
#49543=CARTESIAN_POINT('Origin',(3.12167427535308,0.,26.5));
#49544=CARTESIAN_POINT('',(3.24334855070616,0.,26.5));
#49545=CARTESIAN_POINT('',(3.12167427535308,-2.4799097682734E-17,26.2975));
#49546=CARTESIAN_POINT('Origin',(2.25,-0.25,27.2));
#49547=CARTESIAN_POINT('',(3.75,-0.25,27.4682458365519));
#49548=CARTESIAN_POINT('',(2.25,-0.25,27.4682458365519));
#49549=CARTESIAN_POINT('',(5.1,-0.25,27.4682458365519));
#49550=CARTESIAN_POINT('',(3.75,-0.25,27.2));
#49551=CARTESIAN_POINT('',(3.75,-0.25,27.2));
#49552=CARTESIAN_POINT('',(2.25,-0.25,27.2));
#49553=CARTESIAN_POINT('',(2.25,-0.25,27.2));
#49554=CARTESIAN_POINT('',(2.25,-0.25,27.2));
#49555=CARTESIAN_POINT('Origin',(2.25,0.,27.2));
#49556=CARTESIAN_POINT('',(2.25,0.25,27.4682458365519));
#49557=CARTESIAN_POINT('Ctrl Pts',(2.25,-0.25,27.4682458365519));
#49558=CARTESIAN_POINT('Ctrl Pts',(2.2184626473304,-0.25,27.4682458365519));
#49559=CARTESIAN_POINT('Ctrl Pts',(2.18491957299737,-0.243669763522489,
27.4699471586642));
#49560=CARTESIAN_POINT('Ctrl Pts',(2.12336732874239,-0.218115996279034,
27.4760111944473));
#49561=CARTESIAN_POINT('Ctrl Pts',(2.09534588636318,-0.198899276956455,
27.4802776512909));
#49562=CARTESIAN_POINT('Ctrl Pts',(2.05110381617461,-0.154657206767882,
27.4882237616694));
#49563=CARTESIAN_POINT('Ctrl Pts',(2.03188468517318,-0.126634476150511,
27.4924312594508));
#49564=CARTESIAN_POINT('Ctrl Pts',(2.00632915724249,-0.0650776639541235,
27.4983591502449));
#49565=CARTESIAN_POINT('Ctrl Pts',(2.,-0.0315329431858092,27.5));
#49566=CARTESIAN_POINT('Ctrl Pts',(2.,0.0315329431858092,27.5));
#49567=CARTESIAN_POINT('Ctrl Pts',(2.00632915724249,0.065077663954124,27.4983591502449));
#49568=CARTESIAN_POINT('Ctrl Pts',(2.03188468517318,0.126634476150511,27.4924312594508));
#49569=CARTESIAN_POINT('Ctrl Pts',(2.05110381617461,0.154657206767882,27.4882237616694));
#49570=CARTESIAN_POINT('Ctrl Pts',(2.09534588636318,0.198899276956455,27.4802776512909));
#49571=CARTESIAN_POINT('Ctrl Pts',(2.12336732874239,0.218115996279034,27.4760111944473));
#49572=CARTESIAN_POINT('Ctrl Pts',(2.18491957299737,0.243669763522489,27.4699471586642));
#49573=CARTESIAN_POINT('Ctrl Pts',(2.2184626473304,0.25,27.4682458365519));
#49574=CARTESIAN_POINT('Ctrl Pts',(2.25,0.25,27.4682458365519));
#49575=CARTESIAN_POINT('',(2.25,0.25,27.2));
#49576=CARTESIAN_POINT('Origin',(2.25,0.,27.2));
#49577=CARTESIAN_POINT('',(2.25,0.25,27.2));
#49578=CARTESIAN_POINT('Origin',(3.75,0.25,27.2));
#49579=CARTESIAN_POINT('',(3.75,0.25,27.4682458365519));
#49580=CARTESIAN_POINT('',(5.1,0.25,27.4682458365519));
#49581=CARTESIAN_POINT('',(3.75,0.25,27.2));
#49582=CARTESIAN_POINT('',(3.75,0.25,27.2));
#49583=CARTESIAN_POINT('',(3.75,0.25,27.2));
#49584=CARTESIAN_POINT('Origin',(3.75,0.,27.2));
#49585=CARTESIAN_POINT('Ctrl Pts',(3.75,0.25,27.4682458365519));
#49586=CARTESIAN_POINT('Ctrl Pts',(3.7815373526696,0.25,27.4682458365519));
#49587=CARTESIAN_POINT('Ctrl Pts',(3.81508042700262,0.243669763522489,27.4699471586642));
#49588=CARTESIAN_POINT('Ctrl Pts',(3.87663267125761,0.218115996279034,27.4760111944473));
#49589=CARTESIAN_POINT('Ctrl Pts',(3.90465411363682,0.198899276956455,27.4802776512909));
#49590=CARTESIAN_POINT('Ctrl Pts',(3.94889618382539,0.154657206767882,27.4882237616694));
#49591=CARTESIAN_POINT('Ctrl Pts',(3.96811531482682,0.126634476150511,27.4924312594508));
#49592=CARTESIAN_POINT('Ctrl Pts',(3.99367084275751,0.065077663954124,27.4983591502449));
#49593=CARTESIAN_POINT('Ctrl Pts',(4.,0.0315329431858092,27.5));
#49594=CARTESIAN_POINT('Ctrl Pts',(4.,-0.0315329431858091,27.5));
#49595=CARTESIAN_POINT('Ctrl Pts',(3.99367084275751,-0.0650776639541237,
27.4983591502449));
#49596=CARTESIAN_POINT('Ctrl Pts',(3.96811531482682,-0.126634476150511,
27.4924312594508));
#49597=CARTESIAN_POINT('Ctrl Pts',(3.94889618382539,-0.154657206767882,
27.4882237616694));
#49598=CARTESIAN_POINT('Ctrl Pts',(3.90465411363682,-0.198899276956454,
27.4802776512909));
#49599=CARTESIAN_POINT('Ctrl Pts',(3.87663267125761,-0.218115996279034,
27.4760111944473));
#49600=CARTESIAN_POINT('Ctrl Pts',(3.81508042700263,-0.243669763522489,
27.4699471586642));
#49601=CARTESIAN_POINT('Ctrl Pts',(3.7815373526696,-0.25,27.4682458365519));
#49602=CARTESIAN_POINT('Ctrl Pts',(3.75,-0.25,27.4682458365519));
#49603=CARTESIAN_POINT('Origin',(3.75,0.,27.2));
#49604=CARTESIAN_POINT('Origin',(3.,0.,27.2));
#49605=CARTESIAN_POINT('Origin',(1.375,0.,26.5));
#49606=CARTESIAN_POINT('',(1.4,-0.999999999999999,26.5));
#49607=CARTESIAN_POINT('Origin',(1.4,0.,26.5));
#49608=CARTESIAN_POINT('',(1.375,-0.975,26.5));
#49609=CARTESIAN_POINT('Origin',(5.1,0.,26.5));
#49610=CARTESIAN_POINT('',(8.8,-1.,26.5));
#49611=CARTESIAN_POINT('Origin',(8.8,0.,26.5));
#49612=CARTESIAN_POINT('',(5.1,-1.,26.5));
#49613=CARTESIAN_POINT('Origin',(8.8,1.55,26.5));
#49614=CARTESIAN_POINT('',(8.8,-1.55,26.5));
#49615=CARTESIAN_POINT('Origin',(8.8,0.,26.5));
#49616=CARTESIAN_POINT('Origin',(8.825,0.,26.5));
#49617=CARTESIAN_POINT('',(8.85,-1.6,26.5));
#49618=CARTESIAN_POINT('Origin',(8.85,0.,26.5));
#49619=CARTESIAN_POINT('',(8.825,-1.575,26.5));
#49620=CARTESIAN_POINT('Origin',(9.2,0.,26.5));
#49621=CARTESIAN_POINT('',(9.55,-1.6,26.5));
#49622=CARTESIAN_POINT('Origin',(9.55,0.,26.5));
#49623=CARTESIAN_POINT('',(9.2,-1.6,26.5));
#49624=CARTESIAN_POINT('Origin',(9.575,0.,26.5));
#49625=CARTESIAN_POINT('',(9.6,-1.55,26.5));
#49626=CARTESIAN_POINT('Origin',(9.6,0.,26.5));
#49627=CARTESIAN_POINT('',(9.575,-1.575,26.5));
#49628=CARTESIAN_POINT('Origin',(9.6,1.,26.5));
#49629=CARTESIAN_POINT('',(0.,0.,0.));
#49630=CARTESIAN_POINT('Origin',(10.0176776695297,0.,26.5));
#49631=CARTESIAN_POINT('',(10.,1.155,26.5));
#49632=CARTESIAN_POINT('Origin',(10.,0.,26.5));
#49633=CARTESIAN_POINT('',(10.0353553390593,1.06964466094067,26.5));
#49634=CARTESIAN_POINT('',(10.0176776695297,1.11232233047034,26.5));
#49635=CARTESIAN_POINT('',(10.0353553390593,-1.06964466094068,26.5));
#49636=CARTESIAN_POINT('Origin',(10.0353553390593,0.,26.5));
#49637=CARTESIAN_POINT('Origin',(10.0353553390593,0.,26.5));
#49638=CARTESIAN_POINT('Origin',(10.05,0.,26.5));
#49639=CARTESIAN_POINT('',(10.0646446609407,1.04035533905933,26.5));
#49640=CARTESIAN_POINT('',(10.0646446609407,-1.04035533905933,26.5));
#49641=CARTESIAN_POINT('Origin',(10.0646446609407,0.,26.5));
#49642=CARTESIAN_POINT('Origin',(10.0646446609407,0.,26.5));
#49643=CARTESIAN_POINT('',(10.05,-1.055,26.5));
#49644=CARTESIAN_POINT('Origin',(10.,1.95,26.5));
#49645=CARTESIAN_POINT('',(10.,-1.95,26.5));
#49646=CARTESIAN_POINT('Origin',(10.,0.,26.5));
#49647=CARTESIAN_POINT('Origin',(10.1073223304703,0.,26.5));
#49648=CARTESIAN_POINT('',(10.15,1.005,26.5));
#49649=CARTESIAN_POINT('',(10.1073223304703,1.02267766952966,26.5));
#49650=CARTESIAN_POINT('',(10.15,-1.005,26.5));
#49651=CARTESIAN_POINT('Origin',(10.15,0.,26.5));
#49652=CARTESIAN_POINT('Origin',(10.15,0.,26.5));
#49653=CARTESIAN_POINT('Origin',(12.5,0.,26.5));
#49654=CARTESIAN_POINT('',(14.9,-1.005,26.5));
#49655=CARTESIAN_POINT('Origin',(14.9,0.,26.5));
#49656=CARTESIAN_POINT('',(12.5,-1.005,26.5));
#49657=CARTESIAN_POINT('Origin',(12.6,1.92,26.5));
#49658=CARTESIAN_POINT('',(12.6,-2.,26.5));
#49659=CARTESIAN_POINT('Origin',(12.6,0.,26.5));
#49660=CARTESIAN_POINT('',(12.6,-1.92,26.5));
#49661=CARTESIAN_POINT('Origin',(12.6,0.,26.5));
#49662=CARTESIAN_POINT('Origin',(12.5,0.,26.5));
#49663=CARTESIAN_POINT('',(12.4,-1.92,26.5));
#49664=CARTESIAN_POINT('Origin',(12.4,0.,26.5));
#49665=CARTESIAN_POINT('',(12.5,-1.92,26.5));
#49666=CARTESIAN_POINT('Origin',(12.4,2.01,26.5));
#49667=CARTESIAN_POINT('',(12.4,-2.,26.5));
#49668=CARTESIAN_POINT('Origin',(12.4,0.,26.5));
#49669=CARTESIAN_POINT('Origin',(12.5,0.,26.5));
#49670=CARTESIAN_POINT('',(10.05,-2.,26.5));
#49671=CARTESIAN_POINT('',(12.5,-2.,26.5));
#49672=CARTESIAN_POINT('Origin',(10.05,0.,26.5));
#49673=CARTESIAN_POINT('Origin',(10.025,0.,26.5));
#49674=CARTESIAN_POINT('',(10.025,-1.975,26.5));
#49675=CARTESIAN_POINT('Origin',(12.5,0.,26.5));
#49676=CARTESIAN_POINT('',(14.95,-2.,26.5));
#49677=CARTESIAN_POINT('Origin',(14.95,0.,26.5));
#49678=CARTESIAN_POINT('',(12.5,-2.,26.5));
#49679=CARTESIAN_POINT('Origin',(14.975,0.,26.5));
#49680=CARTESIAN_POINT('',(15.,-1.95,26.5));
#49681=CARTESIAN_POINT('Origin',(15.,0.,26.5));
#49682=CARTESIAN_POINT('',(14.975,-1.975,26.5));
#49683=CARTESIAN_POINT('Origin',(15.,1.105,26.5));
#49684=CARTESIAN_POINT('',(15.,-1.105,26.5));
#49685=CARTESIAN_POINT('Origin',(15.,0.,26.5));
#49686=CARTESIAN_POINT('Origin',(14.95,0.,26.5));
#49687=CARTESIAN_POINT('',(14.95,-1.055,26.5));
#49688=CARTESIAN_POINT('',(0.,0.,0.));
#49689=CARTESIAN_POINT('Origin',(9.375,0.,26.5));
#49690=CARTESIAN_POINT('',(9.35,1.8,26.5));
#49691=CARTESIAN_POINT('',(9.35,-1.8,26.5));
#49692=CARTESIAN_POINT('Origin',(9.35,0.,26.5));
#49693=CARTESIAN_POINT('Origin',(9.35,0.,26.5));
#49694=CARTESIAN_POINT('',(9.4,1.85,26.5));
#49695=CARTESIAN_POINT('',(9.375,1.825,26.5));
#49696=CARTESIAN_POINT('Origin',(9.4,0.,26.5));
#49697=CARTESIAN_POINT('Origin',(9.4,1.8,26.5));
#49698=CARTESIAN_POINT('',(9.4,-3.445,26.5));
#49699=CARTESIAN_POINT('Origin',(9.4,0.,26.5));
#49700=CARTESIAN_POINT('Origin',(8.6,0.,26.5));
#49701=CARTESIAN_POINT('',(7.8,-1.8,26.5));
#49702=CARTESIAN_POINT('',(8.6,-1.8,26.5));
#49703=CARTESIAN_POINT('Origin',(7.8,0.,26.5));
#49704=CARTESIAN_POINT('Origin',(7.98232233047034,0.,26.5));
#49705=CARTESIAN_POINT('',(8.,6.1,26.5));
#49706=CARTESIAN_POINT('Origin',(8.,0.,26.5));
#49707=CARTESIAN_POINT('',(7.96464466094067,6.18535533905933,26.5));
#49708=CARTESIAN_POINT('',(7.98232233047034,6.14267766952966,26.5));
#49709=CARTESIAN_POINT('',(7.96464466094067,-6.18535533905933,26.5));
#49710=CARTESIAN_POINT('Origin',(7.96464466094067,0.,26.5));
#49711=CARTESIAN_POINT('Origin',(7.96464466094067,0.,26.5));
#49712=CARTESIAN_POINT('Origin',(7.95,0.,26.5));
#49713=CARTESIAN_POINT('',(7.93535533905933,-6.21464466094067,26.5));
#49714=CARTESIAN_POINT('',(7.95,-6.2,26.5));
#49715=CARTESIAN_POINT('',(7.93535533905933,6.21464466094067,26.5));
#49716=CARTESIAN_POINT('Origin',(7.93535533905933,0.,26.5));
#49717=CARTESIAN_POINT('Origin',(7.93535533905933,0.,26.5));
#49718=CARTESIAN_POINT('Origin',(8.,3.495,26.5));
#49719=CARTESIAN_POINT('',(8.,-3.495,26.5));
#49720=CARTESIAN_POINT('Origin',(8.,0.,26.5));
#49721=CARTESIAN_POINT('',(8.,3.53553390593274,29.7055339059327));
#49722=CARTESIAN_POINT('Origin',(8.,3.53553390593274,30.0355339059327));
#49723=CARTESIAN_POINT('',(8.,-3.53553390593274,29.7055339059327));
#49724=CARTESIAN_POINT('Origin',(8.,-3.53553390593274,30.0355339059327));
#49725=CARTESIAN_POINT('',(8.,-3.53553390593274,22.6344660940673));
#49726=CARTESIAN_POINT('Origin',(8.,-3.53553390593274,22.9644660940673));
#49727=CARTESIAN_POINT('',(8.,3.53553390593274,22.6344660940673));
#49728=CARTESIAN_POINT('Origin',(8.,3.53553390593274,22.9644660940673));
#49729=CARTESIAN_POINT('Origin',(7.89267766952966,0.,26.5));
#49730=CARTESIAN_POINT('',(7.85,6.25,26.5));
#49731=CARTESIAN_POINT('',(7.89267766952966,6.23232233047034,26.5));
#49732=CARTESIAN_POINT('',(7.85,-6.25,26.5));
#49733=CARTESIAN_POINT('Origin',(7.85,0.,26.5));
#49734=CARTESIAN_POINT('Origin',(7.85,0.,26.5));
#49735=CARTESIAN_POINT('Origin',(7.4,0.,26.5));
#49736=CARTESIAN_POINT('',(6.95,-6.25,26.5));
#49737=CARTESIAN_POINT('',(7.4,-6.25,26.5));
#49738=CARTESIAN_POINT('',(6.95,6.25,26.5));
#49739=CARTESIAN_POINT('Origin',(6.95,0.,26.5));
#49740=CARTESIAN_POINT('Origin',(6.95,0.,26.5));
#49741=CARTESIAN_POINT('Origin',(6.90732233047034,0.,26.5));
#49742=CARTESIAN_POINT('',(6.86464466094067,6.21464466094067,26.5));
#49743=CARTESIAN_POINT('',(6.90732233047034,6.23232233047034,26.5));
#49744=CARTESIAN_POINT('',(6.86464466094067,-6.21464466094067,26.5));
#49745=CARTESIAN_POINT('Origin',(6.86464466094067,0.,26.5));
#49746=CARTESIAN_POINT('Origin',(6.86464466094067,0.,26.5));
#49747=CARTESIAN_POINT('Origin',(6.85,0.,26.5));
#49748=CARTESIAN_POINT('',(6.83535533905933,-6.18535533905933,26.5));
#49749=CARTESIAN_POINT('',(6.85,-6.2,26.5));
#49750=CARTESIAN_POINT('',(6.83535533905933,6.18535533905933,26.5));
#49751=CARTESIAN_POINT('Origin',(6.83535533905933,0.,26.5));
#49752=CARTESIAN_POINT('Origin',(6.83535533905933,0.,26.5));
#49753=CARTESIAN_POINT('Origin',(6.81767766952966,0.,26.5));
#49754=CARTESIAN_POINT('',(6.8,6.1,26.5));
#49755=CARTESIAN_POINT('',(6.81767766952966,6.14267766952966,26.5));
#49756=CARTESIAN_POINT('Origin',(6.8,0.,26.5));
#49757=CARTESIAN_POINT('Origin',(6.8,6.15,26.5));
#49758=CARTESIAN_POINT('',(6.8,-2.8,26.5));
#49759=CARTESIAN_POINT('Origin',(6.8,0.,26.5));
#49760=CARTESIAN_POINT('',(6.8,3.53553390593274,29.7055339059327));
#49761=CARTESIAN_POINT('Origin',(6.8,3.53553390593274,30.0355339059327));
#49762=CARTESIAN_POINT('',(6.8,-3.53553390593274,29.7055339059327));
#49763=CARTESIAN_POINT('Origin',(6.8,-3.53553390593274,30.0355339059327));
#49764=CARTESIAN_POINT('',(6.8,-3.53553390593274,22.6344660940673));
#49765=CARTESIAN_POINT('Origin',(6.8,-3.53553390593274,22.9644660940673));
#49766=CARTESIAN_POINT('',(6.8,3.53553390593274,22.6344660940673));
#49767=CARTESIAN_POINT('Origin',(6.8,3.53553390593274,22.9644660940673));
#49768=CARTESIAN_POINT('Origin',(5.15732233047034,0.,26.5));
#49769=CARTESIAN_POINT('',(5.2,2.8,26.5));
#49770=CARTESIAN_POINT('',(5.2,-2.8,26.5));
#49771=CARTESIAN_POINT('Origin',(5.2,0.,26.5));
#49772=CARTESIAN_POINT('Origin',(5.2,0.,26.5));
#49773=CARTESIAN_POINT('',(5.11464466094067,2.76464466094067,26.5));
#49774=CARTESIAN_POINT('',(5.15732233047034,2.78232233047034,26.5));
#49775=CARTESIAN_POINT('',(5.11464466094067,-2.76464466094067,26.5));
#49776=CARTESIAN_POINT('Origin',(5.11464466094067,0.,26.5));
#49777=CARTESIAN_POINT('Origin',(5.11464466094067,0.,26.5));
#49778=CARTESIAN_POINT('Origin',(5.1,0.,26.5));
#49779=CARTESIAN_POINT('',(5.08535533905933,-2.73535533905933,26.5));
#49780=CARTESIAN_POINT('',(5.1,-2.75,26.5));
#49781=CARTESIAN_POINT('',(5.08535533905933,2.73535533905933,26.5));
#49782=CARTESIAN_POINT('Origin',(5.08535533905933,0.,26.5));
#49783=CARTESIAN_POINT('Origin',(5.08535533905933,0.,26.5));
#49784=CARTESIAN_POINT('Origin',(5.975,0.,26.5));
#49785=CARTESIAN_POINT('',(5.975,-2.8,26.5));
#49786=CARTESIAN_POINT('Origin',(5.06767766952966,0.,26.5));
#49787=CARTESIAN_POINT('',(5.05,2.65,26.5));
#49788=CARTESIAN_POINT('',(5.06767766952966,2.69267766952966,26.5));
#49789=CARTESIAN_POINT('Origin',(5.05,0.,26.5));
#49790=CARTESIAN_POINT('Origin',(5.05,2.7,26.5));
#49791=CARTESIAN_POINT('',(5.05,1.85,26.5));
#49792=CARTESIAN_POINT('Origin',(5.05,0.,26.5));
#49793=CARTESIAN_POINT('Origin',(5.075,0.,26.5));
#49794=CARTESIAN_POINT('',(5.1,1.8,26.5));
#49795=CARTESIAN_POINT('',(5.075,1.825,26.5));
#49796=CARTESIAN_POINT('',(5.1,-1.8,26.5));
#49797=CARTESIAN_POINT('Origin',(5.1,0.,26.5));
#49798=CARTESIAN_POINT('Origin',(5.1,0.,26.5));
#49799=CARTESIAN_POINT('Origin',(5.525,0.,26.5));
#49800=CARTESIAN_POINT('',(6.,-1.8,26.5));
#49801=CARTESIAN_POINT('Origin',(6.,0.,26.5));
#49802=CARTESIAN_POINT('',(5.525,-1.8,26.5));
#49803=CARTESIAN_POINT('Origin',(7.41,3.53553390593274,22.9644660940673));
#49804=CARTESIAN_POINT('',(7.41,3.53553390593274,22.6344660940673));
#49805=CARTESIAN_POINT('Origin',(7.41,-3.53553390593274,22.9644660940673));
#49806=CARTESIAN_POINT('',(7.41,-3.53553390593274,22.6344660940673));
#49807=CARTESIAN_POINT('Origin',(7.41,-3.53553390593274,30.0355339059327));
#49808=CARTESIAN_POINT('',(7.41,-3.53553390593274,29.7055339059327));
#49809=CARTESIAN_POINT('Origin',(7.41,3.53553390593274,30.0355339059327));
#49810=CARTESIAN_POINT('',(7.41,3.53553390593274,29.7055339059327));
#49811=CARTESIAN_POINT('Origin',(8.675,0.,26.5));
#49812=CARTESIAN_POINT('',(9.35,-3.495,26.5));
#49813=CARTESIAN_POINT('Origin',(9.35,0.,26.5));
#49814=CARTESIAN_POINT('',(8.675,-3.495,26.5));
#49815=CARTESIAN_POINT('Origin',(9.375,0.,26.5));
#49816=CARTESIAN_POINT('',(9.375,-3.47,26.5));
#49817=CARTESIAN_POINT('Origin',(7.8,1.05,26.5));
#49818=CARTESIAN_POINT('',(7.8,-1.05,26.5));
#49819=CARTESIAN_POINT('Origin',(7.8,0.,26.5));
#49820=CARTESIAN_POINT('Origin',(6.9,0.,26.5));
#49821=CARTESIAN_POINT('',(6.,-1.05,26.5));
#49822=CARTESIAN_POINT('',(6.9,-1.05,26.5));
#49823=CARTESIAN_POINT('Origin',(6.,0.,26.5));
#49824=CARTESIAN_POINT('Origin',(6.,1.8,26.5));
#49825=CARTESIAN_POINT('',(0.,0.,0.));
#49826=CARTESIAN_POINT('Origin',(4.89267766952966,0.,26.5));
#49827=CARTESIAN_POINT('',(4.93535533905933,2.46464466094067,26.5));
#49828=CARTESIAN_POINT('',(4.93535533905933,-2.46464466094067,26.5));
#49829=CARTESIAN_POINT('Origin',(4.93535533905933,0.,26.5));
#49830=CARTESIAN_POINT('Origin',(4.93535533905933,0.,26.5));
#49831=CARTESIAN_POINT('',(4.85,2.5,26.5));
#49832=CARTESIAN_POINT('',(4.89267766952966,2.48232233047034,26.5));
#49833=CARTESIAN_POINT('',(4.85,-2.5,26.5));
#49834=CARTESIAN_POINT('Origin',(4.85,0.,26.5));
#49835=CARTESIAN_POINT('Origin',(4.85,0.,26.5));
#49836=CARTESIAN_POINT('Origin',(2.9,0.,26.5));
#49837=CARTESIAN_POINT('',(0.95,-2.5,26.5));
#49838=CARTESIAN_POINT('',(2.9,-2.5,26.5));
#49839=CARTESIAN_POINT('',(0.95,2.5,26.5));
#49840=CARTESIAN_POINT('Origin',(0.95,0.,26.5));
#49841=CARTESIAN_POINT('Origin',(0.95,0.,26.5));
#49842=CARTESIAN_POINT('',(3.,2.28093439095105,25.4766045221046));
#49843=CARTESIAN_POINT('',(3.,1.0233954778954,24.219065609049));
#49844=CARTESIAN_POINT('Ctrl Pts',(3.,2.28093439095105,25.4766045221046));
#49845=CARTESIAN_POINT('Ctrl Pts',(2.88748169685465,2.28093439095105,25.4766045221046));
#49846=CARTESIAN_POINT('Ctrl Pts',(2.76831828254861,2.27115802886789,25.453965453567));
#49847=CARTESIAN_POINT('Ctrl Pts',(2.55048659094197,2.2289273827889,25.3667614364727));
#49848=CARTESIAN_POINT('Ctrl Pts',(2.45171547905721,2.19611046218737,25.3026299254791));
#49849=CARTESIAN_POINT('Ctrl Pts',(2.29613442646035,2.1138506187664,25.1627625092691));
#49850=CARTESIAN_POINT('Ctrl Pts',(2.22853784361638,2.05876256550245,25.0774506340239));
#49851=CARTESIAN_POINT('Ctrl Pts',(2.13845834389792,1.92557429855738,24.9017779820919));
#49852=CARTESIAN_POINT('Ctrl Pts',(2.11602564102564,1.8471621020331,24.8116281961004));
#49853=CARTESIAN_POINT('Ctrl Pts',(2.11602564102564,1.68837180389964,24.6528378979669));
#49854=CARTESIAN_POINT('Ctrl Pts',(2.13845834389792,1.59822201790808,24.5744257014426));
#49855=CARTESIAN_POINT('Ctrl Pts',(2.22853784361638,1.42254936597615,24.4412374344975));
#49856=CARTESIAN_POINT('Ctrl Pts',(2.29613442646035,1.33723749073094,24.3861493812336));
#49857=CARTESIAN_POINT('Ctrl Pts',(2.45171547905721,1.19737007452087,24.3038895378126));
#49858=CARTESIAN_POINT('Ctrl Pts',(2.55048659094197,1.1332385635273,24.2710726172111));
#49859=CARTESIAN_POINT('Ctrl Pts',(2.76831828254861,1.04603454643297,24.2288419711321));
#49860=CARTESIAN_POINT('Ctrl Pts',(2.88748169685465,1.0233954778954,24.219065609049));
#49861=CARTESIAN_POINT('Ctrl Pts',(3.,1.0233954778954,24.219065609049));
#49862=CARTESIAN_POINT('Ctrl Pts',(3.,1.0233954778954,24.2190656090489));
#49863=CARTESIAN_POINT('Ctrl Pts',(3.11251830314535,1.0233954778954,24.2190656090489));
#49864=CARTESIAN_POINT('Ctrl Pts',(3.23168171745139,1.04603454643297,24.2288419711321));
#49865=CARTESIAN_POINT('Ctrl Pts',(3.44951340905803,1.1332385635273,24.2710726172111));
#49866=CARTESIAN_POINT('Ctrl Pts',(3.54828452094279,1.19737007452087,24.3038895378126));
#49867=CARTESIAN_POINT('Ctrl Pts',(3.70386557353965,1.33723749073094,24.3861493812336));
#49868=CARTESIAN_POINT('Ctrl Pts',(3.77146215638362,1.42254936597615,24.4412374344975));
#49869=CARTESIAN_POINT('Ctrl Pts',(3.86154165610208,1.59822201790808,24.5744257014426));
#49870=CARTESIAN_POINT('Ctrl Pts',(3.88397435897436,1.68837180389964,24.6528378979669));
#49871=CARTESIAN_POINT('Ctrl Pts',(3.88397435897436,1.8471621020331,24.8116281961004));
#49872=CARTESIAN_POINT('Ctrl Pts',(3.86154165610208,1.92557429855738,24.9017779820919));
#49873=CARTESIAN_POINT('Ctrl Pts',(3.77146215638363,2.05876256550245,25.0774506340238));
#49874=CARTESIAN_POINT('Ctrl Pts',(3.70386557353965,2.1138506187664,25.1627625092691));
#49875=CARTESIAN_POINT('Ctrl Pts',(3.54828452094279,2.19611046218737,25.3026299254791));
#49876=CARTESIAN_POINT('Ctrl Pts',(3.44951340905803,2.2289273827889,25.3667614364727));
#49877=CARTESIAN_POINT('Ctrl Pts',(3.23168171745139,2.27115802886789,25.453965453567));
#49878=CARTESIAN_POINT('Ctrl Pts',(3.11251830314535,2.28093439095105,25.4766045221046));
#49879=CARTESIAN_POINT('Ctrl Pts',(3.,2.28093439095105,25.4766045221046));
#49880=CARTESIAN_POINT('',(3.,-1.0233954778954,24.219065609049));
#49881=CARTESIAN_POINT('',(3.,-2.28093439095105,25.4766045221046));
#49882=CARTESIAN_POINT('Ctrl Pts',(3.,-1.0233954778954,24.219065609049));
#49883=CARTESIAN_POINT('Ctrl Pts',(2.88748169685465,-1.0233954778954,24.219065609049));
#49884=CARTESIAN_POINT('Ctrl Pts',(2.76831828254861,-1.04603454643297,24.2288419711321));
#49885=CARTESIAN_POINT('Ctrl Pts',(2.55048659094197,-1.13323856352731,24.2710726172111));
#49886=CARTESIAN_POINT('Ctrl Pts',(2.45171547905721,-1.19737007452087,24.3038895378126));
#49887=CARTESIAN_POINT('Ctrl Pts',(2.29613442646035,-1.33723749073094,24.3861493812336));
#49888=CARTESIAN_POINT('Ctrl Pts',(2.22853784361638,-1.42254936597615,24.4412374344975));
#49889=CARTESIAN_POINT('Ctrl Pts',(2.13845834389792,-1.59822201790808,24.5744257014426));
#49890=CARTESIAN_POINT('Ctrl Pts',(2.11602564102564,-1.68837180389964,24.6528378979669));
#49891=CARTESIAN_POINT('Ctrl Pts',(2.11602564102564,-1.8471621020331,24.8116281961004));
#49892=CARTESIAN_POINT('Ctrl Pts',(2.13845834389792,-1.92557429855738,24.9017779820919));
#49893=CARTESIAN_POINT('Ctrl Pts',(2.22853784361637,-2.05876256550245,25.0774506340238));
#49894=CARTESIAN_POINT('Ctrl Pts',(2.29613442646035,-2.1138506187664,25.1627625092691));
#49895=CARTESIAN_POINT('Ctrl Pts',(2.45171547905721,-2.19611046218737,25.3026299254791));
#49896=CARTESIAN_POINT('Ctrl Pts',(2.55048659094197,-2.2289273827889,25.3667614364727));
#49897=CARTESIAN_POINT('Ctrl Pts',(2.76831828254861,-2.27115802886789,25.453965453567));
#49898=CARTESIAN_POINT('Ctrl Pts',(2.88748169685465,-2.28093439095105,25.4766045221046));
#49899=CARTESIAN_POINT('Ctrl Pts',(3.,-2.28093439095105,25.4766045221046));
#49900=CARTESIAN_POINT('Ctrl Pts',(3.,-2.28093439095105,25.4766045221046));
#49901=CARTESIAN_POINT('Ctrl Pts',(3.11251830314535,-2.28093439095105,25.4766045221046));
#49902=CARTESIAN_POINT('Ctrl Pts',(3.23168171745139,-2.27115802886789,25.453965453567));
#49903=CARTESIAN_POINT('Ctrl Pts',(3.44951340905803,-2.2289273827889,25.3667614364727));
#49904=CARTESIAN_POINT('Ctrl Pts',(3.54828452094279,-2.19611046218737,25.3026299254791));
#49905=CARTESIAN_POINT('Ctrl Pts',(3.70386557353965,-2.1138506187664,25.1627625092691));
#49906=CARTESIAN_POINT('Ctrl Pts',(3.77146215638363,-2.05876256550245,25.0774506340238));
#49907=CARTESIAN_POINT('Ctrl Pts',(3.86154165610208,-1.92557429855738,24.9017779820919));
#49908=CARTESIAN_POINT('Ctrl Pts',(3.88397435897436,-1.8471621020331,24.8116281961004));
#49909=CARTESIAN_POINT('Ctrl Pts',(3.88397435897436,-1.68837180389964,24.6528378979669));
#49910=CARTESIAN_POINT('Ctrl Pts',(3.86154165610208,-1.59822201790809,24.5744257014426));
#49911=CARTESIAN_POINT('Ctrl Pts',(3.77146215638363,-1.42254936597616,24.4412374344975));
#49912=CARTESIAN_POINT('Ctrl Pts',(3.70386557353965,-1.33723749073094,24.3861493812336));
#49913=CARTESIAN_POINT('Ctrl Pts',(3.54828452094279,-1.19737007452087,24.3038895378126));
#49914=CARTESIAN_POINT('Ctrl Pts',(3.44951340905803,-1.13323856352731,24.2710726172111));
#49915=CARTESIAN_POINT('Ctrl Pts',(3.23168171745139,-1.04603454643297,24.2288419711321));
#49916=CARTESIAN_POINT('Ctrl Pts',(3.11251830314535,-1.0233954778954,24.219065609049));
#49917=CARTESIAN_POINT('Ctrl Pts',(3.,-1.0233954778954,24.219065609049));
#49918=CARTESIAN_POINT('',(3.,-2.28093439095105,27.5233954778954));
#49919=CARTESIAN_POINT('',(3.,-1.0233954778954,28.7809343909511));
#49920=CARTESIAN_POINT('Ctrl Pts',(3.,-2.28093439095105,27.5233954778954));
#49921=CARTESIAN_POINT('Ctrl Pts',(2.88748169685465,-2.28093439095105,27.5233954778954));
#49922=CARTESIAN_POINT('Ctrl Pts',(2.76831828254861,-2.27115802886789,27.546034546433));
#49923=CARTESIAN_POINT('Ctrl Pts',(2.55048659094197,-2.2289273827889,27.6332385635273));
#49924=CARTESIAN_POINT('Ctrl Pts',(2.45171547905721,-2.19611046218737,27.6973700745209));
#49925=CARTESIAN_POINT('Ctrl Pts',(2.29613442646035,-2.1138506187664,27.8372374907309));
#49926=CARTESIAN_POINT('Ctrl Pts',(2.22853784361637,-2.05876256550245,27.9225493659762));
#49927=CARTESIAN_POINT('Ctrl Pts',(2.13845834389792,-1.92557429855738,28.0982220179081));
#49928=CARTESIAN_POINT('Ctrl Pts',(2.11602564102564,-1.8471621020331,28.1883718038996));
#49929=CARTESIAN_POINT('Ctrl Pts',(2.11602564102564,-1.68837180389964,28.3471621020331));
#49930=CARTESIAN_POINT('Ctrl Pts',(2.13845834389792,-1.59822201790808,28.4255742985574));
#49931=CARTESIAN_POINT('Ctrl Pts',(2.22853784361637,-1.42254936597615,28.5587625655025));
#49932=CARTESIAN_POINT('Ctrl Pts',(2.29613442646035,-1.33723749073094,28.6138506187664));
#49933=CARTESIAN_POINT('Ctrl Pts',(2.45171547905721,-1.19737007452087,28.6961104621874));
#49934=CARTESIAN_POINT('Ctrl Pts',(2.55048659094197,-1.13323856352731,28.7289273827889));
#49935=CARTESIAN_POINT('Ctrl Pts',(2.76831828254861,-1.04603454643297,28.7711580288679));
#49936=CARTESIAN_POINT('Ctrl Pts',(2.88748169685465,-1.0233954778954,28.7809343909511));
#49937=CARTESIAN_POINT('Ctrl Pts',(3.,-1.0233954778954,28.7809343909511));
#49938=CARTESIAN_POINT('Ctrl Pts',(3.,-1.0233954778954,28.7809343909511));
#49939=CARTESIAN_POINT('Ctrl Pts',(3.11251830314535,-1.0233954778954,28.7809343909511));
#49940=CARTESIAN_POINT('Ctrl Pts',(3.23168171745139,-1.04603454643297,28.7711580288679));
#49941=CARTESIAN_POINT('Ctrl Pts',(3.44951340905803,-1.13323856352731,28.7289273827889));
#49942=CARTESIAN_POINT('Ctrl Pts',(3.54828452094279,-1.19737007452087,28.6961104621874));
#49943=CARTESIAN_POINT('Ctrl Pts',(3.70386557353965,-1.33723749073094,28.6138506187664));
#49944=CARTESIAN_POINT('Ctrl Pts',(3.77146215638363,-1.42254936597615,28.5587625655025));
#49945=CARTESIAN_POINT('Ctrl Pts',(3.86154165610208,-1.59822201790808,28.4255742985574));
#49946=CARTESIAN_POINT('Ctrl Pts',(3.88397435897436,-1.68837180389964,28.3471621020331));
#49947=CARTESIAN_POINT('Ctrl Pts',(3.88397435897436,-1.8471621020331,28.1883718038996));
#49948=CARTESIAN_POINT('Ctrl Pts',(3.86154165610208,-1.92557429855738,28.0982220179081));
#49949=CARTESIAN_POINT('Ctrl Pts',(3.77146215638362,-2.05876256550245,27.9225493659761));
#49950=CARTESIAN_POINT('Ctrl Pts',(3.70386557353965,-2.1138506187664,27.8372374907309));
#49951=CARTESIAN_POINT('Ctrl Pts',(3.54828452094279,-2.19611046218737,27.6973700745209));
#49952=CARTESIAN_POINT('Ctrl Pts',(3.44951340905803,-2.2289273827889,27.6332385635273));
#49953=CARTESIAN_POINT('Ctrl Pts',(3.23168171745139,-2.27115802886789,27.546034546433));
#49954=CARTESIAN_POINT('Ctrl Pts',(3.11251830314535,-2.28093439095105,27.5233954778954));
#49955=CARTESIAN_POINT('Ctrl Pts',(3.,-2.28093439095105,27.5233954778954));
#49956=CARTESIAN_POINT('',(3.,1.0233954778954,28.780934390951));
#49957=CARTESIAN_POINT('',(3.,2.28093439095105,27.5233954778954));
#49958=CARTESIAN_POINT('Ctrl Pts',(3.,1.0233954778954,28.780934390951));
#49959=CARTESIAN_POINT('Ctrl Pts',(2.88748169685465,1.0233954778954,28.780934390951));
#49960=CARTESIAN_POINT('Ctrl Pts',(2.76831828254861,1.04603454643297,28.7711580288679));
#49961=CARTESIAN_POINT('Ctrl Pts',(2.55048659094197,1.13323856352731,28.7289273827889));
#49962=CARTESIAN_POINT('Ctrl Pts',(2.45171547905721,1.19737007452087,28.6961104621874));
#49963=CARTESIAN_POINT('Ctrl Pts',(2.29613442646035,1.33723749073094,28.6138506187664));
#49964=CARTESIAN_POINT('Ctrl Pts',(2.22853784361638,1.42254936597615,28.5587625655025));
#49965=CARTESIAN_POINT('Ctrl Pts',(2.13845834389792,1.59822201790808,28.4255742985574));
#49966=CARTESIAN_POINT('Ctrl Pts',(2.11602564102564,1.68837180389964,28.3471621020331));
#49967=CARTESIAN_POINT('Ctrl Pts',(2.11602564102564,1.8471621020331,28.1883718038996));
#49968=CARTESIAN_POINT('Ctrl Pts',(2.13845834389792,1.92557429855738,28.0982220179081));
#49969=CARTESIAN_POINT('Ctrl Pts',(2.22853784361637,2.05876256550245,27.9225493659761));
#49970=CARTESIAN_POINT('Ctrl Pts',(2.29613442646034,2.1138506187664,27.8372374907309));
#49971=CARTESIAN_POINT('Ctrl Pts',(2.45171547905721,2.19611046218737,27.6973700745209));
#49972=CARTESIAN_POINT('Ctrl Pts',(2.55048659094197,2.2289273827889,27.6332385635273));
#49973=CARTESIAN_POINT('Ctrl Pts',(2.76831828254861,2.27115802886789,27.546034546433));
#49974=CARTESIAN_POINT('Ctrl Pts',(2.88748169685465,2.28093439095105,27.5233954778954));
#49975=CARTESIAN_POINT('Ctrl Pts',(3.,2.28093439095105,27.5233954778954));
#49976=CARTESIAN_POINT('Ctrl Pts',(3.,2.28093439095105,27.5233954778954));
#49977=CARTESIAN_POINT('Ctrl Pts',(3.11251830314535,2.28093439095105,27.5233954778954));
#49978=CARTESIAN_POINT('Ctrl Pts',(3.23168171745139,2.27115802886789,27.546034546433));
#49979=CARTESIAN_POINT('Ctrl Pts',(3.44951340905803,2.2289273827889,27.6332385635273));
#49980=CARTESIAN_POINT('Ctrl Pts',(3.54828452094279,2.19611046218737,27.6973700745209));
#49981=CARTESIAN_POINT('Ctrl Pts',(3.70386557353965,2.1138506187664,27.8372374907309));
#49982=CARTESIAN_POINT('Ctrl Pts',(3.77146215638363,2.05876256550245,27.9225493659761));
#49983=CARTESIAN_POINT('Ctrl Pts',(3.86154165610208,1.92557429855738,28.0982220179081));
#49984=CARTESIAN_POINT('Ctrl Pts',(3.88397435897436,1.8471621020331,28.1883718038996));
#49985=CARTESIAN_POINT('Ctrl Pts',(3.88397435897436,1.68837180389964,28.3471621020331));
#49986=CARTESIAN_POINT('Ctrl Pts',(3.86154165610208,1.59822201790808,28.4255742985574));
#49987=CARTESIAN_POINT('Ctrl Pts',(3.77146215638362,1.42254936597615,28.5587625655025));
#49988=CARTESIAN_POINT('Ctrl Pts',(3.70386557353965,1.33723749073094,28.6138506187664));
#49989=CARTESIAN_POINT('Ctrl Pts',(3.54828452094279,1.19737007452087,28.6961104621874));
#49990=CARTESIAN_POINT('Ctrl Pts',(3.44951340905803,1.13323856352731,28.7289273827889));
#49991=CARTESIAN_POINT('Ctrl Pts',(3.23168171745139,1.04603454643297,28.7711580288679));
#49992=CARTESIAN_POINT('Ctrl Pts',(3.11251830314535,1.0233954778954,28.780934390951));
#49993=CARTESIAN_POINT('Ctrl Pts',(3.,1.0233954778954,28.780934390951));
#49994=CARTESIAN_POINT('Origin',(4.95,0.,26.5));
#49995=CARTESIAN_POINT('',(4.96464466094067,2.43535533905933,26.5));
#49996=CARTESIAN_POINT('',(4.96464466094067,-2.43535533905933,26.5));
#49997=CARTESIAN_POINT('Origin',(4.96464466094067,0.,26.5));
#49998=CARTESIAN_POINT('Origin',(4.96464466094067,0.,26.5));
#49999=CARTESIAN_POINT('',(4.95,-2.45,26.5));
#50000=CARTESIAN_POINT('Origin',(0.907322330470336,0.,26.5));
#50001=CARTESIAN_POINT('',(0.864644660940672,2.46464466094067,26.5));
#50002=CARTESIAN_POINT('',(0.907322330470336,2.48232233047034,26.5));
#50003=CARTESIAN_POINT('',(0.864644660940673,-2.46464466094067,26.5));
#50004=CARTESIAN_POINT('Origin',(0.864644660940672,0.,26.5));
#50005=CARTESIAN_POINT('Origin',(0.864644660940672,0.,26.5));
#50006=CARTESIAN_POINT('Origin',(0.85,0.,26.5));
#50007=CARTESIAN_POINT('',(0.835355339059327,-2.43535533905933,26.5));
#50008=CARTESIAN_POINT('',(0.85,-2.45,26.5));
#50009=CARTESIAN_POINT('',(0.835355339059327,2.43535533905933,26.5));
#50010=CARTESIAN_POINT('Origin',(0.835355339059327,0.,26.5));
#50011=CARTESIAN_POINT('Origin',(0.835355339059327,0.,26.5));
#50012=CARTESIAN_POINT('Origin',(0.817677669529664,0.,26.5));
#50013=CARTESIAN_POINT('',(0.8,2.35,26.5));
#50014=CARTESIAN_POINT('',(0.817677669529664,2.39267766952966,26.5));
#50015=CARTESIAN_POINT('Origin',(0.8,0.,26.5));
#50016=CARTESIAN_POINT('Origin',(0.8,2.4,26.5));
#50017=CARTESIAN_POINT('',(0.8,-0.46,26.5));
#50018=CARTESIAN_POINT('Origin',(0.8,0.,26.5));
#50019=CARTESIAN_POINT('Origin',(4.98232233047034,0.,26.5));
#50020=CARTESIAN_POINT('',(5.,2.35,26.5));
#50021=CARTESIAN_POINT('Origin',(5.,0.,26.5));
#50022=CARTESIAN_POINT('',(4.98232233047034,2.39267766952966,26.5));
#50023=CARTESIAN_POINT('Origin',(5.,1.,26.5));
#50024=CARTESIAN_POINT('',(5.,0.3025,27.453149384934));
#50025=CARTESIAN_POINT('',(5.,0.3025,27.78));
#50026=CARTESIAN_POINT('',(5.,0.3025,27.115));
#50027=CARTESIAN_POINT('',(5.,-0.3025,27.453149384934));
#50028=CARTESIAN_POINT('Origin',(5.,0.,26.5));
#50029=CARTESIAN_POINT('',(5.,-0.3025,27.78));
#50030=CARTESIAN_POINT('',(5.,-0.3025,27.115));
#50031=CARTESIAN_POINT('',(5.,0.5,27.78));
#50032=CARTESIAN_POINT('Origin',(4.975,0.2775,27.115));
#50033=CARTESIAN_POINT('',(4.95,0.2525,27.73));
#50034=CARTESIAN_POINT('',(4.95,0.2525,27.4675968943729));
#50035=CARTESIAN_POINT('',(4.95,0.2525,27.115));
#50036=CARTESIAN_POINT('Origin',(4.6975,0.,26.5));
#50037=CARTESIAN_POINT('',(5.,0.3025,27.78));
#50038=CARTESIAN_POINT('Origin',(4.975,-0.2775,27.115));
#50039=CARTESIAN_POINT('',(4.95,-0.2525,27.4675968943729));
#50040=CARTESIAN_POINT('Origin',(4.69750000000001,0.,26.5));
#50041=CARTESIAN_POINT('',(4.95,-0.2525,27.73));
#50042=CARTESIAN_POINT('',(4.95,-0.2525,27.115));
#50043=CARTESIAN_POINT('',(4.95,-0.2525,27.73));
#50044=CARTESIAN_POINT('Origin',(4.975,0.5,27.755));
#50045=CARTESIAN_POINT('',(4.95,0.5,27.73));
#50046=CARTESIAN_POINT('Origin',(3.2,0.,27.73));
#50047=CARTESIAN_POINT('',(1.3,-0.2525,27.73));
#50048=CARTESIAN_POINT('',(1.3,-0.2525,27.73));
#50049=CARTESIAN_POINT('',(1.3,0.2525,27.73));
#50050=CARTESIAN_POINT('',(1.3,0.2525,27.73));
#50051=CARTESIAN_POINT('',(5.1,0.2525,27.73));
#50052=CARTESIAN_POINT('Origin',(5.1,-0.2525,27.73));
#50053=CARTESIAN_POINT('',(1.3,-0.2525,27.4675968943729));
#50054=CARTESIAN_POINT('',(3.15,-0.2525,27.4675968943729));
#50055=CARTESIAN_POINT('',(1.3,-0.2525,27.73));
#50056=CARTESIAN_POINT('Origin',(1.3,0.2525,27.73));
#50057=CARTESIAN_POINT('',(1.3,0.2525,27.4675968943729));
#50058=CARTESIAN_POINT('',(1.3,0.2525,27.73));
#50059=CARTESIAN_POINT('',(3.15,0.2525,27.4675968943729));
#50060=CARTESIAN_POINT('Origin',(3.15,0.,26.5));
#50061=CARTESIAN_POINT('Origin',(1.3,0.,26.5));
#50062=CARTESIAN_POINT('Origin',(3.,4.17193000900063,22.3280699909994));
#50063=CARTESIAN_POINT('',(3.65899840720328,6.73112601132474,19.7688739886753));
#50064=CARTESIAN_POINT('',(3.,6.08767497843372,19.4693376302832));
#50065=CARTESIAN_POINT('Ctrl Pts',(3.65899840720328,6.73112601132474,19.7688739886753));
#50066=CARTESIAN_POINT('Ctrl Pts',(3.65899840720328,6.72679268575653,19.764540663107));
#50067=CARTESIAN_POINT('Ctrl Pts',(3.65891512098012,6.72241218185797,19.7602566839318));
#50068=CARTESIAN_POINT('Ctrl Pts',(3.65781547543884,6.69317457331001,19.7322924236316));
#50069=CARTESIAN_POINT('Ctrl Pts',(3.65428413830508,6.66710502404872,19.7103330586802));
#50070=CARTESIAN_POINT('Ctrl Pts',(3.63870034113718,6.59727918356102,19.6581255858253));
#50071=CARTESIAN_POINT('Ctrl Pts',(3.62306713231032,6.55278988756777,19.6310282895777));
#50072=CARTESIAN_POINT('Ctrl Pts',(3.56551968033953,6.43088892463072,19.5676842688384));
#50073=CARTESIAN_POINT('Ctrl Pts',(3.51273077708496,6.3539988734894,19.53969222603));
#50074=CARTESIAN_POINT('Ctrl Pts',(3.3884774805394,6.2283829770698,19.5010021486756));
#50075=CARTESIAN_POINT('Ctrl Pts',(3.3188912623837,6.1772205194954,19.4887543145494));
#50076=CARTESIAN_POINT('Ctrl Pts',(3.17532557849005,6.11134378631976,19.4739796943783));
#50077=CARTESIAN_POINT('Ctrl Pts',(3.10504775292283,6.09288250834592,19.4703811570922));
#50078=CARTESIAN_POINT('Ctrl Pts',(3.02160267663661,6.08799029722494,19.4694006361368));
#50079=CARTESIAN_POINT('Ctrl Pts',(3.01078870740022,6.08767497843372,19.4693376302832));
#50080=CARTESIAN_POINT('Ctrl Pts',(3.,6.08767497843372,19.4693376302832));
#50081=CARTESIAN_POINT('',(3.,7.03066236971681,20.4123250215663));
#50082=CARTESIAN_POINT('Ctrl Pts',(3.,7.03066236971681,20.4123250215663));
#50083=CARTESIAN_POINT('Ctrl Pts',(3.01771871221482,7.03066236971681,20.4123250215663));
#50084=CARTESIAN_POINT('Ctrl Pts',(3.03548526784966,7.03049271525968,20.4114744757539));
#50085=CARTESIAN_POINT('Ctrl Pts',(3.12997701049201,7.02866026735908,20.4023629263842));
#50086=CARTESIAN_POINT('Ctrl Pts',(3.20348422043859,7.02410185118279,20.379195333342));
#50087=CARTESIAN_POINT('Ctrl Pts',(3.34957484663758,7.00637212768387,20.3026046352004));
#50088=CARTESIAN_POINT('Ctrl Pts',(3.41865686125493,6.99216527474278,20.2459676889049));
#50089=CARTESIAN_POINT('Ctrl Pts',(3.53708659094303,6.94832361568055,20.1129667523922));
#50090=CARTESIAN_POINT('Ctrl Pts',(3.5854928838657,6.91741798080179,20.0347556209823));
#50091=CARTESIAN_POINT('Ctrl Pts',(3.6332576564077,6.8511743356788,19.9182014933262));
#50092=CARTESIAN_POINT('Ctrl Pts',(3.64497180237219,6.82563598060614,19.879439709583));
#50093=CARTESIAN_POINT('Ctrl Pts',(3.65660045499355,6.77613678192328,19.8166848017198));
#50094=CARTESIAN_POINT('Ctrl Pts',(3.65899840720328,6.75441124717323,19.7921592245237));
#50095=CARTESIAN_POINT('Ctrl Pts',(3.65899840720328,6.73112601132474,19.7688739886753));
#50096=CARTESIAN_POINT('Ctrl Pts',(3.,6.08767497843372,19.4693376302832));
#50097=CARTESIAN_POINT('Ctrl Pts',(2.93740375632011,6.08767497843372,19.4693376302832));
#50098=CARTESIAN_POINT('Ctrl Pts',(2.87565789134425,6.09830402968064,19.4713955392217));
#50099=CARTESIAN_POINT('Ctrl Pts',(2.73401545070695,6.14671873130702,19.4817369535417));
#50100=CARTESIAN_POINT('Ctrl Pts',(2.65923300361176,6.19233182892452,19.4918543552589));
#50101=CARTESIAN_POINT('Ctrl Pts',(2.52172868443338,6.31191640618337,19.525619137228));
#50102=CARTESIAN_POINT('Ctrl Pts',(2.46172409835092,6.38885879373983,19.5508628055546));
#50103=CARTESIAN_POINT('Ctrl Pts',(2.39060701245704,6.51897766283336,19.6119448626741));
#50104=CARTESIAN_POINT('Ctrl Pts',(2.36956327353234,6.57078939327557,19.6407922394961));
#50105=CARTESIAN_POINT('Ctrl Pts',(2.34883638351778,6.64971896474124,19.6965382745686));
#50106=CARTESIAN_POINT('Ctrl Pts',(2.34397532261961,6.67778206838811,19.7189689436771));
#50107=CARTESIAN_POINT('Ctrl Pts',(2.34028669329881,6.72781049660135,19.7647333834671));
#50108=CARTESIAN_POINT('Ctrl Pts',(2.34077606978153,6.74979295500866,19.7872890495768));
#50109=CARTESIAN_POINT('Ctrl Pts',(2.34680248319783,6.79615911042744,19.8405985114576));
#50110=CARTESIAN_POINT('Ctrl Pts',(2.35349632945342,6.81939902656569,19.8715417922134));
#50111=CARTESIAN_POINT('Ctrl Pts',(2.38103390803266,6.87804712505273,19.9605120359057));
#50112=CARTESIAN_POINT('Ctrl Pts',(2.40863932166359,6.90772580028368,20.0194824078591));
#50113=CARTESIAN_POINT('Ctrl Pts',(2.49309498094617,6.96395620747032,20.1528861413115));
#50114=CARTESIAN_POINT('Ctrl Pts',(2.55769731566219,6.9858385252213,20.2258560176688));
#50115=CARTESIAN_POINT('Ctrl Pts',(2.69643706868986,7.01339895805737,20.3305435155435));
#50116=CARTESIAN_POINT('Ctrl Pts',(2.76629587634974,7.02135172130659,20.3674349512207));
#50117=CARTESIAN_POINT('Ctrl Pts',(2.89345183041008,7.02914761950448,20.404565188633));
#50118=CARTESIAN_POINT('Ctrl Pts',(2.94650789475061,7.03066236971681,20.4123250215663));
#50119=CARTESIAN_POINT('Ctrl Pts',(3.,7.03066236971681,20.4123250215663));
#50120=CARTESIAN_POINT('',(3.,3.62392225358105,21.7800622355798));
#50121=CARTESIAN_POINT('Origin',(3.,-4.17193000900063,22.3280699909994));
#50122=CARTESIAN_POINT('',(3.65899840720328,-6.73112601132475,19.7688739886753));
#50123=CARTESIAN_POINT('',(3.,-7.03066236971681,20.4123250215663));
#50124=CARTESIAN_POINT('Ctrl Pts',(3.65899840720328,-6.73112601132475,19.7688739886753));
#50125=CARTESIAN_POINT('Ctrl Pts',(3.65899840720328,-6.73545933689293,19.7732073142435));
#50126=CARTESIAN_POINT('Ctrl Pts',(3.65891512098013,-6.73974331606821,19.777587818142));
#50127=CARTESIAN_POINT('Ctrl Pts',(3.65781547543884,-6.76770757636838,19.80682542669));
#50128=CARTESIAN_POINT('Ctrl Pts',(3.65428413830508,-6.78966694131985,19.8328949759513));
#50129=CARTESIAN_POINT('Ctrl Pts',(3.63870034113718,-6.84187441417476,19.902720816439));
#50130=CARTESIAN_POINT('Ctrl Pts',(3.6230671323103,-6.86897171042233,19.9472101124323));
#50131=CARTESIAN_POINT('Ctrl Pts',(3.56551968033951,-6.93231573116165,20.0691110753693));
#50132=CARTESIAN_POINT('Ctrl Pts',(3.51273077708492,-6.96030777396999,20.1460011265106));
#50133=CARTESIAN_POINT('Ctrl Pts',(3.38847748053938,-6.99899785132438,20.2716170229302));
#50134=CARTESIAN_POINT('Ctrl Pts',(3.31889126238367,-7.0112456854506,20.3227794805046));
#50135=CARTESIAN_POINT('Ctrl Pts',(3.17532557849002,-7.02602030562166,20.3886562136803));
#50136=CARTESIAN_POINT('Ctrl Pts',(3.10504775292279,-7.0296188429078,20.4071174916541));
#50137=CARTESIAN_POINT('Ctrl Pts',(3.0216026766366,-7.03059936386324,20.4120097027751));
#50138=CARTESIAN_POINT('Ctrl Pts',(3.01078870740021,-7.03066236971681,20.4123250215663));
#50139=CARTESIAN_POINT('Ctrl Pts',(3.,-7.03066236971681,20.4123250215663));
#50140=CARTESIAN_POINT('',(3.,-6.08767497843373,19.4693376302832));
#50141=CARTESIAN_POINT('Ctrl Pts',(3.,-6.08767497843373,19.4693376302832));
#50142=CARTESIAN_POINT('Ctrl Pts',(3.01771871221484,-6.08767497843373,19.4693376302832));
#50143=CARTESIAN_POINT('Ctrl Pts',(3.03548526784968,-6.08852552424608,19.4695072847403));
#50144=CARTESIAN_POINT('Ctrl Pts',(3.12997701049206,-6.09763707361583,19.4713397326409));
#50145=CARTESIAN_POINT('Ctrl Pts',(3.20348422043864,-6.12080466665799,19.4758981488172));
#50146=CARTESIAN_POINT('Ctrl Pts',(3.34957484663764,-6.19739536479959,19.4936278723161));
#50147=CARTESIAN_POINT('Ctrl Pts',(3.41865686125498,-6.25403231109519,19.5078347252572));
#50148=CARTESIAN_POINT('Ctrl Pts',(3.53708659094306,-6.38703324760786,19.5516763843195));
#50149=CARTESIAN_POINT('Ctrl Pts',(3.58549288386572,-6.46524437901772,19.5825820191982));
#50150=CARTESIAN_POINT('Ctrl Pts',(3.63325765640772,-6.58179850667387,19.6488256643212));
#50151=CARTESIAN_POINT('Ctrl Pts',(3.64497180237219,-6.62056029041704,19.6743640193939));
#50152=CARTESIAN_POINT('Ctrl Pts',(3.65660045499355,-6.68331519828019,19.7238632180767));
#50153=CARTESIAN_POINT('Ctrl Pts',(3.65899840720328,-6.70784077547626,19.7455887528268));
#50154=CARTESIAN_POINT('Ctrl Pts',(3.65899840720328,-6.73112601132475,19.7688739886753));
#50155=CARTESIAN_POINT('Ctrl Pts',(3.,-7.03066236971681,20.4123250215663));
#50156=CARTESIAN_POINT('Ctrl Pts',(2.93740375632008,-7.03066236971681,20.4123250215663));
#50157=CARTESIAN_POINT('Ctrl Pts',(2.87565789134422,-7.02860446077828,20.4016959703194));
#50158=CARTESIAN_POINT('Ctrl Pts',(2.73401545070689,-7.01826304645833,20.353281268693));
#50159=CARTESIAN_POINT('Ctrl Pts',(2.6592330036117,-7.00814564474112,20.3076681710754));
#50160=CARTESIAN_POINT('Ctrl Pts',(2.52172868443334,-6.97438086277199,20.1880835938166));
#50161=CARTESIAN_POINT('Ctrl Pts',(2.46172409835089,-6.94913719444542,20.1111412062601));
#50162=CARTESIAN_POINT('Ctrl Pts',(2.39060701245703,-6.88805513732593,19.9810223371666));
#50163=CARTESIAN_POINT('Ctrl Pts',(2.36956327353233,-6.85920776050386,19.9292106067244));
#50164=CARTESIAN_POINT('Ctrl Pts',(2.34883638351777,-6.80346172543135,19.8502810352587));
#50165=CARTESIAN_POINT('Ctrl Pts',(2.34397532261961,-6.78103105632287,19.8222179316119));
#50166=CARTESIAN_POINT('Ctrl Pts',(2.34028669329881,-6.73526661653286,19.7721895033986));
#50167=CARTESIAN_POINT('Ctrl Pts',(2.34077606978153,-6.71271095042321,19.7502070449913));
#50168=CARTESIAN_POINT('Ctrl Pts',(2.34680248319783,-6.65940148854232,19.7038408895725));
#50169=CARTESIAN_POINT('Ctrl Pts',(2.35349632945343,-6.62845820778657,19.6806009734343));
#50170=CARTESIAN_POINT('Ctrl Pts',(2.38103390803267,-6.53948796409423,19.6219528749472));
#50171=CARTESIAN_POINT('Ctrl Pts',(2.40863932166361,-6.48051759214088,19.5922741997163));
#50172=CARTESIAN_POINT('Ctrl Pts',(2.49309498094621,-6.34711385868844,19.5360437925297));
#50173=CARTESIAN_POINT('Ctrl Pts',(2.55769731566224,-6.2741439823312,19.5141614747787));
#50174=CARTESIAN_POINT('Ctrl Pts',(2.6964370686899,-6.16945648445649,19.4866010419426));
#50175=CARTESIAN_POINT('Ctrl Pts',(2.76629587634979,-6.13256504877927,19.4786482786934));
#50176=CARTESIAN_POINT('Ctrl Pts',(2.89345183041011,-6.09543481136695,19.4708523804955));
#50177=CARTESIAN_POINT('Ctrl Pts',(2.94650789475063,-6.08767497843372,19.4693376302832));
#50178=CARTESIAN_POINT('Ctrl Pts',(3.,-6.08767497843372,19.4693376302832));
#50179=CARTESIAN_POINT('',(3.,-4.71993776442021,22.8760777464189));
#50180=CARTESIAN_POINT('Origin',(3.,-4.17193000900063,30.6719300090006));
#50181=CARTESIAN_POINT('',(3.65899840720328,-6.73112601132474,33.2311260113247));
#50182=CARTESIAN_POINT('',(3.,-6.08767497843372,33.5306623697168));
#50183=CARTESIAN_POINT('Ctrl Pts',(3.65899840720328,-6.73112601132474,33.2311260113247));
#50184=CARTESIAN_POINT('Ctrl Pts',(3.65899840720328,-6.72679268575659,33.2354593368929));
#50185=CARTESIAN_POINT('Ctrl Pts',(3.65891512098013,-6.72241218185809,33.2397433160682));
#50186=CARTESIAN_POINT('Ctrl Pts',(3.65781547543884,-6.69317457330999,33.2677075763684));
#50187=CARTESIAN_POINT('Ctrl Pts',(3.65428413830508,-6.6671050240487,33.2896669413199));
#50188=CARTESIAN_POINT('Ctrl Pts',(3.63870034113717,-6.59727918356096,33.3418744141748));
#50189=CARTESIAN_POINT('Ctrl Pts',(3.62306713231028,-6.55278988756768,33.3689717104224));
#50190=CARTESIAN_POINT('Ctrl Pts',(3.5655196803395,-6.43088892463065,33.4323157311617));
#50191=CARTESIAN_POINT('Ctrl Pts',(3.51273077708491,-6.35399887348934,33.46030777397));
#50192=CARTESIAN_POINT('Ctrl Pts',(3.38847748053935,-6.22838297706974,33.4989978513244));
#50193=CARTESIAN_POINT('Ctrl Pts',(3.31889126238363,-6.17722051949536,33.5112456854506));
#50194=CARTESIAN_POINT('Ctrl Pts',(3.17532557849001,-6.11134378631973,33.5260203056217));
#50195=CARTESIAN_POINT('Ctrl Pts',(3.10504775292278,-6.09288250834591,33.5296188429078));
#50196=CARTESIAN_POINT('Ctrl Pts',(3.02160267663661,-6.08799029722494,33.5305993638632));
#50197=CARTESIAN_POINT('Ctrl Pts',(3.01078870740022,-6.08767497843372,33.5306623697168));
#50198=CARTESIAN_POINT('Ctrl Pts',(3.,-6.08767497843372,33.5306623697168));
#50199=CARTESIAN_POINT('',(3.,-7.03066236971681,32.5876749784337));
#50200=CARTESIAN_POINT('Ctrl Pts',(3.,-7.03066236971681,32.5876749784337));
#50201=CARTESIAN_POINT('Ctrl Pts',(3.01771871221484,-7.03066236971681,32.5876749784337));
#50202=CARTESIAN_POINT('Ctrl Pts',(3.03548526784969,-7.03049271525968,32.5885255242461));
#50203=CARTESIAN_POINT('Ctrl Pts',(3.1299770104921,-7.02866026735908,32.5976370736158));
#50204=CARTESIAN_POINT('Ctrl Pts',(3.20348422043866,-7.02410185118278,32.620804666658));
#50205=CARTESIAN_POINT('Ctrl Pts',(3.34957484663769,-7.00637212768386,32.6973953647996));
#50206=CARTESIAN_POINT('Ctrl Pts',(3.41865686125501,-6.99216527474276,32.7540323110952));
#50207=CARTESIAN_POINT('Ctrl Pts',(3.53708659094313,-6.94832361568051,32.8870332476079));
#50208=CARTESIAN_POINT('Ctrl Pts',(3.58549288386575,-6.91741798080174,32.9652443790178));
#50209=CARTESIAN_POINT('Ctrl Pts',(3.63325765640772,-6.85117433567877,33.0817985066739));
#50210=CARTESIAN_POINT('Ctrl Pts',(3.6449718023722,-6.8256359806061,33.1205602904171));
#50211=CARTESIAN_POINT('Ctrl Pts',(3.65660045499355,-6.77613678192326,33.1833151982802));
#50212=CARTESIAN_POINT('Ctrl Pts',(3.65899840720328,-6.75441124717321,33.2078407754763));
#50213=CARTESIAN_POINT('Ctrl Pts',(3.65899840720328,-6.73112601132474,33.2311260113247));
#50214=CARTESIAN_POINT('Ctrl Pts',(3.,-6.08767497843372,33.5306623697168));
#50215=CARTESIAN_POINT('Ctrl Pts',(2.93740375632004,-6.08767497843372,33.5306623697168));
#50216=CARTESIAN_POINT('Ctrl Pts',(2.87565789134417,-6.09830402968066,33.5286044607783));
#50217=CARTESIAN_POINT('Ctrl Pts',(2.7340154507069,-6.14671873130704,33.5182630464583));
#50218=CARTESIAN_POINT('Ctrl Pts',(2.65923300361173,-6.19233182892453,33.5081456447411));
#50219=CARTESIAN_POINT('Ctrl Pts',(2.52172868443329,-6.31191640618344,33.474380862772));
#50220=CARTESIAN_POINT('Ctrl Pts',(2.46172409835087,-6.38885879373992,33.4491371944454));
#50221=CARTESIAN_POINT('Ctrl Pts',(2.39060701245703,-6.51897766283339,33.3880551373259));
#50222=CARTESIAN_POINT('Ctrl Pts',(2.36956327353233,-6.57078939327562,33.3592077605039));
#50223=CARTESIAN_POINT('Ctrl Pts',(2.34883638351776,-6.64971896474131,33.3034617254313));
#50224=CARTESIAN_POINT('Ctrl Pts',(2.3439753226196,-6.67778206838815,33.2810310563229));
#50225=CARTESIAN_POINT('Ctrl Pts',(2.34028669329881,-6.72781049660138,33.2352666165328));
#50226=CARTESIAN_POINT('Ctrl Pts',(2.34077606978153,-6.74979295500869,33.2127109504232));
#50227=CARTESIAN_POINT('Ctrl Pts',(2.34680248319783,-6.79615911042747,33.1594014885423));
#50228=CARTESIAN_POINT('Ctrl Pts',(2.35349632945343,-6.81939902656572,33.1284582077866));
#50229=CARTESIAN_POINT('Ctrl Pts',(2.38103390803268,-6.87804712505278,33.0394879640942));
#50230=CARTESIAN_POINT('Ctrl Pts',(2.40863932166365,-6.90772580028372,32.9805175921408));
#50231=CARTESIAN_POINT('Ctrl Pts',(2.49309498094623,-6.96395620747035,32.8471138586884));
#50232=CARTESIAN_POINT('Ctrl Pts',(2.55769731566228,-6.98583852522132,32.7741439823312));
#50233=CARTESIAN_POINT('Ctrl Pts',(2.69643706868993,-7.01339895805738,32.6694564844565));
#50234=CARTESIAN_POINT('Ctrl Pts',(2.76629587634983,-7.0213517213066,32.6325650487793));
#50235=CARTESIAN_POINT('Ctrl Pts',(2.89345183041014,-7.02914761950449,32.5954348113669));
#50236=CARTESIAN_POINT('Ctrl Pts',(2.94650789475066,-7.03066236971681,32.5876749784337));
#50237=CARTESIAN_POINT('Ctrl Pts',(3.,-7.03066236971681,32.5876749784337));
#50238=CARTESIAN_POINT('',(3.,-3.62392225358105,31.2199377644202));
#50239=CARTESIAN_POINT('Origin',(3.,4.17193000900063,30.6719300090006));
#50240=CARTESIAN_POINT('',(3.65899840720327,6.73112601132474,33.2311260113247));
#50241=CARTESIAN_POINT('',(3.,7.0306623697168,32.5876749784337));
#50242=CARTESIAN_POINT('Ctrl Pts',(3.65899840720327,6.73112601132474,33.2311260113247));
#50243=CARTESIAN_POINT('Ctrl Pts',(3.65899840720327,6.7354593368928,33.2267926857567));
#50244=CARTESIAN_POINT('Ctrl Pts',(3.65891512098013,6.73974331606797,33.2224121818583));
#50245=CARTESIAN_POINT('Ctrl Pts',(3.65781547543883,6.76770757636843,33.1931745733099));
#50246=CARTESIAN_POINT('Ctrl Pts',(3.65428413830506,6.7896669413199,33.1671050240486));
#50247=CARTESIAN_POINT('Ctrl Pts',(3.63870034113715,6.84187441417481,33.0972791835609));
#50248=CARTESIAN_POINT('Ctrl Pts',(3.62306713231026,6.86897171042236,33.0527898875676));
#50249=CARTESIAN_POINT('Ctrl Pts',(3.56551968033943,6.93231573116172,32.9308889246305));
#50250=CARTESIAN_POINT('Ctrl Pts',(3.51273077708478,6.96030777397002,32.8539988734892));
#50251=CARTESIAN_POINT('Ctrl Pts',(3.38847748053925,6.99899785132441,32.7283829770697));
#50252=CARTESIAN_POINT('Ctrl Pts',(3.31889126238351,7.01124568545061,32.6772205194953));
#50253=CARTESIAN_POINT('Ctrl Pts',(3.1753255784899,7.02602030562166,32.6113437863197));
#50254=CARTESIAN_POINT('Ctrl Pts',(3.10504775292266,7.02961884290778,32.5928825083459));
#50255=CARTESIAN_POINT('Ctrl Pts',(3.0216026766366,7.03059936386323,32.587990297225));
#50256=CARTESIAN_POINT('Ctrl Pts',(3.01078870740021,7.0306623697168,32.5876749784337));
#50257=CARTESIAN_POINT('Ctrl Pts',(3.,7.0306623697168,32.5876749784337));
#50258=CARTESIAN_POINT('',(3.,6.08767497843373,33.5306623697168));
#50259=CARTESIAN_POINT('Ctrl Pts',(3.,6.08767497843373,33.5306623697168));
#50260=CARTESIAN_POINT('Ctrl Pts',(3.01771871221484,6.08767497843373,33.5306623697168));
#50261=CARTESIAN_POINT('Ctrl Pts',(3.03548526784969,6.08852552424608,33.5304927152597));
#50262=CARTESIAN_POINT('Ctrl Pts',(3.12997701049221,6.09763707361585,33.5286602673591));
#50263=CARTESIAN_POINT('Ctrl Pts',(3.20348422043877,6.12080466665807,33.5241018511828));
#50264=CARTESIAN_POINT('Ctrl Pts',(3.34957484663778,6.19739536479966,33.5063721276838));
#50265=CARTESIAN_POINT('Ctrl Pts',(3.41865686125508,6.2540323110953,33.4921652747427));
#50266=CARTESIAN_POINT('Ctrl Pts',(3.53708659094318,6.38703324760799,33.4483236156805));
#50267=CARTESIAN_POINT('Ctrl Pts',(3.58549288386577,6.46524437901786,33.4174179808017));
#50268=CARTESIAN_POINT('Ctrl Pts',(3.63325765640775,6.58179850667398,33.3511743356787));
#50269=CARTESIAN_POINT('Ctrl Pts',(3.6449718023722,6.62056029041712,33.325635980606));
#50270=CARTESIAN_POINT('Ctrl Pts',(3.65660045499355,6.68331519828023,33.2761367819232));
#50271=CARTESIAN_POINT('Ctrl Pts',(3.65899840720327,6.7078407754763,33.2544112471732));
#50272=CARTESIAN_POINT('Ctrl Pts',(3.65899840720327,6.73112601132474,33.2311260113247));
#50273=CARTESIAN_POINT('Ctrl Pts',(3.,7.0306623697168,32.5876749784337));
#50274=CARTESIAN_POINT('Ctrl Pts',(2.93740375631998,7.0306623697168,32.5876749784337));
#50275=CARTESIAN_POINT('Ctrl Pts',(2.87565789134411,7.02860446077826,32.5983040296807));
#50276=CARTESIAN_POINT('Ctrl Pts',(2.73401545070677,7.01826304645831,32.6467187313071));
#50277=CARTESIAN_POINT('Ctrl Pts',(2.65923300361162,7.0081456447411,32.6923318289246));
#50278=CARTESIAN_POINT('Ctrl Pts',(2.52172868443319,6.97438086277194,32.8119164061835));
#50279=CARTESIAN_POINT('Ctrl Pts',(2.46172409835081,6.94913719444534,32.88885879374));
#50280=CARTESIAN_POINT('Ctrl Pts',(2.39060701245699,6.88805513732588,33.0189776628335));
#50281=CARTESIAN_POINT('Ctrl Pts',(2.36956327353232,6.85920776050379,33.0707893932757));
#50282=CARTESIAN_POINT('Ctrl Pts',(2.34883638351776,6.80346172543131,33.1497189647413));
#50283=CARTESIAN_POINT('Ctrl Pts',(2.34397532261961,6.78103105632281,33.1777820683882));
#50284=CARTESIAN_POINT('Ctrl Pts',(2.34028669329882,6.73526661653279,33.2278104966014));
#50285=CARTESIAN_POINT('Ctrl Pts',(2.34077606978155,6.71271095042312,33.2497929550087));
#50286=CARTESIAN_POINT('Ctrl Pts',(2.34680248319785,6.65940148854226,33.2961591104275));
#50287=CARTESIAN_POINT('Ctrl Pts',(2.35349632945345,6.62845820778652,33.3193990265657));
#50288=CARTESIAN_POINT('Ctrl Pts',(2.38103390803271,6.53948796409412,33.3780471250528));
#50289=CARTESIAN_POINT('Ctrl Pts',(2.40863932166368,6.48051759214078,33.4077258002837));
#50290=CARTESIAN_POINT('Ctrl Pts',(2.49309498094631,6.34711385868828,33.4639562074704));
#50291=CARTESIAN_POINT('Ctrl Pts',(2.55769731566239,6.27414398233109,33.4858385252213));
#50292=CARTESIAN_POINT('Ctrl Pts',(2.69643706869003,6.16945648445639,33.5133989580574));
#50293=CARTESIAN_POINT('Ctrl Pts',(2.76629587634994,6.13256504877923,33.5213517213066));
#50294=CARTESIAN_POINT('Ctrl Pts',(2.89345183041017,6.09543481136693,33.5291476195045));
#50295=CARTESIAN_POINT('Ctrl Pts',(2.94650789475069,6.08767497843373,33.5306623697168));
#50296=CARTESIAN_POINT('Ctrl Pts',(3.,6.08767497843373,33.5306623697168));
#50297=CARTESIAN_POINT('',(3.,4.7199377644202,30.1239222535811));
#50298=CARTESIAN_POINT('Origin',(3.,0.,26.5));
#50299=CARTESIAN_POINT('',(3.,-1.13892152320704E-15,35.8));
#50300=CARTESIAN_POINT('Origin',(3.,-1.27363267111325E-15,36.9));
#50301=CARTESIAN_POINT('Origin',(3.,0.,26.5));
#50302=CARTESIAN_POINT('Origin',(3.,0.,26.5));
#50303=CARTESIAN_POINT('Origin',(3.,0.,26.5));
#50304=CARTESIAN_POINT('Origin',(3.,0.,26.5));
#50305=CARTESIAN_POINT('Origin',(3.,0.,26.5));
#50306=CARTESIAN_POINT('Origin',(1.05,0.,26.5));
#50307=CARTESIAN_POINT('',(1.3,-0.46,26.5));
#50308=CARTESIAN_POINT('Origin',(1.3,0.,26.5));
#50309=CARTESIAN_POINT('',(1.05,-0.46,26.5));
#50310=CARTESIAN_POINT('Origin',(1.3,0.46,26.5));
#50311=CARTESIAN_POINT('',(0.,0.,0.));
#50312=CARTESIAN_POINT('Origin',(0.,0.,-0.975));
#50313=CARTESIAN_POINT('',(-0.393684988231328,0.000287216083460287,-1.9162836477965));
#50314=CARTESIAN_POINT('',(-0.393656552223556,0.000403437008091592,-1.9346163522035));
#50315=CARTESIAN_POINT('',(-0.3933,-4.81653586104654E-17,-0.975));
#50316=CARTESIAN_POINT('',(0.175074362083496,0.352527701706987,-1.9567));
#50317=CARTESIAN_POINT('Ctrl Pts',(-0.393684988231328,0.000287216083460287,
-1.9162836477965));
#50318=CARTESIAN_POINT('Ctrl Pts',(-0.393812206257712,0.016808807481143,
-1.91712178211581));
#50319=CARTESIAN_POINT('Ctrl Pts',(-0.392861270962247,0.0333148644649716,
-1.91795991643512));
#50320=CARTESIAN_POINT('Ctrl Pts',(-0.390782425694577,0.0496765903311048,
-1.91879805075443));
#50321=CARTESIAN_POINT('Ctrl Pts',(-0.37447258502525,0.178044557924503,
-1.92537373843066));
#50322=CARTESIAN_POINT('Ctrl Pts',(-0.288735561555079,0.297528391908798,
-1.93194942610689));
#50323=CARTESIAN_POINT('Ctrl Pts',(-0.172352287678191,0.354187200525085,
-1.93852511378312));
#50324=CARTESIAN_POINT('Ctrl Pts',(-0.0651263535802379,0.406387946185369,
-1.94458340918875));
#50325=CARTESIAN_POINT('Ctrl Pts',(0.0681129064719315,0.405261193659393,
-1.95064170459437));
#50326=CARTESIAN_POINT('Ctrl Pts',(0.175279276633879,0.352769203968886,
-1.9567));
#50327=CARTESIAN_POINT('',(-0.17486944753311,0.352286199445089,-1.9567));
#50328=CARTESIAN_POINT('Origin',(0.,0.,-1.9567));
#50329=CARTESIAN_POINT('Ctrl Pts',(-0.17486944753311,0.352286199445089,
-1.9567));
#50330=CARTESIAN_POINT('Ctrl Pts',(-0.291310645032561,0.294486581098141,
-1.95012431232377));
#50331=CARTESIAN_POINT('Ctrl Pts',(-0.375888601233118,0.174960586654857,
-1.94354862464754));
#50332=CARTESIAN_POINT('Ctrl Pts',(-0.391123834940899,0.0466546186985258,
-1.93697293697131));
#50333=CARTESIAN_POINT('Ctrl Pts',(-0.392943828096371,0.0313272539881675,
-1.93618740871537));
#50334=CARTESIAN_POINT('Ctrl Pts',(-0.393774261195228,0.0158745940662237,
-1.93540188045944));
#50335=CARTESIAN_POINT('Ctrl Pts',(-0.393656552223556,0.000403437008091592,
-1.9346163522035));
#50336=CARTESIAN_POINT('Origin',(0.,0.,-0.975));
#50337=CARTESIAN_POINT('',(-0.392686056089118,7.50994904183955E-5,-1.7912836477965));
#50338=CARTESIAN_POINT('',(-0.392691811994703,9.34764795687181E-5,-1.8096163522035));
#50339=CARTESIAN_POINT('',(-0.3933,-4.81653586104654E-17,-0.975));
#50340=CARTESIAN_POINT('Ctrl Pts',(-0.392686056089118,7.50994904183955E-5,
-1.7912836477965));
#50341=CARTESIAN_POINT('Ctrl Pts',(-0.392790040690049,0.0606067827725276,
-1.79433432272509));
#50342=CARTESIAN_POINT('Ctrl Pts',(-0.379632353738202,0.121095544704464,
-1.79738499765368));
#50343=CARTESIAN_POINT('Ctrl Pts',(-0.352975241504574,0.174895223853803,
-1.80043567258227));
#50344=CARTESIAN_POINT('Ctrl Pts',(-0.295516204241772,0.290859689242099,
-1.8070113602585));
#50345=CARTESIAN_POINT('Ctrl Pts',(-0.17533720758107,0.375745868571807,
-1.81358704793474));
#50346=CARTESIAN_POINT('Ctrl Pts',(-0.0468355728346856,0.391133692962758,
-1.82016273561097));
#50347=CARTESIAN_POINT('Ctrl Pts',(0.0816660619116985,0.406521517353708,
-1.8267384232872));
#50348=CARTESIAN_POINT('Ctrl Pts',(0.218490334743764,0.3524109868059,-1.83331411096343));
#50349=CARTESIAN_POINT('Ctrl Pts',(0.301704002577892,0.253289260265722,
-1.83988979863966));
#50350=CARTESIAN_POINT('Ctrl Pts',(0.384917670412021,0.154167533725544,
-1.84646548631589));
#50351=CARTESIAN_POINT('Ctrl Pts',(0.414520733248213,0.0100346111929961,
-1.85304117399212));
#50352=CARTESIAN_POINT('Ctrl Pts',(0.377115660733795,-0.11385867192349,
-1.85961686166835));
#50353=CARTESIAN_POINT('Ctrl Pts',(0.339710588219377,-0.237751955039975,
-1.86619254934458));
#50354=CARTESIAN_POINT('Ctrl Pts',(0.235297380354349,-0.341405598740398,
-1.87276823702081));
#50355=CARTESIAN_POINT('Ctrl Pts',(0.111133817323469,-0.377921810128355,
-1.87934392469704));
#50356=CARTESIAN_POINT('Ctrl Pts',(-0.0130297457074104,-0.414438021516312,
-1.88591961237327));
#50357=CARTESIAN_POINT('Ctrl Pts',(-0.156943663904142,-0.383816800591803,
-1.8924953000495));
#50358=CARTESIAN_POINT('Ctrl Pts',(-0.255459294068266,-0.299880139528298,
-1.89907098772573));
#50359=CARTESIAN_POINT('Ctrl Pts',(-0.341418164438697,-0.226642009135542,
-1.90480854108266));
#50360=CARTESIAN_POINT('Ctrl Pts',(-0.392814101313171,-0.112813405143687,
-1.91054609443958));
#50361=CARTESIAN_POINT('Ctrl Pts',(-0.393684988231328,0.000287216083460287,
-1.9162836477965));
#50362=CARTESIAN_POINT('Ctrl Pts',(-0.393656552223556,0.000403437008091592,
-1.9346163522035));
#50363=CARTESIAN_POINT('Ctrl Pts',(-0.392788914801179,-0.11363506524309,
-1.9288261927832));
#50364=CARTESIAN_POINT('Ctrl Pts',(-0.340406617480196,-0.228678557895452,
-1.92303603336291));
#50365=CARTESIAN_POINT('Ctrl Pts',(-0.253096937644416,-0.301956026031023,
-1.91724587394262));
#50366=CARTESIAN_POINT('Ctrl Pts',(-0.153942295425146,-0.385174761334857,
-1.91067018626639));
#50367=CARTESIAN_POINT('Ctrl Pts',(-0.00974049977160341,-0.414526290473145,
-1.90409449859016));
#50368=CARTESIAN_POINT('Ctrl Pts',(0.114141367823281,-0.37699543192958,
-1.89751881091392));
#50369=CARTESIAN_POINT('Ctrl Pts',(0.238023235418165,-0.339464573386015,
-1.89094312323769));
#50370=CARTESIAN_POINT('Ctrl Pts',(0.341585174954392,-0.235051327160598,
-1.88436743556146));
#50371=CARTESIAN_POINT('Ctrl Pts',(0.378000101690373,-0.110880914803365,
-1.87779174788523));
#50372=CARTESIAN_POINT('Ctrl Pts',(0.414415028426353,0.0132894975538674,
-1.871216060209));
#50373=CARTESIAN_POINT('Ctrl Pts',(0.383682942362089,0.157217076042915,
-1.86464037253277));
#50374=CARTESIAN_POINT('Ctrl Pts',(0.2996888006567,0.255683706134081,-1.85806468485654));
#50375=CARTESIAN_POINT('Ctrl Pts',(0.21569465895131,0.354150336225248,-1.85148899718031));
#50376=CARTESIAN_POINT('Ctrl Pts',(0.0784384616047951,0.407156017918534,
-1.84491330950408));
#50377=CARTESIAN_POINT('Ctrl Pts',(-0.0499387246305632,0.390745066784524,
-1.83833762182785));
#50378=CARTESIAN_POINT('Ctrl Pts',(-0.178315910865922,0.374334115650513,
-1.83176193415162));
#50379=CARTESIAN_POINT('Ctrl Pts',(-0.297814085990123,0.288506531689206,
-1.82518624647539));
#50380=CARTESIAN_POINT('Ctrl Pts',(-0.354350523610512,0.172092132577462,
-1.81861055879916));
#50381=CARTESIAN_POINT('Ctrl Pts',(-0.380127315594231,0.119015039712826,
-1.81561248993394));
#50382=CARTESIAN_POINT('Ctrl Pts',(-0.392815978841773,0.0595797332697563,
-1.81261442106872));
#50383=CARTESIAN_POINT('Ctrl Pts',(-0.392691811994703,9.34764795687181E-5,
-1.8096163522035));
#50384=CARTESIAN_POINT('Origin',(0.,0.,-0.975));
#50385=CARTESIAN_POINT('',(-0.393429058327419,-0.000336684366980755,-1.6662836477965));
#50386=CARTESIAN_POINT('',(-0.393398187730971,-0.000340795866165029,-1.6846163522035));
#50387=CARTESIAN_POINT('',(-0.3933,-4.81653586104654E-17,-0.975));
#50388=CARTESIAN_POINT('Ctrl Pts',(-0.393429058327419,-0.000336684366980755,
-1.6662836477965));
#50389=CARTESIAN_POINT('Ctrl Pts',(-0.392492058309276,0.103596594079765,
-1.67154686333438));
#50390=CARTESIAN_POINT('Ctrl Pts',(-0.350086285532408,0.208206253664161,
-1.67681007887225));
#50391=CARTESIAN_POINT('Ctrl Pts',(-0.276234805241032,0.280845339194954,
-1.68207329441012));
#50392=CARTESIAN_POINT('Ctrl Pts',(-0.183967204697426,0.371598213763818,
-1.68864898208635));
#50393=CARTESIAN_POINT('Ctrl Pts',(-0.0426154383454463,0.412447648980525,
-1.69522466976258));
#50394=CARTESIAN_POINT('Ctrl Pts',(0.0838389849720331,0.384903597594179,
-1.70180035743881));
#50395=CARTESIAN_POINT('Ctrl Pts',(0.210293408289513,0.357359546207833,
-1.70837604511505));
#50396=CARTESIAN_POINT('Ctrl Pts',(0.321850488572492,0.261422008218435,
-1.71495173279128));
#50397=CARTESIAN_POINT('Ctrl Pts',(0.368014963339217,0.140516079073615,
-1.72152742046751));
#50398=CARTESIAN_POINT('Ctrl Pts',(0.414179438105941,0.0196101499287949,
-1.72810310814374));
#50399=CARTESIAN_POINT('Ctrl Pts',(0.394951307356412,-0.126264170371447,
-1.73467879581997));
#50400=CARTESIAN_POINT('Ctrl Pts',(0.319034040445492,-0.231078060471686,
-1.7412544834962));
#50401=CARTESIAN_POINT('Ctrl Pts',(0.243116773534572,-0.335891950571925,
-1.74783017117243));
#50402=CARTESIAN_POINT('Ctrl Pts',(0.110510370462263,-0.399645410472161,
-1.75440585884866));
#50403=CARTESIAN_POINT('Ctrl Pts',(-0.0187622313884131,-0.393481452764923,
-1.76098154652489));
#50404=CARTESIAN_POINT('Ctrl Pts',(-0.148034833239089,-0.387317495057686,
-1.76755723420112));
#50405=CARTESIAN_POINT('Ctrl Pts',(-0.273973633868132,-0.311236119742974,
-1.77413292187735));
#50406=CARTESIAN_POINT('Ctrl Pts',(-0.339573495250203,-0.199674056362176,
-1.78070860955358));
#50407=CARTESIAN_POINT('Ctrl Pts',(-0.374739451877235,-0.139869254958381,
-1.78423362230122));
#50408=CARTESIAN_POINT('Ctrl Pts',(-0.392565903318857,-0.0698684245494068,
-1.78775863504886));
#50409=CARTESIAN_POINT('Ctrl Pts',(-0.392686056089118,7.50994904183955E-5,
-1.7912836477965));
#50410=CARTESIAN_POINT('Ctrl Pts',(-0.392691811994703,9.34764795687181E-5,
-1.8096163522035));
#50411=CARTESIAN_POINT('Ctrl Pts',(-0.392543642733838,-0.0708919347490211,
-1.80603873339249));
#50412=CARTESIAN_POINT('Ctrl Pts',(-0.374150216296977,-0.141949898425392,
-1.80246111458148));
#50413=CARTESIAN_POINT('Ctrl Pts',(-0.3379793340135,-0.202362794921726,
-1.79888349577047));
#50414=CARTESIAN_POINT('Ctrl Pts',(-0.271497006679522,-0.31340210904699,
-1.79230780809423));
#50415=CARTESIAN_POINT('Ctrl Pts',(-0.144957651894991,-0.388479523035339,
-1.785732120418));
#50416=CARTESIAN_POINT('Ctrl Pts',(-0.0156399934846813,-0.393617199251612,
-1.77915643274177));
#50417=CARTESIAN_POINT('Ctrl Pts',(0.113677664925628,-0.398754875467886,
-1.77258074506554));
#50418=CARTESIAN_POINT('Ctrl Pts',(0.245773626961716,-0.333952813912084,
-1.76600505738931));
#50419=CARTESIAN_POINT('Ctrl Pts',(0.320856915188691,-0.228540314522024,
-1.75942936971308));
#50420=CARTESIAN_POINT('Ctrl Pts',(0.395940203415666,-0.123127815131962,
-1.75285368203685));
#50421=CARTESIAN_POINT('Ctrl Pts',(0.414010817833527,0.0228951220923579,
-1.74627799436062));
#50422=CARTESIAN_POINT('Ctrl Pts',(0.366888750868655,0.143431191298164,
-1.73970230668439));
#50423=CARTESIAN_POINT('Ctrl Pts',(0.319766683903784,0.263967260503969,
-1.73312661900816));
#50424=CARTESIAN_POINT('Ctrl Pts',(0.207451935556179,0.35901646169126,-1.72655093133193));
#50425=CARTESIAN_POINT('Ctrl Pts',(0.0807829683652689,0.385556430393323,
-1.7199752436557));
#50426=CARTESIAN_POINT('Ctrl Pts',(-0.0458859988256416,0.412096399095387,
-1.71339955597947));
#50427=CARTESIAN_POINT('Ctrl Pts',(-0.186909184859858,0.370127135312224,
-1.70682386830324));
#50428=CARTESIAN_POINT('Ctrl Pts',(-0.278453939513988,0.278645235121949,
-1.700248180627));
#50429=CARTESIAN_POINT('Ctrl Pts',(-0.350994484233901,0.20615449660954,
-1.6950375711525));
#50430=CARTESIAN_POINT('Ctrl Pts',(-0.392467220602993,0.102574472201558,
-1.689826961678));
#50431=CARTESIAN_POINT('Ctrl Pts',(-0.393398187730971,-0.000340795866165029,
-1.6846163522035));
#50432=CARTESIAN_POINT('Origin',(0.,0.,-0.975));
#50433=CARTESIAN_POINT('',(-0.393658757357236,0.000274916615761227,-1.5412836477965));
#50434=CARTESIAN_POINT('',(-0.393685317967325,0.000263450781192951,-1.5596163522035));
#50435=CARTESIAN_POINT('',(-0.3933,-4.81653586104654E-17,-0.975));
#50436=CARTESIAN_POINT('Ctrl Pts',(-0.393658757357236,0.000274916615761227,
-1.5412836477965));
#50437=CARTESIAN_POINT('Ctrl Pts',(-0.393800352394406,0.0180217662467705,
-1.54218371626743));
#50438=CARTESIAN_POINT('Ctrl Pts',(-0.392702743301847,0.0357510060110471,
-1.54308378473835));
#50439=CARTESIAN_POINT('Ctrl Pts',(-0.390305752494891,0.0533027934246246,
-1.54398385320928));
#50440=CARTESIAN_POINT('Ctrl Pts',(-0.372793903765057,0.181532007000592,
-1.55055954088551));
#50441=CARTESIAN_POINT('Ctrl Pts',(-0.285928614910863,0.300289845966023,
-1.55713522856174));
#50442=CARTESIAN_POINT('Ctrl Pts',(-0.169028625036337,0.355821714128369,
-1.56371091623797));
#50443=CARTESIAN_POINT('Ctrl Pts',(-0.0521286351618115,0.411353582290715,
-1.5702866039142));
#50444=CARTESIAN_POINT('Ctrl Pts',(0.0948060557330462,0.403659479649976,
-1.57686229159043));
#50445=CARTESIAN_POINT('Ctrl Pts',(0.205266870788755,0.336222069051615,
-1.58343797926666));
#50446=CARTESIAN_POINT('Ctrl Pts',(0.315727685844463,0.268784658453253,
-1.59001366694289));
#50447=CARTESIAN_POINT('Ctrl Pts',(0.389714625061023,0.141603939897268,
-1.59658935461912));
#50448=CARTESIAN_POINT('Ctrl Pts',(0.393738210339229,0.0122470423297462,
-1.60316504229535));
#50449=CARTESIAN_POINT('Ctrl Pts',(0.397761795617435,-0.117109855237775,
-1.60974072997159));
#50450=CARTESIAN_POINT('Ctrl Pts',(0.331822026957288,-0.248642931816833,
-1.61631641764782));
#50451=CARTESIAN_POINT('Ctrl Pts',(0.225765908359775,-0.322814998917635,
-1.62289210532405));
#50452=CARTESIAN_POINT('Ctrl Pts',(0.119709789762263,-0.396987066018437,
-1.62946779300028));
#50453=CARTESIAN_POINT('Ctrl Pts',(-0.0264626787726145,-0.413798123640983,
-1.63604348067651));
#50454=CARTESIAN_POINT('Ctrl Pts',(-0.146587934364655,-0.365638816110993,
-1.64261916835274));
#50455=CARTESIAN_POINT('Ctrl Pts',(-0.266713189956696,-0.317479508581004,
-1.64919485602897));
#50456=CARTESIAN_POINT('Ctrl Pts',(-0.3607912326059,-0.204349835898478,
-1.6557705437052));
#50457=CARTESIAN_POINT('Ctrl Pts',(-0.386238536562886,-0.0774568425967047,
-1.66234623138143));
#50458=CARTESIAN_POINT('Ctrl Pts',(-0.391317682514508,-0.0521296788898022,
-1.66365870351979));
#50459=CARTESIAN_POINT('Ctrl Pts',(-0.39366271518768,-0.0262542116329496,
-1.66497117565815));
#50460=CARTESIAN_POINT('Ctrl Pts',(-0.393429058327419,-0.000336684366980755,
-1.6662836477965));
#50461=CARTESIAN_POINT('Ctrl Pts',(-0.393398187730971,-0.000340795866165029,
-1.6846163522035));
#50462=CARTESIAN_POINT('Ctrl Pts',(-0.393642082987207,-0.0273025917466196,
-1.68325127400177));
#50463=CARTESIAN_POINT('Ctrl Pts',(-0.391103442761171,-0.0542187628766391,
-1.68188619580004));
#50464=CARTESIAN_POINT('Ctrl Pts',(-0.385611918437396,-0.0805183487896309,
-1.68052111759831));
#50465=CARTESIAN_POINT('Ctrl Pts',(-0.35915881943263,-0.20720549591355,
-1.67394542992208));
#50466=CARTESIAN_POINT('Ctrl Pts',(-0.264186298149056,-0.319585253564002,
-1.66736974224585));
#50467=CARTESIAN_POINT('Ctrl Pts',(-0.143682792882962,-0.366790109162457,
-1.66079405456962));
#50468=CARTESIAN_POINT('Ctrl Pts',(-0.0231792876168675,-0.413994964760912,
-1.65421836689339));
#50469=CARTESIAN_POINT('Ctrl Pts',(0.122855201631747,-0.39602491830737,
-1.64764267921716));
#50470=CARTESIAN_POINT('Ctrl Pts',(0.228319585447469,-0.321013883609743,
-1.64106699154093));
#50471=CARTESIAN_POINT('Ctrl Pts',(0.333783969263191,-0.246002848912117,
-1.6344913038647));
#50472=CARTESIAN_POINT('Ctrl Pts',(0.39867824764602,-0.113950825970406,
-1.62791561618847));
#50473=CARTESIAN_POINT('Ctrl Pts',(0.393628638093698,0.0153700760896384,
-1.62133992851224));
#50474=CARTESIAN_POINT('Ctrl Pts',(0.388579028541375,0.144690978149683,
-1.61476424083601));
#50475=CARTESIAN_POINT('Ctrl Pts',(0.313585531053901,0.271280759328061,
-1.60818855315978));
#50476=CARTESIAN_POINT('Ctrl Pts',(0.202593237697407,0.337839785620704,
-1.60161286548355));
#50477=CARTESIAN_POINT('Ctrl Pts',(0.0916009443409129,0.404398811913346,
-1.59503717780731));
#50478=CARTESIAN_POINT('Ctrl Pts',(-0.0553901448846022,0.410927083320253,
-1.58846149013108));
#50479=CARTESIAN_POINT('Ctrl Pts',(-0.171845927581847,0.354469632623865,
-1.58188580245485));
#50480=CARTESIAN_POINT('Ctrl Pts',(-0.288301710279093,0.298012181927477,
-1.57531011477862));
#50481=CARTESIAN_POINT('Ctrl Pts',(-0.374222186448069,0.178569009127795,
-1.56873442710239));
#50482=CARTESIAN_POINT('Ctrl Pts',(-0.390716276005324,0.0502049236873175,
-1.56215873942616));
#50483=CARTESIAN_POINT('Ctrl Pts',(-0.392842003615096,0.0336615989056209,
-1.56131127701861));
#50484=CARTESIAN_POINT('Ctrl Pts',(-0.393814588422652,0.0169701015529035,
-1.56046381461105));
#50485=CARTESIAN_POINT('Ctrl Pts',(-0.393685317967325,0.000263450781192951,
-1.5596163522035));
#50486=CARTESIAN_POINT('Origin',(0.,0.,-0.975));
#50487=CARTESIAN_POINT('',(-0.392680002949509,5.54103040254772E-5,-1.4162836477965));
#50488=CARTESIAN_POINT('',(-0.39268505468958,7.18397355967851E-5,-1.4346163522035));
#50489=CARTESIAN_POINT('',(-0.3933,-4.81653586104654E-17,-0.975));
#50490=CARTESIAN_POINT('Ctrl Pts',(-0.392680002949509,5.54103040254772E-5,
-1.4162836477965));
#50491=CARTESIAN_POINT('Ctrl Pts',(-0.392758615348053,0.0618182368767579,
-1.41939625687671));
#50492=CARTESIAN_POINT('Ctrl Pts',(-0.379036335622443,0.123548029294639,
-1.42250886595692));
#50493=CARTESIAN_POINT('Ctrl Pts',(-0.351326532985881,0.178183712592334,
-1.42562147503713));
#50494=CARTESIAN_POINT('Ctrl Pts',(-0.292786895333777,0.293606876916932,
-1.43219716271336));
#50495=CARTESIAN_POINT('Ctrl Pts',(-0.171820036208097,0.37736857237224,
-1.43877285038959));
#50496=CARTESIAN_POINT('Ctrl Pts',(-0.043180442965895,0.391554871712072,
-1.44534853806582));
#50497=CARTESIAN_POINT('Ctrl Pts',(0.0854591502763071,0.405741171051904,
-1.45192422574205));
#50498=CARTESIAN_POINT('Ctrl Pts',(0.221771477635032,0.35035207427626,-1.45849991341828));
#50499=CARTESIAN_POINT('Ctrl Pts',(0.304056072899483,0.250458924261499,
-1.46507560109451));
#50500=CARTESIAN_POINT('Ctrl Pts',(0.386340668163933,0.150565774246737,
-1.47165128877074));
#50501=CARTESIAN_POINT('Ctrl Pts',(0.414597531334111,0.00616857099285846,
-1.47822697644697));
#50502=CARTESIAN_POINT('Ctrl Pts',(0.376036464587567,-0.117372677880283,
-1.4848026641232));
#50503=CARTESIAN_POINT('Ctrl Pts',(0.337475397841023,-0.240913926753425,
-1.49137835179943));
#50504=CARTESIAN_POINT('Ctrl Pts',(0.232096401177758,-0.34359922124583,
-1.49795403947566));
#50505=CARTESIAN_POINT('Ctrl Pts',(0.107598265687765,-0.378949048623052,
-1.50452972715189));
#50506=CARTESIAN_POINT('Ctrl Pts',(-0.0168998698022284,-0.414298876000273,
-1.51110541482813));
#50507=CARTESIAN_POINT('Ctrl Pts',(-0.16051714411895,-0.382313236262312,
-1.51768110250436));
#50508=CARTESIAN_POINT('Ctrl Pts',(-0.258246576974574,-0.297470122300079,
-1.52425679018059));
#50509=CARTESIAN_POINT('Ctrl Pts',(-0.342598978327816,-0.22424018335657,
-1.52993240938589));
#50510=CARTESIAN_POINT('Ctrl Pts',(-0.392765892493847,-0.11163252582122,
-1.5356080285912));
#50511=CARTESIAN_POINT('Ctrl Pts',(-0.393658757357236,0.000274916615761227,
-1.5412836477965));
#50512=CARTESIAN_POINT('Ctrl Pts',(-0.393685317967325,0.000263450781192951,
-1.5596163522035));
#50513=CARTESIAN_POINT('Ctrl Pts',(-0.392811544355544,-0.112661273964597,
-1.55388812693482));
#50514=CARTESIAN_POINT('Ctrl Pts',(-0.341596538395714,-0.22627832356657,
-1.54815990166615));
#50515=CARTESIAN_POINT('Ctrl Pts',(-0.255878681665093,-0.299509336414108,
-1.54243167639747));
#50516=CARTESIAN_POINT('Ctrl Pts',(-0.157479294822075,-0.383574512993783,
-1.53585598872124));
#50517=CARTESIAN_POINT('Ctrl Pts',(-0.0136128181905055,-0.41441986807186,
-1.52928030104501));
#50518=CARTESIAN_POINT('Ctrl Pts',(0.110600969279798,-0.37808354670996,
-1.52270461336878));
#50519=CARTESIAN_POINT('Ctrl Pts',(0.234814756750101,-0.34174722534806,
-1.51612892569255));
#50520=CARTESIAN_POINT('Ctrl Pts',(0.339375855059138,-0.238229227546182,
-1.50955323801632));
#50521=CARTESIAN_POINT('Ctrl Pts',(0.376955686759376,-0.114385981693005,
-1.50297755034009));
#50522=CARTESIAN_POINT('Ctrl Pts',(0.414535518459615,0.0094572641601714,
-1.49640186266386));
#50523=CARTESIAN_POINT('Ctrl Pts',(0.385134083551055,0.153625758064647,
-1.48982617498762));
#50524=CARTESIAN_POINT('Ctrl Pts',(0.302059659365895,0.252863015750642,
-1.48325048731139));
#50525=CARTESIAN_POINT('Ctrl Pts',(0.218985235180735,0.352100273436638,
-1.47667479963516));
#50526=CARTESIAN_POINT('Ctrl Pts',(0.0822378217189762,0.406406294904155,
-1.47009911195893));
#50527=CARTESIAN_POINT('Ctrl Pts',(-0.0462851773144539,0.391199980781066,
-1.4635234242827));
#50528=CARTESIAN_POINT('Ctrl Pts',(-0.174808176347883,0.375993666657979,
-1.45694773660647));
#50529=CARTESIAN_POINT('Ctrl Pts',(-0.295106760952984,0.291275016944286,
-1.45037204893024));
#50530=CARTESIAN_POINT('Ctrl Pts',(-0.352728931790508,0.175391115113851,
-1.44379636125401));
#50531=CARTESIAN_POINT('Ctrl Pts',(-0.379543468198143,0.121464422323106,
-1.44073635823717));
#50532=CARTESIAN_POINT('Ctrl Pts',(-0.392785328249549,0.0607888449821143,
-1.43767635522034));
#50533=CARTESIAN_POINT('Ctrl Pts',(-0.39268505468958,7.18397355967851E-5,
-1.4346163522035));
#50534=CARTESIAN_POINT('Origin',(0.,0.,-0.975));
#50535=CARTESIAN_POINT('',(-0.393465141926397,-0.00033072980931359,-1.2912836477965));
#50536=CARTESIAN_POINT('',(-0.393434478492496,-0.000335863925950309,-1.3096163522035));
#50537=CARTESIAN_POINT('',(-0.3933,-4.81653586104654E-17,-0.975));
#50538=CARTESIAN_POINT('Ctrl Pts',(-0.393465141926397,-0.00033072980931359,
-1.2912836477965));
#50539=CARTESIAN_POINT('Ctrl Pts',(-0.392524065374241,0.104800679194081,
-1.29660879748599));
#50540=CARTESIAN_POINT('Ctrl Pts',(-0.349003498856052,0.210620107401743,
-1.30193394717549));
#50541=CARTESIAN_POINT('Ctrl Pts',(-0.273599856866439,0.283412925845174,
-1.30725909686498));
#50542=CARTESIAN_POINT('Ctrl Pts',(-0.180488709145554,0.373300134105479,
-1.31383478454121));
#50543=CARTESIAN_POINT('Ctrl Pts',(-0.0387615952056478,0.412827691645586,
-1.32041047221744));
#50544=CARTESIAN_POINT('Ctrl Pts',(0.0874300675804848,0.384103829057202,
-1.32698615989367));
#50545=CARTESIAN_POINT('Ctrl Pts',(0.213621730366617,0.355379966468818,
-1.3335618475699));
#50546=CARTESIAN_POINT('Ctrl Pts',(0.324277941998977,0.258404683751943,
-1.34013753524613));
#50547=CARTESIAN_POINT('Ctrl Pts',(0.369311230716079,0.137072911548536,
-1.34671322292236));
#50548=CARTESIAN_POINT('Ctrl Pts',(0.414344519433181,0.0157411393451306,
-1.35328891059859));
#50549=CARTESIAN_POINT('Ctrl Pts',(0.393754885235027,-0.129947122344807,
-1.35986459827482));
#50550=CARTESIAN_POINT('Ctrl Pts',(0.316862028355783,-0.234047480652203,
-1.36644028595105));
#50551=CARTESIAN_POINT('Ctrl Pts',(0.239969171476537,-0.338147838959601,
-1.37301597362728));
#50552=CARTESIAN_POINT('Ctrl Pts',(0.106773091916198,-0.400660293884456,
-1.37959166130351));
#50553=CARTESIAN_POINT('Ctrl Pts',(-0.0224362837557882,-0.393289182898671,
-1.38616734897974));
#50554=CARTESIAN_POINT('Ctrl Pts',(-0.151645659427774,-0.385918071912887,
-1.39274303665597));
#50555=CARTESIAN_POINT('Ctrl Pts',(-0.276868331211408,-0.308663395016463,
-1.3993187243322));
#50556=CARTESIAN_POINT('Ctrl Pts',(-0.341423459013961,-0.196493739971308,
-1.40589441200844));
#50557=CARTESIAN_POINT('Ctrl Pts',(-0.375421345222065,-0.137419715985304,
-1.40935749060446));
#50558=CARTESIAN_POINT('Ctrl Pts',(-0.392592539054185,-0.0686617068225455,
-1.41282056920048));
#50559=CARTESIAN_POINT('Ctrl Pts',(-0.392680002949509,5.54103040254772E-5,
-1.4162836477965));
#50560=CARTESIAN_POINT('Ctrl Pts',(-0.39268505468958,7.18397355967851E-5,
-1.4346163522035));
#50561=CARTESIAN_POINT('Ctrl Pts',(-0.392569848850048,-0.0696868640091281,
-1.43110066754411));
#50562=CARTESIAN_POINT('Ctrl Pts',(-0.374842937939681,-0.139500252864576,
-1.42758498288471));
#50563=CARTESIAN_POINT('Ctrl Pts',(-0.339853957551454,-0.199195959086854,
-1.42406929822532));
#50564=CARTESIAN_POINT('Ctrl Pts',(-0.274411055404927,-0.310849977509947,
-1.41749361054909));
#50565=CARTESIAN_POINT('Ctrl Pts',(-0.148579494041927,-0.387108860408956,
-1.41091792287286));
#50566=CARTESIAN_POINT('Ctrl Pts',(-0.0193157215696609,-0.39345475659486,
-1.40434223519663));
#50567=CARTESIAN_POINT('Ctrl Pts',(0.109948050902604,-0.399800652780763,
-1.3977665475204));
#50568=CARTESIAN_POINT('Ctrl Pts',(0.242644034484135,-0.33623356225356,
-1.39119085984416));
#50569=CARTESIAN_POINT('Ctrl Pts',(0.318708666244829,-0.231526518231,-1.38461517216793));
#50570=CARTESIAN_POINT('Ctrl Pts',(0.394773298005524,-0.126819474208439,
-1.3780394844917));
#50571=CARTESIAN_POINT('Ctrl Pts',(0.414206577945384,0.0190275233094804,
-1.37146379681547));
#50572=CARTESIAN_POINT('Ctrl Pts',(0.368212218484911,0.139998231210439,
-1.36488810913924));
#50573=CARTESIAN_POINT('Ctrl Pts',(0.322217859024438,0.260968939111397,
-1.35831242146301));
#50574=CARTESIAN_POINT('Ctrl Pts',(0.210795860163633,0.357063357395395,
-1.35173673378678));
#50575=CARTESIAN_POINT('Ctrl Pts',(0.0843803198993765,0.384785270245916,
-1.34516104611055));
#50576=CARTESIAN_POINT('Ctrl Pts',(-0.0420352203648793,0.412507183096438,
-1.33858535843432));
#50577=CARTESIAN_POINT('Ctrl Pts',(-0.183444302032587,0.371856590513483,
-1.33200967075809));
#50578=CARTESIAN_POINT('Ctrl Pts',(-0.275839461984906,0.281233592936417,
-1.32543398308186));
#50579=CARTESIAN_POINT('Ctrl Pts',(-0.349924110720866,0.208569906371435,
-1.32016143945574));
#50580=CARTESIAN_POINT('Ctrl Pts',(-0.392496651065346,0.103777881823186,
-1.31488889582962));
#50581=CARTESIAN_POINT('Ctrl Pts',(-0.393434478492496,-0.000335863925950309,
-1.3096163522035));
#50582=CARTESIAN_POINT('Origin',(0.,0.,-0.975));
#50583=CARTESIAN_POINT('',(-0.393626427439675,0.000287423903241796,-1.1662836477965));
#50584=CARTESIAN_POINT('',(-0.393653923221138,0.000276869757435893,-1.1846163522035));
#50585=CARTESIAN_POINT('',(-0.3933,-4.81653586104654E-17,-0.975));
#50586=CARTESIAN_POINT('Ctrl Pts',(-0.393626427439675,0.000287423903241796,
-1.1662836477965));
#50587=CARTESIAN_POINT('Ctrl Pts',(-0.393782557155591,0.0192595098298366,
-1.16724565041905));
#50588=CARTESIAN_POINT('Ctrl Pts',(-0.392527937158206,0.0382108672674389,
-1.16820765304159));
#50589=CARTESIAN_POINT('Ctrl Pts',(-0.389790918787831,0.0569456569372362,
-1.16916965566413));
#50590=CARTESIAN_POINT('Ctrl Pts',(-0.371082260884058,0.185005729396081,
-1.17574534334036));
#50591=CARTESIAN_POINT('Ctrl Pts',(-0.283111643718684,0.302947126481015,
-1.18232103101659));
#50592=CARTESIAN_POINT('Ctrl Pts',(-0.165698122527018,0.357384807181973,
-1.18889671869282));
#50593=CARTESIAN_POINT('Ctrl Pts',(-0.0482846013353533,0.41182248788293,
-1.19547240636906));
#50594=CARTESIAN_POINT('Ctrl Pts',(0.0985718238826033,0.402756452199911,
-1.20204809404529));
#50595=CARTESIAN_POINT('Ctrl Pts',(0.208398002251702,0.334290354139894,
-1.20862378172152));
#50596=CARTESIAN_POINT('Ctrl Pts',(0.318224180620801,0.265824256079877,
-1.21519946939775));
#50597=CARTESIAN_POINT('Ctrl Pts',(0.391020112141041,0.137958095642862,
-1.22177515707398));
#50598=CARTESIAN_POINT('Ctrl Pts',(0.393835417339004,0.00856926268048242,
-1.22835084475021));
#50599=CARTESIAN_POINT('Ctrl Pts',(0.396650722536966,-0.120819570281897,
-1.23492653242644));
#50600=CARTESIAN_POINT('Ctrl Pts',(0.329485401412651,-0.25173107576964,
-1.24150222010267));
#50601=CARTESIAN_POINT('Ctrl Pts',(0.222741191704447,-0.324909417732935,
-1.2480779077789));
#50602=CARTESIAN_POINT('Ctrl Pts',(0.115996981996244,-0.398087759696229,
-1.25465359545513));
#50603=CARTESIAN_POINT('Ctrl Pts',(-0.0303261162958466,-0.413532938135074,
-1.26122928313136));
#50604=CARTESIAN_POINT('Ctrl Pts',(-0.149996357609078,-0.364253841321533,
-1.26780497080759));
#50605=CARTESIAN_POINT('Ctrl Pts',(-0.269666598922309,-0.314974744507992,
-1.27438065848382));
#50606=CARTESIAN_POINT('Ctrl Pts',(-0.362683983256681,-0.200971372442066,
-1.28095634616005));
#50607=CARTESIAN_POINT('Ctrl Pts',(-0.386945084672934,-0.0738462569188511,
-1.28753203383628));
#50608=CARTESIAN_POINT('Ctrl Pts',(-0.391558963922528,-0.0496701108094308,
-1.28878257182302));
#50609=CARTESIAN_POINT('Ctrl Pts',(-0.393686140780048,-0.0250193917670572,
-1.29003310980976));
#50610=CARTESIAN_POINT('Ctrl Pts',(-0.393465141926397,-0.00033072980931359,
-1.2912836477965));
#50611=CARTESIAN_POINT('Ctrl Pts',(-0.393434478492496,-0.000335863925950309,
-1.3096163522035));
#50612=CARTESIAN_POINT('Ctrl Pts',(-0.39366626874752,-0.0260682651972441,
-1.30831320815339));
#50613=CARTESIAN_POINT('Ctrl Pts',(-0.391354744535682,-0.0517592328627442,
-1.30701006410328));
#50614=CARTESIAN_POINT('Ctrl Pts',(-0.386347075720562,-0.0769134556904893,
-1.30570692005317));
#50615=CARTESIAN_POINT('Ctrl Pts',(-0.361078291266969,-0.203842104169159,
-1.29913123237694));
#50616=CARTESIAN_POINT('Ctrl Pts',(-0.267159484122848,-0.31710399855532,
-1.29255554470071));
#50617=CARTESIAN_POINT('Ctrl Pts',(-0.147102100607386,-0.365432229806147,
-1.28597985702447));
#50618=CARTESIAN_POINT('Ctrl Pts',(-0.0270447170919244,-0.413760461056975,
-1.27940416934824));
#50619=CARTESIAN_POINT('Ctrl Pts',(0.119151242794877,-0.39715502917247,
-1.27282848167201));
#50620=CARTESIAN_POINT('Ctrl Pts',(0.225311581468663,-0.32313222346311,
-1.26625279399578));
#50621=CARTESIAN_POINT('Ctrl Pts',(0.331471920142449,-0.24910941775375,
-1.25967710631955));
#50622=CARTESIAN_POINT('Ctrl Pts',(0.39759663760322,-0.117669238219534,
-1.25310141864332));
#50623=CARTESIAN_POINT('Ctrl Pts',(0.393755015369873,0.0116931798586055,
-1.24652573096709));
#50624=CARTESIAN_POINT('Ctrl Pts',(0.389913393136526,0.141055597936746,
-1.23995004329086));
#50625=CARTESIAN_POINT('Ctrl Pts',(0.31610543120906,0.26834025455881,-1.23337435561463));
#50626=CARTESIAN_POINT('Ctrl Pts',(0.205739594907986,0.335932971991804,
-1.2267986679384));
#50627=CARTESIAN_POINT('Ctrl Pts',(0.0953737586069128,0.403525689424797,
-1.22022298026217));
#50628=CARTESIAN_POINT('Ctrl Pts',(-0.0515499520677672,0.411426467668722,
-1.21364729258594));
#50629=CARTESIAN_POINT('Ctrl Pts',(-0.168527930124931,0.356059095308551,
-1.20707160490971));
#50630=CARTESIAN_POINT('Ctrl Pts',(-0.285505908182095,0.30069172294838,
-1.20049591723348));
#50631=CARTESIAN_POINT('Ctrl Pts',(-0.372538153621742,0.182056199984112,
-1.19392022955725));
#50632=CARTESIAN_POINT('Ctrl Pts',(-0.390230356160714,0.0538517568406279,
-1.18734454188102));
#50633=CARTESIAN_POINT('Ctrl Pts',(-0.392677131145371,0.0361214926909641,
-1.18643514532184));
#50634=CARTESIAN_POINT('Ctrl Pts',(-0.393797708142816,0.0182082133288689,
-1.18552574876267));
#50635=CARTESIAN_POINT('Ctrl Pts',(-0.393653923221138,0.000276869757435893,
-1.1846163522035));
#50636=CARTESIAN_POINT('Origin',(0.,0.,-0.975));
#50637=CARTESIAN_POINT('',(-0.392675709594332,3.59123229115022E-5,-1.0412836477965));
#50638=CARTESIAN_POINT('',(-0.392679206567132,5.24831113405046E-5,-1.0596163522035));
#50639=CARTESIAN_POINT('',(-0.3933,-4.81653586104654E-17,-0.975));
#50640=CARTESIAN_POINT('Ctrl Pts',(-0.392675709594332,3.59123229115022E-5,
-1.0412836477965));
#50641=CARTESIAN_POINT('Ctrl Pts',(-0.392727640745588,0.0630294066245346,
-1.04445819102833));
#50642=CARTESIAN_POINT('Ctrl Pts',(-0.378427444911321,0.126000646034939,
-1.04763273426015));
#50643=CARTESIAN_POINT('Ctrl Pts',(-0.349647097122614,0.181457090484786,
-1.05080727749198));
#50644=CARTESIAN_POINT('Ctrl Pts',(-0.290032039316968,0.29632850085984,
-1.05738296516821));
#50645=CARTESIAN_POINT('Ctrl Pts',(-0.16828817904421,0.37895679575142,-1.06395865284444));
#50646=CARTESIAN_POINT('Ctrl Pts',(-0.0395217057681203,0.391941070808678,
-1.07053434052067));
#50647=CARTESIAN_POINT('Ctrl Pts',(0.0892447675079717,0.404925345865936,
-1.0771100281969));
#50648=CARTESIAN_POINT('Ctrl Pts',(0.225033853787397,0.348265601088871,
-1.08368571587313));
#50649=CARTESIAN_POINT('Ctrl Pts',(0.306381926905658,0.247608325948566,
-1.09026140354936));
#50650=CARTESIAN_POINT('Ctrl Pts',(0.387730000023918,0.146951050808262,
-1.0968370912256));
#50651=CARTESIAN_POINT('Ctrl Pts',(0.414637059981015,0.00229624530471971,
-1.10341277890183));
#50652=CARTESIAN_POINT('Ctrl Pts',(0.374923884427774,-0.120879481712424,
-1.10998846657806));
#50653=CARTESIAN_POINT('Ctrl Pts',(0.335210708874532,-0.244055208729568,
-1.11656415425429));
#50654=CARTESIAN_POINT('Ctrl Pts',(0.228877297810951,-0.345751857260314,
-1.12313984193052));
#50655=CARTESIAN_POINT('Ctrl Pts',(0.104054448825274,-0.379937415758363,
-1.12971552960675));
#50656=CARTESIAN_POINT('Ctrl Pts',(-0.020768400160404,-0.414122974256413,
-1.13629121728298));
#50657=CARTESIAN_POINT('Ctrl Pts',(-0.164080687068179,-0.380797442721763,
-1.14286690495921));
#50658=CARTESIAN_POINT('Ctrl Pts',(-0.261013481200979,-0.295045303038061,
-1.14944259263544));
#50659=CARTESIAN_POINT('Ctrl Pts',(-0.343765309515822,-0.221838434256229,
-1.15505627768913));
#50660=CARTESIAN_POINT('Ctrl Pts',(-0.392715345669069,-0.110422581150446,
-1.16066996274281));
#50661=CARTESIAN_POINT('Ctrl Pts',(-0.393626427439675,0.000287423903241796,
-1.1662836477965));
#50662=CARTESIAN_POINT('Ctrl Pts',(-0.393653923221138,0.000276869757435893,
-1.1846163522035));
#50663=CARTESIAN_POINT('Ctrl Pts',(-0.392758024488892,-0.11145019999114,
-1.17895006108644));
#50664=CARTESIAN_POINT('Ctrl Pts',(-0.34277556993753,-0.22387857986823,
-1.17328376996938));
#50665=CARTESIAN_POINT('Ctrl Pts',(-0.258664734133429,-0.297106543010793,
-1.16761747885232));
#50666=CARTESIAN_POINT('Ctrl Pts',(-0.161054749928876,-0.38208703639603,
-1.16104179117609));
#50667=CARTESIAN_POINT('Ctrl Pts',(-0.0174826218814731,-0.414274659843806,
-1.15446610349986));
#50668=CARTESIAN_POINT('Ctrl Pts',(0.107065104714644,-0.379099994640705,
-1.14789041582363));
#50669=CARTESIAN_POINT('Ctrl Pts',(0.231612831310762,-0.343925329437603,
-1.1413147281474));
#50670=CARTESIAN_POINT('Ctrl Pts',(0.337136156455594,-0.241388375583624,
-1.13473904047117));
#50671=CARTESIAN_POINT('Ctrl Pts',(0.375870960174213,-0.117901500761677,
-1.12816335279494));
#50672=CARTESIAN_POINT('Ctrl Pts',(0.414605763892832,0.00558537406027194,
-1.12158766511871));
#50673=CARTESIAN_POINT('Ctrl Pts',(0.386552046185236,0.15002216985019,-1.11501197744248));
#50674=CARTESIAN_POINT('Ctrl Pts',(0.304408053022061,0.250030957762152,
-1.10843628976625));
#50675=CARTESIAN_POINT('Ctrl Pts',(0.222264059858886,0.350039745674113,
-1.10186060209002));
#50676=CARTESIAN_POINT('Ctrl Pts',(0.0860297912401334,0.405620525708119,
-1.09528491441379));
#50677=CARTESIAN_POINT('Ctrl Pts',(-0.0426296191580955,0.391615191424664,
-1.08870922673755));
#50678=CARTESIAN_POINT('Ctrl Pts',(-0.171289029556324,0.377609857141209,
-1.08213353906132));
#50679=CARTESIAN_POINT('Ctrl Pts',(-0.292373581734029,0.294018408540293,
-1.07555785138509));
#50680=CARTESIAN_POINT('Ctrl Pts',(-0.351075515706501,0.17867771225185,
-1.06898216370886));
#50681=CARTESIAN_POINT('Ctrl Pts',(-0.378945414423148,0.123917446176563,
-1.06586022654041));
#50682=CARTESIAN_POINT('Ctrl Pts',(-0.392753880852442,0.0620007011111865,
-1.06273828937195));
#50683=CARTESIAN_POINT('Ctrl Pts',(-0.392679206567132,5.24831113405046E-5,
-1.0596163522035));
#50684=CARTESIAN_POINT('Origin',(0.,0.,-0.975));
#50685=CARTESIAN_POINT('',(-0.393500865148788,-0.000323575883594496,-0.916283647796503));
#50686=CARTESIAN_POINT('',(-0.393470515958058,-0.000329728814630641,-0.934616352203498));
#50687=CARTESIAN_POINT('',(-0.3933,-4.81653586104654E-17,-0.975));
#50688=CARTESIAN_POINT('Ctrl Pts',(-0.393500865148788,-0.000323575883594496,
-0.916283647796503));
#50689=CARTESIAN_POINT('Ctrl Pts',(-0.392559185254019,0.106005602838139,
-0.921670731637612));
#50690=CARTESIAN_POINT('Ctrl Pts',(-0.347906081227037,0.213031985603417,
-0.92705781547872));
#50691=CARTESIAN_POINT('Ctrl Pts',(-0.27094104215407,0.28595580058803,-0.932444899319829));
#50692=CARTESIAN_POINT('Ctrl Pts',(-0.176994470342677,0.374969494386296,
-0.93902058699606));
#50693=CARTESIAN_POINT('Ctrl Pts',(-0.0349043771728895,0.413171693980084,
-0.94559627467229));
#50694=CARTESIAN_POINT('Ctrl Pts',(0.0910135209191817,0.383270540510706,
-0.952171962348521));
#50695=CARTESIAN_POINT('Ctrl Pts',(0.216931419011254,0.353369387041328,
-0.958747650024752));
#50696=CARTESIAN_POINT('Ctrl Pts',(0.32667712202561,0.255364880508782,-0.965323337700983));
#50697=CARTESIAN_POINT('Ctrl Pts',(0.370575291184627,0.133617819832924,
-0.971899025377213));
#50698=CARTESIAN_POINT('Ctrl Pts',(0.414473460343644,0.0118707591570669,
-0.978474713053443));
#50699=CARTESIAN_POINT('Ctrl Pts',(0.392524095647324,-0.133618855662101,
-0.985050400729674));
#50700=CARTESIAN_POINT('Ctrl Pts',(0.31466236628494,-0.23699654735341,-0.991626088405904));
#50701=CARTESIAN_POINT('Ctrl Pts',(0.236800636922554,-0.340374239044721,
-0.998201776082135));
#50702=CARTESIAN_POINT('Ctrl Pts',(0.1030265428941,-0.401640007608169,-1.00477746375837));
#50703=CARTESIAN_POINT('Ctrl Pts',(-0.026108356531957,-0.393062491129178,
-1.0113531514346));
#50704=CARTESIAN_POINT('Ctrl Pts',(-0.155243255958012,-0.384484974650187,
-1.01792883911083));
#50705=CARTESIAN_POINT('Ctrl Pts',(-0.279738960781671,-0.306064173128758,
-1.02450452678706));
#50706=CARTESIAN_POINT('Ctrl Pts',(-0.343243685524234,-0.193296509438779,
-1.03108021446329));
#50707=CARTESIAN_POINT('Ctrl Pts',(-0.376090248862751,-0.134969664893826,
-1.03448135890769));
#50708=CARTESIAN_POINT('Ctrl Pts',(-0.392620071559601,-0.0674541035728149,
-1.0378825033521));
#50709=CARTESIAN_POINT('Ctrl Pts',(-0.392675709594332,3.59123229115022E-5,
-1.0412836477965));
#50710=CARTESIAN_POINT('Ctrl Pts',(-0.392679206567132,5.24831113405046E-5,
-1.0596163522035));
#50711=CARTESIAN_POINT('Ctrl Pts',(-0.39259659556733,-0.0684798664614236,
-1.05616260169572));
#50712=CARTESIAN_POINT('Ctrl Pts',(-0.375522890959624,-0.137050734665287,
-1.05270885118795));
#50713=CARTESIAN_POINT('Ctrl Pts',(-0.34169948938714,-0.196013268777163,
-1.04925510068017));
#50714=CARTESIAN_POINT('Ctrl Pts',(-0.27730221332807,-0.30827360954176,
-1.04267941300394));
#50715=CARTESIAN_POINT('Ctrl Pts',(-0.152188345442694,-0.385704347094983,
-1.03610372532771));
#50716=CARTESIAN_POINT('Ctrl Pts',(-0.0229894767844834,-0.393257201512339,
-1.02952803765148));
#50717=CARTESIAN_POINT('Ctrl Pts',(0.106209391873727,-0.400810055929695,
-1.02295234997525));
#50718=CARTESIAN_POINT('Ctrl Pts',(0.239493261304774,-0.338485027211183,
-1.01637666229902));
#50719=CARTESIAN_POINT('Ctrl Pts',(0.316532467697458,-0.234492941210388,
-1.00980097462279));
#50720=CARTESIAN_POINT('Ctrl Pts',(0.393571674090142,-0.130500855209592,
-1.00322528694656));
#50721=CARTESIAN_POINT('Ctrl Pts',(0.414366217444464,0.0151582880734869,
-0.996649599270326));
#50722=CARTESIAN_POINT('Ctrl Pts',(0.369503647363922,0.136553275936165,
-0.990073911594096));
#50723=CARTESIAN_POINT('Ctrl Pts',(0.32464107728338,0.257948263798845,-0.983498223917865));
#50724=CARTESIAN_POINT('Ctrl Pts',(0.214121393767973,0.355079096241123,
-0.976922536241634));
#50725=CARTESIAN_POINT('Ctrl Pts',(0.0879702704379724,0.383980434531775,
-0.970346848565403));
#50726=CARTESIAN_POINT('Ctrl Pts',(-0.0381808528920271,0.412881772822426,
-0.963771160889173));
#50727=CARTESIAN_POINT('Ctrl Pts',(-0.179963416036617,0.373553616961452,
-0.957195473212943));
#50728=CARTESIAN_POINT('Ctrl Pts',(-0.273200903072934,0.283797479101337,
-0.950619785536712));
#50729=CARTESIAN_POINT('Ctrl Pts',(-0.348839121786578,0.210983479044568,
-0.945285307758974));
#50730=CARTESIAN_POINT('Ctrl Pts',(-0.392529121558599,0.104982092359763,
-0.939950829981236));
#50731=CARTESIAN_POINT('Ctrl Pts',(-0.393470515958058,-0.000329728814630641,
-0.934616352203498));
#50732=CARTESIAN_POINT('Origin',(0.,0.,-0.975));
#50733=CARTESIAN_POINT('',(-0.393593124134507,0.000298827634702806,-0.791283647796503));
#50734=CARTESIAN_POINT('',(-0.39362143792178,0.00028921277307428,-0.809616352203499));
#50735=CARTESIAN_POINT('',(-0.3933,-4.81653586104654E-17,-0.975));
#50736=CARTESIAN_POINT('Ctrl Pts',(-0.393593124134507,0.000298827634702806,
-0.791283647796503));
#50737=CARTESIAN_POINT('Ctrl Pts',(-0.393763705766818,0.0204967956566175,
-0.792307584570663));
#50738=CARTESIAN_POINT('Ctrl Pts',(-0.392341422207924,0.0406706868593803,
-0.793331521344824));
#50739=CARTESIAN_POINT('Ctrl Pts',(-0.389242085705192,0.0605835532908611,
-0.794355458118985));
#50740=CARTESIAN_POINT('Ctrl Pts',(-0.369338250468678,0.188463314713854,
-0.800931145795216));
#50741=CARTESIAN_POINT('Ctrl Pts',(-0.28026997813637,0.305577982858121,
-0.807506833471447));
#50742=CARTESIAN_POINT('Ctrl Pts',(-0.162353167016069,0.358916727630976,
-0.814082521147678));
#50743=CARTESIAN_POINT('Ctrl Pts',(-0.0444363558957643,0.412255472403833,
-0.820658208823909));
#50744=CARTESIAN_POINT('Ctrl Pts',(0.102328994012537,0.401818293805276,
-0.827233896500139));
#50745=CARTESIAN_POINT('Ctrl Pts',(0.211510956198164,0.332329480518375,
-0.83380958417637));
#50746=CARTESIAN_POINT('Ctrl Pts',(0.320692918383789,0.262840667231475,
-0.8403852718526));
#50747=CARTESIAN_POINT('Ctrl Pts',(0.392291492846743,0.134300219256238,
-0.846960959528831));
#50748=CARTESIAN_POINT('Ctrl Pts',(0.393898272289506,0.00489073622447934,
-0.853536647205062));
#50749=CARTESIAN_POINT('Ctrl Pts',(0.395505051732269,-0.124518746807278,
-0.860112334881293));
#50750=CARTESIAN_POINT('Ctrl Pts',(0.32712003615484,-0.254797264895555,
-0.866688022557523));
#50751=CARTESIAN_POINT('Ctrl Pts',(0.219697046279269,-0.326975497659441,
-0.873263710233753));
#50752=CARTESIAN_POINT('Ctrl Pts',(0.112274056403699,-0.399153730423328,
-0.879839397909984));
#50753=CARTESIAN_POINT('Ctrl Pts',(-0.0341869077700128,-0.413231677862823,
-0.886415085586215));
#50754=CARTESIAN_POINT('Ctrl Pts',(-0.15339169701149,-0.362837092234807,
-0.892990773262446));
#50755=CARTESIAN_POINT('Ctrl Pts',(-0.27259648625297,-0.312442506606791,
-0.899566460938676));
#50756=CARTESIAN_POINT('Ctrl Pts',(-0.364545100562215,-0.19757538791126,
-0.906142148614907));
#50757=CARTESIAN_POINT('Ctrl Pts',(-0.387617882490338,-0.0702292345621217,
-0.912717836291137));
#50758=CARTESIAN_POINT('Ctrl Pts',(-0.391788457255595,-0.0472104821955896,
-0.913906440126259));
#50759=CARTESIAN_POINT('Ctrl Pts',(-0.393708636991104,-0.0237839996196404,
-0.915095043961381));
#50760=CARTESIAN_POINT('Ctrl Pts',(-0.393500865148788,-0.000323575883594496,
-0.916283647796503));
#50761=CARTESIAN_POINT('Ctrl Pts',(-0.393470515958058,-0.000329728814630641,
-0.934616352203498));
#50762=CARTESIAN_POINT('Ctrl Pts',(-0.393689556714375,-0.0248333597821209,
-0.933375142305005));
#50763=CARTESIAN_POINT('Ctrl Pts',(-0.391594249852963,-0.0492996586709999,
-0.932133932406512));
#50764=CARTESIAN_POINT('Ctrl Pts',(-0.38704854515182,-0.0733018845596751,
-0.930892722508019));
#50765=CARTESIAN_POINT('Ctrl Pts',(-0.362966289266348,-0.200460990501319,
-0.924317034831789));
#50766=CARTESIAN_POINT('Ctrl Pts',(-0.27010936656736,-0.31459508252535,
-0.917741347155559));
#50767=CARTESIAN_POINT('Ctrl Pts',(-0.150508571575497,-0.364042459702771,
-0.911165659479328));
#50768=CARTESIAN_POINT('Ctrl Pts',(-0.0309077765836359,-0.413489836880192,
-0.904589971803098));
#50769=CARTESIAN_POINT('Ctrl Pts',(0.115436890701099,-0.398250499211004,
-0.898014284126867));
#50770=CARTESIAN_POINT('Ctrl Pts',(0.222283921718536,-0.325222386575045,
-0.891438596450636));
#50771=CARTESIAN_POINT('Ctrl Pts',(0.329130952735972,-0.252194273939086,
-0.884862908774405));
#50772=CARTESIAN_POINT('Ctrl Pts',(0.396480347486111,-0.121377386336356,
-0.878287221098174));
#50773=CARTESIAN_POINT('Ctrl Pts',(0.393847049071157,0.00801526806051965,
-0.871711533421944));
#50774=CARTESIAN_POINT('Ctrl Pts',(0.391213750656204,0.137407922457395,
-0.865135845745713));
#50775=CARTESIAN_POINT('Ctrl Pts',(0.318597759076159,0.265376343648415,
-0.858560158069483));
#50776=CARTESIAN_POINT('Ctrl Pts',(0.208868005718157,0.333996854433482,
-0.851984470393252));
#50777=CARTESIAN_POINT('Ctrl Pts',(0.0991382523601543,0.402617365218549,
-0.845408782717021));
#50778=CARTESIAN_POINT('Ctrl Pts',(-0.0477052627758059,0.411889965597663,
-0.83883309504079));
#50779=CARTESIAN_POINT('Ctrl Pts',(-0.165195232439238,0.357617502037424,
-0.83225740736456));
#50780=CARTESIAN_POINT('Ctrl Pts',(-0.282685202102669,0.303345038477185,
-0.825681719688329));
#50781=CARTESIAN_POINT('Ctrl Pts',(-0.370821626293572,0.185527510977596,
-0.819106032012099));
#50782=CARTESIAN_POINT('Ctrl Pts',(-0.389710398818481,0.0574938921702172,
-0.812530344335868));
#50783=CARTESIAN_POINT('Ctrl Pts',(-0.392500562485909,0.0385813476449172,
-0.811559013625078));
#50784=CARTESIAN_POINT('Ctrl Pts',(-0.393779752347368,0.0194458894757019,
-0.810587682914289));
#50785=CARTESIAN_POINT('Ctrl Pts',(-0.39362143792178,0.00028921277307428,
-0.809616352203499));
#50786=CARTESIAN_POINT('Origin',(0.,0.,-0.975));
#50787=CARTESIAN_POINT('',(-0.392673255853308,1.63036301740749E-5,-0.666283647796503));
#50788=CARTESIAN_POINT('',(-0.392675189741302,3.29645964630328E-5,-0.684616352203499));
#50789=CARTESIAN_POINT('',(-0.3933,-4.81653586104654E-17,-0.975));
#50790=CARTESIAN_POINT('Ctrl Pts',(-0.392673255853308,1.63036301740749E-5,
-0.666283647796503));
#50791=CARTESIAN_POINT('Ctrl Pts',(-0.392697283129928,0.0642397806098739,
-0.669520125179946));
#50792=CARTESIAN_POINT('Ctrl Pts',(-0.377805755035603,0.128452760339452,
-0.67275660256339));
#50793=CARTESIAN_POINT('Ctrl Pts',(-0.347937163399018,0.184714640836245,
-0.675993079946833));
#50794=CARTESIAN_POINT('Ctrl Pts',(-0.287251885344617,0.299024277639788,
-0.682568767623064));
#50795=CARTESIAN_POINT('Ctrl Pts',(-0.164741642994295,0.380511964747164,
-0.689144455299295));
#50796=CARTESIAN_POINT('Ctrl Pts',(-0.0358595213010159,0.392293082969346,
-0.695720142975526));
#50797=CARTESIAN_POINT('Ctrl Pts',(0.0930226003922591,0.404074201191528,
-0.702295830651757));
#50798=CARTESIAN_POINT('Ctrl Pts',(0.228276601428489,0.34614875052852,-0.708871518327987));
#50799=CARTESIAN_POINT('Ctrl Pts',(0.30868105684103,0.244736130068616,-0.715447206004218));
#50800=CARTESIAN_POINT('Ctrl Pts',(0.38908551225357,0.143323509608713,-0.722022893680448));
#50801=CARTESIAN_POINT('Ctrl Pts',(0.414640422042422,-0.00157628064808814,
-0.728598581356679));
#50802=CARTESIAN_POINT('Ctrl Pts',(0.37377860164979,-0.124375741855866,
-0.73517426903291));
#50803=CARTESIAN_POINT('Ctrl Pts',(0.332916781257156,-0.247175203063647,
-0.741749956709141));
#50804=CARTESIAN_POINT('Ctrl Pts',(0.225638230683036,-0.347874335222406,
-0.748325644385371));
#50805=CARTESIAN_POINT('Ctrl Pts',(0.100501555840629,-0.380892642994185,
-0.754901332061602));
#50806=CARTESIAN_POINT('Ctrl Pts',(-0.0246351190017731,-0.413910950765964,
-0.761477019737833));
#50807=CARTESIAN_POINT('Ctrl Pts',(-0.167629918112459,-0.379248434150768,
-0.768052707414064));
#50808=CARTESIAN_POINT('Ctrl Pts',(-0.263757618597442,-0.29259474849231,
-0.774628395090294));
#50809=CARTESIAN_POINT('Ctrl Pts',(-0.344916742047071,-0.219434388510343,
-0.780180145992364));
#50810=CARTESIAN_POINT('Ctrl Pts',(-0.392668236236193,-0.109213878633263,
-0.785731896894433));
#50811=CARTESIAN_POINT('Ctrl Pts',(-0.393593124134507,0.000298827634702806,
-0.791283647796503));
#50812=CARTESIAN_POINT('Ctrl Pts',(-0.39362143792178,0.00028921277307428,
-0.809616352203499));
#50813=CARTESIAN_POINT('Ctrl Pts',(-0.392707999744733,-0.110240448567251,
-0.804011995238058));
#50814=CARTESIAN_POINT('Ctrl Pts',(-0.343939653374366,-0.221476480648583,
-0.798407638272616));
#50815=CARTESIAN_POINT('Ctrl Pts',(-0.261428224532134,-0.294677834256525,
-0.792803281307176));
#50816=CARTESIAN_POINT('Ctrl Pts',(-0.164616156861964,-0.380566231760713,
-0.786227593630945));
#50817=CARTESIAN_POINT('Ctrl Pts',(-0.0213509006627109,-0.414093316653921,
-0.779651905954716));
#50818=CARTESIAN_POINT('Ctrl Pts',(0.103519901367221,-0.380083375859906,
-0.773076218278485));
#50819=CARTESIAN_POINT('Ctrl Pts',(0.228390703397158,-0.346073435065889,
-0.766500530602254));
#50820=CARTESIAN_POINT('Ctrl Pts',(0.334867051257771,-0.244526468584641,
-0.759924842926023));
#50821=CARTESIAN_POINT('Ctrl Pts',(0.374753448392003,-0.121406735819898,
-0.753349155249792));
#50822=CARTESIAN_POINT('Ctrl Pts',(0.414639845526233,0.00171299694484139,
-0.746773467573561));
#50823=CARTESIAN_POINT('Ctrl Pts',(0.387936291934087,0.146405495993077,
-0.740197779897331));
#50824=CARTESIAN_POINT('Ctrl Pts',(0.306729894762555,0.247177090854086,
-0.7336220922211));
#50825=CARTESIAN_POINT('Ctrl Pts',(0.225523497591022,0.347948685715098,
-0.72704640454487));
#50826=CARTESIAN_POINT('Ctrl Pts',(0.0898142568401032,0.404799376388883,
-0.720470716868639));
#50827=CARTESIAN_POINT('Ctrl Pts',(-0.0389703426375748,0.391996243577485,
-0.713895029192408));
#50828=CARTESIAN_POINT('Ctrl Pts',(-0.167754942115248,0.379193110766087,
-0.707319341516178));
#50829=CARTESIAN_POINT('Ctrl Pts',(-0.289614900319681,0.296736154469509,
-0.700743653839948));
#50830=CARTESIAN_POINT('Ctrl Pts',(-0.349391477172996,0.181948724268698,
-0.694167966163717));
#50831=CARTESIAN_POINT('Ctrl Pts',(-0.378334598870116,0.12636998864196,
-0.690984094843644));
#50832=CARTESIAN_POINT('Ctrl Pts',(-0.392722994987612,0.0632117500098348,
-0.687800223523571));
#50833=CARTESIAN_POINT('Ctrl Pts',(-0.392675189741302,3.29645964630328E-5,
-0.684616352203499));
#50834=CARTESIAN_POINT('Origin',(0.,0.,-0.975));
#50835=CARTESIAN_POINT('',(-0.393536100995357,-0.000315234482339499,-0.541283647796502));
#50836=CARTESIAN_POINT('',(-0.393506173951298,-0.000322395119289577,-0.559616352203498));
#50837=CARTESIAN_POINT('',(-0.3933,-4.81653586104654E-17,-0.975));
#50838=CARTESIAN_POINT('Ctrl Pts',(-0.393536100995357,-0.000315234482339499,
-0.541283647796502));
#50839=CARTESIAN_POINT('Ctrl Pts',(-0.392597489512059,0.107211443487718,
-0.546732665789229));
#50840=CARTESIAN_POINT('Ctrl Pts',(-0.346793977563156,0.215441809949464,
-0.552181683781956));
#50841=CARTESIAN_POINT('Ctrl Pts',(-0.26825859469211,0.288473732917049,
-0.557630701774682));
#50842=CARTESIAN_POINT('Ctrl Pts',(-0.173484793250727,0.376606148055041,
-0.564206389450913));
#50843=CARTESIAN_POINT('Ctrl Pts',(-0.0310441146165509,0.413479657540965,
-0.570782077127143));
#50844=CARTESIAN_POINT('Ctrl Pts',(0.0945890356312672,0.382403821312673,
-0.577357764803374));
#50845=CARTESIAN_POINT('Ctrl Pts',(0.220222185879085,0.351327985084382,
-0.583933452479604));
#50846=CARTESIAN_POINT('Ctrl Pts',(0.329047807740543,0.252302803141877,
-0.590509140155835));
#50847=CARTESIAN_POINT('Ctrl Pts',(0.371807028337272,0.130151073341996,
-0.597084827832066));
#50848=CARTESIAN_POINT('Ctrl Pts',(0.414566248934001,0.00799934354211448,
-0.603660515508297));
#50849=CARTESIAN_POINT('Ctrl Pts',(0.391259068265997,-0.137278934115147,
-0.610236203184528));
#50850=CARTESIAN_POINT('Ctrl Pts',(0.312435257885808,-0.239924942102313,
-0.616811890860758));
#50851=CARTESIAN_POINT('Ctrl Pts',(0.23361144750562,-0.342570950089479,
-0.623387578536989));
#50852=CARTESIAN_POINT('Ctrl Pts',(0.0992710074132505,-0.402584688406554,
-0.629963266213219));
#50853=CARTESIAN_POINT('Ctrl Pts',(-0.0297781520148116,-0.392801514605605,
-0.63653895388945));
#50854=CARTESIAN_POINT('Ctrl Pts',(-0.158827311442874,-0.383018340804656,
-0.643114641565681));
#50855=CARTESIAN_POINT('Ctrl Pts',(-0.282585190206626,-0.303438254885682,
-0.649690329241912));
#50856=CARTESIAN_POINT('Ctrl Pts',(-0.345033972709263,-0.190082418676341,
-0.656266016918142));
#50857=CARTESIAN_POINT('Ctrl Pts',(-0.376746187092345,-0.132519013348265,
-0.659605227210929));
#50858=CARTESIAN_POINT('Ctrl Pts',(-0.392648465898091,-0.0662457677398398,
-0.662944437503716));
#50859=CARTESIAN_POINT('Ctrl Pts',(-0.392673255853308,1.63036301740749E-5,
-0.666283647796503));
#50860=CARTESIAN_POINT('Ctrl Pts',(-0.392675189741302,3.29645964630328E-5,
-0.684616352203499));
#50861=CARTESIAN_POINT('Ctrl Pts',(-0.392624262238258,-0.0672721542933228,
-0.68122453584734));
#50862=CARTESIAN_POINT('Ctrl Pts',(-0.376189838802812,-0.134600591513086,
-0.677832719491182));
#50863=CARTESIAN_POINT('Ctrl Pts',(-0.343515216587402,-0.192813481263717,
-0.674440903135024));
#50864=CARTESIAN_POINT('Ctrl Pts',(-0.280169183646299,-0.305670352490252,
-0.667865215458793));
#50865=CARTESIAN_POINT('Ctrl Pts',(-0.155783922261904,-0.384266190838277,
-0.661289527782563));
#50866=CARTESIAN_POINT('Ctrl Pts',(-0.0266612267504973,-0.393025344694661,
-0.654713840106333));
#50867=CARTESIAN_POINT('Ctrl Pts',(0.102461468760913,-0.401784498551045,
-0.648138152430102));
#50868=CARTESIAN_POINT('Ctrl Pts',(0.236321598399336,-0.340706967915784,
-0.641562464753871));
#50869=CARTESIAN_POINT('Ctrl Pts',(0.314328659703452,-0.237438910613055,
-0.63498677707764));
#50870=CARTESIAN_POINT('Ctrl Pts',(0.392335721007567,-0.134170853310328,
-0.62841108940141));
#50871=CARTESIAN_POINT('Ctrl Pts',(0.414489713977377,0.0112877306598665,
-0.621835401725179));
#50872=CARTESIAN_POINT('Ctrl Pts',(0.370762846400388,0.133096409843133,
-0.615259714048949));
#50873=CARTESIAN_POINT('Ctrl Pts',(0.327035978823398,0.254905089026401,
-0.608684026372718));
#50874=CARTESIAN_POINT('Ctrl Pts',(0.217428250699609,0.353063863422739,
-0.602108338696487));
#50875=CARTESIAN_POINT('Ctrl Pts',(0.091552547796971,0.383142106243137,
-0.595532651020257));
#50876=CARTESIAN_POINT('Ctrl Pts',(-0.034323155105665,0.413220349063535,
-0.588956963344026));
#50877=CARTESIAN_POINT('Ctrl Pts',(-0.176466832787148,0.375218060307994,
-0.582381275667795));
#50878=CARTESIAN_POINT('Ctrl Pts',(-0.270538514296277,0.286336611117046,
-0.575805587991565));
#50879=CARTESIAN_POINT('Ctrl Pts',(-0.34773949604993,0.213395051796,-0.570409176062209));
#50880=CARTESIAN_POINT('Ctrl Pts',(-0.392564716544902,0.106187148606209,
-0.565012764132854));
#50881=CARTESIAN_POINT('Ctrl Pts',(-0.393506173951298,-0.000322395119289577,
-0.559616352203498));
#50882=CARTESIAN_POINT('Origin',(0.,0.,-0.975));
#50883=CARTESIAN_POINT('',(-0.393558983542489,0.000309099215769798,-0.416283647796503));
#50884=CARTESIAN_POINT('',(-0.393587999858846,0.00030044772715955,-0.434616352203498));
#50885=CARTESIAN_POINT('',(-0.3933,-4.81653586104654E-17,-0.975));
#50886=CARTESIAN_POINT('Ctrl Pts',(-0.393558983542489,0.000309099215769798,
-0.416283647796503));
#50887=CARTESIAN_POINT('Ctrl Pts',(-0.393743822683672,0.0217335979797476,
-0.417369518722281));
#50888=CARTESIAN_POINT('Ctrl Pts',(-0.392143183010408,0.0431304611559441,
-0.41845538964806));
#50889=CARTESIAN_POINT('Ctrl Pts',(-0.388659301138879,0.0642161659179647,
-0.419541260573839));
#50890=CARTESIAN_POINT('Ctrl Pts',(-0.367562024709244,0.191904462617531,
-0.426116948250069));
#50891=CARTESIAN_POINT('Ctrl Pts',(-0.277403866089175,0.308182185252994,
-0.4326926359263));
#50892=CARTESIAN_POINT('Ctrl Pts',(-0.158994050280294,0.360417341336711,
-0.43926832360253));
#50893=CARTESIAN_POINT('Ctrl Pts',(-0.040584234471411,0.412652497420429,
-0.445844011278761));
#50894=CARTESIAN_POINT('Ctrl Pts',(0.106077238526287,0.400845086952398,
-0.452419698954992));
#50895=CARTESIAN_POINT('Ctrl Pts',(0.214605461156142,0.330339619738361,
-0.458995386631223));
#50896=CARTESIAN_POINT('Ctrl Pts',(0.323133683785996,0.259834152524326,
-0.465571074307454));
#50897=CARTESIAN_POINT('Ctrl Pts',(0.393528656048009,0.130630628564292,
-0.472146761983684));
#50898=CARTESIAN_POINT('Ctrl Pts',(0.393926769589517,0.00121178308243824,
-0.478722449659915));
#50899=CARTESIAN_POINT('Ctrl Pts',(0.394324883131026,-0.128207062399414,
-0.485298137336145));
#50900=CARTESIAN_POINT('Ctrl Pts',(0.324726137952028,-0.257841229403082,
-0.491873825012376));
#50901=CARTESIAN_POINT('Ctrl Pts',(0.216633737843898,-0.329013057199999,
-0.498449512688606));
#50902=CARTESIAN_POINT('Ctrl Pts',(0.108541337735769,-0.400184884996917,
-0.505025200364837));
#50903=CARTESIAN_POINT('Ctrl Pts',(-0.0380447173014935,-0.412894373587085,
-0.511600888041068));
#50904=CARTESIAN_POINT('Ctrl Pts',(-0.156773656868775,-0.361388694819473,
-0.518176575717298));
#50905=CARTESIAN_POINT('Ctrl Pts',(-0.275502596436061,-0.309883016051859,
-0.524752263393529));
#50906=CARTESIAN_POINT('Ctrl Pts',(-0.366374420533366,-0.194162169926462,
-0.53132795106976));
#50907=CARTESIAN_POINT('Ctrl Pts',(-0.388256870457723,-0.066606086468731,
-0.53790363874599));
#50908=CARTESIAN_POINT('Ctrl Pts',(-0.392006180665944,-0.0447507947860351,
-0.539030308429494));
#50909=CARTESIAN_POINT('Ctrl Pts',(-0.393730173597839,-0.0225480566896565,
-0.540156978112998));
#50910=CARTESIAN_POINT('Ctrl Pts',(-0.393536100995357,-0.000315234482339499,
-0.541283647796502));
#50911=CARTESIAN_POINT('Ctrl Pts',(-0.393506173951298,-0.000322395119289577,
-0.559616352203498));
#50912=CARTESIAN_POINT('Ctrl Pts',(-0.393711910262872,-0.0235978832344477,
-0.558437076456623));
#50913=CARTESIAN_POINT('Ctrl Pts',(-0.391821969279263,-0.0468400210630716,
-0.557257800709748));
#50914=CARTESIAN_POINT('Ctrl Pts',(-0.387716254392333,-0.0696839196924745,
-0.556078524962873));
#50915=CARTESIAN_POINT('Ctrl Pts',(-0.364822627642485,-0.197062391684688,
-0.549502837286642));
#50916=CARTESIAN_POINT('Ctrl Pts',(-0.273035688806017,-0.312058726042759,
-0.542927149610411));
#50917=CARTESIAN_POINT('Ctrl Pts',(-0.153901914480065,-0.362620936111316,
-0.536351461934181));
#50918=CARTESIAN_POINT('Ctrl Pts',(-0.0347681401541137,-0.413183146179874,
-0.52977577425795));
#50919=CARTESIAN_POINT('Ctrl Pts',(0.111712469661326,-0.399311231958917,
-0.52320008658172));
#50920=CARTESIAN_POINT('Ctrl Pts',(0.219236873322318,-0.32728418225721,
-0.516624398905489));
#50921=CARTESIAN_POINT('Ctrl Pts',(0.326761276983311,-0.255257132555503,
-0.510048711229258));
#50922=CARTESIAN_POINT('Ctrl Pts',(0.395329474489862,-0.125074947373046,
-0.503473023553027));
#50923=CARTESIAN_POINT('Ctrl Pts',(0.393904729583154,0.00433665711985055,
-0.496897335876797));
#50924=CARTESIAN_POINT('Ctrl Pts',(0.392479984676447,0.133748261612745,
-0.490321648200566));
#50925=CARTESIAN_POINT('Ctrl Pts',(0.321062297356485,0.262389285416077,
-0.483745960524336));
#50926=CARTESIAN_POINT('Ctrl Pts',(0.211978198083273,0.332031604127538,
-0.477170272848105));
#50927=CARTESIAN_POINT('Ctrl Pts',(0.10289409881006,0.401673922838999,-0.470594585171874));
#50928=CARTESIAN_POINT('Ctrl Pts',(-0.0438564124164029,0.412317536458589,
-0.464018897495644));
#50929=CARTESIAN_POINT('Ctrl Pts',(-0.161848125655116,0.359144715640751,
-0.457443209819413));
#50930=CARTESIAN_POINT('Ctrl Pts',(-0.27983983889383,0.305971894822913,
-0.450867522143182));
#50931=CARTESIAN_POINT('Ctrl Pts',(-0.369072754144792,0.188982639567648,
-0.444291834466952));
#50932=CARTESIAN_POINT('Ctrl Pts',(-0.389156449096802,0.0611310127061034,
-0.437716146790721));
#50933=CARTESIAN_POINT('Ctrl Pts',(-0.392312282725616,0.0410411604895479,
-0.436682881928313));
#50934=CARTESIAN_POINT('Ctrl Pts',(-0.393760743963613,0.0206831040430797,
-0.435649617065905));
#50935=CARTESIAN_POINT('Ctrl Pts',(-0.393587999858846,0.000300447727159551,
-0.434616352203498));
#50936=CARTESIAN_POINT('Origin',(0.,0.,-0.975));
#50937=CARTESIAN_POINT('',(-0.392672644806505,-3.40218946998094E-6,-0.291283647796502));
#50938=CARTESIAN_POINT('',(-0.392673014342038,1.33379860697712E-5,-0.309616352203498));
#50939=CARTESIAN_POINT('',(-0.3933,-4.81653586104654E-17,-0.975));
#50940=CARTESIAN_POINT('Ctrl Pts',(-0.392672644806505,-3.40218946998094E-6,
-0.291283647796502));
#50941=CARTESIAN_POINT('Ctrl Pts',(-0.392667607343535,0.0654493539976286,
-0.294582059331564));
#50942=CARTESIAN_POINT('Ctrl Pts',(-0.377171222422322,0.130904364537333,
-0.297880470866626));
#50943=CARTESIAN_POINT('Ctrl Pts',(-0.346196882833469,0.187956111994733,
-0.301178882401688));
#50944=CARTESIAN_POINT('Ctrl Pts',(-0.284446679455652,0.301694033620098,
-0.307754570077918));
#50945=CARTESIAN_POINT('Ctrl Pts',(-0.16118073730096,0.382033941893919,
-0.314330257754149));
#50946=CARTESIAN_POINT('Ctrl Pts',(-0.0321942080223583,0.392610860537372,
-0.320905945430379));
#50947=CARTESIAN_POINT('Ctrl Pts',(0.0967923212562433,0.403187779180824,
-0.32748163310661));
#50948=CARTESIAN_POINT('Ctrl Pts',(0.231499437658754,0.344001708193907,
-0.33405732078284));
#50949=CARTESIAN_POINT('Ctrl Pts',(0.310953261656869,0.241842595997965,
-0.340633008459071));
#50950=CARTESIAN_POINT('Ctrl Pts',(0.390407085654983,0.139683483802024,
-0.347208696135302));
#50951=CARTESIAN_POINT('Ctrl Pts',(0.414607617248701,-0.00544866960294094,
-0.353784383811532));
#50952=CARTESIAN_POINT('Ctrl Pts',(0.372600716413692,-0.127861157977292,
-0.360360071487763));
#50953=CARTESIAN_POINT('Ctrl Pts',(0.330593815578682,-0.250273646351647,
-0.366935759163993));
#50954=CARTESIAN_POINT('Ctrl Pts',(0.222379482314941,-0.349966469695386,
-0.373511446840224));
#50955=CARTESIAN_POINT('Ctrl Pts',(0.0969398965000496,-0.381814644578891,
-0.380087134516455));
#50956=CARTESIAN_POINT('Ctrl Pts',(-0.0284996893148387,-0.413662819462395,
-0.386662822192686));
#50957=CARTESIAN_POINT('Ctrl Pts',(-0.171164527680877,-0.377666345885669,
-0.393238509868916));
#50958=CARTESIAN_POINT('Ctrl Pts',(-0.266478749744296,-0.290118673715471,
-0.399814197545147));
#50959=CARTESIAN_POINT('Ctrl Pts',(-0.3460533339709,-0.217028116376449,
-0.405304014295599));
#50960=CARTESIAN_POINT('Ctrl Pts',(-0.392624495852183,-0.108006327040057,
-0.410793831046051));
#50961=CARTESIAN_POINT('Ctrl Pts',(-0.393558983542489,0.000309099215769798,
-0.416283647796503));
#50962=CARTESIAN_POINT('Ctrl Pts',(-0.393587999858846,0.000300447727159551,
-0.434616352203498));
#50963=CARTESIAN_POINT('Ctrl Pts',(-0.392661402137344,-0.109031925299077,
-0.429073929389675));
#50964=CARTESIAN_POINT('Ctrl Pts',(-0.345088846953124,-0.219072095440072,
-0.423531506575852));
#50965=CARTESIAN_POINT('Ctrl Pts',(-0.264168911952582,-0.292223422497586,
-0.417989083762029));
#50966=CARTESIAN_POINT('Ctrl Pts',(-0.168163205203291,-0.379012232371915,
-0.411413396085799));
#50967=CARTESIAN_POINT('Ctrl Pts',(-0.02521731705165,-0.41387585365275,
-0.404837708409568));
#50968=CARTESIAN_POINT('Ctrl Pts',(0.0999656685633583,-0.381033604080488,
-0.398262020733337));
#50969=CARTESIAN_POINT('Ctrl Pts',(0.225148654178365,-0.348191354508227,
-0.391686333057106));
#50970=CARTESIAN_POINT('Ctrl Pts',(0.332568737256739,-0.24764323408287,
-0.385110645380876));
#50971=CARTESIAN_POINT('Ctrl Pts',(0.373603248787966,-0.124901381869836,
-0.378534957704645));
#50972=CARTESIAN_POINT('Ctrl Pts',(0.414637760319194,-0.00215952965679984,
-0.371959270028415));
#50973=CARTESIAN_POINT('Ctrl Pts',(0.389286700303273,0.142776054343914,
-0.365383582352184));
#50974=CARTESIAN_POINT('Ctrl Pts',(0.309024982211233,0.24430166525898,-0.358807894675953));
#50975=CARTESIAN_POINT('Ctrl Pts',(0.228763264119195,0.345827276174044,
-0.352232206999723));
#50976=CARTESIAN_POINT('Ctrl Pts',(0.0935908879510408,0.403942914003462,
-0.345656519323492));
#50977=CARTESIAN_POINT('Ctrl Pts',(-0.0353076671881922,0.392343101566332,
-0.339080831647261));
#50978=CARTESIAN_POINT('Ctrl Pts',(-0.164206222327427,0.380743289129201,
-0.332505143971031));
#50979=CARTESIAN_POINT('Ctrl Pts',(-0.286830956437741,0.29942802642552,
-0.3259294562948));
#50980=CARTESIAN_POINT('Ctrl Pts',(-0.347676962601307,0.185203870485553,
-0.319353768618569));
#50981=CARTESIAN_POINT('Ctrl Pts',(-0.377710977210929,0.128822027459561,
-0.316107963146879));
#50982=CARTESIAN_POINT('Ctrl Pts',(-0.39269273627193,0.0644220026535589,
-0.312862157675188));
#50983=CARTESIAN_POINT('Ctrl Pts',(-0.392673014342038,1.33379860697712E-5,
-0.309616352203498));
#50984=CARTESIAN_POINT('Origin',(0.,0.,-0.975));
#50985=CARTESIAN_POINT('',(-0.39357050162471,-0.000309514899277608,-0.166283647796502));
#50986=CARTESIAN_POINT('',(-0.393541380507519,-0.000314415350656495,-0.184616352203498));
#50987=CARTESIAN_POINT('',(-0.3933,-4.81653586104654E-17,-0.975));
#50988=CARTESIAN_POINT('Ctrl Pts',(-0.39357050162471,-0.000309514899277608,
-0.166283647796502));
#50989=CARTESIAN_POINT('Ctrl Pts',(-0.392638816960889,0.108414271758575,
-0.171794599940847));
#50990=CARTESIAN_POINT('Ctrl Pts',(-0.345667153138374,0.21784992059622,
-0.177305552085191));
#50991=CARTESIAN_POINT('Ctrl Pts',(-0.265552841170859,0.290968113516863,
-0.182816504229535));
#50992=CARTESIAN_POINT('Ctrl Pts',(-0.169960159525979,0.378213001061378,
-0.189392191905766));
#50993=CARTESIAN_POINT('Ctrl Pts',(-0.0271811390814353,0.413751465759291,
-0.195967879581997));
#50994=CARTESIAN_POINT('Ctrl Pts',(0.0981563482167165,0.381502906880402,
-0.202543567258227));
#50995=CARTESIAN_POINT('Ctrl Pts',(0.223493835514872,0.349254348001512,
-0.209119254934458));
#50996=CARTESIAN_POINT('Ctrl Pts',(0.331389789666634,0.249218765545815,
-0.215694942610689));
#50997=CARTESIAN_POINT('Ctrl Pts',(0.373006309497566,0.126673412826409,
-0.22227063028692));
#50998=CARTESIAN_POINT('Ctrl Pts',(0.414622829328497,0.00412806010700609,
-0.22884631796315));
#50999=CARTESIAN_POINT('Ctrl Pts',(0.389959914838601,-0.140927062876106,
-0.235422005639381));
#51000=CARTESIAN_POINT('Ctrl Pts',(0.310180910585397,-0.24283263818725,
-0.241997693315612));
#51001=CARTESIAN_POINT('Ctrl Pts',(0.230401906332192,-0.344738213498393,
-0.248573380991842));
#51002=CARTESIAN_POINT('Ctrl Pts',(0.0955068123156797,-0.403494241137569,
-0.255149068668073));
#51003=CARTESIAN_POINT('Ctrl Pts',(-0.0334453569779658,-0.392506156758443,
-0.261724756344303));
#51004=CARTESIAN_POINT('Ctrl Pts',(-0.162397526271611,-0.381518072379317,
-0.268300444020534));
#51005=CARTESIAN_POINT('Ctrl Pts',(-0.285406770842389,-0.300785875981889,
-0.274876131696764));
#51006=CARTESIAN_POINT('Ctrl Pts',(-0.346794160827309,-0.186851810294721,
-0.281451819372995));
#51007=CARTESIAN_POINT('Ctrl Pts',(-0.377389200992225,-0.130067879316267,
-0.284729095514164));
#51008=CARTESIAN_POINT('Ctrl Pts',(-0.392677649990676,-0.0650367535301259,
-0.288006371655333));
#51009=CARTESIAN_POINT('Ctrl Pts',(-0.392672644806505,-3.40218946998094E-6,
-0.291283647796502));
#51010=CARTESIAN_POINT('Ctrl Pts',(-0.392673014342038,1.33379860697712E-5,
-0.309616352203498));
#51011=CARTESIAN_POINT('Ctrl Pts',(-0.392652781551145,-0.0660637168975515,
-0.306286469998958));
#51012=CARTESIAN_POINT('Ctrl Pts',(-0.376843829560755,-0.132149865039833,
-0.302956587794418));
#51013=CARTESIAN_POINT('Ctrl Pts',(-0.345300981686382,-0.189596884509043,
-0.299626705589878));
#51014=CARTESIAN_POINT('Ctrl Pts',(-0.283011716391069,-0.303040434387422,
-0.293051017913647));
#51015=CARTESIAN_POINT('Ctrl Pts',(-0.159365907583621,-0.38279448496793,
-0.286475330237417));
#51016=CARTESIAN_POINT('Ctrl Pts',(-0.0303306494593879,-0.392759189393994,
-0.279899642561186));
#51017=CARTESIAN_POINT('Ctrl Pts',(0.098704608664847,-0.402723893820058,
-0.273323954884955));
#51018=CARTESIAN_POINT('Ctrl Pts',(0.23312931610587,-0.342899252091675,
-0.266748267208724));
#51019=CARTESIAN_POINT('Ctrl Pts',(0.312097431154972,-0.240364201991988,
-0.260172579532494));
#51020=CARTESIAN_POINT('Ctrl Pts',(0.391065546204075,-0.137829151892299,
-0.253596891856263));
#51021=CARTESIAN_POINT('Ctrl Pts',(0.414577068861256,0.00741630657869134,
-0.247021204180032));
#51022=CARTESIAN_POINT('Ctrl Pts',(0.37198971214902,0.12962799675346,-0.240445516503802));
#51023=CARTESIAN_POINT('Ctrl Pts',(0.329402355436786,0.251839686928225,
-0.233869828827571));
#51024=CARTESIAN_POINT('Ctrl Pts',(0.220716119355136,0.351017608806766,
-0.227294141151341));
#51025=CARTESIAN_POINT('Ctrl Pts',(0.0951268272738348,0.382270239135038,
-0.22071845347511));
#51026=CARTESIAN_POINT('Ctrl Pts',(-0.0304624648074687,0.413522869463311,
-0.214142765798879));
#51027=CARTESIAN_POINT('Ctrl Pts',(-0.172954812888427,0.376850208241315,
-0.207567078122649));
#51028=CARTESIAN_POINT('Ctrl Pts',(-0.26785250442914,0.288850996228523,
-0.200991390446418));
#51029=CARTESIAN_POINT('Ctrl Pts',(-0.346625169467209,0.215804620295093,
-0.195533044365445));
#51030=CARTESIAN_POINT('Ctrl Pts',(-0.392603563695526,0.107392576685488,
-0.190074698284471));
#51031=CARTESIAN_POINT('Ctrl Pts',(-0.393541380507519,-0.000314415350656495,
-0.184616352203498));
#51032=CARTESIAN_POINT('Origin',(0.,0.,-0.975));
#51033=CARTESIAN_POINT('',(-0.393507845663966,0.000361442601786236,-0.041283647796502));
#51034=CARTESIAN_POINT('',(-0.39355449651014,0.000302947205131077,-0.0596163522034978));
#51035=CARTESIAN_POINT('',(-0.3933,-4.81653586104654E-17,-0.975));
#51036=CARTESIAN_POINT('Ctrl Pts',(-0.393507845663966,0.000361442601786235,
-0.041283647796502));
#51037=CARTESIAN_POINT('Ctrl Pts',(-0.393708754658372,0.0229520255586643,
-0.0424314528738986));
#51038=CARTESIAN_POINT('Ctrl Pts',(-0.391919131196423,0.045518558677657,
-0.0435792579512952));
#51039=CARTESIAN_POINT('Ctrl Pts',(-0.388028994497127,0.0677340385174255,
-0.0447270630286917));
#51040=CARTESIAN_POINT('Ctrl Pts',(-0.365742698281716,0.195004826807769,
-0.0513027507049226));
#51041=CARTESIAN_POINT('Ctrl Pts',(-0.274516367855314,0.310753847632281,
-0.0578784383811535));
#51042=CARTESIAN_POINT('Ctrl Pts',(-0.155626506858587,0.361961149852793,
-0.0644541260573843));
#51043=CARTESIAN_POINT('Ctrl Pts',(-0.0367366458618627,0.413168452073304,
-0.0710298137336149));
#51044=CARTESIAN_POINT('Ctrl Pts',(0.109816745705184,0.399834035689818,
-0.0776055014098452));
#51045=CARTESIAN_POINT('Ctrl Pts',(0.217683740091212,0.328279870512349,
-0.0841811890860759));
#51046=CARTESIAN_POINT('Ctrl Pts',(0.32555073447724,0.256725705334881,-0.0907568767623065));
#51047=CARTESIAN_POINT('Ctrl Pts',(0.394731331682247,0.126951791363431,
-0.0973325644385373));
#51048=CARTESIAN_POINT('Ctrl Pts',(0.393919645176791,-0.00244560881035578,
-0.103908252114768));
#51049=CARTESIAN_POINT('Ctrl Pts',(0.393107958671335,-0.131843008984141,
-0.110483939790998));
#51050=CARTESIAN_POINT('Ctrl Pts',(0.322303988455414,-0.260863895360267,
-0.117059627467229));
#51051=CARTESIAN_POINT('Ctrl Pts',(0.213552187511225,-0.331033249415431,
-0.123635315143459));
#51052=CARTESIAN_POINT('Ctrl Pts',(0.10480038656703,-0.401202603470599,
-0.13021100281969));
#51053=CARTESIAN_POINT('Ctrl Pts',(-0.0418992451054321,-0.412520425204803,
-0.136786690495921));
#51054=CARTESIAN_POINT('Ctrl Pts',(-0.160142282896379,-0.359902860717048,
-0.143362378172152));
#51055=CARTESIAN_POINT('Ctrl Pts',(-0.278385320687322,-0.307285296229296,
-0.149938065848383));
#51056=CARTESIAN_POINT('Ctrl Pts',(-0.368171764596748,-0.190732345519584,
-0.156513753524613));
#51057=CARTESIAN_POINT('Ctrl Pts',(-0.38886181512885,-0.0629802149691723,
-0.163089441200844));
#51058=CARTESIAN_POINT('Ctrl Pts',(-0.392211948687912,-0.0422945864283189,
-0.16415417673273));
#51059=CARTESIAN_POINT('Ctrl Pts',(-0.393750506411561,-0.0213153367216679,
-0.165218912264616));
#51060=CARTESIAN_POINT('Ctrl Pts',(-0.39357050162471,-0.000309514899277608,
-0.166283647796502));
#51061=CARTESIAN_POINT('Ctrl Pts',(-0.393541380507519,-0.000314415350656495,
-0.184616352203498));
#51062=CARTESIAN_POINT('Ctrl Pts',(-0.393733354727773,-0.0223623948148967,
-0.18349901060824));
#51063=CARTESIAN_POINT('Ctrl Pts',(-0.392037973295506,-0.0443808301847042,
-0.182381669012983));
#51064=CARTESIAN_POINT('Ctrl Pts',(-0.38835019013725,-0.066060314914406,
-0.181264327417726));
#51065=CARTESIAN_POINT('Ctrl Pts',(-0.366647149304176,-0.193646651240961,
-0.174688639741495));
#51066=CARTESIAN_POINT('Ctrl Pts',(-0.275938032637555,-0.309493561090483,
-0.168112952065265));
#51067=CARTESIAN_POINT('Ctrl Pts',(-0.157281747236539,-0.361166943295072,
-0.161537264389034));
#51068=CARTESIAN_POINT('Ctrl Pts',(-0.0386254618355239,-0.412840325499661,
-0.154961576712803));
#51069=CARTESIAN_POINT('Ctrl Pts',(0.107977992299886,-0.400340180059318,
-0.148385889036573));
#51070=CARTESIAN_POINT('Ctrl Pts',(0.21617053708177,-0.329319039665975,
-0.141810201360342));
#51071=CARTESIAN_POINT('Ctrl Pts',(0.324363081863656,-0.258297899272631,
-0.135234513684112));
#51072=CARTESIAN_POINT('Ctrl Pts',(0.394144717292015,-0.128755763926285,
-0.128658826007881));
#51073=CARTESIAN_POINT('Ctrl Pts',(0.393928367963568,0.000660750832538935,
-0.12208313833165));
#51074=CARTESIAN_POINT('Ctrl Pts',(0.393712018635121,0.130077265591359,
-0.11550745065542));
#51075=CARTESIAN_POINT('Ctrl Pts',(0.323497684549871,0.259368159762656,
-0.108931762979189));
#51076=CARTESIAN_POINT('Ctrl Pts',(0.215069295256064,0.330031485880104,
-0.102356075302959));
#51077=CARTESIAN_POINT('Ctrl Pts',(0.106640905962253,0.400694811997555,
-0.095780387626728));
#51078=CARTESIAN_POINT('Ctrl Pts',(-0.0400015385401184,0.412730570061151,
-0.0892046999504971));
#51079=CARTESIAN_POINT('Ctrl Pts',(-0.158485743372544,0.360651915243996,
-0.0826290122742663));
#51080=CARTESIAN_POINT('Ctrl Pts',(-0.276969948204966,0.308573260426843,
-0.0760533245980357));
#51081=CARTESIAN_POINT('Ctrl Pts',(-0.367295913367443,0.192380192728942,
-0.0694776369218051));
#51082=CARTESIAN_POINT('Ctrl Pts',(-0.388570758753071,0.0647411738202655,
-0.0629019492455745));
#51083=CARTESIAN_POINT('Ctrl Pts',(-0.392114143238029,0.0434825413330083,
-0.061806750231549));
#51084=CARTESIAN_POINT('Ctrl Pts',(-0.393742061671785,0.0219064001501816,
-0.0607115512175234));
#51085=CARTESIAN_POINT('Ctrl Pts',(-0.39355449651014,0.000302947205131077,
-0.0596163522034978));
#51086=CARTESIAN_POINT('Origin',(0.,0.,-2.18777734492731));
#51087=CARTESIAN_POINT('',(-0.322496652456404,-0.000253620427588302,-0.125277344927309));
#51088=CARTESIAN_POINT('',(-0.322483537662866,0.00024823877578703,-0.100622655072689));
#51089=CARTESIAN_POINT('',(-0.322275,-3.08760083991297E-14,-2.18777734492731));
#51090=CARTESIAN_POINT('',(-0.104132061245188,0.305520369126831,-0.0250000000000002));
#51091=CARTESIAN_POINT('Ctrl Pts',(-0.322496652456404,-0.000253620427588306,
-0.125277344927308));
#51092=CARTESIAN_POINT('Ctrl Pts',(-0.322644150657985,-0.0174660568064599,
-0.124212609395423));
#51093=CARTESIAN_POINT('Ctrl Pts',(-0.313597410155885,-0.140824332617286,
-0.116572186187306));
#51094=CARTESIAN_POINT('Ctrl Pts',(-0.154540307687754,-0.347298426219855,
-0.102356075302959));
#51095=CARTESIAN_POINT('Ctrl Pts',(0.206082299461314,-0.319476526910996,
-0.0826290122742663));
#51096=CARTESIAN_POINT('Ctrl Pts',(0.380135308624816,-0.00231248299897462,
-0.0629019492455747));
#51097=CARTESIAN_POINT('Ctrl Pts',(0.214533253773463,0.308335699989221,
-0.0436922784874857));
#51098=CARTESIAN_POINT('Ctrl Pts',(-0.0114010986281019,0.336540681884783,
-0.0310582954056278));
#51099=CARTESIAN_POINT('Ctrl Pts',(-0.104132061245188,0.305520369126832,
-0.0250000000000003));
#51100=CARTESIAN_POINT('',(0.254670486854674,0.19749460435719,-0.0249999999999999));
#51101=CARTESIAN_POINT('Origin',(0.,0.,-0.0249999999999999));
#51102=CARTESIAN_POINT('Ctrl Pts',(-0.322483537662866,0.000248238775787049,
-0.100622655072689));
#51103=CARTESIAN_POINT('Ctrl Pts',(-0.321714440718607,-0.0883351074034859,
-0.0951421664104844));
#51104=CARTESIAN_POINT('Ctrl Pts',(-0.238074661536136,-0.284436749901765,
-0.0830859900720496));
#51105=CARTESIAN_POINT('Ctrl Pts',(0.0930026936990432,-0.368843116278878,
-0.0644541260573834));
#51106=CARTESIAN_POINT('Ctrl Pts',(0.359454556187757,-0.123370117592038,
-0.0447270630286919));
#51107=CARTESIAN_POINT('Ctrl Pts',(0.319948400855436,0.113318339423062,
-0.0315756876762305));
#51108=CARTESIAN_POINT('Ctrl Pts',(0.254670486854674,0.19749460435719,-0.0249999999999999));
#51109=CARTESIAN_POINT('Origin',(0.,0.,-2.18777734492731));
#51110=CARTESIAN_POINT('',(-0.321760937210822,-2.78779714989989E-6,-0.250277344927308));
#51111=CARTESIAN_POINT('',(-0.322472790244243,-0.000257635919520965,-0.225622655072689));
#51112=CARTESIAN_POINT('',(-0.322275,-3.08760083991297E-14,-2.18777734492731));
#51113=CARTESIAN_POINT('Ctrl Pts',(-0.321760937210822,-2.7877971498988E-6,
-0.250277344927308));
#51114=CARTESIAN_POINT('Ctrl Pts',(-0.321765038522105,-0.053291939343827,
-0.247000068786139));
#51115=CARTESIAN_POINT('Ctrl Pts',(-0.284101601363802,-0.213497576922093,
-0.23714710496874));
#51116=CARTESIAN_POINT('Ctrl Pts',(-0.032275256763624,-0.378773723290174,
-0.22071845347511));
#51117=CARTESIAN_POINT('Ctrl Pts',(0.299328987509231,-0.234337424225216,
-0.200991390446418));
#51118=CARTESIAN_POINT('Ctrl Pts',(0.359956300760417,0.122242589194944,
-0.181264327417726));
#51119=CARTESIAN_POINT('Ctrl Pts',(0.0947223676997066,0.368153857966175,
-0.161537264389034));
#51120=CARTESIAN_POINT('Ctrl Pts',(-0.237318620500534,0.285507073440862,
-0.142874936892228));
#51121=CARTESIAN_POINT('Ctrl Pts',(-0.321733218245798,0.0888360270302314,
-0.130788297071653));
#51122=CARTESIAN_POINT('Ctrl Pts',(-0.322496652456404,-0.000253620427588306,
-0.125277344927308));
#51123=CARTESIAN_POINT('Ctrl Pts',(-0.322472790244243,-0.000257635919520943,
-0.225622655072689));
#51124=CARTESIAN_POINT('Ctrl Pts',(-0.322630096351111,-0.0183240294660091,
-0.224505313477432));
#51125=CARTESIAN_POINT('Ctrl Pts',(-0.313065172617578,-0.142546609137769,
-0.216812284205945));
#51126=CARTESIAN_POINT('Ctrl Pts',(-0.151778919131785,-0.348529367587568,
-0.202543567258227));
#51127=CARTESIAN_POINT('Ctrl Pts',(0.208607260742278,-0.317801035232212,
-0.182816504229535));
#51128=CARTESIAN_POINT('Ctrl Pts',(0.380147127696309,0.000644362698709406,
-0.163089441200843));
#51129=CARTESIAN_POINT('Ctrl Pts',(0.207543584467282,0.318472150029413,
-0.143362378172152));
#51130=CARTESIAN_POINT('Ctrl Pts',(-0.152938443007933,0.348058907694893,
-0.12363531514346));
#51131=CARTESIAN_POINT('Ctrl Pts',(-0.313294198957135,0.141781264569365,
-0.109388740776972));
#51132=CARTESIAN_POINT('Ctrl Pts',(-0.322637230931287,0.0179503816638393,
-0.101717854086715));
#51133=CARTESIAN_POINT('Ctrl Pts',(-0.322483537662866,0.000248238775787049,
-0.100622655072689));
#51134=CARTESIAN_POINT('Origin',(0.,0.,-2.18777734492731));
#51135=CARTESIAN_POINT('',(-0.322487214393989,0.000253279811224501,-0.375277344927309));
#51136=CARTESIAN_POINT('',(-0.321761240012917,1.0929314634589E-5,-0.350622655072689));
#51137=CARTESIAN_POINT('',(-0.322275,-3.08760083991297E-14,-2.18777734492731));
#51138=CARTESIAN_POINT('Ctrl Pts',(-0.322487214393989,0.000253279811224492,
-0.375277344927309));
#51139=CARTESIAN_POINT('Ctrl Pts',(-0.321721483347979,-0.0885017519624719,
-0.369787528176857));
#51140=CARTESIAN_POINT('Ctrl Pts',(-0.237851341202248,-0.28483941242138,
-0.357722023750175));
#51141=CARTESIAN_POINT('Ctrl Pts',(0.093548368701956,-0.368456518342696,
-0.339080831647262));
#51142=CARTESIAN_POINT('Ctrl Pts',(0.359564953389757,-0.12338783304061,
-0.319353768618569));
#51143=CARTESIAN_POINT('Ctrl Pts',(0.300074287338146,0.233381539488646,
-0.299626705589878));
#51144=CARTESIAN_POINT('Ctrl Pts',(-0.0310678632234075,0.378874987446754,
-0.279899642561186));
#51145=CARTESIAN_POINT('Ctrl Pts',(-0.283744372563332,0.214190345213263,
-0.263449855673663));
#51146=CARTESIAN_POINT('Ctrl Pts',(-0.321756809449883,0.0536300293912535,
-0.25357575646237));
#51147=CARTESIAN_POINT('Ctrl Pts',(-0.321760937210822,-2.7877971498988E-6,
-0.250277344927308));
#51148=CARTESIAN_POINT('Ctrl Pts',(-0.321761240012917,1.09293146345925E-5,
-0.350622655072689));
#51149=CARTESIAN_POINT('Ctrl Pts',(-0.321744661007864,-0.0541334461306104,
-0.34729277286815));
#51150=CARTESIAN_POINT('Ctrl Pts',(-0.283209573736967,-0.215221637656999,
-0.33738720298738));
#51151=CARTESIAN_POINT('Ctrl Pts',(-0.029269501228293,-0.379018126859581,
-0.320905945430379));
#51152=CARTESIAN_POINT('Ctrl Pts',(0.301178420896456,-0.231954920047871,
-0.301178882401687));
#51153=CARTESIAN_POINT('Ctrl Pts',(0.358975339007382,0.125092983298727,
-0.281451819372995));
#51154=CARTESIAN_POINT('Ctrl Pts',(0.0917987048867537,0.368895918259873,
-0.261724756344303));
#51155=CARTESIAN_POINT('Ctrl Pts',(-0.238641519661772,0.283851896091718,
-0.243115034910868));
#51156=CARTESIAN_POINT('Ctrl Pts',(-0.321704331273786,0.0879988371505342,
-0.231081001153663));
#51157=CARTESIAN_POINT('Ctrl Pts',(-0.322472790244243,-0.000257635919520943,
-0.225622655072689));
#51158=CARTESIAN_POINT('Origin',(0.,0.,-2.18777734492731));
#51159=CARTESIAN_POINT('',(-0.322468464145128,-0.000258307126375694,-0.500277344927309));
#51160=CARTESIAN_POINT('',(-0.322510990731018,0.000246190671888573,-0.475622655072689));
#51161=CARTESIAN_POINT('',(-0.322275,-3.08760083991297E-14,-2.18777734492731));
#51162=CARTESIAN_POINT('Ctrl Pts',(-0.322468464145128,-0.000258307126375657,
-0.500277344927309));
#51163=CARTESIAN_POINT('Ctrl Pts',(-0.322627489692965,-0.0184761631570425,
-0.499150675243805));
#51164=CARTESIAN_POINT('Ctrl Pts',(-0.312969978781256,-0.142852070661369,
-0.49144831788407));
#51165=CARTESIAN_POINT('Ctrl Pts',(-0.151288792665831,-0.348745193702454,
-0.477170272848105));
#51166=CARTESIAN_POINT('Ctrl Pts',(0.209054616084237,-0.317502246064031,
-0.457443209819413));
#51167=CARTESIAN_POINT('Ctrl Pts',(0.380144895279971,0.00116938758285907,
-0.437716146790722));
#51168=CARTESIAN_POINT('Ctrl Pts',(0.207097300423056,0.318782398141369,
-0.41798908376203));
#51169=CARTESIAN_POINT('Ctrl Pts',(-0.15343150362219,0.34780782307336,-0.398262020733337));
#51170=CARTESIAN_POINT('Ctrl Pts',(-0.313384552995844,0.141515052741351,
-0.384024774455097));
#51171=CARTESIAN_POINT('Ctrl Pts',(-0.322638673926724,0.0178087853773642,
-0.376363215853088));
#51172=CARTESIAN_POINT('Ctrl Pts',(-0.322487214393989,0.000253279811224492,
-0.375277344927309));
#51173=CARTESIAN_POINT('Ctrl Pts',(-0.322510990731018,0.000246190671888582,
-0.475622655072689));
#51174=CARTESIAN_POINT('Ctrl Pts',(-0.321751724825343,-0.0893421401621455,
-0.470080232258867));
#51175=CARTESIAN_POINT('Ctrl Pts',(-0.236521348985171,-0.286488688677642,
-0.457962121768814));
#51176=CARTESIAN_POINT('Ctrl Pts',(0.096468281849101,-0.367702807740199,
-0.43926832360253));
#51177=CARTESIAN_POINT('Ctrl Pts',(0.360532410560641,-0.120531598662528,
-0.419541260573839));
#51178=CARTESIAN_POINT('Ctrl Pts',(0.298213471837286,0.235754559490252,
-0.399814197545147));
#51179=CARTESIAN_POINT('Ctrl Pts',(-0.0340723979536573,0.378616627998834,
-0.380087134516455));
#51180=CARTESIAN_POINT('Ctrl Pts',(-0.284630677265904,0.212465708670196,
-0.363689953692302));
#51181=CARTESIAN_POINT('Ctrl Pts',(-0.321777400411997,0.0527882046914952,
-0.35386846054438));
#51182=CARTESIAN_POINT('Ctrl Pts',(-0.321761240012917,1.09293146345925E-5,
-0.350622655072689));
#51183=CARTESIAN_POINT('Origin',(0.,0.,-2.18777734492731));
#51184=CARTESIAN_POINT('',(-0.32176143791031,1.33594009879692E-5,-0.625277344927309));
#51185=CARTESIAN_POINT('',(-0.322443941546287,-0.000264174642984033,-0.600622655072689));
#51186=CARTESIAN_POINT('',(-0.322275,-3.08760083991297E-14,-2.18777734492731));
#51187=CARTESIAN_POINT('Ctrl Pts',(-0.32176143791031,1.33594009879487E-5,
-0.625277344927309));
#51188=CARTESIAN_POINT('Ctrl Pts',(-0.32174112470711,-0.0542826208959099,
-0.621938134634522));
#51189=CARTESIAN_POINT('Ctrl Pts',(-0.283050431304305,-0.215527298967927,
-0.612023236665505));
#51190=CARTESIAN_POINT('Ctrl Pts',(-0.0287363371895775,-0.37905900832026,
-0.595532651020257));
#51191=CARTESIAN_POINT('Ctrl Pts',(0.30150443573772,-0.231530957091147,
-0.575805587991564));
#51192=CARTESIAN_POINT('Ctrl Pts',(0.358799032608658,0.125597623625804,
-0.556078524962874));
#51193=CARTESIAN_POINT('Ctrl Pts',(0.0912797550693568,0.36902508747417,
-0.53635146193418));
#51194=CARTESIAN_POINT('Ctrl Pts',(-0.238875075374452,0.283558159143536,
-0.517751068588993));
#51195=CARTESIAN_POINT('Ctrl Pts',(-0.321699354010936,0.0878504143147682,
-0.505726362920035));
#51196=CARTESIAN_POINT('Ctrl Pts',(-0.322468464145128,-0.000258307126375657,
-0.500277344927309));
#51197=CARTESIAN_POINT('Ctrl Pts',(-0.322443941546287,-0.000264174642983971,
-0.600622655072689));
#51198=CARTESIAN_POINT('Ctrl Pts',(-0.32261252448504,-0.0193364043208577,
-0.599443379325814));
#51199=CARTESIAN_POINT('Ctrl Pts',(-0.312428596949323,-0.144576424763027,
-0.591688415902709));
#51200=CARTESIAN_POINT('Ctrl Pts',(-0.148517520713027,-0.349934323902057,
-0.577357764803375));
#51201=CARTESIAN_POINT('Ctrl Pts',(0.211566678587274,-0.315833857421815,
-0.557630701774681));
#51202=CARTESIAN_POINT('Ctrl Pts',(0.380123626347935,0.00418493532934027,
-0.537903638745991));
#51203=CARTESIAN_POINT('Ctrl Pts',(0.204561954486446,0.320415186635358,
-0.518176575717298));
#51204=CARTESIAN_POINT('Ctrl Pts',(-0.156185726714996,0.346579721946209,
-0.498449512688607));
#51205=CARTESIAN_POINT('Ctrl Pts',(-0.313912311423948,0.139791502294731,
-0.484264872473737));
#51206=CARTESIAN_POINT('Ctrl Pts',(-0.322652539437768,0.0169479973441946,
-0.476655919935097));
#51207=CARTESIAN_POINT('Ctrl Pts',(-0.322510990731018,0.000246190671888582,
-0.475622655072689));
#51208=CARTESIAN_POINT('Origin',(0.,0.,-2.18777734492731));
#51209=CARTESIAN_POINT('',(-0.322515189627379,0.000244863147638563,-0.750277344927309));
#51210=CARTESIAN_POINT('',(-0.321763022562619,2.70116077047966E-5,-0.72562265507269));
#51211=CARTESIAN_POINT('',(-0.322275,-3.08760083991297E-14,-2.18777734492731));
#51212=CARTESIAN_POINT('Ctrl Pts',(-0.322515189627379,0.000244863147638597,
-0.750277344927309));
#51213=CARTESIAN_POINT('Ctrl Pts',(-0.321757324772481,-0.0894912350280718,
-0.744725594025239));
#51214=CARTESIAN_POINT('Ctrl Pts',(-0.236284363982717,-0.286780837770945,
-0.73259815544694));
#51215=CARTESIAN_POINT('Ctrl Pts',(0.0969854205621785,-0.36756677904974,
-0.713895029192408));
#51216=CARTESIAN_POINT('Ctrl Pts',(0.36070162869546,-0.120024347192654,
-0.694167966163718));
#51217=CARTESIAN_POINT('Ctrl Pts',(0.297881578716796,0.236173821419171,
-0.674440903135024));
#51218=CARTESIAN_POINT('Ctrl Pts',(-0.0346049444254762,0.378568364610783,
-0.654713840106333));
#51219=CARTESIAN_POINT('Ctrl Pts',(-0.284786878082418,0.212159852647683,
-0.638325987370427));
#51220=CARTESIAN_POINT('Ctrl Pts',(-0.32178112616501,0.0526388896416031,
-0.628513822310753));
#51221=CARTESIAN_POINT('Ctrl Pts',(-0.32176143791031,1.33594009879487E-5,
-0.625277344927309));
#51222=CARTESIAN_POINT('Ctrl Pts',(-0.321763022562619,2.70116077047897E-5,
-0.72562265507269));
#51223=CARTESIAN_POINT('Ctrl Pts',(-0.32172129192177,-0.0551236550340476,
-0.722230838716532));
#51224=CARTESIAN_POINT('Ctrl Pts',(-0.282147174958169,-0.217250635635261,
-0.712263334684144));
#51225=CARTESIAN_POINT('Ctrl Pts',(-0.0257284602956936,-0.379275007515933,
-0.695720142975526));
#51226=CARTESIAN_POINT('Ctrl Pts',(0.303331595228502,-0.22913190160076,
-0.675993079946833));
#51227=CARTESIAN_POINT('Ctrl Pts',(0.357791382294441,0.128439914943824,
-0.656266016918142));
#51228=CARTESIAN_POINT('Ctrl Pts',(0.0883495014317826,0.369737542850607,
-0.63653895388945));
#51229=CARTESIAN_POINT('Ctrl Pts',(-0.240185123468634,0.281903402878257,
-0.617991166607633));
#51230=CARTESIAN_POINT('Ctrl Pts',(-0.321672499426679,0.0870110941191312,
-0.606019067002045));
#51231=CARTESIAN_POINT('Ctrl Pts',(-0.322443941546287,-0.000264174642983971,
-0.600622655072689));
#51232=CARTESIAN_POINT('Origin',(0.,0.,-2.18777734492731));
#51233=CARTESIAN_POINT('',(-0.32243959144629,-0.00026514217618365,-0.875277344927309));
#51234=CARTESIAN_POINT('',(-0.322538390303182,0.000236984608253048,-0.850622655072689));
#51235=CARTESIAN_POINT('',(-0.322275,-3.08760083991297E-14,-2.18777734492731));
#51236=CARTESIAN_POINT('Ctrl Pts',(-0.32243959144629,-0.00026514217618364,
-0.875277344927309));
#51237=CARTESIAN_POINT('Ctrl Pts',(-0.322609842324708,-0.0194889104434921,
-0.874088741092187));
#51238=CARTESIAN_POINT('Ctrl Pts',(-0.312331827063556,-0.144882247836869,
-0.866324449580835));
#51239=CARTESIAN_POINT('Ctrl Pts',(-0.148025153650298,-0.350142917605659,
-0.851984470393253));
#51240=CARTESIAN_POINT('Ctrl Pts',(0.212010751987255,-0.315535972441172,
-0.832257407364559));
#51241=CARTESIAN_POINT('Ctrl Pts',(0.380117394971352,0.00471962951840088,
-0.81253034433587));
#51242=CARTESIAN_POINT('Ctrl Pts',(0.204111059463726,0.320702641503297,
-0.792803281307175));
#51243=CARTESIAN_POINT('Ctrl Pts',(-0.156673098749063,0.346359710403747,
-0.773076218278485));
#51244=CARTESIAN_POINT('Ctrl Pts',(-0.314005130821476,0.139485946692706,
-0.758900906151862));
#51245=CARTESIAN_POINT('Ctrl Pts',(-0.322654966376816,0.0167953338932892,
-0.75130128170147));
#51246=CARTESIAN_POINT('Ctrl Pts',(-0.322515189627379,0.000244863147638597,
-0.750277344927309));
#51247=CARTESIAN_POINT('Ctrl Pts',(-0.322538390303182,0.000236984608253082,
-0.85062265507269));
#51248=CARTESIAN_POINT('Ctrl Pts',(-0.321789907494861,-0.0903324194305184,
-0.845018298107249));
#51249=CARTESIAN_POINT('Ctrl Pts',(-0.234941113718784,-0.288426386720931,
-0.832838253465578));
#51250=CARTESIAN_POINT('Ctrl Pts',(0.0998981666172007,-0.366785824837531,
-0.814082521147678));
#51251=CARTESIAN_POINT('Ctrl Pts',(0.361642369567447,-0.117159214442841,
-0.794355458118984));
#51252=CARTESIAN_POINT('Ctrl Pts',(0.295998679758828,0.238529383045872,
-0.774628395090294));
#51253=CARTESIAN_POINT('Ctrl Pts',(-0.0376069309429452,0.37828191040585,
-0.754901332061601));
#51254=CARTESIAN_POINT('Ctrl Pts',(-0.285662062070785,0.210434559988762,
-0.738566085389067));
#51255=CARTESIAN_POINT('Ctrl Pts',(-0.321802194786766,0.0517965083508985,
-0.728806526392763));
#51256=CARTESIAN_POINT('Ctrl Pts',(-0.321763022562619,2.70116077047897E-5,
-0.72562265507269));
#51257=CARTESIAN_POINT('Origin',(0.,0.,-2.18777734492731));
#51258=CARTESIAN_POINT('',(-0.321763448536774,2.94270121017112E-5,-1.00027734492731));
#51259=CARTESIAN_POINT('',(-0.322414722935121,-0.000270183965801862,-0.97562265507269));
#51260=CARTESIAN_POINT('',(-0.322275,-3.08760083991297E-14,-2.18777734492731));
#51261=CARTESIAN_POINT('Ctrl Pts',(-0.321763448536774,2.94270121016932E-5,
-1.00027734492731));
#51262=CARTESIAN_POINT('Ctrl Pts',(-0.321717858026619,-0.0552727465775086,
-0.996876200482905));
#51263=CARTESIAN_POINT('Ctrl Pts',(-0.281986038527001,-0.217556162740986,
-0.986899368362269));
#51264=CARTESIAN_POINT('Ctrl Pts',(-0.0251949327277424,-0.379310854349625,
-0.970346848565404));
#51265=CARTESIAN_POINT('Ctrl Pts',(0.303653626791853,-0.228705014808928,
-0.950619785536712));
#51266=CARTESIAN_POINT('Ctrl Pts',(0.357610388862838,0.128943082947354,
-0.930892722508019));
#51267=CARTESIAN_POINT('Ctrl Pts',(0.0878293328830358,0.3698614837313,-0.911165659479328));
#51268=CARTESIAN_POINT('Ctrl Pts',(-0.240416277942781,0.281609698819248,
-0.892627200285757));
#51269=CARTESIAN_POINT('Ctrl Pts',(-0.321667967016886,0.0868623332180409,
-0.880664428768418));
#51270=CARTESIAN_POINT('Ctrl Pts',(-0.32243959144629,-0.00026514217618364,
-0.875277344927309));
#51271=CARTESIAN_POINT('Ctrl Pts',(-0.322414722935121,-0.000270183965801866,
-0.97562265507269));
#51272=CARTESIAN_POINT('Ctrl Pts',(-0.322594207704359,-0.0203487694477343,
-0.974381445174198));
#51273=CARTESIAN_POINT('Ctrl Pts',(-0.311781374671243,-0.146607127922807,
-0.966564547599475));
#51274=CARTESIAN_POINT('Ctrl Pts',(-0.145242896892136,-0.351306114233161,
-0.952171962348521));
#51275=CARTESIAN_POINT('Ctrl Pts',(0.214507123315248,-0.313844195489162,
-0.932444899319828));
#51276=CARTESIAN_POINT('Ctrl Pts',(0.380067963842326,0.00773484686148907,
-0.912717836291137));
#51277=CARTESIAN_POINT('Ctrl Pts',(0.20156057492959,0.322311680876253,-0.892990773262445));
#51278=CARTESIAN_POINT('Ctrl Pts',(-0.159415732015043,0.345105939359686,
-0.873263710233753));
#51279=CARTESIAN_POINT('Ctrl Pts',(-0.314523961336012,0.137762968037702,
-0.859141004170502));
#51280=CARTESIAN_POINT('Ctrl Pts',(-0.322668115148103,0.015934208061963,
-0.85159398578348));
#51281=CARTESIAN_POINT('Ctrl Pts',(-0.322538390303182,0.000236984608253082,
-0.85062265507269));
#51282=CARTESIAN_POINT('Origin',(0.,0.,-2.18777734492731));
#51283=CARTESIAN_POINT('',(-0.322542478777324,0.000235518785689083,-1.12527734492731));
#51284=CARTESIAN_POINT('',(-0.321766314000566,4.30053259428964E-5,-1.10062265507269));
#51285=CARTESIAN_POINT('',(-0.322275,-3.08760083991297E-14,-2.18777734492731));
#51286=CARTESIAN_POINT('Ctrl Pts',(-0.322542478777324,0.000235518785689073,
-1.12527734492731));
#51287=CARTESIAN_POINT('Ctrl Pts',(-0.321795926838285,-0.0904816611753488,
-1.11966365987362));
#51288=CARTESIAN_POINT('Ctrl Pts',(-0.234701773596145,-0.288717865815097,
-1.1074742871437));
#51289=CARTESIAN_POINT('Ctrl Pts',(0.100414012462523,-0.366644971278448,
-1.08870922673756));
#51290=CARTESIAN_POINT('Ctrl Pts',(0.361806842748681,-0.116650406783812,
-1.06898216370886));
#51291=CARTESIAN_POINT('Ctrl Pts',(0.295662885863291,0.2389455310015,-1.04925510068017));
#51292=CARTESIAN_POINT('Ctrl Pts',(-0.0381390041496891,0.378228667904838,
-1.02952803765148));
#51293=CARTESIAN_POINT('Ctrl Pts',(-0.285816294598986,0.210128591668202,
-1.01320211906719));
#51294=CARTESIAN_POINT('Ctrl Pts',(-0.321806001579673,0.0516470938721495,
-1.00345188815914));
#51295=CARTESIAN_POINT('Ctrl Pts',(-0.321763448536774,2.94270121016932E-5,
-1.00027734492731));
#51296=CARTESIAN_POINT('Ctrl Pts',(-0.321766314000566,4.30053259428721E-5,
-1.10062265507269));
#51297=CARTESIAN_POINT('Ctrl Pts',(-0.321698621501294,-0.0561132696767489,
-1.09716890456491));
#51298=CARTESIAN_POINT('Ctrl Pts',(-0.281071497630043,-0.219278629537744,
-1.08713946638091));
#51299=CARTESIAN_POINT('Ctrl Pts',(-0.022185169729932,-0.379498752618868,
-1.07053434052067));
#51300=CARTESIAN_POINT('Ctrl Pts',(0.305458301062517,-0.226288999527647,
-1.05080727749198));
#51301=CARTESIAN_POINT('Ctrl Pts',(0.356576237443244,0.131775839538367,
-1.03108021446329));
#51302=CARTESIAN_POINT('Ctrl Pts',(0.0848925531951284,0.370546541485998,
-1.0113531514346));
#51303=CARTESIAN_POINT('Ctrl Pts',(-0.241713188057519,0.279951469622511,
-0.992867298304396));
#51304=CARTESIAN_POINT('Ctrl Pts',(-0.321643332444194,0.0860236557722655,
-0.980957132850428));
#51305=CARTESIAN_POINT('Ctrl Pts',(-0.322414722935121,-0.000270183965801866,
-0.97562265507269));
#51306=CARTESIAN_POINT('Origin',(0.,0.,-2.18777734492731));
#51307=CARTESIAN_POINT('',(-0.322410319385532,-0.000271004193501387,-1.25027734492731));
#51308=CARTESIAN_POINT('',(-0.322565009168808,0.000226870584957552,-1.22562265507269));
#51309=CARTESIAN_POINT('',(-0.322275,-3.08760083991297E-14,-2.18777734492731));
#51310=CARTESIAN_POINT('Ctrl Pts',(-0.322410319385532,-0.000271004193501456,
-1.25027734492731));
#51311=CARTESIAN_POINT('Ctrl Pts',(-0.32259140864452,-0.0205012064117319,
-1.24902680694057));
#51312=CARTESIAN_POINT('Ctrl Pts',(-0.311682991233502,-0.146913042759608,
-1.2412005812776));
#51313=CARTESIAN_POINT('Ctrl Pts',(-0.144748603181605,-0.351510100480195,
-1.2267986679384));
#51314=CARTESIAN_POINT('Ctrl Pts',(0.214948395308735,-0.313542176137101,
-1.20707160490971));
#51315=CARTESIAN_POINT('Ctrl Pts',(0.380056739056546,0.00826945949266903,
-1.18734454188101));
#51316=CARTESIAN_POINT('Ctrl Pts',(0.201107014947573,0.322594912237434,
-1.16761747885232));
#51317=CARTESIAN_POINT('Ctrl Pts',(-0.15990102805103,0.344881385538304,
-1.14789041582363));
#51318=CARTESIAN_POINT('Ctrl Pts',(-0.314615202650056,0.137457515057215,
-1.13377703784863));
#51319=CARTESIAN_POINT('Ctrl Pts',(-0.322670413443474,0.0157814862202043,
-1.12623934754985));
#51320=CARTESIAN_POINT('Ctrl Pts',(-0.322542478777324,0.000235518785689073,
-1.12527734492731));
#51321=CARTESIAN_POINT('Ctrl Pts',(-0.322565009168808,0.00022687058495755,
-1.22562265507269));
#51322=CARTESIAN_POINT('Ctrl Pts',(-0.321830898403645,-0.0913237050652294,
-1.21995636395563));
#51323=CARTESIAN_POINT('Ctrl Pts',(-0.233345219009216,-0.290359580072423,
-1.20771438516234));
#51324=CARTESIAN_POINT('Ctrl Pts',(0.103319337909045,-0.365836848074736,
-1.18889671869282));
#51325=CARTESIAN_POINT('Ctrl Pts',(0.362720784217591,-0.113776613114465,
-1.16916965566413));
#51326=CARTESIAN_POINT('Ctrl Pts',(0.293758069692678,0.241283404911434,
-1.14944259263544));
#51327=CARTESIAN_POINT('Ctrl Pts',(-0.0411381844576584,0.377914189697542,
-1.12971552960675));
#51328=CARTESIAN_POINT('Ctrl Pts',(-0.286680415754695,0.208402634031067,
-1.11344221708583));
#51329=CARTESIAN_POINT('Ctrl Pts',(-0.321827503055486,0.050804159548938,
-1.10374459224114));
#51330=CARTESIAN_POINT('Ctrl Pts',(-0.321766314000566,4.30053259428721E-5,
-1.10062265507269));
#51331=CARTESIAN_POINT('Origin',(0.,0.,-2.18777734492731));
#51332=CARTESIAN_POINT('',(-0.321766966566369,4.5403904709377E-5,-1.37527734492731));
#51333=CARTESIAN_POINT('',(-0.322385193379531,-0.000275211153700466,-1.35062265507269));
#51334=CARTESIAN_POINT('',(-0.322275,-3.08760083991297E-14,-2.18777734492731));
#51335=CARTESIAN_POINT('Ctrl Pts',(-0.321766966566369,4.54039047093589E-5,
-1.37527734492731));
#51336=CARTESIAN_POINT('Ctrl Pts',(-0.321695297543061,-0.0562622719711204,
-1.37181426633129));
#51337=CARTESIAN_POINT('Ctrl Pts',(-0.280908354535491,-0.21958399720779,
-1.36177550005904));
#51338=CARTESIAN_POINT('Ctrl Pts',(-0.0216513306458494,-0.379529615109383,
-1.34516104611055));
#51339=CARTESIAN_POINT('Ctrl Pts',(0.305776331751614,-0.225859123798109,
-1.32543398308186));
#51340=CARTESIAN_POINT('Ctrl Pts',(0.356390552660915,0.132277295241747,
-1.30570692005317));
#51341=CARTESIAN_POINT('Ctrl Pts',(0.0843712498095106,0.370665618945638,
-1.28597985702447));
#51342=CARTESIAN_POINT('Ctrl Pts',(-0.241942017400318,0.279657158481209,
-1.26750333198252));
#51343=CARTESIAN_POINT('Ctrl Pts',(-0.321639189342704,0.0858750035272477,
-1.2556024946168));
#51344=CARTESIAN_POINT('Ctrl Pts',(-0.322410319385532,-0.000271004193501456,
-1.25027734492731));
#51345=CARTESIAN_POINT('Ctrl Pts',(-0.322385193379531,-0.000275211153700449,
-1.35062265507269));
#51346=CARTESIAN_POINT('Ctrl Pts',(-0.322575125249444,-0.0213606665813696,
-1.34931951102258));
#51347=CARTESIAN_POINT('Ctrl Pts',(-0.311123410622023,-0.148638429323664,
-1.34144067929624));
#51348=CARTESIAN_POINT('Ctrl Pts',(-0.141955604305407,-0.352647262007924,
-1.32698615989367));
#51349=CARTESIAN_POINT('Ctrl Pts',(0.217428857727536,-0.311827158571008,
-1.30725909686498));
#51350=CARTESIAN_POINT('Ctrl Pts',(0.37997915002097,0.0112840836821547,
-1.28753203383628));
#51351=CARTESIAN_POINT('Ctrl Pts',(0.198541614321699,0.324180061659845,
-1.26780497080759));
#51352=CARTESIAN_POINT('Ctrl Pts',(-0.16263183234255,0.343602054860151,
-1.2480779077789));
#51353=CARTESIAN_POINT('Ctrl Pts',(-0.31512516123277,0.135735123126218,
-1.23401713586727));
#51354=CARTESIAN_POINT('Ctrl Pts',(-0.32268282835425,0.0149200405556859,
-1.22653205163186));
#51355=CARTESIAN_POINT('Ctrl Pts',(-0.322565009168808,0.00022687058495755,
-1.22562265507269));
#51356=CARTESIAN_POINT('Origin',(0.,0.,-2.18777734492731));
#51357=CARTESIAN_POINT('',(-0.322568970321137,0.00022527015596577,-1.50027734492731));
#51358=CARTESIAN_POINT('',(-0.321771106026149,5.88663889491414E-5,-1.47562265507269));
#51359=CARTESIAN_POINT('',(-0.322275,-3.08760083991297E-14,-2.18777734492731));
#51360=CARTESIAN_POINT('Ctrl Pts',(-0.322568970321137,0.000225270155965756,
-1.50027734492731));
#51361=CARTESIAN_POINT('Ctrl Pts',(-0.321837345546539,-0.0914731051590046,
-1.49460172572201));
#51362=CARTESIAN_POINT('Ctrl Pts',(-0.233103515511503,-0.290650369905947,
-1.48235041884047));
#51363=CARTESIAN_POINT('Ctrl Pts',(0.103833845766363,-0.365691183090615,
-1.4635234242827));
#51364=CARTESIAN_POINT('Ctrl Pts',(0.362880498319019,-0.113266291538057,
-1.44379636125401));
#51365=CARTESIAN_POINT('Ctrl Pts',(0.293418403901249,0.24169639861178,-1.42406929822532));
#51366=CARTESIAN_POINT('Ctrl Pts',(-0.0416697372088447,0.377855980330849,
-1.40434223519663));
#51367=CARTESIAN_POINT('Ctrl Pts',(-0.286832692350314,0.208096552551141,
-1.38807825076396));
#51368=CARTESIAN_POINT('Ctrl Pts',(-0.321831382561136,0.0506546460448801,
-1.37838995400752));
#51369=CARTESIAN_POINT('Ctrl Pts',(-0.321766966566369,4.54039047093589E-5,
-1.37527734492731));
#51370=CARTESIAN_POINT('Ctrl Pts',(-0.321771106026149,5.88663889491171E-5,
-1.47562265507269));
#51371=CARTESIAN_POINT('Ctrl Pts',(-0.321676704902483,-0.0571022987504526,
-1.4721069704133));
#51372=CARTESIAN_POINT('Ctrl Pts',(-0.279982466127999,-0.221305532991997,
-1.46201559807767));
#51373=CARTESIAN_POINT('Ctrl Pts',(-0.0186399440734759,-0.37968939607062,
-1.44534853806582));
#51374=CARTESIAN_POINT('Ctrl Pts',(0.307558363392102,-0.223426359459979,
-1.42562147503713));
#51375=CARTESIAN_POINT('Ctrl Pts',(0.355329990338077,0.135100270022,-1.40589441200844));
#51376=CARTESIAN_POINT('Ctrl Pts',(0.0814282002323064,0.371323219316239,
-1.38616734897974));
#51377=CARTESIAN_POINT('Ctrl Pts',(-0.243225838729499,0.277995556675306,
-1.36774343000116));
#51378=CARTESIAN_POINT('Ctrl Pts',(-0.321616725710878,0.085036910410772,
-1.35589519869881));
#51379=CARTESIAN_POINT('Ctrl Pts',(-0.322385193379531,-0.000275211153700449,
-1.35062265507269));
#51380=CARTESIAN_POINT('Origin',(0.,0.,-2.18777734492731));
#51381=CARTESIAN_POINT('',(-0.322380752027636,-0.000275883433438568,-1.62527734492731));
#51382=CARTESIAN_POINT('',(-0.322590734421357,0.00021587490590607,-1.60062265507269));
#51383=CARTESIAN_POINT('',(-0.322275,-3.08760083991297E-14,-2.18777734492731));
#51384=CARTESIAN_POINT('Ctrl Pts',(-0.322380752027636,-0.000275883433438602,
-1.62527734492731));
#51385=CARTESIAN_POINT('Ctrl Pts',(-0.322572213417517,-0.0215130334452361,
-1.62396487278895));
#51386=CARTESIAN_POINT('Ctrl Pts',(-0.31102340500336,-0.148944440860085,
-1.61607671297436));
#51387=CARTESIAN_POINT('Ctrl Pts',(-0.141459425625526,-0.352846615539549,
-1.60161286548355));
#51388=CARTESIAN_POINT('Ctrl Pts',(0.217867289073768,-0.311521035102426,
-1.58188580245485));
#51389=CARTESIAN_POINT('Ctrl Pts',(0.379962933199995,0.0118185701951804,
-1.56215873942616));
#51390=CARTESIAN_POINT('Ctrl Pts',(0.198085428729991,0.324459043670616,
-1.54243167639747));
#51391=CARTESIAN_POINT('Ctrl Pts',(-0.163115009928593,0.343372979052334,
-1.52270461336878));
#51392=CARTESIAN_POINT('Ctrl Pts',(-0.315214834387717,0.135429775293384,
-1.50865316954539));
#51393=CARTESIAN_POINT('Ctrl Pts',(-0.322684995087483,0.0147672634558229,
-1.50117741339824));
#51394=CARTESIAN_POINT('Ctrl Pts',(-0.322568970321137,0.000225270155965756,
-1.50027734492731));
#51395=CARTESIAN_POINT('Ctrl Pts',(-0.322590734421357,0.000215874905906053,
-1.60062265507269));
#51396=CARTESIAN_POINT('Ctrl Pts',(-0.321874753260051,-0.0923160744138115,
-1.59489442980401));
#51397=CARTESIAN_POINT('Ctrl Pts',(-0.231733610569791,-0.292288142917499,
-1.58259051685911));
#51398=CARTESIAN_POINT('Ctrl Pts',(0.106731497010161,-0.36485596183739,
-1.56371091623797));
#51399=CARTESIAN_POINT('Ctrl Pts',(0.363767560759545,-0.110384087378192,
-1.54398385320928));
#51400=CARTESIAN_POINT('Ctrl Pts',(0.291491836616472,0.244016380761125,
-1.52425679018059));
#51401=CARTESIAN_POINT('Ctrl Pts',(-0.0446658496794004,0.377513505615764,
-1.50452972715189));
#51402=CARTESIAN_POINT('Ctrl Pts',(-0.287685814152671,0.206369985421987,
-1.4883183487826));
#51403=CARTESIAN_POINT('Ctrl Pts',(-0.321853271450867,0.0498111492921424,
-1.47868265808953));
#51404=CARTESIAN_POINT('Ctrl Pts',(-0.321771106026149,5.88663889491171E-5,
-1.47562265507269));
#51405=CARTESIAN_POINT('Origin',(0.,0.,-2.18777734492731));
#51406=CARTESIAN_POINT('',(-0.321771926585611,6.15374733540274E-5,-1.75027734492731));
#51407=CARTESIAN_POINT('',(-0.32235545627002,-0.000279252447957873,-1.72562265507269));
#51408=CARTESIAN_POINT('',(-0.322275,-3.08760083991297E-14,-2.18777734492731));
#51409=CARTESIAN_POINT('Ctrl Pts',(-0.32177192658561,6.15374733539953E-5,
-1.75027734492731));
#51410=CARTESIAN_POINT('Ctrl Pts',(-0.321673471884271,-0.0572510717560738,
-1.74675233217967));
#51411=CARTESIAN_POINT('Ctrl Pts',(-0.279817409473859,-0.221611271876293,
-1.7366516317558));
#51412=CARTESIAN_POINT('Ctrl Pts',(-0.0181057689026194,-0.379714901981348,
-1.7199752436557));
#51413=CARTESIAN_POINT('Ctrl Pts',(0.307872328352363,-0.22299372509844,
-1.70024818062701));
#51414=CARTESIAN_POINT('Ctrl Pts',(0.355139649765817,0.135600070284936,
-1.68052111759831));
#51415=CARTESIAN_POINT('Ctrl Pts',(0.0809057973768194,0.371437370479693,
-1.66079405456962));
#51416=CARTESIAN_POINT('Ctrl Pts',(-0.243452347477783,0.277700678203372,
-1.64237946367929));
#51417=CARTESIAN_POINT('Ctrl Pts',(-0.321612962348392,0.084888360938352,
-1.63054056046518));
#51418=CARTESIAN_POINT('Ctrl Pts',(-0.322380752027636,-0.000275883433438602,
-1.62527734492731));
#51419=CARTESIAN_POINT('Ctrl Pts',(-0.32235545627002,-0.000279252447957852,
-1.72562265507269));
#51420=CARTESIAN_POINT('Ctrl Pts',(-0.322555307131201,-0.0223720893850791,
-1.72425757687096));
#51421=CARTESIAN_POINT('Ctrl Pts',(-0.310454657452169,-0.150670362690872,
-1.716316810993));
#51422=CARTESIAN_POINT('Ctrl Pts',(-0.138655911363643,-0.353957599768978,
-1.70180035743881));
#51423=CARTESIAN_POINT('Ctrl Pts',(0.220331617412842,-0.309782948961838,
-1.68207329441012));
#51424=CARTESIAN_POINT('Ctrl Pts',(0.379857197625088,0.0148323499972791,
-1.66234623138143));
#51425=CARTESIAN_POINT('Ctrl Pts',(0.195505333378129,0.326020158763575,
-1.64261916835274));
#51426=CARTESIAN_POINT('Ctrl Pts',(-0.165833745799237,0.342068203520708,
-1.62289210532405));
#51427=CARTESIAN_POINT('Ctrl Pts',(-0.31571597672073,0.133707984795308,
-1.60889326756403));
#51428=CARTESIAN_POINT('Ctrl Pts',(-0.322696660269288,0.0139055160893734,
-1.60147011748025));
#51429=CARTESIAN_POINT('Ctrl Pts',(-0.322590734421357,0.000215874905906053,
-1.60062265507269));
#51430=CARTESIAN_POINT('Origin',(0.,0.,-2.18777734492731));
#51431=CARTESIAN_POINT('',(-0.322590464231506,0.000235348495535938,-1.87527734492731));
#51432=CARTESIAN_POINT('',(-0.321776643047528,7.65958109301412E-5,-1.85062265507269));
#51433=CARTESIAN_POINT('',(-0.322275,-3.08760083991297E-14,-2.18777734492731));
#51434=CARTESIAN_POINT('Ctrl Pts',(-0.322590464231506,0.000235348495535932,
-1.87527734492731));
#51435=CARTESIAN_POINT('Ctrl Pts',(-0.321876848463517,-0.092440732628234,
-1.86953979157039));
#51436=CARTESIAN_POINT('Ctrl Pts',(-0.231495856970855,-0.292611071270677,
-1.85722655053723));
#51437=CARTESIAN_POINT('Ctrl Pts',(0.107248148204929,-0.364687178636194,
-1.83833762182785));
#51438=CARTESIAN_POINT('Ctrl Pts',(0.363920662047043,-0.109881854276511,
-1.81861055879916));
#51439=CARTESIAN_POINT('Ctrl Pts',(0.291149288473172,0.244431170965113,
-1.79888349577046));
#51440=CARTESIAN_POINT('Ctrl Pts',(-0.0451973364463865,0.377447732614952,
-1.77915643274177));
#51441=CARTESIAN_POINT('Ctrl Pts',(-0.287836020952351,0.206064450530742,
-1.76295438246072));
#51442=CARTESIAN_POINT('Ctrl Pts',(-0.321857132884277,0.0496619652123383,
-1.7533280198559));
#51443=CARTESIAN_POINT('Ctrl Pts',(-0.32177192658561,6.15374733539953E-5,
-1.75027734492731));
#51444=CARTESIAN_POINT('Ctrl Pts',(-0.321776643047528,7.65958109301274E-5,
-1.85062265507269));
#51445=CARTESIAN_POINT('Ctrl Pts',(-0.321655231279037,-0.0580897489734325,
-1.84704503626168));
#51446=CARTESIAN_POINT('Ctrl Pts',(-0.27888134199293,-0.223334951199449,
-1.83689172977444));
#51447=CARTESIAN_POINT('Ctrl Pts',(-0.0150921858664401,-0.37984442379687,
-1.82016273561096));
#51448=CARTESIAN_POINT('Ctrl Pts',(0.309631125843552,-0.220545534491785,
-1.80043567258228));
#51449=CARTESIAN_POINT('Ctrl Pts',(0.354052996640771,0.138413596659764,
-1.78070860955358));
#51450=CARTESIAN_POINT('Ctrl Pts',(0.0779566158343278,0.372067153582978,
-1.76098154652489));
#51451=CARTESIAN_POINT('Ctrl Pts',(-0.244723080491218,0.276035928694378,
-1.74261956169792));
#51452=CARTESIAN_POINT('Ctrl Pts',(-0.321592610017374,0.084050821329131,
-1.73083326454719));
#51453=CARTESIAN_POINT('Ctrl Pts',(-0.32235545627002,-0.000279252447957852,
-1.72562265507269));
#51454=CARTESIAN_POINT('Origin',(5.160062080289E-17,2.1385152528819E-17,
-0.0249999999999999));
#51455=CARTESIAN_POINT('',(-0.268747084003623,-0.287158309717044,-0.0249999999999999));
#51456=CARTESIAN_POINT('Ctrl Pts',(-0.104132061245197,0.305520369126829,
-0.0249999999999997));
#51457=CARTESIAN_POINT('Ctrl Pts',(-0.112382861583866,0.303711558952992,
-0.0249999999999997));
#51458=CARTESIAN_POINT('Ctrl Pts',(-0.12054122005697,0.301562047182125,
-0.0249999999999994));
#51459=CARTESIAN_POINT('Ctrl Pts',(-0.128586133842392,0.299069778023146,
-0.0249999999999996));
#51460=CARTESIAN_POINT('Ctrl Pts',(-0.143668026017499,0.294397492436297,
-0.0249999999999999));
#51461=CARTESIAN_POINT('Ctrl Pts',(-0.158351562516306,0.28852241268013,
-0.0250000000000008));
#51462=CARTESIAN_POINT('Ctrl Pts',(-0.172564002552817,0.281564854373729,
-0.0250000000000009));
#51463=CARTESIAN_POINT('Ctrl Pts',(-0.17986959675151,0.277988473578474,
-0.025000000000001));
#51464=CARTESIAN_POINT('Ctrl Pts',(-0.187054604234899,0.274122843885494,
-0.0250000000000012));
#51465=CARTESIAN_POINT('Ctrl Pts',(-0.194083144462788,0.269997831741318,
-0.0250000000000011));
#51466=CARTESIAN_POINT('Ctrl Pts',(-0.207302501963761,0.262239462512193,
-0.025000000000001));
#51467=CARTESIAN_POINT('Ctrl Pts',(-0.219985327166613,0.253558036789537,
-0.0250000000000006));
#51468=CARTESIAN_POINT('Ctrl Pts',(-0.232067036805025,0.24405627624154,
-0.0250000000000008));
#51469=CARTESIAN_POINT('Ctrl Pts',(-0.239195615380843,0.238449946615834,
-0.0250000000000009));
#51470=CARTESIAN_POINT('Ctrl Pts',(-0.246114852768324,0.232557607409542,
-0.0250000000000013));
#51471=CARTESIAN_POINT('Ctrl Pts',(-0.252810300802026,0.226397178208491,
-0.0250000000000013));
#51472=CARTESIAN_POINT('Ctrl Pts',(-0.257040953740688,0.222504587634768,
-0.0250000000000012));
#51473=CARTESIAN_POINT('Ctrl Pts',(-0.261176314178513,0.218510243733399,
-0.0250000000000011));
#51474=CARTESIAN_POINT('Ctrl Pts',(-0.26520952408131,0.21442325237044,-0.025000000000001));
#51475=CARTESIAN_POINT('Ctrl Pts',(-0.279321174873982,0.200123427591488,
-0.025000000000001));
#51476=CARTESIAN_POINT('Ctrl Pts',(-0.292199058467302,0.184679362555137,
-0.0250000000000009));
#51477=CARTESIAN_POINT('Ctrl Pts',(-0.303703189948864,0.168295762170721,
-0.0250000000000008));
#51478=CARTESIAN_POINT('Ctrl Pts',(-0.311111775688651,0.15774483024084,
-0.0250000000000008));
#51479=CARTESIAN_POINT('Ctrl Pts',(-0.317950298791598,0.146803153286562,
-0.0250000000000007));
#51480=CARTESIAN_POINT('Ctrl Pts',(-0.324174543496671,0.135516327909584,
-0.0250000000000006));
#51481=CARTESIAN_POINT('Ctrl Pts',(-0.32697171144007,0.130444042415813,
-0.0250000000000005));
#51482=CARTESIAN_POINT('Ctrl Pts',(-0.329644730323056,0.125301970959981,
-0.0250000000000003));
#51483=CARTESIAN_POINT('Ctrl Pts',(-0.332189090490657,0.120093907801464,
-0.0250000000000003));
#51484=CARTESIAN_POINT('Ctrl Pts',(-0.33440192208225,0.115564452091959,
-0.0250000000000003));
#51485=CARTESIAN_POINT('Ctrl Pts',(-0.336515604770219,0.110988494106281,
-0.0250000000000002));
#51486=CARTESIAN_POINT('Ctrl Pts',(-0.338523889172115,0.10637780910622,
-0.0250000000000002));
#51487=CARTESIAN_POINT('Ctrl Pts',(-0.344841785747123,0.0918729755563301,
-0.0250000000000004));
#51488=CARTESIAN_POINT('Ctrl Pts',(-0.350129984567197,0.0770003032114229,
-0.0249999999999999));
#51489=CARTESIAN_POINT('Ctrl Pts',(-0.354318642179587,0.0618495857195709,
-0.0250000000000001));
#51490=CARTESIAN_POINT('Ctrl Pts',(-0.358443070227919,0.0469311918191192,
-0.0250000000000002));
#51491=CARTESIAN_POINT('Ctrl Pts',(-0.361501838911406,0.0317428915652387,
-0.0250000000000007));
#51492=CARTESIAN_POINT('Ctrl Pts',(-0.363538379759458,0.0163776637643565,
-0.025000000000001));
#51493=CARTESIAN_POINT('Ctrl Pts',(-0.364528551563602,0.00890704742624304,
-0.0250000000000011));
#51494=CARTESIAN_POINT('Ctrl Pts',(-0.365276802527859,0.00139448624501336,
-0.0250000000000007));
#51495=CARTESIAN_POINT('Ctrl Pts',(-0.365786589585033,-0.00614981576697971,
-0.0250000000000008));
#51496=CARTESIAN_POINT('Ctrl Pts',(-0.3662576514167,-0.0131210259505516,
-0.0250000000000008));
#51497=CARTESIAN_POINT('Ctrl Pts',(-0.366524835382005,-0.0201241583178749,
-0.0250000000000003));
#51498=CARTESIAN_POINT('Ctrl Pts',(-0.366590738824205,-0.0271210817527391,
-0.0250000000000003));
#51499=CARTESIAN_POINT('Ctrl Pts',(-0.366785036131083,-0.0477494940852813,
-0.0250000000000004));
#51500=CARTESIAN_POINT('Ctrl Pts',(-0.365238886576527,-0.0683667701686375,
-0.025000000000001));
#51501=CARTESIAN_POINT('Ctrl Pts',(-0.36205686275022,-0.0887617369955776,
-0.025000000000001));
#51502=CARTESIAN_POINT('Ctrl Pts',(-0.359210072782657,-0.107008045043846,
-0.0250000000000011));
#51503=CARTESIAN_POINT('Ctrl Pts',(-0.355053174048432,-0.125077451846666,
-0.0250000000000003));
#51504=CARTESIAN_POINT('Ctrl Pts',(-0.34962800436616,-0.142823830653435,
-0.0250000000000004));
#51505=CARTESIAN_POINT('Ctrl Pts',(-0.348118456848888,-0.147761741103659,
-0.0250000000000004));
#51506=CARTESIAN_POINT('Ctrl Pts',(-0.346510536019648,-0.152674628656446,
-0.0250000000000007));
#51507=CARTESIAN_POINT('Ctrl Pts',(-0.344804729560613,-0.157559276549724,
-0.0250000000000007));
#51508=CARTESIAN_POINT('Ctrl Pts',(-0.342956790976082,-0.162850925708409,
-0.0250000000000007));
#51509=CARTESIAN_POINT('Ctrl Pts',(-0.340996925380781,-0.168100787300376,
-0.0250000000000002));
#51510=CARTESIAN_POINT('Ctrl Pts',(-0.33892857690435,-0.173300715737075,
-0.0250000000000002));
#51511=CARTESIAN_POINT('Ctrl Pts',(-0.330624815413151,-0.194176775067354,
-0.0250000000000002));
#51512=CARTESIAN_POINT('Ctrl Pts',(-0.320569495551667,-0.214270328721061,
-0.0250000000000002));
#51513=CARTESIAN_POINT('Ctrl Pts',(-0.30885225511758,-0.233331936432522,
-0.0250000000000001));
#51514=CARTESIAN_POINT('Ctrl Pts',(-0.297135014683494,-0.252393544143984,
-0.025));
#51515=CARTESIAN_POINT('Ctrl Pts',(-0.283755567106122,-0.270425122759551,
-0.0249999999999999));
#51516=CARTESIAN_POINT('Ctrl Pts',(-0.268747084003623,-0.287158309717044,
-0.0249999999999999));
#51517=CARTESIAN_POINT('',(-0.3933,-4.81653586104654E-17,-0.025));
#51518=CARTESIAN_POINT('Origin',(0.,0.,-0.025));
#51519=CARTESIAN_POINT('',(0.0664872943522231,-0.388263316286114,-0.0249999999999998));
#51520=CARTESIAN_POINT('Origin',(0.,0.,-0.025));
#51521=CARTESIAN_POINT('Ctrl Pts',(0.0664872943522175,-0.388263316286115,
-0.0250000000000001));
#51522=CARTESIAN_POINT('Ctrl Pts',(0.0763674397481634,-0.385721382737377,
-0.0250000000000001));
#51523=CARTESIAN_POINT('Ctrl Pts',(0.0861252300852847,-0.382774239928317,
-0.0250000000000006));
#51524=CARTESIAN_POINT('Ctrl Pts',(0.0957372764438226,-0.379413846983949,
-0.0250000000000004));
#51525=CARTESIAN_POINT('Ctrl Pts',(0.110536106803841,-0.374240142730792,
-0.0250000000000001));
#51526=CARTESIAN_POINT('Ctrl Pts',(0.124989950584507,-0.368087330733362,
-0.025));
#51527=CARTESIAN_POINT('Ctrl Pts',(0.139034449099689,-0.361026667091296,
-0.0249999999999998));
#51528=CARTESIAN_POINT('Ctrl Pts',(0.145280104385201,-0.357886756389064,
-0.0249999999999998));
#51529=CARTESIAN_POINT('Ctrl Pts',(0.151444690667498,-0.35456715588149,
-0.0249999999999999));
#51530=CARTESIAN_POINT('Ctrl Pts',(0.157521916343542,-0.35107350179203,
-0.0249999999999999));
#51531=CARTESIAN_POINT('Ctrl Pts',(0.163617093981208,-0.347569527542108,
-0.0249999999999999));
#51532=CARTESIAN_POINT('Ctrl Pts',(0.169617845149672,-0.343894082667936,
-0.0249999999999997));
#51533=CARTESIAN_POINT('Ctrl Pts',(0.175512137101354,-0.340057896274778,
-0.0249999999999997));
#51534=CARTESIAN_POINT('Ctrl Pts',(0.193576222159083,-0.328301234427794,
-0.0249999999999996));
#51535=CARTESIAN_POINT('Ctrl Pts',(0.210662951284164,-0.315026093188845,
-0.0249999999999999));
#51536=CARTESIAN_POINT('Ctrl Pts',(0.226591694629148,-0.30040837774134,
-0.0249999999999998));
#51537=CARTESIAN_POINT('Ctrl Pts',(0.230914684688862,-0.296441194818828,
-0.0249999999999998));
#51538=CARTESIAN_POINT('Ctrl Pts',(0.235153530321517,-0.292373552875338,
-0.0249999999999999));
#51539=CARTESIAN_POINT('Ctrl Pts',(0.239299599657318,-0.288213122078874,
-0.0249999999999999));
#51540=CARTESIAN_POINT('Ctrl Pts',(0.254163153237533,-0.273298083025847,
-0.0249999999999999));
#51541=CARTESIAN_POINT('Ctrl Pts',(0.267772763215115,-0.257259583514981,
-0.025));
#51542=CARTESIAN_POINT('Ctrl Pts',(0.27996909329752,-0.240266943756375,
-0.0249999999999999));
#51543=CARTESIAN_POINT('Ctrl Pts',(0.291835834713897,-0.223733506186666,
-0.0249999999999999));
#51544=CARTESIAN_POINT('Ctrl Pts',(0.302365270717635,-0.206295554373272,
-0.0249999999999997));
#51545=CARTESIAN_POINT('Ctrl Pts',(0.311365267785366,-0.188092496425583,
-0.0249999999999994));
#51546=CARTESIAN_POINT('Ctrl Pts',(0.313924553682842,-0.182916180350604,
-0.0249999999999994));
#51547=CARTESIAN_POINT('Ctrl Pts',(0.316359844881218,-0.177677952152454,
-0.025));
#51548=CARTESIAN_POINT('Ctrl Pts',(0.318665922757951,-0.172380970932363,
-0.025));
#51549=CARTESIAN_POINT('Ctrl Pts',(0.320708024180543,-0.167690334508447,
-0.025));
#51550=CARTESIAN_POINT('Ctrl Pts',(0.322644714126049,-0.16296297370313,
-0.025));
#51551=CARTESIAN_POINT('Ctrl Pts',(0.324473225180541,-0.15820205171735,
-0.0249999999999999));
#51552=CARTESIAN_POINT('Ctrl Pts',(0.329742881883041,-0.144481366578025,
-0.0249999999999999));
#51553=CARTESIAN_POINT('Ctrl Pts',(0.334116071089045,-0.130480116961365,
-0.0249999999999995));
#51554=CARTESIAN_POINT('Ctrl Pts',(0.33752407445594,-0.116254171752792,
-0.0249999999999995));
#51555=CARTESIAN_POINT('Ctrl Pts',(0.341948241078035,-0.0977864810894237,
-0.0249999999999996));
#51556=CARTESIAN_POINT('Ctrl Pts',(0.344746961684114,-0.0789392408706085,
-0.025));
#51557=CARTESIAN_POINT('Ctrl Pts',(0.345959731177688,-0.0599047281750491,
-0.025));
#51558=CARTESIAN_POINT('Ctrl Pts',(0.346400164826157,-0.052992087382431,
-0.025));
#51559=CARTESIAN_POINT('Ctrl Pts',(0.346631052578019,-0.0460548358467735,
-0.0249999999999997));
#51560=CARTESIAN_POINT('Ctrl Pts',(0.34665305150596,-0.0391026545023186,
-0.0249999999999997));
#51561=CARTESIAN_POINT('Ctrl Pts',(0.346668273612427,-0.0342921089662239,
-0.0249999999999997));
#51562=CARTESIAN_POINT('Ctrl Pts',(0.346583436030999,-0.0294839208695866,
-0.0249999999999996));
#51563=CARTESIAN_POINT('Ctrl Pts',(0.346399784667637,-0.024681649273416,
-0.0249999999999996));
#51564=CARTESIAN_POINT('Ctrl Pts',(0.34561706202097,-0.00421435371424099,
-0.0249999999999996));
#51565=CARTESIAN_POINT('Ctrl Pts',(0.343043935277294,0.0161498773801879,
-0.0250000000000001));
#51566=CARTESIAN_POINT('Ctrl Pts',(0.338740270637847,0.0361681817656505,
-0.0250000000000001));
#51567=CARTESIAN_POINT('Ctrl Pts',(0.33524286737294,0.0524361972782629,
-0.0250000000000002));
#51568=CARTESIAN_POINT('Ctrl Pts',(0.330601279695819,0.0684760729038806,
-0.0249999999999997));
#51569=CARTESIAN_POINT('Ctrl Pts',(0.324822539663527,0.0841424234540789,
-0.0249999999999998));
#51570=CARTESIAN_POINT('Ctrl Pts',(0.322815809216327,0.0895827343990095,
-0.0249999999999998));
#51571=CARTESIAN_POINT('Ctrl Pts',(0.320670868222856,0.0949792610338929,
-0.0249999999999995));
#51572=CARTESIAN_POINT('Ctrl Pts',(0.318396443334708,0.100306333711764,
-0.0249999999999996));
#51573=CARTESIAN_POINT('Ctrl Pts',(0.310719203745818,0.118287676366146,
-0.0249999999999997));
#51574=CARTESIAN_POINT('Ctrl Pts',(0.301552401900112,0.135532171812037,
-0.0249999999999999));
#51575=CARTESIAN_POINT('Ctrl Pts',(0.290927725018398,0.151813099285338,
-0.025));
#51576=CARTESIAN_POINT('Ctrl Pts',(0.281011201280672,0.167008874701251,
-0.025));
#51577=CARTESIAN_POINT('Ctrl Pts',(0.269823771969094,0.181365979603481,
-0.0249999999999998));
#51578=CARTESIAN_POINT('Ctrl Pts',(0.257360178851843,0.194662425271939,
-0.0249999999999996));
#51579=CARTESIAN_POINT('Ctrl Pts',(0.256470135840318,0.195611943475398,
-0.0249999999999996));
#51580=CARTESIAN_POINT('Ctrl Pts',(0.255573574088629,0.196556033243165,
-0.0249999999999999));
#51581=CARTESIAN_POINT('Ctrl Pts',(0.254670486854674,0.19749460435719,-0.0249999999999999));
#51582=CARTESIAN_POINT('Ctrl Pts',(-0.143290239521314,0.288667772504872,
-1.99770630286919));
#51583=CARTESIAN_POINT('Ctrl Pts',(-0.238703631141289,0.241306033367412,
-1.99113061519296));
#51584=CARTESIAN_POINT('Ctrl Pts',(-0.377312127630152,0.0454238067759526,
-1.9779792398405));
#51585=CARTESIAN_POINT('Ctrl Pts',(-0.244303043357189,-0.291566061927666,
-1.95825217681181));
#51586=CARTESIAN_POINT('Ctrl Pts',(0.110179288406698,-0.36371910581051,
-1.93852511378312));
#51587=CARTESIAN_POINT('Ctrl Pts',(0.364759182106444,-0.107046497669421,
-1.91879805075442));
#51588=CARTESIAN_POINT('Ctrl Pts',(0.289212400745945,0.246761743044216,
-1.89907098772573));
#51589=CARTESIAN_POINT('Ctrl Pts',(-0.0481959974222359,0.377062323270783,
-1.87934392469704));
#51590=CARTESIAN_POINT('Ctrl Pts',(-0.341950950802492,0.166077696107313,
-1.85961686166835));
#51591=CARTESIAN_POINT('Ctrl Pts',(-0.326156034555877,-0.195286272819796,
-1.83988979863966));
#51592=CARTESIAN_POINT('Ctrl Pts',(-0.0150921858664401,-0.37984442379687,
-1.82016273561096));
#51593=CARTESIAN_POINT('Ctrl Pts',(0.309631125843552,-0.220545534491785,
-1.80043567258228));
#51594=CARTESIAN_POINT('Ctrl Pts',(0.354052996640771,0.138413596659764,
-1.78070860955358));
#51595=CARTESIAN_POINT('Ctrl Pts',(0.0779566158343278,0.372067153582978,
-1.76098154652489));
#51596=CARTESIAN_POINT('Ctrl Pts',(-0.268711937019807,0.268896715095413,
-1.7412544834962));
#51597=CARTESIAN_POINT('Ctrl Pts',(-0.372120970834768,-0.077701410624822,
-1.72152742046751));
#51598=CARTESIAN_POINT('Ctrl Pts',(-0.138655911363643,-0.353957599768978,
-1.70180035743881));
#51599=CARTESIAN_POINT('Ctrl Pts',(0.220331617412842,-0.309782948961838,
-1.68207329441012));
#51600=CARTESIAN_POINT('Ctrl Pts',(0.379857197625088,0.0148323499972791,
-1.66234623138143));
#51601=CARTESIAN_POINT('Ctrl Pts',(0.195505333378129,0.326020158763575,
-1.64261916835274));
#51602=CARTESIAN_POINT('Ctrl Pts',(-0.165833745799237,0.342068203520708,
-1.62289210532405));
#51603=CARTESIAN_POINT('Ctrl Pts',(-0.377046724116218,0.0484484589439102,
-1.60316504229535));
#51604=CARTESIAN_POINT('Ctrl Pts',(-0.246926540796393,-0.289030738284479,
-1.58343797926666));
#51605=CARTESIAN_POINT('Ctrl Pts',(0.106731497010161,-0.36485596183739,
-1.56371091623797));
#51606=CARTESIAN_POINT('Ctrl Pts',(0.363767560759545,-0.110384087378192,
-1.54398385320928));
#51607=CARTESIAN_POINT('Ctrl Pts',(0.291491836616472,0.244016380761125,
-1.52425679018059));
#51608=CARTESIAN_POINT('Ctrl Pts',(-0.0446658496794004,0.377513505615764,
-1.50452972715189));
#51609=CARTESIAN_POINT('Ctrl Pts',(-0.340388400050172,0.169254902744056,
-1.48480266412321));
#51610=CARTESIAN_POINT('Ctrl Pts',(-0.327963868087676,-0.192226913337763,
-1.46507560109451));
#51611=CARTESIAN_POINT('Ctrl Pts',(-0.0186399440734759,-0.37968939607062,
-1.44534853806582));
#51612=CARTESIAN_POINT('Ctrl Pts',(0.307558363392102,-0.223426359459979,
-1.42562147503713));
#51613=CARTESIAN_POINT('Ctrl Pts',(0.355329990338077,0.135100270022,-1.40589441200844));
#51614=CARTESIAN_POINT('Ctrl Pts',(0.0814282002323064,0.371323219316239,
-1.38616734897974));
#51615=CARTESIAN_POINT('Ctrl Pts',(-0.266188975926808,0.271394388464428,
-1.36644028595105));
#51616=CARTESIAN_POINT('Ctrl Pts',(-0.372830383652258,-0.0742225708309672,
-1.34671322292236));
#51617=CARTESIAN_POINT('Ctrl Pts',(-0.141955604305407,-0.352647262007924,
-1.32698615989367));
#51618=CARTESIAN_POINT('Ctrl Pts',(0.217428857727536,-0.311827158571008,
-1.30725909686498));
#51619=CARTESIAN_POINT('Ctrl Pts',(0.37997915002097,0.0112840836821547,
-1.28753203383628));
#51620=CARTESIAN_POINT('Ctrl Pts',(0.198541614321699,0.324180061659845,
-1.26780497080759));
#51621=CARTESIAN_POINT('Ctrl Pts',(-0.16263183234255,0.343602054860151,
-1.2480779077789));
#51622=CARTESIAN_POINT('Ctrl Pts',(-0.376577804112661,0.0519677057883744,
-1.22835084475021));
#51623=CARTESIAN_POINT('Ctrl Pts',(-0.249615121026705,-0.286712009427665,
-1.20862378172152));
#51624=CARTESIAN_POINT('Ctrl Pts',(0.103319337909045,-0.365836848074736,
-1.18889671869282));
#51625=CARTESIAN_POINT('Ctrl Pts',(0.362720784217591,-0.113776613114465,
-1.16916965566413));
#51626=CARTESIAN_POINT('Ctrl Pts',(0.293758069692678,0.241283404911434,
-1.14944259263544));
#51627=CARTESIAN_POINT('Ctrl Pts',(-0.0411381844576584,0.377914189697542,
-1.12971552960675));
#51628=CARTESIAN_POINT('Ctrl Pts',(-0.338792830171386,0.172426515419424,
-1.10998846657806));
#51629=CARTESIAN_POINT('Ctrl Pts',(-0.329744832374935,-0.189155572260636,
-1.09026140354936));
#51630=CARTESIAN_POINT('Ctrl Pts',(-0.022185169729932,-0.379498752618868,
-1.07053434052067));
#51631=CARTESIAN_POINT('Ctrl Pts',(0.305458301062517,-0.226288999527647,
-1.05080727749198));
#51632=CARTESIAN_POINT('Ctrl Pts',(0.356576237443244,0.131775839538367,
-1.03108021446329));
#51633=CARTESIAN_POINT('Ctrl Pts',(0.0848925531951284,0.370546541485998,
-1.0113531514346));
#51634=CARTESIAN_POINT('Ctrl Pts',(-0.263642729317636,0.273868574818599,
-0.991626088405904));
#51635=CARTESIAN_POINT('Ctrl Pts',(-0.373507311558931,-0.0707373536912577,
-0.971899025377214));
#51636=CARTESIAN_POINT('Ctrl Pts',(-0.145242896892136,-0.351306114233161,
-0.952171962348521));
#51637=CARTESIAN_POINT('Ctrl Pts',(0.214507123315248,-0.313844195489162,
-0.932444899319828));
#51638=CARTESIAN_POINT('Ctrl Pts',(0.380067963842326,0.00773484686148907,
-0.912717836291137));
#51639=CARTESIAN_POINT('Ctrl Pts',(0.20156057492959,0.322311680876253,-0.892990773262445));
#51640=CARTESIAN_POINT('Ctrl Pts',(-0.159415732015043,0.345105939359686,
-0.873263710233753));
#51641=CARTESIAN_POINT('Ctrl Pts',(-0.376076037935125,0.0554824178117764,
-0.853536647205062));
#51642=CARTESIAN_POINT('Ctrl Pts',(-0.252281928284525,-0.284368271184151,
-0.833809584176369));
#51643=CARTESIAN_POINT('Ctrl Pts',(0.0998981666172007,-0.366785824837531,
-0.814082521147678));
#51644=CARTESIAN_POINT('Ctrl Pts',(0.361642369567447,-0.117159214442841,
-0.794355458118984));
#51645=CARTESIAN_POINT('Ctrl Pts',(0.295998679758828,0.238529383045872,
-0.774628395090294));
#51646=CARTESIAN_POINT('Ctrl Pts',(-0.0376069309429452,0.37828191040585,
-0.754901332061601));
#51647=CARTESIAN_POINT('Ctrl Pts',(-0.337167709206362,0.175583088205384,
-0.73517426903291));
#51648=CARTESIAN_POINT('Ctrl Pts',(-0.331497034762949,-0.186067732126079,
-0.715447206004218));
#51649=CARTESIAN_POINT('Ctrl Pts',(-0.0257284602956936,-0.379275007515933,
-0.695720142975526));
#51650=CARTESIAN_POINT('Ctrl Pts',(0.303331595228502,-0.22913190160076,
-0.675993079946833));
#51651=CARTESIAN_POINT('Ctrl Pts',(0.357791382294441,0.128439914943824,
-0.656266016918142));
#51652=CARTESIAN_POINT('Ctrl Pts',(0.0883495014317826,0.369737542850607,
-0.63653895388945));
#51653=CARTESIAN_POINT('Ctrl Pts',(-0.261073486552964,0.276318873066526,
-0.616811890860758));
#51654=CARTESIAN_POINT('Ctrl Pts',(-0.374151660404283,-0.0672459665012387,
-0.597084827832066));
#51655=CARTESIAN_POINT('Ctrl Pts',(-0.148517520713027,-0.349934323902057,
-0.577357764803375));
#51656=CARTESIAN_POINT('Ctrl Pts',(0.211566678587274,-0.315833857421815,
-0.557630701774681));
#51657=CARTESIAN_POINT('Ctrl Pts',(0.380123626347935,0.00418493532934027,
-0.537903638745991));
#51658=CARTESIAN_POINT('Ctrl Pts',(0.204561954486446,0.320415186635358,
-0.518176575717298));
#51659=CARTESIAN_POINT('Ctrl Pts',(-0.156185726714996,0.346579721946209,
-0.498449512688607));
#51660=CARTESIAN_POINT('Ctrl Pts',(-0.375541468610517,0.0589922906922721,
-0.478722449659914));
#51661=CARTESIAN_POINT('Ctrl Pts',(-0.254926730386367,-0.281999729568725,
-0.458995386631223));
#51662=CARTESIAN_POINT('Ctrl Pts',(0.096468281849101,-0.367702807740199,
-0.43926832360253));
#51663=CARTESIAN_POINT('Ctrl Pts',(0.360532410560641,-0.120531598662528,
-0.419541260573839));
#51664=CARTESIAN_POINT('Ctrl Pts',(0.298213471837286,0.235754559490252,
-0.399814197545147));
#51665=CARTESIAN_POINT('Ctrl Pts',(-0.0340723979536573,0.378616627998834,
-0.380087134516455));
#51666=CARTESIAN_POINT('Ctrl Pts',(-0.335513177399885,0.178724360357116,
-0.360360071487763));
#51667=CARTESIAN_POINT('Ctrl Pts',(-0.333220325281847,-0.182963690163682,
-0.340633008459071));
#51668=CARTESIAN_POINT('Ctrl Pts',(-0.029269501228293,-0.379018126859581,
-0.320905945430379));
#51669=CARTESIAN_POINT('Ctrl Pts',(0.301178420896456,-0.231954920047871,
-0.301178882401687));
#51670=CARTESIAN_POINT('Ctrl Pts',(0.358975339007382,0.125092983298727,
-0.281451819372995));
#51671=CARTESIAN_POINT('Ctrl Pts',(0.0917987048867537,0.368895918259873,
-0.261724756344303));
#51672=CARTESIAN_POINT('Ctrl Pts',(-0.258481397918661,0.278745789386344,
-0.241997693315611));
#51673=CARTESIAN_POINT('Ctrl Pts',(-0.374763515422673,-0.0637500932034806,
-0.222270630286919));
#51674=CARTESIAN_POINT('Ctrl Pts',(-0.151778919131785,-0.348529367587568,
-0.202543567258227));
#51675=CARTESIAN_POINT('Ctrl Pts',(0.208607260742278,-0.317801035232212,
-0.182816504229535));
#51676=CARTESIAN_POINT('Ctrl Pts',(0.380147127696309,0.000644362698709406,
-0.163089441200843));
#51677=CARTESIAN_POINT('Ctrl Pts',(0.207543584467282,0.318472150029413,
-0.143362378172152));
#51678=CARTESIAN_POINT('Ctrl Pts',(-0.152938443007933,0.348058907694893,
-0.12363531514346));
#51679=CARTESIAN_POINT('Ctrl Pts',(-0.374981161716835,0.0624286949386616,
-0.103908252114768));
#51680=CARTESIAN_POINT('Ctrl Pts',(-0.257535709165863,-0.279475261928206,
-0.084181189086076));
#51681=CARTESIAN_POINT('Ctrl Pts',(0.0930026936990432,-0.368843116278878,
-0.0644541260573834));
#51682=CARTESIAN_POINT('Ctrl Pts',(0.359454556187757,-0.123370117592038,
-0.0447270630286919));
#51683=CARTESIAN_POINT('Ctrl Pts',(0.319948400855436,0.113318339423062,
-0.0315756876762305));
#51684=CARTESIAN_POINT('Ctrl Pts',(0.254670486854674,0.19749460435719,-0.0249999999999999));
#51685=CARTESIAN_POINT('Ctrl Pts',(-0.15381664219191,0.309873914818279,
-1.98403753524613));
#51686=CARTESIAN_POINT('Ctrl Pts',(-0.256239302438379,0.25903288261099,
-1.9774618475699));
#51687=CARTESIAN_POINT('Ctrl Pts',(-0.405030270897994,0.0487607352544926,
-1.96431047221744));
#51688=CARTESIAN_POINT('Ctrl Pts',(-0.262250059264355,-0.312985118683967,
-1.94458340918874));
#51689=CARTESIAN_POINT('Ctrl Pts',(0.118273290898445,-0.390438677077484,
-1.92485634616005));
#51690=CARTESIAN_POINT('Ctrl Pts',(0.391555159567835,-0.114910358758007,
-1.90512928313136));
#51691=CARTESIAN_POINT('Ctrl Pts',(0.310458552596572,0.264889380206798,
-1.88540222010267));
#51692=CARTESIAN_POINT('Ctrl Pts',(-0.0517365768620641,0.404762115384463,
-1.86567515707398));
#51693=CARTESIAN_POINT('Ctrl Pts',(-0.367071387573103,0.178278113314174,
-1.84594809404529));
#51694=CARTESIAN_POINT('Ctrl Pts',(-0.35011614352527,-0.209632413566078,
-1.82622103101659));
#51695=CARTESIAN_POINT('Ctrl Pts',(-0.0162008896144463,-0.407748594872476,
-1.8064939679879));
#51696=CARTESIAN_POINT('Ctrl Pts',(0.332377280228303,-0.236747273779951,
-1.78676690495921));
#51697=CARTESIAN_POINT('Ctrl Pts',(0.380062475177643,0.148581750878735,
-1.76703984193052));
#51698=CARTESIAN_POINT('Ctrl Pts',(0.0836834729590768,0.399399990014835,
-1.74731277890183));
#51699=CARTESIAN_POINT('Ctrl Pts',(-0.288452081644563,0.288650433906628,
-1.72758571587313));
#51700=CARTESIAN_POINT('Ctrl Pts',(-0.399457760795247,-0.0834095198375802,
-1.70785865284444));
#51701=CARTESIAN_POINT('Ctrl Pts',(-0.148841866530923,-0.379960070250804,
-1.68813158981575));
#51702=CARTESIAN_POINT('Ctrl Pts',(0.236517641902015,-0.332540256592501,
-1.66840452678706));
#51703=CARTESIAN_POINT('Ctrl Pts',(0.407762307093009,0.0159219656552873,
-1.64867746375837));
#51704=CARTESIAN_POINT('Ctrl Pts',(0.209867566774228,0.349970286011197,
-1.62895040072967));
#51705=CARTESIAN_POINT('Ctrl Pts',(-0.178016241902864,0.367197253922858,
-1.60922333770098));
#51706=CARTESIAN_POINT('Ctrl Pts',(-0.40474537028316,0.0520075847386445,
-1.58949627467229));
#51707=CARTESIAN_POINT('Ctrl Pts',(-0.265066284348811,-0.310263544828221,
-1.5697692116436));
#51708=CARTESIAN_POINT('Ctrl Pts',(0.114572217487129,-0.391659048941573,
-1.5500421486149));
#51709=CARTESIAN_POINT('Ctrl Pts',(0.390490691629088,-0.118493134833562,
-1.53031508558622));
#51710=CARTESIAN_POINT('Ctrl Pts',(0.312905440625146,0.261942337830458,
-1.51058802255752));
#51711=CARTESIAN_POINT('Ctrl Pts',(-0.0479470970338614,0.4052464425344,
-1.49086095952883));
#51712=CARTESIAN_POINT('Ctrl Pts',(-0.365394048552809,0.181688724239568,
-1.47113389650014));
#51713=CARTESIAN_POINT('Ctrl Pts',(-0.352056784314427,-0.206348307095488,
-1.45140683347145));
#51714=CARTESIAN_POINT('Ctrl Pts',(-0.0200092736086255,-0.407582178483068,
-1.43167977044275));
#51715=CARTESIAN_POINT('Ctrl Pts',(0.330152248283289,-0.239839730215439,
-1.41195270741406));
#51716=CARTESIAN_POINT('Ctrl Pts',(0.381433279520466,0.145025020290467,
-1.39222564438537));
#51717=CARTESIAN_POINT('Ctrl Pts',(0.087410087255813,0.398601404770623,
-1.37249858135668));
#51718=CARTESIAN_POINT('Ctrl Pts',(-0.285743778517969,0.291331591619795,
-1.35277151832799));
#51719=CARTESIAN_POINT('Ctrl Pts',(-0.400219288571868,-0.0796751171483121,
-1.3330444552993));
#51720=CARTESIAN_POINT('Ctrl Pts',(-0.152383961863179,-0.378553472319109,
-1.3133173922706));
#51721=CARTESIAN_POINT('Ctrl Pts',(0.233401639378917,-0.334734638143327,
-1.29359032924191));
#51722=CARTESIAN_POINT('Ctrl Pts',(0.407893218368644,0.0121130362263305,
-1.27386326621322));
#51723=CARTESIAN_POINT('Ctrl Pts',(0.213126899308332,0.347995011500187,
-1.25413620318453));
#51724=CARTESIAN_POINT('Ctrl Pts',(-0.174579109142516,0.368843785210984,
-1.23440914015583));
#51725=CARTESIAN_POINT('Ctrl Pts',(-0.404242002428904,0.0557853628655306,
-1.21468207712715));
#51726=CARTESIAN_POINT('Ctrl Pts',(-0.267952373343229,-0.307774477267861,
-1.19495501409845));
#51727=CARTESIAN_POINT('Ctrl Pts',(0.110909393994673,-0.392711993147018,
-1.17522795106976));
#51728=CARTESIAN_POINT('Ctrl Pts',(0.389367016678535,-0.122134882652859,
-1.15550088804106));
#51729=CARTESIAN_POINT('Ctrl Pts',(0.315338155954333,0.259008591820991,
-1.13577382501238));
#51730=CARTESIAN_POINT('Ctrl Pts',(-0.0441602820979793,0.405676561712403,
-1.11604676198368));
#51731=CARTESIAN_POINT('Ctrl Pts',(-0.363681264751502,0.185093330259408,
-1.09631969895499));
#51732=CARTESIAN_POINT('Ctrl Pts',(-0.353968581987773,-0.203051338836603,
-1.0765926359263));
#51733=CARTESIAN_POINT('Ctrl Pts',(-0.023814939005727,-0.40737752996198,
-1.05686557289761));
#51734=CARTESIAN_POINT('Ctrl Pts',(0.327897910953617,-0.242912665849322,
-1.03713850986892));
#51735=CARTESIAN_POINT('Ctrl Pts',(0.382771078561759,0.141456370144433,
-1.01741144684022));
#51736=CARTESIAN_POINT('Ctrl Pts',(0.0911289388809415,0.397767670551799,
-0.997684383811531));
#51737=CARTESIAN_POINT('Ctrl Pts',(-0.28301047927216,0.293987536912559,
-0.977957320782842));
#51738=CARTESIAN_POINT('Ctrl Pts',(-0.400945945027732,-0.0759338686199355,
-0.958230257754147));
#51739=CARTESIAN_POINT('Ctrl Pts',(-0.155912745884214,-0.377113801005234,
-0.938503194725458));
#51740=CARTESIAN_POINT('Ctrl Pts',(0.230265268205443,-0.336899850840047,
-0.918776131696764));
#51741=CARTESIAN_POINT('Ctrl Pts',(0.4079885566403,0.00830306499645114,
-0.899049068668072));
#51742=CARTESIAN_POINT('Ctrl Pts',(0.216367639118431,0.345989375530647,
-0.879322005639381));
#51743=CARTESIAN_POINT('Ctrl Pts',(-0.171126747313949,0.370458148232049,
-0.859594942610688));
#51744=CARTESIAN_POINT('Ctrl Pts',(-0.403703375451576,0.0595582730338527,
-0.839867879581998));
#51745=CARTESIAN_POINT('Ctrl Pts',(-0.270815089876757,-0.305258563078602,
-0.820140816553304));
#51746=CARTESIAN_POINT('Ctrl Pts',(0.107236896256985,-0.393730683740731,
-0.800413753524614));
#51747=CARTESIAN_POINT('Ctrl Pts',(0.388209379417758,-0.125765976996359,
-0.780686690495921));
#51748=CARTESIAN_POINT('Ctrl Pts',(0.317743365953199,0.256052253711019,
-0.76095962746723));
#51749=CARTESIAN_POINT('Ctrl Pts',(-0.0403696152655688,0.406071295958122,
-0.741232564438537));
#51750=CARTESIAN_POINT('Ctrl Pts',(-0.361936758978947,0.188481791527898,
-0.721505501409845));
#51751=CARTESIAN_POINT('Ctrl Pts',(-0.3558495048522,-0.199736659464793,
-0.701778438381154));
#51752=CARTESIAN_POINT('Ctrl Pts',(-0.0276185271562979,-0.407137348072724,
-0.68205137535246));
#51753=CARTESIAN_POINT('Ctrl Pts',(0.325614972831586,-0.245964413494015,
-0.662324312323771));
#51754=CARTESIAN_POINT('Ctrl Pts',(0.384075490512023,0.137875381505904,
-0.642597249295077));
#51755=CARTESIAN_POINT('Ctrl Pts',(0.0948398418131284,0.39689924117343,
-0.622870186266386));
#51756=CARTESIAN_POINT('Ctrl Pts',(-0.280252494524853,0.296617839228501,
-0.603143123237693));
#51757=CARTESIAN_POINT('Ctrl Pts',(-0.40163762909584,-0.0721859967763643,
-0.583416060209001));
#51758=CARTESIAN_POINT('Ctrl Pts',(-0.1594279304652,-0.375641236068315,
-0.563688997180311));
#51759=CARTESIAN_POINT('Ctrl Pts',(0.227108812217102,-0.339035677527198,
-0.543961934151617));
#51760=CARTESIAN_POINT('Ctrl Pts',(0.408048308230761,0.00449236948936304,
-0.524234871122926));
#51761=CARTESIAN_POINT('Ctrl Pts',(0.219589506336472,0.343953560830042,
-0.504507808094233));
#51762=CARTESIAN_POINT('Ctrl Pts',(-0.167659459024287,0.372040197990199,
-0.484780745065542));
#51763=CARTESIAN_POINT('Ctrl Pts',(-0.403129535538929,0.0633259885656422,
-0.46505368203685));
#51764=CARTESIAN_POINT('Ctrl Pts',(-0.273654184709222,-0.30271602340951,
-0.445326619008158));
#51765=CARTESIAN_POINT('Ctrl Pts',(0.10355504493273,-0.394715030137994,
-0.425599555979466));
#51766=CARTESIAN_POINT('Ctrl Pts',(0.387017880485466,-0.129386103660856,
-0.405872492950774));
#51767=CARTESIAN_POINT('Ctrl Pts',(0.320120861320641,0.253073585775043,
-0.386145429922083));
#51768=CARTESIAN_POINT('Ctrl Pts',(-0.0365754280414766,0.406430602610184,
-0.36641836689339));
#51769=CARTESIAN_POINT('Ctrl Pts',(-0.360160681782608,0.191853828145357,
-0.346691303864698));
#51770=CARTESIAN_POINT('Ctrl Pts',(-0.357699391920736,-0.19640458804476,
-0.326964240836007));
#51771=CARTESIAN_POINT('Ctrl Pts',(-0.0314197004109189,-0.406861596422534,
-0.307237177807315));
#51772=CARTESIAN_POINT('Ctrl Pts',(0.323303621779935,-0.248994816819678,
-0.287510114778622));
#51773=CARTESIAN_POINT('Ctrl Pts',(0.385346423177733,0.134282577215712,
-0.267783051749931));
#51774=CARTESIAN_POINT('Ctrl Pts',(0.0985424310156646,0.395995789068351,
-0.248055988721239));
#51775=CARTESIAN_POINT('Ctrl Pts',(-0.277469985602234,0.29922304193067,
-0.228328925692547));
#51776=CARTESIAN_POINT('Ctrl Pts',(-0.402294432272047,-0.0684333092661341,
-0.208601862663855));
#51777=CARTESIAN_POINT('Ctrl Pts',(-0.162928918078169,-0.374133068705046,
-0.188874799635163));
#51778=CARTESIAN_POINT('Ctrl Pts',(0.223931989306618,-0.341147368361133,
-0.169147736606471));
#51779=CARTESIAN_POINT('Ctrl Pts',(0.408073536037664,0.000691698939159734,
-0.149420673577779));
#51780=CARTESIAN_POINT('Ctrl Pts',(0.22279017313306,0.341867784664262,-0.129693610549087));
#51781=CARTESIAN_POINT('Ctrl Pts',(-0.164173623019451,0.373628047838177,
-0.109966547520395));
#51782=CARTESIAN_POINT('Ctrl Pts',(-0.402528067321197,0.0670148383027876,
-0.0902394844917032));
#51783=CARTESIAN_POINT('Ctrl Pts',(-0.276454824562659,-0.300006103061243,
-0.0705124214630116));
#51784=CARTESIAN_POINT('Ctrl Pts',(0.0998348673809113,-0.395939108142667,
-0.050785358434319));
#51785=CARTESIAN_POINT('Ctrl Pts',(0.385860844661094,-0.132433146166989,
-0.0310582954056275));
#51786=CARTESIAN_POINT('Ctrl Pts',(0.343452483983984,0.121642943211257,
-0.0179069200531661));
#51787=CARTESIAN_POINT('Ctrl Pts',(0.273379116988209,0.212002973787509,
-0.0113312323769355));
#51788=CARTESIAN_POINT('Ctrl Pts',(-0.164343044862507,0.331080057131685,
-1.97036876762306));
#51789=CARTESIAN_POINT('Ctrl Pts',(-0.273774973735468,0.276759731854568,
-1.96379307994683));
#51790=CARTESIAN_POINT('Ctrl Pts',(-0.432748414165835,0.0520976637330328,
-1.95064170459437));
#51791=CARTESIAN_POINT('Ctrl Pts',(-0.280197075171522,-0.334404175440268,
-1.93091464156568));
#51792=CARTESIAN_POINT('Ctrl Pts',(0.126367293390191,-0.417158248344458,
-1.91118757853699));
#51793=CARTESIAN_POINT('Ctrl Pts',(0.418351137029226,-0.122774219846594,
-1.8914605155083));
#51794=CARTESIAN_POINT('Ctrl Pts',(0.331704704447198,0.28301701736938,-1.8717334524796));
#51795=CARTESIAN_POINT('Ctrl Pts',(-0.055277156301892,0.432461907498141,
-1.85200638945091));
#51796=CARTESIAN_POINT('Ctrl Pts',(-0.392191824343714,0.190478530521036,
-1.83227932642222));
#51797=CARTESIAN_POINT('Ctrl Pts',(-0.374076252494662,-0.22397855431236,
-1.81255226339353));
#51798=CARTESIAN_POINT('Ctrl Pts',(-0.0173095933624528,-0.435652765948081,
-1.79282520036484));
#51799=CARTESIAN_POINT('Ctrl Pts',(0.355123434613053,-0.252949013068117,
-1.77309813733615));
#51800=CARTESIAN_POINT('Ctrl Pts',(0.406071953714516,0.158749905097707,
-1.75337107430745));
#51801=CARTESIAN_POINT('Ctrl Pts',(0.0894103300838258,0.426732826446693,
-1.73364401127876));
#51802=CARTESIAN_POINT('Ctrl Pts',(-0.30819222626932,0.308404152717844,
-1.71391694825007));
#51803=CARTESIAN_POINT('Ctrl Pts',(-0.426794550755725,-0.0891176290503394,
-1.69418988522138));
#51804=CARTESIAN_POINT('Ctrl Pts',(-0.159027821698202,-0.405962540732628,
-1.67446282219268));
#51805=CARTESIAN_POINT('Ctrl Pts',(0.252703666391189,-0.355297564223164,
-1.65473575916399));
#51806=CARTESIAN_POINT('Ctrl Pts',(0.435667416560929,0.0170115813132962,
-1.6350086961353));
#51807=CARTESIAN_POINT('Ctrl Pts',(0.224229800170327,0.373920413258818,
-1.61528163310661));
#51808=CARTESIAN_POINT('Ctrl Pts',(-0.19019873800649,0.392326304325009,
-1.59555457007792));
#51809=CARTESIAN_POINT('Ctrl Pts',(-0.432444016450103,0.0555667105333784,
-1.57582750704923));
#51810=CARTESIAN_POINT('Ctrl Pts',(-0.283206027901227,-0.331496351371963,
-1.55610044402053));
#51811=CARTESIAN_POINT('Ctrl Pts',(0.122412937964096,-0.418462136045755,
-1.53637338099184));
#51812=CARTESIAN_POINT('Ctrl Pts',(0.417213822498632,-0.126602182288933,
-1.51664631796315));
#51813=CARTESIAN_POINT('Ctrl Pts',(0.33431904463382,0.27986829489979,-1.49691925493446));
#51814=CARTESIAN_POINT('Ctrl Pts',(-0.0512283443883222,0.432979379453035,
-1.47719219190577));
#51815=CARTESIAN_POINT('Ctrl Pts',(-0.390399697055447,0.194122545735081,
-1.45746512887707));
#51816=CARTESIAN_POINT('Ctrl Pts',(-0.376149700541177,-0.220469700853213,
-1.43773806584838));
#51817=CARTESIAN_POINT('Ctrl Pts',(-0.0213786031437756,-0.435474960895517,
-1.41801100281969));
#51818=CARTESIAN_POINT('Ctrl Pts',(0.352746133174477,-0.256253100970898,
-1.398283939791));
#51819=CARTESIAN_POINT('Ctrl Pts',(0.407536568702855,0.154949770558933,
-1.37855687676231));
#51820=CARTESIAN_POINT('Ctrl Pts',(0.0933919742793201,0.425879590225008,
-1.35882981373362));
#51821=CARTESIAN_POINT('Ctrl Pts',(-0.30529858110913,0.311268794775162,
-1.33910275070492));
#51822=CARTESIAN_POINT('Ctrl Pts',(-0.427608193491478,-0.085127663465657,
-1.31937568767623));
#51823=CARTESIAN_POINT('Ctrl Pts',(-0.162812319420953,-0.404459682630294,
-1.29964862464754));
#51824=CARTESIAN_POINT('Ctrl Pts',(0.249374421030298,-0.357642117715646,
-1.27992156161885));
#51825=CARTESIAN_POINT('Ctrl Pts',(0.435807286716317,0.0129419887705061,
-1.26019449859016));
#51826=CARTESIAN_POINT('Ctrl Pts',(0.227712184294964,0.371809961340529,
-1.24046743556146));
#51827=CARTESIAN_POINT('Ctrl Pts',(-0.186526385942482,0.394085515561816,
-1.22074037253277));
#51828=CARTESIAN_POINT('Ctrl Pts',(-0.431906200745147,0.0596030199426871,
-1.20101330950408));
#51829=CARTESIAN_POINT('Ctrl Pts',(-0.286289625659754,-0.328836945108058,
-1.18128624647539));
#51830=CARTESIAN_POINT('Ctrl Pts',(0.118499450080301,-0.4195871382193,-1.16155918344669));
#51831=CARTESIAN_POINT('Ctrl Pts',(0.416013249139481,-0.130493152191252,
-1.141832120418));
#51832=CARTESIAN_POINT('Ctrl Pts',(0.336918242215987,0.276733778730547,
-1.12210505738931));
#51833=CARTESIAN_POINT('Ctrl Pts',(-0.047182379738299,0.433438933727265,
-1.10237799436062));
#51834=CARTESIAN_POINT('Ctrl Pts',(-0.38856969933162,0.197760145099391,
-1.08265093133193));
#51835=CARTESIAN_POINT('Ctrl Pts',(-0.378192331600609,-0.21694710541257,
-1.06292386830324));
#51836=CARTESIAN_POINT('Ctrl Pts',(-0.0254447082815231,-0.435256307305093,
-1.04319680527454));
#51837=CARTESIAN_POINT('Ctrl Pts',(0.350337520844719,-0.259536332170997,
-1.02346974224585));
#51838=CARTESIAN_POINT('Ctrl Pts',(0.408965919680273,0.1511369007505,-1.00374267921716));
#51839=CARTESIAN_POINT('Ctrl Pts',(0.0973653245667549,0.424988799617599,
-0.984015616188466));
#51840=CARTESIAN_POINT('Ctrl Pts',(-0.302378229226684,0.314106499006519,
-0.964288553159777));
#51841=CARTESIAN_POINT('Ctrl Pts',(-0.428384578496533,-0.0811303835486135,
-0.944561490131084));
#51842=CARTESIAN_POINT('Ctrl Pts',(-0.166582594876293,-0.402921487777307,
-0.924834427102392));
#51843=CARTESIAN_POINT('Ctrl Pts',(0.246023413095639,-0.359955506190932,
-0.905107364073701));
#51844=CARTESIAN_POINT('Ctrl Pts',(0.435909149438275,0.00887128313141311,
-0.885380301045008));
#51845=CARTESIAN_POINT('Ctrl Pts',(0.231174703307272,0.369667070185041,
-0.865653238016316));
#51846=CARTESIAN_POINT('Ctrl Pts',(-0.182837762612857,0.395810357104412,
-0.845926174987624));
#51847=CARTESIAN_POINT('Ctrl Pts',(-0.431330712968026,0.0636341282559295,
-0.826199111958933));
#51848=CARTESIAN_POINT('Ctrl Pts',(-0.289348251468989,-0.326148854973054,
-0.80647204893024));
#51849=CARTESIAN_POINT('Ctrl Pts',(0.114575625896769,-0.420675542643931,
-0.786744985901549));
#51850=CARTESIAN_POINT('Ctrl Pts',(0.414776389268069,-0.134372739549877,
-0.767017922872856));
#51851=CARTESIAN_POINT('Ctrl Pts',(0.339488052147569,0.273575124376166,
-0.747290859844165));
#51852=CARTESIAN_POINT('Ctrl Pts',(-0.0431322995881918,0.433860681510395,
-0.727563796815472));
#51853=CARTESIAN_POINT('Ctrl Pts',(-0.386705808751533,0.201380494850412,
-0.707836733786781));
#51854=CARTESIAN_POINT('Ctrl Pts',(-0.38020197494145,-0.213405586803507,
-0.688109670758089));
#51855=CARTESIAN_POINT('Ctrl Pts',(-0.0295085940169031,-0.434999688629514,
-0.668382607729396));
#51856=CARTESIAN_POINT('Ctrl Pts',(0.347898350434672,-0.26279692538727,
-0.648655544700706));
#51857=CARTESIAN_POINT('Ctrl Pts',(0.410359598729604,0.147310848067984,
-0.628928481672012));
#51858=CARTESIAN_POINT('Ctrl Pts',(0.101330182194475,0.424060939496253,
-0.609201418643322));
#51859=CARTESIAN_POINT('Ctrl Pts',(-0.299431502496743,0.316916805390477,
-0.589474355614628));
#51860=CARTESIAN_POINT('Ctrl Pts',(-0.429123597787398,-0.0771260270514894,
-0.569747292585937));
#51861=CARTESIAN_POINT('Ctrl Pts',(-0.170338340217374,-0.401348148234573,
-0.550020229557245));
#51862=CARTESIAN_POINT('Ctrl Pts',(0.242650945846931,-0.36223749763258,
-0.530293166528553));
#51863=CARTESIAN_POINT('Ctrl Pts',(0.435972990113586,0.00479980364938559,
-0.510566103499861));
#51864=CARTESIAN_POINT('Ctrl Pts',(0.234617058186499,0.367491935024725,
-0.490839040471169));
#51865=CARTESIAN_POINT('Ctrl Pts',(-0.179133191333578,0.397500674034188,
-0.471111977442477));
#51866=CARTESIAN_POINT('Ctrl Pts',(-0.430717602467341,0.0676596864390125,
-0.451384914413786));
#51867=CARTESIAN_POINT('Ctrl Pts',(-0.292381639032076,-0.323432317250295,
-0.431657851385093));
#51868=CARTESIAN_POINT('Ctrl Pts',(0.11064180801636,-0.42172725253579,-0.411930788356402));
#51869=CARTESIAN_POINT('Ctrl Pts',(0.41350335041029,-0.138240608659184,
-0.39220372532771));
#51870=CARTESIAN_POINT('Ctrl Pts',(0.342028250803996,0.270392612059835,
-0.372476662299018));
#51871=CARTESIAN_POINT('Ctrl Pts',(-0.0390784581292962,0.434244577221532,
-0.352749599270326));
#51872=CARTESIAN_POINT('Ctrl Pts',(-0.38480818616533,0.204983295933599,
-0.333022536241634));
#51873=CARTESIAN_POINT('Ctrl Pts',(-0.382178458559626,-0.209845485925839,
-0.313295473212942));
#51874=CARTESIAN_POINT('Ctrl Pts',(-0.0335698995935445,-0.434705065985486,
-0.29356841018425));
#51875=CARTESIAN_POINT('Ctrl Pts',(0.345428822663414,-0.266034713591485,
-0.273841347155558));
#51876=CARTESIAN_POINT('Ctrl Pts',(0.411717507348085,0.143472171132698,
-0.254114284126866));
#51877=CARTESIAN_POINT('Ctrl Pts',(0.105286157144576,0.423095659876829,
-0.234387221098174));
#51878=CARTESIAN_POINT('Ctrl Pts',(-0.296458573285809,0.319700294474994,
-0.214660158069482));
#51879=CARTESIAN_POINT('Ctrl Pts',(-0.42982534912142,-0.0731165253287872,
-0.19493309504079));
#51880=CARTESIAN_POINT('Ctrl Pts',(-0.174078917024553,-0.399736769822525,
-0.175206032012098));
#51881=CARTESIAN_POINT('Ctrl Pts',(0.239256717870959,-0.364493701490054,
-0.155478968983406));
#51882=CARTESIAN_POINT('Ctrl Pts',(0.435999944379018,0.000739035179609862,
-0.135751905954714));
#51883=CARTESIAN_POINT('Ctrl Pts',(0.238036761798838,0.365263419299111,
-0.116024842926023));
#51884=CARTESIAN_POINT('Ctrl Pts',(-0.175408803030969,0.399197187981461,
-0.0962977798973306));
#51885=CARTESIAN_POINT('Ctrl Pts',(-0.43007497292556,0.0716009816669133,
-0.076570716868639));
#51886=CARTESIAN_POINT('Ctrl Pts',(-0.295373939959455,-0.320536944194281,
-0.056843653839947));
#51887=CARTESIAN_POINT('Ctrl Pts',(0.106667041062779,-0.423035100006457,
-0.0371165908112548));
#51888=CARTESIAN_POINT('Ctrl Pts',(0.412267133134432,-0.14149617474194,
-0.017389527782563));
#51889=CARTESIAN_POINT('Ctrl Pts',(0.366956567112532,0.129967546999451,
-0.00423815243010174));
#51890=CARTESIAN_POINT('Ctrl Pts',(0.292087747121744,0.226511343217827,
0.00233753524612886));
#51891=CARTESIAN_POINT('Ctrl Pts',(-0.174869447533103,0.352286199445092,
-1.9567));
#51892=CARTESIAN_POINT('Ctrl Pts',(-0.291310645032558,0.294486581098146,
-1.95012431232377));
#51893=CARTESIAN_POINT('Ctrl Pts',(-0.460466557433677,0.055434592211573,
-1.93697293697131));
#51894=CARTESIAN_POINT('Ctrl Pts',(-0.298144091078689,-0.355823232196569,
-1.91724587394261));
#51895=CARTESIAN_POINT('Ctrl Pts',(0.134461295881938,-0.443877819611432,
-1.89751881091393));
#51896=CARTESIAN_POINT('Ctrl Pts',(0.445147114490617,-0.130638080935181,
-1.87779174788523));
#51897=CARTESIAN_POINT('Ctrl Pts',(0.352950856297826,0.301144654531963,
-1.85806468485654));
#51898=CARTESIAN_POINT('Ctrl Pts',(-0.0588177357417202,0.46016169961182,
-1.83833762182785));
#51899=CARTESIAN_POINT('Ctrl Pts',(-0.417312261114324,0.202678947727898,
-1.81861055879916));
#51900=CARTESIAN_POINT('Ctrl Pts',(-0.398036361464054,-0.238324695058641,
-1.79888349577047));
#51901=CARTESIAN_POINT('Ctrl Pts',(-0.0184182971104594,-0.463556937023687,
-1.77915643274177));
#51902=CARTESIAN_POINT('Ctrl Pts',(0.377869588997804,-0.269150752356283,
-1.75942936971308));
#51903=CARTESIAN_POINT('Ctrl Pts',(0.432081432251388,0.168918059316679,
-1.73970230668439));
#51904=CARTESIAN_POINT('Ctrl Pts',(0.0951371872085753,0.45406566287855,
-1.7199752436557));
#51905=CARTESIAN_POINT('Ctrl Pts',(-0.327932370894076,0.32815787152906,
-1.700248180627));
#51906=CARTESIAN_POINT('Ctrl Pts',(-0.454131340716204,-0.0948257382630977,
-1.68052111759831));
#51907=CARTESIAN_POINT('Ctrl Pts',(-0.169213776865482,-0.431965011214454,
-1.66079405456962));
#51908=CARTESIAN_POINT('Ctrl Pts',(0.268889690880362,-0.378054871853828,
-1.64106699154093));
#51909=CARTESIAN_POINT('Ctrl Pts',(0.463572526028849,0.0181011969713046,
-1.62133992851224));
#51910=CARTESIAN_POINT('Ctrl Pts',(0.238592033566427,0.39787054050644,-1.60161286548354));
#51911=CARTESIAN_POINT('Ctrl Pts',(-0.202381234110116,0.41745535472716,
-1.58188580245485));
#51912=CARTESIAN_POINT('Ctrl Pts',(-0.460142662617045,0.0591258363281124,
-1.56215873942616));
#51913=CARTESIAN_POINT('Ctrl Pts',(-0.301345771453645,-0.352729157915705,
-1.54243167639747));
#51914=CARTESIAN_POINT('Ctrl Pts',(0.130253658441064,-0.445265223149938,
-1.52270461336878));
#51915=CARTESIAN_POINT('Ctrl Pts',(0.443936953368175,-0.134711229744303,
-1.50297755034009));
#51916=CARTESIAN_POINT('Ctrl Pts',(0.355732648642495,0.297794251969122,
-1.48325048731139));
#51917=CARTESIAN_POINT('Ctrl Pts',(-0.0545095917427835,0.460712316371671,
-1.4635234242827));
#51918=CARTESIAN_POINT('Ctrl Pts',(-0.415405345558084,0.206556367230593,
-1.44379636125401));
#51919=CARTESIAN_POINT('Ctrl Pts',(-0.400242616767928,-0.234591094610938,
-1.42406929822532));
#51920=CARTESIAN_POINT('Ctrl Pts',(-0.0227479326789253,-0.463367743307965,
-1.40434223519663));
#51921=CARTESIAN_POINT('Ctrl Pts',(0.375340018065664,-0.272666471726358,
-1.38461517216793));
#51922=CARTESIAN_POINT('Ctrl Pts',(0.433639857885243,0.1648745208274,-1.36488810913924));
#51923=CARTESIAN_POINT('Ctrl Pts',(0.0993738613028271,0.453157775679392,
-1.34516104611055));
#51924=CARTESIAN_POINT('Ctrl Pts',(-0.324853383700292,0.331205997930529,
-1.32543398308186));
#51925=CARTESIAN_POINT('Ctrl Pts',(-0.454997098411088,-0.0905802097830019,
-1.30570692005317));
#51926=CARTESIAN_POINT('Ctrl Pts',(-0.173240676978726,-0.430365892941479,
-1.28597985702447));
#51927=CARTESIAN_POINT('Ctrl Pts',(0.265347202681679,-0.380549597287965,
-1.26625279399578));
#51928=CARTESIAN_POINT('Ctrl Pts',(0.463721355063991,0.0137709413146816,
-1.24652573096709));
#51929=CARTESIAN_POINT('Ctrl Pts',(0.242297469281596,0.395624911180872,
-1.2267986679384));
#51930=CARTESIAN_POINT('Ctrl Pts',(-0.198473662742448,0.419327245912648,
-1.20707160490971));
#51931=CARTESIAN_POINT('Ctrl Pts',(-0.45957039906139,0.0634206770198437,
-1.18734454188102));
#51932=CARTESIAN_POINT('Ctrl Pts',(-0.304626877976278,-0.349899412948255,
-1.16761747885232));
#51933=CARTESIAN_POINT('Ctrl Pts',(0.126089506165929,-0.446462283291582,
-1.14789041582363));
#51934=CARTESIAN_POINT('Ctrl Pts',(0.442659481600427,-0.138851421729646,
-1.12816335279494));
#51935=CARTESIAN_POINT('Ctrl Pts',(0.358498328477641,0.294458965640105,
-1.10843628976625));
#51936=CARTESIAN_POINT('Ctrl Pts',(-0.0502044773786194,0.461201305742126,
-1.08870922673755));
#51937=CARTESIAN_POINT('Ctrl Pts',(-0.413458133911737,0.210426959939374,
-1.06898216370886));
#51938=CARTESIAN_POINT('Ctrl Pts',(-0.402416081213446,-0.230842871988537,
-1.04925510068017));
#51939=CARTESIAN_POINT('Ctrl Pts',(-0.0270744775573185,-0.463135084648206,
-1.02952803765148));
#51940=CARTESIAN_POINT('Ctrl Pts',(0.37277713073582,-0.276159998492671,
-1.00980097462279));
#51941=CARTESIAN_POINT('Ctrl Pts',(0.435160760798787,0.160817431356566,
-0.990073911594096));
#51942=CARTESIAN_POINT('Ctrl Pts',(0.103601710252568,0.4522099286834,-0.970346848565403));
#51943=CARTESIAN_POINT('Ctrl Pts',(-0.321745979181209,0.334225461100479,
-0.950619785536713));
#51944=CARTESIAN_POINT('Ctrl Pts',(-0.455823211965335,-0.0863268984772914,
-0.930892722508018));
#51945=CARTESIAN_POINT('Ctrl Pts',(-0.177252443868371,-0.42872917454938,
-0.911165659479329));
#51946=CARTESIAN_POINT('Ctrl Pts',(0.261781557985834,-0.383011161541817,
-0.891438596450636));
#51947=CARTESIAN_POINT('Ctrl Pts',(0.463829742236249,0.00943950126637505,
-0.871711533421944));
#51948=CARTESIAN_POINT('Ctrl Pts',(0.245981767496114,0.393344764839436,
-0.851984470393252));
#51949=CARTESIAN_POINT('Ctrl Pts',(-0.194548777911764,0.421162565976776,
-0.83225740736456));
#51950=CARTESIAN_POINT('Ctrl Pts',(-0.458958050484476,0.0677099834780056,
-0.812530344335869));
#51951=CARTESIAN_POINT('Ctrl Pts',(-0.307881413061222,-0.347039146867505,
-0.792803281307175));
#51952=CARTESIAN_POINT('Ctrl Pts',(0.121914355536553,-0.447620401547131,
-0.773076218278485));
#51953=CARTESIAN_POINT('Ctrl Pts',(0.44134339911838,-0.142979502103395,
-0.753349155249792));
#51954=CARTESIAN_POINT('Ctrl Pts',(0.36123273834194,0.291097995041313,-0.733622092221101));
#51955=CARTESIAN_POINT('Ctrl Pts',(-0.0458949839108151,0.461650067062667,
-0.713895029192408));
#51956=CARTESIAN_POINT('Ctrl Pts',(-0.411474858524119,0.214279198172926,
-0.694167966163717));
#51957=CARTESIAN_POINT('Ctrl Pts',(-0.404554445030701,-0.227074514142221,
-0.674440903135024));
#51958=CARTESIAN_POINT('Ctrl Pts',(-0.0313986608775075,-0.462862029186305,
-0.654713840106333));
#51959=CARTESIAN_POINT('Ctrl Pts',(0.370181728037756,-0.279629437280525,
-0.63498677707764));
#51960=CARTESIAN_POINT('Ctrl Pts',(0.436643706947187,0.156746314630063,
-0.615259714048949));
#51961=CARTESIAN_POINT('Ctrl Pts',(0.10782052257582,0.451222637819076,-0.595532651020257));
#51962=CARTESIAN_POINT('Ctrl Pts',(-0.318610510468633,0.337215771552452,
-0.575805587991564));
#51963=CARTESIAN_POINT('Ctrl Pts',(-0.456609566478955,-0.0820660573266146,
-0.556078524962873));
#51964=CARTESIAN_POINT('Ctrl Pts',(-0.181248749969547,-0.427055060400831,
-0.53635146193418));
#51965=CARTESIAN_POINT('Ctrl Pts',(0.258193079476759,-0.385439317737961,
-0.51662439890549));
#51966=CARTESIAN_POINT('Ctrl Pts',(0.46389767199641,0.00510723780940766,
-0.496897335876797));
#51967=CARTESIAN_POINT('Ctrl Pts',(0.249644610036525,0.391030309219409,
-0.477170272848105));
#51968=CARTESIAN_POINT('Ctrl Pts',(-0.190606923642869,0.422961150078178,
-0.457443209819413));
#51969=CARTESIAN_POINT('Ctrl Pts',(-0.458305669395753,0.0719933843123827,
-0.437716146790721));
#51970=CARTESIAN_POINT('Ctrl Pts',(-0.31110909335493,-0.344148611091079,
-0.41798908376203));
#51971=CARTESIAN_POINT('Ctrl Pts',(0.117728571099989,-0.448739474933585,
-0.398262020733337));
#51972=CARTESIAN_POINT('Ctrl Pts',(0.439988820335115,-0.147095113657511,
-0.378534957704645));
#51973=CARTESIAN_POINT('Ctrl Pts',(0.363935640287352,0.287711638344625,
-0.358807894675954));
#51974=CARTESIAN_POINT('Ctrl Pts',(-0.0415814882171155,0.462058551832881,
-0.339080831647261));
#51975=CARTESIAN_POINT('Ctrl Pts',(-0.409455690548052,0.21811276372184,
-0.31935376861857));
#51976=CARTESIAN_POINT('Ctrl Pts',(-0.406657525198516,-0.223286383806917,
-0.299626705589878));
#51977=CARTESIAN_POINT('Ctrl Pts',(-0.0357200987761702,-0.462548535548439,
-0.279899642561186));
#51978=CARTESIAN_POINT('Ctrl Pts',(0.367554023546892,-0.283074610363292,
-0.260172579532494));
#51979=CARTESIAN_POINT('Ctrl Pts',(0.438088591518437,0.152661765049684,
-0.240445516503802));
#51980=CARTESIAN_POINT('Ctrl Pts',(0.112029883273486,0.450195530685307,
-0.22071845347511));
#51981=CARTESIAN_POINT('Ctrl Pts',(-0.315447160969382,0.340177547019319,
-0.200991390446418));
#51982=CARTESIAN_POINT('Ctrl Pts',(-0.457356265970795,-0.0777997413914402,
-0.181264327417726));
#51983=CARTESIAN_POINT('Ctrl Pts',(-0.185228915970936,-0.425340470940003,
-0.161537264389034));
#51984=CARTESIAN_POINT('Ctrl Pts',(0.254581446435298,-0.387840034618976,
-0.141810201360342));
#51985=CARTESIAN_POINT('Ctrl Pts',(0.463926352720374,0.000786371420059956,
-0.12208313833165));
#51986=CARTESIAN_POINT('Ctrl Pts',(0.253283350464616,0.38865905393396,-0.102356075302958));
#51987=CARTESIAN_POINT('Ctrl Pts',(-0.186643983042487,0.424766328124745,
-0.0826290122742664));
#51988=CARTESIAN_POINT('Ctrl Pts',(-0.457621878529922,0.0761871250310393,
-0.0629019492455744));
#51989=CARTESIAN_POINT('Ctrl Pts',(-0.314293055356251,-0.341067785327318,
-0.0431748862168827));
#51990=CARTESIAN_POINT('Ctrl Pts',(0.113499214744647,-0.450131091870246,
-0.0234478231881903));
#51991=CARTESIAN_POINT('Ctrl Pts',(0.43867342160777,-0.150559203316891,
-0.00372076015949866));
#51992=CARTESIAN_POINT('Ctrl Pts',(0.390460650241079,0.138292150787645,
0.00943061519296265));
#51993=CARTESIAN_POINT('Ctrl Pts',(0.310796377255278,0.241019712648146,
0.0160063028691932));
#51994=CARTESIAN_POINT('Ctrl Pts',(-0.39355449651014,0.000302947205131077,
-0.0596163522034978));
#51995=CARTESIAN_POINT('Ctrl Pts',(-0.392615901123677,-0.10780295630061,
-0.0541358635412927));
#51996=CARTESIAN_POINT('Ctrl Pts',(-0.346215696154532,-0.216592774920967,
-0.0486553748790877));
#51997=CARTESIAN_POINT('Ctrl Pts',(-0.266882480868379,-0.289702518024748,
-0.0431748862168825));
#51998=CARTESIAN_POINT('Ctrl Pts',(-0.179185181721266,-0.370520205652994,
-0.037116590811255));
#51999=CARTESIAN_POINT('Ctrl Pts',(-0.0512445669495005,-0.407737732630776,
-0.0310582954056274));
#52000=CARTESIAN_POINT('Ctrl Pts',(0.0664872943522231,-0.388263316286114,
-0.0249999999999998));
#52001=CARTESIAN_POINT('',(-0.187158653173901,-0.262360084935059,-1.9567));
#52002=CARTESIAN_POINT('Ctrl Pts',(-0.187552813085389,-0.262697816057798,
-1.9567));
#52003=CARTESIAN_POINT('Ctrl Pts',(-0.194935548663329,-0.258593826308098,
-1.9567));
#52004=CARTESIAN_POINT('Ctrl Pts',(-0.202131816688224,-0.254190080955628,
-1.9567));
#52005=CARTESIAN_POINT('Ctrl Pts',(-0.209120909772877,-0.24949064758629,
-1.9567));
#52006=CARTESIAN_POINT('Ctrl Pts',(-0.222223442058356,-0.240680566407027,
-1.9567));
#52007=CARTESIAN_POINT('Ctrl Pts',(-0.234598714218232,-0.230832940046298,
-1.9567));
#52008=CARTESIAN_POINT('Ctrl Pts',(-0.246211636410528,-0.22008391613474,
-1.9567));
#52009=CARTESIAN_POINT('Ctrl Pts',(-0.25218100502691,-0.214558615531508,
-1.9567));
#52010=CARTESIAN_POINT('Ctrl Pts',(-0.257951737717882,-0.208790930776044,
-1.9567));
#52011=CARTESIAN_POINT('Ctrl Pts',(-0.263498052368722,-0.202819781274129,
-1.9567));
#52012=CARTESIAN_POINT('Ctrl Pts',(-0.27392963993244,-0.191589158273713,
-1.9567));
#52013=CARTESIAN_POINT('Ctrl Pts',(-0.283582022411786,-0.179628639232479,
-1.9567));
#52014=CARTESIAN_POINT('Ctrl Pts',(-0.292422866190421,-0.167055175905498,
-1.9567));
#52015=CARTESIAN_POINT('Ctrl Pts',(-0.297639339867104,-0.159636298011915,
-1.9567));
#52016=CARTESIAN_POINT('Ctrl Pts',(-0.302573086946691,-0.152003640288341,
-1.9567));
#52017=CARTESIAN_POINT('Ctrl Pts',(-0.307215418838992,-0.144178520553397,
-1.9567));
#52018=CARTESIAN_POINT('Ctrl Pts',(-0.310148605333973,-0.139234338176816,
-1.9567));
#52019=CARTESIAN_POINT('Ctrl Pts',(-0.312961281228168,-0.13422009210485,
-1.9567));
#52020=CARTESIAN_POINT('Ctrl Pts',(-0.315649496491177,-0.129146472523924,
-1.9567));
#52021=CARTESIAN_POINT('Ctrl Pts',(-0.325055516088252,-0.111393963689168,
-1.9567));
#52022=CARTESIAN_POINT('Ctrl Pts',(-0.332950944425937,-0.0929001179375588,
-1.9567));
#52023=CARTESIAN_POINT('Ctrl Pts',(-0.339260540400532,-0.073901239993573,
-1.9567));
#52024=CARTESIAN_POINT('Ctrl Pts',(-0.343323872756722,-0.0616661054791059,
-1.9567));
#52025=CARTESIAN_POINT('Ctrl Pts',(-0.346728888529677,-0.0492205679713237,
-1.9567));
#52026=CARTESIAN_POINT('Ctrl Pts',(-0.349446343340807,-0.0366210092019528,
-1.9567));
#52027=CARTESIAN_POINT('Ctrl Pts',(-0.350667565657802,-0.0309587761850763,
-1.9567));
#52028=CARTESIAN_POINT('Ctrl Pts',(-0.351749819276766,-0.0252653862353323,
-1.9567));
#52029=CARTESIAN_POINT('Ctrl Pts',(-0.352689875393039,-0.0195457697562147,
-1.9567));
#52030=CARTESIAN_POINT('Ctrl Pts',(-0.353507442449902,-0.014571417767787,
-1.9567));
#52031=CARTESIAN_POINT('Ctrl Pts',(-0.354216678467517,-0.00958102422836672,
-1.9567));
#52032=CARTESIAN_POINT('Ctrl Pts',(-0.35481498228772,-0.00458766379930495,
-1.9567));
#52033=CARTESIAN_POINT('Ctrl Pts',(-0.356697198872877,0.0111210539087855,
-1.9567));
#52034=CARTESIAN_POINT('Ctrl Pts',(-0.357487439202542,0.0268861216299494,
-1.9567));
#52035=CARTESIAN_POINT('Ctrl Pts',(-0.357144615700508,0.0426014586103036,
-1.9567));
#52036=CARTESIAN_POINT('Ctrl Pts',(-0.356807049244469,0.0580758078846414,
-1.9567));
#52037=CARTESIAN_POINT('Ctrl Pts',(-0.355371211339537,0.073502369822222,
-1.9567));
#52038=CARTESIAN_POINT('Ctrl Pts',(-0.352905425918931,0.0888045736652499,
-1.9567));
#52039=CARTESIAN_POINT('Ctrl Pts',(-0.351706553656186,0.0962445510424256,
-1.9567));
#52040=CARTESIAN_POINT('Ctrl Pts',(-0.350263912372945,0.103655167772351,
-1.9567));
#52041=CARTESIAN_POINT('Ctrl Pts',(-0.348583746098634,0.111027644159136,
-1.9567));
#52042=CARTESIAN_POINT('Ctrl Pts',(-0.347031212449488,0.117840075668466,
-1.9567));
#52043=CARTESIAN_POINT('Ctrl Pts',(-0.345274228680375,0.124624481655365,
-1.9567));
#52044=CARTESIAN_POINT('Ctrl Pts',(-0.343326242497342,0.131345086743347,
-1.9567));
#52045=CARTESIAN_POINT('Ctrl Pts',(-0.337583166709954,0.151158853747225,
-1.9567));
#52046=CARTESIAN_POINT('Ctrl Pts',(-0.33017628709199,0.170461698596435,
-1.9567));
#52047=CARTESIAN_POINT('Ctrl Pts',(-0.321266461276679,0.189081419077276,
-1.9567));
#52048=CARTESIAN_POINT('Ctrl Pts',(-0.31329530345099,0.20573951472354,-1.9567));
#52049=CARTESIAN_POINT('Ctrl Pts',(-0.304120165756624,0.221851611522826,
-1.9567));
#52050=CARTESIAN_POINT('Ctrl Pts',(-0.293823122110593,0.237289775994537,
-1.9567));
#52051=CARTESIAN_POINT('Ctrl Pts',(-0.290958000853211,0.241585398575482,
-1.9567));
#52052=CARTESIAN_POINT('Ctrl Pts',(-0.28800585086645,0.24582877974099,-1.9567));
#52053=CARTESIAN_POINT('Ctrl Pts',(-0.284968063826039,0.250016978740807,
-1.9567));
#52054=CARTESIAN_POINT('Ctrl Pts',(-0.281677119186157,0.254554206290288,
-1.9567));
#52055=CARTESIAN_POINT('Ctrl Pts',(-0.27829098021799,0.259019238257219,
-1.9567));
#52056=CARTESIAN_POINT('Ctrl Pts',(-0.274815287336952,0.263405262319202,
-1.9567));
#52057=CARTESIAN_POINT('Ctrl Pts',(-0.260861563440262,0.2810136560582,-1.9567));
#52058=CARTESIAN_POINT('Ctrl Pts',(-0.245455106563924,0.297369120256383,
-1.9567));
#52059=CARTESIAN_POINT('Ctrl Pts',(-0.228753469246794,0.312258507679545,
-1.9567));
#52060=CARTESIAN_POINT('Ctrl Pts',(-0.212051831929664,0.327147895102707,
-1.9567));
#52061=CARTESIAN_POINT('Ctrl Pts',(-0.194054188732127,0.340572959327143,
-1.9567));
#52062=CARTESIAN_POINT('Ctrl Pts',(-0.174869447533103,0.352286199445092,
-1.9567));
#52063=CARTESIAN_POINT('Ctrl Pts',(-0.187552813085386,-0.2626978160578,
-1.9567));
#52064=CARTESIAN_POINT('Ctrl Pts',(-0.107650951219408,-0.319062579074347,
-1.95064170459437));
#52065=CARTESIAN_POINT('Ctrl Pts',(0.116856291925146,-0.356987215547139,
-1.93800772151252));
#52066=CARTESIAN_POINT('Ctrl Pts',(0.364759182106444,-0.107046497669421,
-1.91879805075442));
#52067=CARTESIAN_POINT('Ctrl Pts',(0.289212400745945,0.246761743044216,
-1.89907098772573));
#52068=CARTESIAN_POINT('Ctrl Pts',(-0.0481959974222359,0.377062323270783,
-1.87934392469704));
#52069=CARTESIAN_POINT('Ctrl Pts',(-0.288676763686436,0.204340998144533,
-1.86319448047936));
#52070=CARTESIAN_POINT('Ctrl Pts',(-0.321878386934234,0.0488203878451577,
-1.85362072393791));
#52071=CARTESIAN_POINT('Ctrl Pts',(-0.321776643047528,7.65958109301274E-5,
-1.85062265507269));
#52072=CARTESIAN_POINT('Origin',(-5.160062080289E-17,2.1385152528819E-17,
-1.9567));
#52073=CARTESIAN_POINT('',(-0.3933,-4.81653586104654E-17,-1.9567));
#52074=CARTESIAN_POINT('Origin',(0.,0.,-1.9567));
#52075=CARTESIAN_POINT('Origin',(0.,0.,-1.9567));
#52076=CARTESIAN_POINT('',(0.1871586531739,-0.26236008493506,-1.9567));
#52077=CARTESIAN_POINT('Ctrl Pts',(0.175279276633882,0.352769203968885,
-1.9567));
#52078=CARTESIAN_POINT('Ctrl Pts',(0.18401188138755,0.347494710900982,-1.9567));
#52079=CARTESIAN_POINT('Ctrl Pts',(0.192510825180566,0.341867276831141,
-1.9567));
#52080=CARTESIAN_POINT('Ctrl Pts',(0.200751394782037,0.335885922983975,
-1.9567));
#52081=CARTESIAN_POINT('Ctrl Pts',(0.213438686096218,0.326676950500004,
-1.9567));
#52082=CARTESIAN_POINT('Ctrl Pts',(0.225514123628146,0.31662934757912,-1.9567));
#52083=CARTESIAN_POINT('Ctrl Pts',(0.236936545916664,0.305829861134869,
-1.9567));
#52084=CARTESIAN_POINT('Ctrl Pts',(0.242016167800701,0.301027262676071,
-1.9567));
#52085=CARTESIAN_POINT('Ctrl Pts',(0.24696649261074,0.296075857763358,-1.9567));
#52086=CARTESIAN_POINT('Ctrl Pts',(0.251783114237367,0.290982853163268,
-1.9567));
#52087=CARTESIAN_POINT('Ctrl Pts',(0.256613931187417,0.285874838696699,
-1.9567));
#52088=CARTESIAN_POINT('Ctrl Pts',(0.261305021417189,0.28062973144462,-1.9567));
#52089=CARTESIAN_POINT('Ctrl Pts',(0.265847944049976,0.275261265940149,
-1.9567));
#52090=CARTESIAN_POINT('Ctrl Pts',(0.279770568182666,0.258808613445338,
-1.9567));
#52091=CARTESIAN_POINT('Ctrl Pts',(0.292320623894356,0.241182479441691,
-1.9567));
#52092=CARTESIAN_POINT('Ctrl Pts',(0.303375664813956,0.222603261998498,
-1.9567));
#52093=CARTESIAN_POINT('Ctrl Pts',(0.306375953356426,0.217560945680695,
-1.9567));
#52094=CARTESIAN_POINT('Ctrl Pts',(0.309266773479844,0.212446594923143,
-1.9567));
#52095=CARTESIAN_POINT('Ctrl Pts',(0.312042062173041,0.207270037278723,
-1.9567));
#52096=CARTESIAN_POINT('Ctrl Pts',(0.321991404607397,0.188712204084018,
-1.9567));
#52097=CARTESIAN_POINT('Ctrl Pts',(0.330416802963934,0.169438735026911,
-1.9567));
#52098=CARTESIAN_POINT('Ctrl Pts',(0.337214313055224,0.14965760095231,-1.9567));
#52099=CARTESIAN_POINT('Ctrl Pts',(0.343828133188892,0.13041101491531,-1.9567));
#52100=CARTESIAN_POINT('Ctrl Pts',(0.348901095948526,0.110682458297764,
-1.9567));
#52101=CARTESIAN_POINT('Ctrl Pts',(0.352289246031495,0.0906606792142431,
-1.9567));
#52102=CARTESIAN_POINT('Ctrl Pts',(0.353252716161339,0.0849671929102308,
-1.9567));
#52103=CARTESIAN_POINT('Ctrl Pts',(0.354079629151872,0.0792500462139911,
-1.9567));
#52104=CARTESIAN_POINT('Ctrl Pts',(0.354765894650996,0.0735137648268453,
-1.9567));
#52105=CARTESIAN_POINT('Ctrl Pts',(0.355373602604548,0.0684341217044198,
-1.9567));
#52106=CARTESIAN_POINT('Ctrl Pts',(0.355869792336237,0.0633496018900003,
-1.9567));
#52107=CARTESIAN_POINT('Ctrl Pts',(0.356252722462039,0.0582640302401743,
-1.9567));
#52108=CARTESIAN_POINT('Ctrl Pts',(0.357356305926245,0.0436076937426857,
-1.9567));
#52109=CARTESIAN_POINT('Ctrl Pts',(0.357520611329765,0.02894029824759,-1.9567));
#52110=CARTESIAN_POINT('Ctrl Pts',(0.356695878885865,0.014335105717066,
-1.9567));
#52111=CARTESIAN_POINT('Ctrl Pts',(0.355625235707653,-0.00462492170141671,
-1.9567));
#52112=CARTESIAN_POINT('Ctrl Pts',(0.352888647131212,-0.0234812913700506,
-1.9567));
#52113=CARTESIAN_POINT('Ctrl Pts',(0.348579205973286,-0.0420611896612138,
-1.9567));
#52114=CARTESIAN_POINT('Ctrl Pts',(0.347014174789672,-0.0488087281815105,
-1.9567));
#52115=CARTESIAN_POINT('Ctrl Pts',(0.345241366742302,-0.0555196103104209,
-1.9567));
#52116=CARTESIAN_POINT('Ctrl Pts',(0.343264193680855,-0.0621847523977205,
-1.9567));
#52117=CARTESIAN_POINT('Ctrl Pts',(0.341896092993538,-0.0667966832643223,
-1.9567));
#52118=CARTESIAN_POINT('Ctrl Pts',(0.340432832629664,-0.0713775965145813,
-1.9567));
#52119=CARTESIAN_POINT('Ctrl Pts',(0.338876628876197,-0.0759244413272143,
-1.9567));
#52120=CARTESIAN_POINT('Ctrl Pts',(0.332244083465024,-0.0953031085680316,
-1.9567));
#52121=CARTESIAN_POINT('Ctrl Pts',(0.323926310238762,-0.114068452668091,
-1.9567));
#52122=CARTESIAN_POINT('Ctrl Pts',(0.3140504528883,-0.132005064082091,-1.9567));
#52123=CARTESIAN_POINT('Ctrl Pts',(0.306024769014135,-0.146581375573242,
-1.9567));
#52124=CARTESIAN_POINT('Ctrl Pts',(0.29696875672258,-0.160610304807908,
-1.9567));
#52125=CARTESIAN_POINT('Ctrl Pts',(0.286930938141069,-0.173954621270129,
-1.9567));
#52126=CARTESIAN_POINT('Ctrl Pts',(0.283445195364828,-0.178588581760084,
-1.9567));
#52127=CARTESIAN_POINT('Ctrl Pts',(0.279839658893929,-0.183140879903125,
-1.9567));
#52128=CARTESIAN_POINT('Ctrl Pts',(0.27613006525648,-0.187589437428766,
-1.9567));
#52129=CARTESIAN_POINT('Ctrl Pts',(0.263608466539964,-0.202605381935755,
-1.9567));
#52130=CARTESIAN_POINT('Ctrl Pts',(0.249871950203262,-0.216487429108968,
-1.9567));
#52131=CARTESIAN_POINT('Ctrl Pts',(0.235016030681469,-0.229027530560931,
-1.9567));
#52132=CARTESIAN_POINT('Ctrl Pts',(0.221150303831382,-0.240731795729455,
-1.9567));
#52133=CARTESIAN_POINT('Ctrl Pts',(0.206308357805613,-0.251267486368473,
-1.9567));
#52134=CARTESIAN_POINT('Ctrl Pts',(0.19054896038177,-0.260420468537189,
-1.9567));
#52135=CARTESIAN_POINT('Ctrl Pts',(0.189423535078913,-0.261074110136054,
-1.9567));
#52136=CARTESIAN_POINT('Ctrl Pts',(0.188293426184883,-0.261720678387043,
-1.9567));
#52137=CARTESIAN_POINT('Ctrl Pts',(0.187158653173905,-0.262360084935056,
-1.9567));
#52138=CARTESIAN_POINT('Origin',(0.,0.,-1.9567));
#52139=CARTESIAN_POINT('Origin',(0.,0.,-2.18777734492731));
#52140=CARTESIAN_POINT('Ctrl Pts',(0.187158653173899,-0.26236008493506,
-1.9567));
#52141=CARTESIAN_POINT('Ctrl Pts',(0.273876561834578,-0.200498514052405,
-1.95012431232377));
#52142=CARTESIAN_POINT('Ctrl Pts',(0.379746143677233,0.0148475562970276,
-1.93697293697131));
#52143=CARTESIAN_POINT('Ctrl Pts',(0.195093989204632,0.326547069892489,
-1.91724587394262));
#52144=CARTESIAN_POINT('Ctrl Pts',(-0.166339572492541,0.341705098143136,
-1.89751881091393));
#52145=CARTESIAN_POINT('Ctrl Pts',(-0.315802122696145,0.133412836380506,
-1.88352930124216));
#52146=CARTESIAN_POINT('Ctrl Pts',(-0.322694708293171,0.013773349684675,
-1.87611547924662));
#52147=CARTESIAN_POINT('Ctrl Pts',(-0.322590464231506,0.000235348495535932,
-1.87527734492731));
#52148=CARTESIAN_POINT('Ctrl Pts',(0.228405859260858,-0.320180657528385,
-1.99770630286919));
#52149=CARTESIAN_POINT('Ctrl Pts',(0.334235208345475,-0.2446856429348,-1.99113061519296));
#52150=CARTESIAN_POINT('Ctrl Pts',(0.463436997310544,0.0181197545314356,
-1.9779792398405));
#52151=CARTESIAN_POINT('Ctrl Pts',(0.238090034765911,0.398513575637932,
-1.95825217681181));
#52152=CARTESIAN_POINT('Ctrl Pts',(-0.202998538084909,0.417012225893093,
-1.93852511378312));
#52153=CARTESIAN_POINT('Ctrl Pts',(-0.46020960849542,0.0585607239402074,
-1.91879805075443));
#52154=CARTESIAN_POINT('Ctrl Pts',(-0.300857582100874,-0.353195579667294,
-1.89907098772573));
#52155=CARTESIAN_POINT('Ctrl Pts',(0.130884172489321,-0.445059242440821,
-1.87934392469704));
#52156=CARTESIAN_POINT('Ctrl Pts',(0.444123796084404,-0.134098311339552,
-1.85961686166835));
#52157=CARTESIAN_POINT('Ctrl Pts',(0.355314607575829,0.298300456258092,
-1.83988979863966));
#52158=CARTESIAN_POINT('Ctrl Pts',(-0.0551582109203669,0.460632047901516,
-1.82016273561097));
#52159=CARTESIAN_POINT('Ctrl Pts',(-0.415695200902475,0.205973509912391,
-1.80043567258227));
#52160=CARTESIAN_POINT('Ctrl Pts',(-0.399912434497174,-0.235154744428263,
-1.78070860955358));
#52161=CARTESIAN_POINT('Ctrl Pts',(-0.0220960326100466,-0.463398870372397,
-1.76098154652489));
#52162=CARTESIAN_POINT('Ctrl Pts',(0.375723176606882,-0.272138490671688,
-1.7412544834962));
#52163=CARTESIAN_POINT('Ctrl Pts',(0.433407568855471,0.165484470229036,
-1.72152742046751));
#52164=CARTESIAN_POINT('Ctrl Pts',(0.0987363280065334,0.453297084197232,
-1.70180035743881));
#52165=CARTESIAN_POINT('Ctrl Pts',(-0.325318971049406,0.330748778547112,
-1.68207329441012));
#52166=CARTESIAN_POINT('Ctrl Pts',(-0.454869275255104,-0.0912201632159526,
-1.66234623138143));
#52167=CARTESIAN_POINT('Ctrl Pts',(-0.172635147307492,-0.430609181263529,
-1.64261916835274));
#52168=CARTESIAN_POINT('Ctrl Pts',(0.26588225829714,-0.38017600839589,-1.62289210532405));
#52169=CARTESIAN_POINT('Ctrl Pts',(0.463701564277583,0.0144232213412824,
-1.60316504229535));
#52170=CARTESIAN_POINT('Ctrl Pts',(0.241740746627904,0.395965377009238,
-1.58343797926666));
#52171=CARTESIAN_POINT('Ctrl Pts',(-0.199063326056669,0.419047684931453,
-1.56371091623797));
#52172=CARTESIAN_POINT('Ctrl Pts',(-0.459659192619251,0.062774168035161,
-1.54398385320928));
#52173=CARTESIAN_POINT('Ctrl Pts',(-0.304134418435672,-0.35032759652435,
-1.52425679018059));
#52174=CARTESIAN_POINT('Ctrl Pts',(0.126717404514493,-0.446284515738235,
-1.50452972715189));
#52175=CARTESIAN_POINT('Ctrl Pts',(0.442854394504287,-0.13822863226102,
-1.4848026641232));
#52176=CARTESIAN_POINT('Ctrl Pts',(0.358083804993756,0.294962977500616,
-1.46507560109451));
#52177=CARTESIAN_POINT('Ctrl Pts',(-0.0508531770824176,0.461130267827548,
-1.44534853806582));
#52178=CARTESIAN_POINT('Ctrl Pts',(-0.413753754459456,0.209845181461624,
-1.42562147503713));
#52179=CARTESIAN_POINT('Ctrl Pts',(-0.402091002995042,-0.23140871812004,
-1.40589441200844));
#52180=CARTESIAN_POINT('Ctrl Pts',(-0.0264229876441398,-0.46317274880931,
-1.38616734897974));
#52181=CARTESIAN_POINT('Ctrl Pts',(0.373165251036872,-0.275635384034748,
-1.36644028595105));
#52182=CARTESIAN_POINT('Ctrl Pts',(0.434934153631336,0.161429401035068,
-1.34671322292236));
#52183=CARTESIAN_POINT('Ctrl Pts',(0.102965518734258,0.452355249185692,
-1.32698615989367));
#52184=CARTESIAN_POINT('Ctrl Pts',(-0.322215823085459,0.333772576565373,
-1.30725909686498));
#52185=CARTESIAN_POINT('Ctrl Pts',(-0.455701367591052,-0.0869680003761401,
-1.28753203383628));
#52186=CARTESIAN_POINT('Ctrl Pts',(-0.176649214587937,-0.428978116573918,
-1.26780497080759));
#52187=CARTESIAN_POINT('Ctrl Pts',(0.262320080288335,-0.382642581257384,
-1.2480779077789));
#52188=CARTESIAN_POINT('Ctrl Pts',(0.463816043661282,0.0100919352058466,
-1.22835084475021));
#52189=CARTESIAN_POINT('Ctrl Pts',(0.24542824910056,0.393690416516892,-1.20862378172152));
#52190=CARTESIAN_POINT('Ctrl Pts',(-0.19514102655331,0.420888523565948,
-1.18889671869283));
#52191=CARTESIAN_POINT('Ctrl Pts',(-0.45905287804943,0.0670643323111496,
-1.16916965566413));
#52192=CARTESIAN_POINT('Ctrl Pts',(-0.307392973975953,-0.347471911187113,
-1.14944259263544));
#52193=CARTESIAN_POINT('Ctrl Pts',(0.122543886747367,-0.447448505791062,
-1.12971552960675));
#52194=CARTESIAN_POINT('Ctrl Pts',(0.441544119938114,-0.142358560198823,
-1.10998846657806));
#52195=CARTESIAN_POINT('Ctrl Pts',(0.360822940066819,0.291605856311808,
-1.09026140354936));
#52196=CARTESIAN_POINT('Ctrl Pts',(-0.0465443187714532,0.461585090643,-1.07053434052067));
#52197=CARTESIAN_POINT('Ctrl Pts',(-0.411775899589728,0.213700205968258,
-1.05080727749198));
#52198=CARTESIAN_POINT('Ctrl Pts',(-0.40423466560533,-0.227643371607329,
-1.03108021446329));
#52199=CARTESIAN_POINT('Ctrl Pts',(-0.0307475511343536,-0.462905776171616,
-1.0113531514346));
#52200=CARTESIAN_POINT('Ctrl Pts',(0.370574730951002,-0.279108470481276,
-0.991626088405904));
#52201=CARTESIAN_POINT('Ctrl Pts',(0.436422825039965,0.157360373976237,
-0.971899025377213));
#52202=CARTESIAN_POINT('Ctrl Pts',(0.107185715996899,0.451373893573872,
-0.952171962348521));
#52203=CARTESIAN_POINT('Ctrl Pts',(-0.319084563512467,0.336767294792508,
-0.932444899319829));
#52204=CARTESIAN_POINT('Ctrl Pts',(-0.456493714871459,-0.0827082692157297,
-0.912717836291138));
#52205=CARTESIAN_POINT('Ctrl Pts',(-0.180647871943726,-0.42730962530232,
-0.892990773262446));
#52206=CARTESIAN_POINT('Ctrl Pts',(0.258735020577411,-0.385075782983832,
-0.873263710233753));
#52207=CARTESIAN_POINT('Ctrl Pts',(0.463890067309698,0.00575977128100029,
-0.853536647205063));
#52208=CARTESIAN_POINT('Ctrl Pts',(0.249094343920831,0.39138111520672,-0.833809584176368));
#52209=CARTESIAN_POINT('Ctrl Pts',(-0.191201705804062,0.422692651002389,
-0.814082521147679));
#52210=CARTESIAN_POINT('Ctrl Pts',(-0.458406522800986,0.071348646569588,
-0.794355458118984));
#52211=CARTESIAN_POINT('Ctrl Pts',(-0.310624717223144,-0.344585917535574,
-0.774628395090295));
#52212=CARTESIAN_POINT('Ctrl Pts',(0.11835968010892,-0.44857346738116,-0.754901332061601));
#52213=CARTESIAN_POINT('Ctrl Pts',(0.440195331831274,-0.146476070904889,
-0.73517426903291));
#52214=CARTESIAN_POINT('Ctrl Pts',(0.363530602464719,0.288223299865512,
-0.715447206004218));
#52215=CARTESIAN_POINT('Ctrl Pts',(-0.0422314006439752,0.461999651854537,
-0.695720142975526));
#52216=CARTESIAN_POINT('Ctrl Pts',(-0.409762127694936,0.217536590532415,
-0.675993079946833));
#52217=CARTESIAN_POINT('Ctrl Pts',(-0.40634306897038,-0.223858168966707,
-0.656266016918143));
#52218=CARTESIAN_POINT('Ctrl Pts',(-0.0350694326791201,-0.46259842672363,
-0.636538953889449));
#52219=CARTESIAN_POINT('Ctrl Pts',(0.367951887597995,-0.2825572117724,-0.616811890860759));
#52220=CARTESIAN_POINT('Ctrl Pts',(0.437873429602004,0.153277621199368,
-0.597084827832066));
#52221=CARTESIAN_POINT('Ctrl Pts',(0.111396564017626,0.450353167026888,
-0.577357764803374));
#52222=CARTESIAN_POINT('Ctrl Pts',(-0.315925471884904,0.339732638569118,
-0.557630701774683));
#52223=CARTESIAN_POINT('Ctrl Pts',(-0.457246244630668,-0.0784413238010682,
-0.53790363874599));
#52224=CARTESIAN_POINT('Ctrl Pts',(-0.184630772338759,-0.425603862177253,
-0.518176575717299));
#52225=CARTESIAN_POINT('Ctrl Pts',(0.25512739277303,-0.387475396406749,
-0.498449512688606));
#52226=CARTESIAN_POINT('Ctrl Pts',(0.463923628310023,0.00142710460425383,
-0.478722449659915));
#52227=CARTESIAN_POINT('Ctrl Pts',(0.252738711523979,0.389037676484367,
-0.458995386631223));
#52228=CARTESIAN_POINT('Ctrl Pts',(-0.187245707469103,0.42445990788846,
-0.43926832360253));
#52229=CARTESIAN_POINT('Ctrl Pts',(-0.457720183329313,0.0756267399820685,
-0.419541260573839));
#52230=CARTESIAN_POINT('Ctrl Pts',(-0.313829366046916,-0.341669872308943,
-0.399814197545147));
#52231=CARTESIAN_POINT('Ctrl Pts',(0.114165149051204,-0.449659293039122,
-0.380087134516455));
#52232=CARTESIAN_POINT('Ctrl Pts',(0.438808148842419,-0.15058082300791,
-0.360360071487763));
#52233=CARTESIAN_POINT('Ctrl Pts',(0.366206554061265,0.284815637206989,
-0.340633008459071));
#52234=CARTESIAN_POINT('Ctrl Pts',(-0.0379147951462677,0.462373850167741,
-0.320905945430379));
#52235=CARTESIAN_POINT('Ctrl Pts',(-0.407712621610348,0.221354125346273,
-0.301178882401688));
#52236=CARTESIAN_POINT('Ctrl Pts',(-0.408416015413171,-0.220053679584459,
-0.281451819372995));
#52237=CARTESIAN_POINT('Ctrl Pts',(-0.0393882817008329,-0.462250268776744,
-0.261724756344303));
#52238=CARTESIAN_POINT('Ctrl Pts',(0.365297000348705,-0.285982185859218,
-0.241997693315612));
#52239=CARTESIAN_POINT('Ctrl Pts',(0.439285743818393,0.149183183090122,
-0.222270630286919));
#52240=CARTESIAN_POINT('Ctrl Pts',(0.115597881363113,0.449289930457205,
-0.202543567258228));
#52241=CARTESIAN_POINT('Ctrl Pts',(-0.312739179970523,0.342674536363465,
-0.182816504229535));
#52242=CARTESIAN_POINT('Ctrl Pts',(-0.457958208506169,-0.0741793948098823,
-0.163089441200844));
#52243=CARTESIAN_POINT('Ctrl Pts',(-0.188598876777895,-0.423838246939006,
-0.143362378172152));
#52244=CARTESIAN_POINT('Ctrl Pts',(0.251500018239493,-0.389884781736394,
-0.123635315143459));
#52245=CARTESIAN_POINT('Ctrl Pts',(0.463911928887255,-0.00282212260801893,
-0.103908252114768));
#52246=CARTESIAN_POINT('Ctrl Pts',(0.256370137272232,0.386499619306331,
-0.0841811890860756));
#52247=CARTESIAN_POINT('Ctrl Pts',(-0.183290037428914,0.42650286845679,
-0.0644541260573842));
#52248=CARTESIAN_POINT('Ctrl Pts',(-0.456969028708115,0.0792558059832603,
-0.0447270630286917));
#52249=CARTESIAN_POINT('Ctrl Pts',(-0.36366155271696,-0.198329305529085,
-0.0315756876762305));
#52250=CARTESIAN_POINT('Ctrl Pts',(-0.268747084003623,-0.287158309717044,
-0.0249999999999999));
#52251=CARTESIAN_POINT('Ctrl Pts',(0.214656790565205,-0.30090713333061,
-1.98403753524613));
#52252=CARTESIAN_POINT('Ctrl Pts',(0.314115659508509,-0.229956599974001,
-1.9774618475699));
#52253=CARTESIAN_POINT('Ctrl Pts',(0.435540046099441,0.0170290217866327,
-1.96431047221744));
#52254=CARTESIAN_POINT('Ctrl Pts',(0.223758019578818,0.374524740389451,
-1.94458340918874));
#52255=CARTESIAN_POINT('Ctrl Pts',(-0.190778882887453,0.391909849976441,
-1.92485634616005));
#52256=CARTESIAN_POINT('Ctrl Pts',(-0.432506932469158,0.0550356155260572,
-1.90512928313136));
#52257=CARTESIAN_POINT('Ctrl Pts',(-0.282747225486995,-0.331934696502731,
-1.88540222010267));
#52258=CARTESIAN_POINT('Ctrl Pts',(0.123005497727857,-0.418268554505945,
-1.86567515707398));
#52259=CARTESIAN_POINT('Ctrl Pts',(0.417389418071951,-0.126026158985205,
-1.84594809404529));
#52260=CARTESIAN_POINT('Ctrl Pts',(0.333926167874943,0.280344027827099,
-1.82622103101659));
#52261=CARTESIAN_POINT('Ctrl Pts',(-0.0518379194290401,0.432903942805994,
-1.8064939679879));
#52262=CARTESIAN_POINT('Ctrl Pts',(-0.390672104331497,0.193574773967371,
-1.78676690495921));
#52263=CARTESIAN_POINT('Ctrl Pts',(-0.375839393849523,-0.22099942133053,
-1.76703984193052));
#52264=CARTESIAN_POINT('Ctrl Pts',(-0.0207659447075708,-0.435504214242047,
-1.74731277890183));
#52265=CARTESIAN_POINT('Ctrl Pts',(0.353106227188709,-0.255756902147272,
-1.72758571587313));
#52266=CARTESIAN_POINT('Ctrl Pts',(0.407318262492253,0.155523003581003,
-1.70785865284444));
#52267=CARTESIAN_POINT('Ctrl Pts',(0.0927928177966288,0.426010512958052,
-1.68813158981575));
#52268=CARTESIAN_POINT('Ctrl Pts',(-0.305736142064931,0.310839098068842,
-1.66840452678706));
#52269=CARTESIAN_POINT('Ctrl Pts',(-0.427488064749981,-0.0857290944029937,
-1.64867746375837));
#52270=CARTESIAN_POINT('Ctrl Pts',(-0.16224324008017,-0.404688326022203,
-1.62895040072967));
#52271=CARTESIAN_POINT('Ctrl Pts',(0.249877268556016,-0.357291017298069,
-1.60922333770098));
#52272=CARTESIAN_POINT('Ctrl Pts',(0.43578868725172,0.0135550042925818,
-1.58949627467229));
#52273=CARTESIAN_POINT('Ctrl Pts',(0.227188973995266,0.372129932563031,
-1.5697692116436));
#52274=CARTESIAN_POINT('Ctrl Pts',(-0.187080554013977,0.393822782971747,
-1.55004214861491));
#52275=CARTESIAN_POINT('Ctrl Pts',(-0.431989649305596,0.0589954280701643,
-1.53031508558622));
#52276=CARTESIAN_POINT('Ctrl Pts',(-0.285826810104969,-0.329239353840106,
-1.51058802255752));
#52277=CARTESIAN_POINT('Ctrl Pts',(0.11908955159845,-0.419420071522361,
-1.49086095952883));
#52278=CARTESIAN_POINT('Ctrl Pts',(0.416196429109198,-0.129907852020033,
-1.47113389650014));
#52279=CARTESIAN_POINT('Ctrl Pts',(0.336528671296254,0.277207451204337,
-1.45140683347145));
#52280=CARTESIAN_POINT('Ctrl Pts',(-0.0477920304578935,0.433372171995315,
-1.43167977044275));
#52281=CARTESIAN_POINT('Ctrl Pts',(-0.388847524770091,0.19721338723049,
-1.41195270741406));
#52282=CARTESIAN_POINT('Ctrl Pts',(-0.377886821718897,-0.217478889995221,
-1.39222564438537));
#52283=CARTESIAN_POINT('Ctrl Pts',(-0.024832435311376,-0.435291704242668,
-1.37249858135668));
#52284=CARTESIAN_POINT('Ctrl Pts',(0.350702277941786,-0.259043297289202,
-1.35277151832799));
#52285=CARTESIAN_POINT('Ctrl Pts',(0.408752953307863,0.151712032437295,
-1.33304445529929));
#52286=CARTESIAN_POINT('Ctrl Pts',(0.0967674290926755,0.425125372439008,
-1.31331739227061));
#52287=CARTESIAN_POINT('Ctrl Pts',(-0.302819790510968,0.313680876208938,
-1.29359032924191));
#52288=CARTESIAN_POINT('Ctrl Pts',(-0.428270068639315,-0.081732893819048,
-1.27386326621322));
#52289=CARTESIAN_POINT('Ctrl Pts',(-0.166015677452493,-0.403155444542677,
-1.25413620318453));
#52290=CARTESIAN_POINT('Ctrl Pts',(0.246529518628468,-0.359609112883956,
-1.23440914015584));
#52291=CARTESIAN_POINT('Ctrl Pts',(0.435896275459704,0.00948444330145363,
-1.21468207712714));
#52292=CARTESIAN_POINT('Ctrl Pts',(0.230654504382898,0.369991915090407,
-1.19495501409845));
#52293=CARTESIAN_POINT('Ctrl Pts',(-0.183394360385883,0.395552810890066,
-1.17522795106976));
#52294=CARTESIAN_POINT('Ctrl Pts',(-0.431419832313808,0.0630273425642208,
-1.15550088804107));
#52295=CARTESIAN_POINT('Ctrl Pts',(-0.2888892143551,-0.326555568707189,
-1.13577382501238));
#52296=CARTESIAN_POINT('Ctrl Pts',(0.115167261985753,-0.420513994286857,
-1.11604676198368));
#52297=CARTESIAN_POINT('Ctrl Pts',(0.414965027541636,-0.133789175727153,
-1.09631969895499));
#52298=CARTESIAN_POINT('Ctrl Pts',(0.339102921998976,0.274052414541705,
-1.0765926359263));
#52299=CARTESIAN_POINT('Ctrl Pts',(-0.0437425472308653,0.433799616396946,
-1.05686557289761));
#52300=CARTESIAN_POINT('Ctrl Pts',(-0.386988728415595,0.200836355532715,
-1.03713850986892));
#52301=CARTESIAN_POINT('Ctrl Pts',(-0.379901444887795,-0.21394020145019,
-1.01741144684022));
#52302=CARTESIAN_POINT('Ctrl Pts',(-0.0288966783321498,-0.435040802230952,
-0.997684383811534));
#52303=CARTESIAN_POINT('Ctrl Pts',(0.348267696231286,-0.262307318590494,
-0.97795732078284));
#52304=CARTESIAN_POINT('Ctrl Pts',(0.410152012980923,0.147887943633276,
-0.958230257754149));
#52305=CARTESIAN_POINT('Ctrl Pts',(0.100733588292278,0.424203090293014,
-0.938503194725457));
#52306=CARTESIAN_POINT('Ctrl Pts',(-0.299877019548172,0.316495325038597,
-0.918776131696764));
#52307=CARTESIAN_POINT('Ctrl Pts',(-0.429014719957699,-0.0777295804954616,
-0.899049068668073));
#52308=CARTESIAN_POINT('Ctrl Pts',(-0.169773632512583,-0.401587389403433,
-0.879322005639382));
#52309=CARTESIAN_POINT('Ctrl Pts',(0.243160264380692,-0.361895846136279,
-0.859594942610688));
#52310=CARTESIAN_POINT('Ctrl Pts',(0.435965843196916,0.00541305736013395,
-0.839867879581998));
#52311=CARTESIAN_POINT('Ctrl Pts',(0.234099915768463,0.367821623972246,
-0.820140816553305));
#52312=CARTESIAN_POINT('Ctrl Pts',(-0.179692170119063,0.397248337469508,
-0.800413753524614));
#52313=CARTESIAN_POINT('Ctrl Pts',(-0.43081238492325,0.0670537591870917,
-0.780686690495921));
#52314=CARTESIAN_POINT('Ctrl Pts',(-0.291926420299019,-0.323843299692569,
-0.76095962746723));
#52315=CARTESIAN_POINT('Ctrl Pts',(0.111234926926673,-0.421571237937353,
-0.741232564438537));
#52316=CARTESIAN_POINT('Ctrl Pts',(0.413697430786003,-0.137658829667478,
-0.721505501409845));
#52317=CARTESIAN_POINT('Ctrl Pts',(0.341647594548745,0.270873473716732,
-0.701778438381154));
#52318=CARTESIAN_POINT('Ctrl Pts',(-0.0396892485711421,0.434189222773285,
-0.682051375352461));
#52319=CARTESIAN_POINT('Ctrl Pts',(-0.38509617708935,0.204441805938325,
-0.66232431232377));
#52320=CARTESIAN_POINT('Ctrl Pts',(-0.3818829312692,-0.210382852032341,
-0.642597249295076));
#52321=CARTESIAN_POINT('Ctrl Pts',(-0.0329584008492724,-0.434751953922507,
-0.622870186266387));
#52322=CARTESIAN_POINT('Ctrl Pts',(0.345802736977903,-0.265548460211983,
-0.603143123237694));
#52323=CARTESIAN_POINT('Ctrl Pts',(0.411515297270889,0.144050955341513,
-0.583416060209001));
#52324=CARTESIAN_POINT('Ctrl Pts',(0.10469096103487,0.423243807175982,-0.56368899718031));
#52325=CARTESIAN_POINT('Ctrl Pts',(-0.296908091903022,0.319282167635671,
-0.543961934151618));
#52326=CARTESIAN_POINT('Ctrl Pts',(-0.429721950601603,-0.0737194871852802,
-0.524234871122926));
#52327=CARTESIAN_POINT('Ctrl Pts',(-0.17351677911445,-0.399984306018987,
-0.504507808094234));
#52328=CARTESIAN_POINT('Ctrl Pts',(0.239769800543433,-0.364151012959176,
-0.484780745065542));
#52329=CARTESIAN_POINT('Ctrl Pts',(0.435997383966672,0.00134119893045557,
-0.465053682036851));
#52330=CARTESIAN_POINT('Ctrl Pts',(0.237524907823671,0.365619250370034,
-0.445326619008158));
#52331=CARTESIAN_POINT('Ctrl Pts',(-0.175974306186799,0.398909212950094,
-0.425599555979466));
#52332=CARTESIAN_POINT('Ctrl Pts',(-0.430167360190942,0.0710743294326753,
-0.405872492950774));
#52333=CARTESIAN_POINT('Ctrl Pts',(-0.29493816278945,-0.321102788080838,
-0.386145429922083));
#52334=CARTESIAN_POINT('Ctrl Pts',(0.107292888934788,-0.422591701473647,
-0.36641836689339));
#52335=CARTESIAN_POINT('Ctrl Pts',(0.412393750358198,-0.14151649301881,
-0.346691303864698));
#52336=CARTESIAN_POINT('Ctrl Pts',(0.344162465153559,0.267670937967541,
-0.326964240836006));
#52337=CARTESIAN_POINT('Ctrl Pts',(-0.0356324845053147,0.434540895927412,
-0.307237177807315));
#52338=CARTESIAN_POINT('Ctrl Pts',(-0.383170042620709,0.208029541269045,
-0.287510114778622));
#52339=CARTESIAN_POINT('Ctrl Pts',(-0.383831095085414,-0.206807376853309,
-0.267783051749931));
#52340=CARTESIAN_POINT('Ctrl Pts',(-0.0370172733884296,-0.434424753614554,
-0.248055988721239));
#52341=CARTESIAN_POINT('Ctrl Pts',(0.343307662735546,-0.26876726531455,
-0.228328925692547));
#52342=CARTESIAN_POINT('Ctrl Pts',(0.412842596132401,0.140202985125062,
-0.208601862663855));
#52343=CARTESIAN_POINT('Ctrl Pts',(0.108639376808644,0.422244572960195,
-0.188874799635163));
#52344=CARTESIAN_POINT('Ctrl Pts',(-0.293913601313514,0.322046975599656,
-0.169147736606471));
#52345=CARTESIAN_POINT('Ctrl Pts',(-0.430391057256783,-0.0697141083310539,
-0.149420673577779));
#52346=CARTESIAN_POINT('Ctrl Pts',(-0.177246020414515,-0.398324973365955,
-0.129693610549087));
#52347=CARTESIAN_POINT('Ctrl Pts',(0.236360778646767,-0.366415363461262,
-0.109966547520395));
#52348=CARTESIAN_POINT('Ctrl Pts',(0.435986388799776,-0.00265224273833729,
-0.0902394844917035));
#52349=CARTESIAN_POINT('Ctrl Pts',(0.240937737069026,0.363233973521747,
-0.0705124214630113));
#52350=CARTESIAN_POINT('Ctrl Pts',(-0.172256750787346,0.400829195914927,
-0.0507853584343198));
#52351=CARTESIAN_POINT('Ctrl Pts',(-0.429461421907545,0.0744849409777822,
-0.0310582954056274));
#52352=CARTESIAN_POINT('Ctrl Pts',(-0.341770662148502,-0.186390718424075,
-0.0179069200531661));
#52353=CARTESIAN_POINT('Ctrl Pts',(-0.252569643846526,-0.2698725914802,
-0.0113312323769355));
#52354=CARTESIAN_POINT('Ctrl Pts',(0.200907721869552,-0.281633609132835,
-1.97036876762307));
#52355=CARTESIAN_POINT('Ctrl Pts',(0.293996110671544,-0.215227557013203,
-1.96379307994683));
#52356=CARTESIAN_POINT('Ctrl Pts',(0.407643094888337,0.0159382890418302,
-1.95064170459437));
#52357=CARTESIAN_POINT('Ctrl Pts',(0.209426004391725,0.35053590514097,-1.93091464156568));
#52358=CARTESIAN_POINT('Ctrl Pts',(-0.178559227689997,0.366807474059788,
-1.91118757853699));
#52359=CARTESIAN_POINT('Ctrl Pts',(-0.404804256442896,0.0515105071119071,
-1.8914605155083));
#52360=CARTESIAN_POINT('Ctrl Pts',(-0.264636868873115,-0.310673813338168,
-1.8717334524796));
#52361=CARTESIAN_POINT('Ctrl Pts',(0.115126822966393,-0.391477866571069,
-1.85200638945091));
#52362=CARTESIAN_POINT('Ctrl Pts',(0.390655040059497,-0.117954006630858,
-1.83227932642222));
#52363=CARTESIAN_POINT('Ctrl Pts',(0.312537728174058,0.262387599396106,
-1.81255226339353));
#52364=CARTESIAN_POINT('Ctrl Pts',(-0.0485176279377133,0.405175837710473,
-1.79282520036483));
#52365=CARTESIAN_POINT('Ctrl Pts',(-0.365649007760519,0.18117603802235,
-1.77309813733615));
#52366=CARTESIAN_POINT('Ctrl Pts',(-0.351766353201873,-0.206844098232797,
-1.75337107430745));
#52367=CARTESIAN_POINT('Ctrl Pts',(-0.019435856805095,-0.407609558111698,
-1.73364401127876));
#52368=CARTESIAN_POINT('Ctrl Pts',(0.330489277770536,-0.239375313622856,
-1.71391694825007));
#52369=CARTESIAN_POINT('Ctrl Pts',(0.381228956129035,0.145561536932969,
-1.69418988522138));
#52370=CARTESIAN_POINT('Ctrl Pts',(0.086849307586724,0.398723941718872,
-1.67446282219269));
#52371=CARTESIAN_POINT('Ctrl Pts',(-0.286153313080456,0.290929417590573,
-1.65473575916399));
#52372=CARTESIAN_POINT('Ctrl Pts',(-0.400106854244859,-0.0802380255900348,
-1.6350086961353));
#52373=CARTESIAN_POINT('Ctrl Pts',(-0.151851332852848,-0.378767470780876,
-1.61528163310661));
#52374=CARTESIAN_POINT('Ctrl Pts',(0.233872278814892,-0.334406026200248,
-1.59555457007792));
#52375=CARTESIAN_POINT('Ctrl Pts',(0.407875810225857,0.0126867872438813,
-1.57582750704923));
#52376=CARTESIAN_POINT('Ctrl Pts',(0.212637201362629,0.348294488116823,
-1.55610044402053));
#52377=CARTESIAN_POINT('Ctrl Pts',(-0.175097781971285,0.368597881012041,
-1.53637338099184));
#52378=CARTESIAN_POINT('Ctrl Pts',(-0.404320105991941,0.055216688105167,
-1.51664631796315));
#52379=CARTESIAN_POINT('Ctrl Pts',(-0.267519201774267,-0.308151111155861,
-1.49691925493446));
#52380=CARTESIAN_POINT('Ctrl Pts',(0.111461698682407,-0.392555627306488,
-1.47719219190577));
#52381=CARTESIAN_POINT('Ctrl Pts',(0.389538463714108,-0.121587071779045,
-1.45746512887707));
#52382=CARTESIAN_POINT('Ctrl Pts',(0.314973537598751,0.259451924908058,
-1.43773806584838));
#52383=CARTESIAN_POINT('Ctrl Pts',(-0.0447308838333691,0.405614076163082,
-1.41801100281969));
#52384=CARTESIAN_POINT('Ctrl Pts',(-0.363941295080726,0.184581592999357,
-1.398283939791));
#52385=CARTESIAN_POINT('Ctrl Pts',(-0.353682640442751,-0.203549061870403,
-1.37855687676231));
#52386=CARTESIAN_POINT('Ctrl Pts',(-0.0232418829786129,-0.407410659676025,
-1.35882981373361));
#52387=CARTESIAN_POINT('Ctrl Pts',(0.3282393048467,-0.242451210543656,-1.33910275070492));
#52388=CARTESIAN_POINT('Ctrl Pts',(0.382571752984389,0.141994663839521,
-1.31937568767623));
#52389=CARTESIAN_POINT('Ctrl Pts',(0.090569339451093,0.397895495692323,
-1.29964862464754));
#52390=CARTESIAN_POINT('Ctrl Pts',(-0.283423757936476,0.293589175852503,
-1.27992156161884));
#52391=CARTESIAN_POINT('Ctrl Pts',(-0.400838769687577,-0.0764977872619564,
-1.26019449859016));
#52392=CARTESIAN_POINT('Ctrl Pts',(-0.155382140317049,-0.377332772511435,
-1.24046743556146));
#52393=CARTESIAN_POINT('Ctrl Pts',(0.230738956968601,-0.336575644510529,
-1.22074037253277));
#52394=CARTESIAN_POINT('Ctrl Pts',(0.407976507258125,0.00887695139706183,
-1.20101330950408));
#52395=CARTESIAN_POINT('Ctrl Pts',(0.215880759665235,0.34629341366392,-1.18128624647539));
#52396=CARTESIAN_POINT('Ctrl Pts',(-0.171647694218456,0.370217098214186,
-1.16155918344669));
#52397=CARTESIAN_POINT('Ctrl Pts',(-0.403786786578187,0.0589903528172908,
-1.14183212041801));
#52398=CARTESIAN_POINT('Ctrl Pts',(-0.270385454734247,-0.305639226227264,
-1.12210505738931));
#52399=CARTESIAN_POINT('Ctrl Pts',(0.107790637224138,-0.393579482782653,
-1.10237799436062));
#52400=CARTESIAN_POINT('Ctrl Pts',(0.388385935145159,-0.125219791255482,
-1.08265093133193));
#52401=CARTESIAN_POINT('Ctrl Pts',(0.317382903931133,0.256498972771602,
-1.06292386830324));
#52402=CARTESIAN_POINT('Ctrl Pts',(-0.0409407756902769,0.406014142150892,
-1.04319680527454));
#52403=CARTESIAN_POINT('Ctrl Pts',(-0.362201557241462,0.187972505097171,
-1.02346974224585));
#52404=CARTESIAN_POINT('Ctrl Pts',(-0.355568224170259,-0.200237031293051,
-1.00374267921716));
#52405=CARTESIAN_POINT('Ctrl Pts',(-0.0270458055299464,-0.407175828290289,
-0.984015616188469));
#52406=CARTESIAN_POINT('Ctrl Pts',(0.32596066151157,-0.245506166699711,
-0.964288553159776));
#52407=CARTESIAN_POINT('Ctrl Pts',(0.38388120092188,0.138415513290315,-0.944561490131084));
#52408=CARTESIAN_POINT('Ctrl Pts',(0.094281460587657,0.397032287012157,
-0.924834427102393));
#52409=CARTESIAN_POINT('Ctrl Pts',(-0.280669475583878,0.296223355284686,
-0.9051073640737));
#52410=CARTESIAN_POINT('Ctrl Pts',(-0.401535725043939,-0.072750891775193,
-0.885380301045009));
#52411=CARTESIAN_POINT('Ctrl Pts',(-0.15889939308144,-0.375865153504546,
-0.865653238016317));
#52412=CARTESIAN_POINT('Ctrl Pts',(0.227585508183973,-0.338715909288726,
-0.845926174987624));
#52413=CARTESIAN_POINT('Ctrl Pts',(0.408041619084134,0.00506634343926735,
-0.826199111958933));
#52414=CARTESIAN_POINT('Ctrl Pts',(0.219105487616094,0.344262132737772,
-0.806472048930241));
#52415=CARTESIAN_POINT('Ctrl Pts',(-0.168182634434063,0.371804023936628,
-0.786744985901549));
#52416=CARTESIAN_POINT('Ctrl Pts',(-0.403218247045515,0.0627588718045951,
-0.767017922872856));
#52417=CARTESIAN_POINT('Ctrl Pts',(-0.273228123374893,-0.303100681849563,
-0.747290859844165));
#52418=CARTESIAN_POINT('Ctrl Pts',(0.104110173744426,-0.394569008493547,
-0.727563796815473));
#52419=CARTESIAN_POINT('Ctrl Pts',(0.387199529740732,-0.128841588430066,
-0.70783673378678));
#52420=CARTESIAN_POINT('Ctrl Pts',(0.31976458663277,0.253523647567951,-0.68810967075809));
#52421=CARTESIAN_POINT('Ctrl Pts',(-0.0371470964983091,0.406378793692034,
-0.668382607729396));
#52422=CARTESIAN_POINT('Ctrl Pts',(-0.360430226483763,0.191347021344234,
-0.648655544700705));
#52423=CARTESIAN_POINT('Ctrl Pts',(-0.357422793568019,-0.196907535097976,
-0.628928481672013));
#52424=CARTESIAN_POINT('Ctrl Pts',(-0.030847369019425,-0.406905481121384,
-0.609201418643321));
#52425=CARTESIAN_POINT('Ctrl Pts',(0.323653586357811,-0.248539708651565,
-0.589474355614629));
#52426=CARTESIAN_POINT('Ctrl Pts',(0.385157164939774,0.134824289483658,
-0.569747292585937));
#52427=CARTESIAN_POINT('Ctrl Pts',(0.0979853580521132,0.396134447325076,
-0.550020229557245));
#52428=CARTESIAN_POINT('Ctrl Pts',(-0.277890711921139,0.298831696702225,
-0.530293166528553));
#52429=CARTESIAN_POINT('Ctrl Pts',(-0.402197656572538,-0.0689976505694917,
-0.510566103499861));
#52430=CARTESIAN_POINT('Ctrl Pts',(-0.16240278589014,-0.374364749860721,
-0.49083904047117));
#52431=CARTESIAN_POINT('Ctrl Pts',(0.224412208313835,-0.340826629511603,
-0.471111977442478));
#52432=CARTESIAN_POINT('Ctrl Pts',(0.408071139623321,0.001255293256657,
-0.451384914413786));
#52433=CARTESIAN_POINT('Ctrl Pts',(0.222311104123364,0.342200824255702,
-0.431657851385094));
#52434=CARTESIAN_POINT('Ctrl Pts',(-0.164702904904495,0.373358518011727,
-0.411930788356401));
#52435=CARTESIAN_POINT('Ctrl Pts',(-0.402614537052571,0.0665219188832822,
-0.39220372532771));
#52436=CARTESIAN_POINT('Ctrl Pts',(-0.276046959531984,-0.300535703852733,
-0.372476662299018));
#52437=CARTESIAN_POINT('Ctrl Pts',(0.100420628818372,-0.395524109908172,
-0.352749599270327));
#52438=CARTESIAN_POINT('Ctrl Pts',(0.385979351873978,-0.132452163029709,
-0.333022536241633));
#52439=CARTESIAN_POINT('Ctrl Pts',(0.322118376245852,0.250526238728093,
-0.313295473212943));
#52440=CARTESIAN_POINT('Ctrl Pts',(-0.0333501738643609,0.406707941687084,
-0.29356841018425));
#52441=CARTESIAN_POINT('Ctrl Pts',(-0.358627463631072,0.194704957191817,
-0.273841347155559));
#52442=CARTESIAN_POINT('Ctrl Pts',(-0.359246174757656,-0.193561074122159,
-0.254114284126866));
#52443=CARTESIAN_POINT('Ctrl Pts',(-0.0346462650760267,-0.406599238452365,
-0.234387221098175));
#52444=CARTESIAN_POINT('Ctrl Pts',(0.321318325122388,-0.251552344769883,
-0.214660158069482));
#52445=CARTESIAN_POINT('Ctrl Pts',(0.386399448446409,0.131222787160003,
-0.194933095040791));
#52446=CARTESIAN_POINT('Ctrl Pts',(0.101680872254175,0.395199215463184,
-0.175206032012099));
#52447=CARTESIAN_POINT('Ctrl Pts',(-0.275088022656505,0.301419414835849,
-0.155478968983407));
#52448=CARTESIAN_POINT('Ctrl Pts',(-0.402823906007397,-0.0652488218522259,
-0.135751905954715));
#52449=CARTESIAN_POINT('Ctrl Pts',(-0.165893164051134,-0.372811699792905,
-0.116024842926023));
#52450=CARTESIAN_POINT('Ctrl Pts',(0.22122153905404,-0.342945945186129,
-0.0962977798973308));
#52451=CARTESIAN_POINT('Ctrl Pts',(0.408060848712296,-0.00248236286865586,
-0.076570716868639));
#52452=CARTESIAN_POINT('Ctrl Pts',(0.22550533686582,0.339968327737163,-0.056843653839947));
#52453=CARTESIAN_POINT('Ctrl Pts',(-0.161223464145778,0.375155523373064,
-0.0371165908112554));
#52454=CARTESIAN_POINT('Ctrl Pts',(-0.401953815106974,0.0697140759723039,
-0.017389527782563));
#52455=CARTESIAN_POINT('Ctrl Pts',(-0.319879771580044,-0.174452131319065,
-0.00423815243010174));
#52456=CARTESIAN_POINT('Ctrl Pts',(-0.236392203689429,-0.252586873243357,
0.00233753524612886));
#52457=CARTESIAN_POINT('Ctrl Pts',(0.187158653173899,-0.26236008493506,
-1.9567));
#52458=CARTESIAN_POINT('Ctrl Pts',(0.273876561834578,-0.200498514052405,
-1.95012431232377));
#52459=CARTESIAN_POINT('Ctrl Pts',(0.379746143677233,0.0148475562970276,
-1.93697293697131));
#52460=CARTESIAN_POINT('Ctrl Pts',(0.195093989204632,0.326547069892489,
-1.91724587394262));
#52461=CARTESIAN_POINT('Ctrl Pts',(-0.166339572492541,0.341705098143136,
-1.89751881091393));
#52462=CARTESIAN_POINT('Ctrl Pts',(-0.377101580416633,0.0479853986977567,
-1.87779174788523));
#52463=CARTESIAN_POINT('Ctrl Pts',(-0.246526512259235,-0.289412930173605,
-1.85806468485654));
#52464=CARTESIAN_POINT('Ctrl Pts',(0.107248148204929,-0.364687178636194,
-1.83833762182785));
#52465=CARTESIAN_POINT('Ctrl Pts',(0.363920662047043,-0.109881854276511,
-1.81861055879916));
#52466=CARTESIAN_POINT('Ctrl Pts',(0.291149288473172,0.244431170965113,
-1.79888349577046));
#52467=CARTESIAN_POINT('Ctrl Pts',(-0.0451973364463865,0.377447732614952,
-1.77915643274177));
#52468=CARTESIAN_POINT('Ctrl Pts',(-0.34062591118954,0.168777302077329,
-1.75942936971308));
#52469=CARTESIAN_POINT('Ctrl Pts',(-0.327693312554222,-0.192688775135064,
-1.73970230668439));
#52470=CARTESIAN_POINT('Ctrl Pts',(-0.0181057689026194,-0.379714901981348,
-1.7199752436557));
#52471=CARTESIAN_POINT('Ctrl Pts',(0.307872328352363,-0.22299372509844,
-1.70024818062701));
#52472=CARTESIAN_POINT('Ctrl Pts',(0.355139649765817,0.135600070284936,
-1.68052111759831));
#52473=CARTESIAN_POINT('Ctrl Pts',(0.0809057973768194,0.371437370479693,
-1.66079405456962));
#52474=CARTESIAN_POINT('Ctrl Pts',(-0.26657048409598,0.271019737112303,
-1.64106699154093));
#52475=CARTESIAN_POINT('Ctrl Pts',(-0.372725643739736,-0.0747469567770755,
-1.62133992851224));
#52476=CARTESIAN_POINT('Ctrl Pts',(-0.141459425625526,-0.352846615539549,
-1.60161286548355));
#52477=CARTESIAN_POINT('Ctrl Pts',(0.217867289073768,-0.311521035102426,
-1.58188580245485));
#52478=CARTESIAN_POINT('Ctrl Pts',(0.379962933199995,0.0118185701951804,
-1.56215873942616));
#52479=CARTESIAN_POINT('Ctrl Pts',(0.198085428729991,0.324459043670616,
-1.54243167639747));
#52480=CARTESIAN_POINT('Ctrl Pts',(-0.163115009928593,0.343372979052334,
-1.52270461336878));
#52481=CARTESIAN_POINT('Ctrl Pts',(-0.376650562678285,0.0514379481401701,
-1.50297755034009));
#52482=CARTESIAN_POINT('Ctrl Pts',(-0.249211593443565,-0.287062868471616,
-1.48325048731139));
#52483=CARTESIAN_POINT('Ctrl Pts',(0.103833845766363,-0.365691183090615,
-1.4635234242827));
#52484=CARTESIAN_POINT('Ctrl Pts',(0.362880498319019,-0.113266291538057,
-1.44379636125401));
#52485=CARTESIAN_POINT('Ctrl Pts',(0.293418403901249,0.24169639861178,-1.42406929822532));
#52486=CARTESIAN_POINT('Ctrl Pts',(-0.0416697372088447,0.377855980330849,
-1.40434223519663));
#52487=CARTESIAN_POINT('Ctrl Pts',(-0.339035065391361,0.171949798768224,
-1.38461517216793));
#52488=CARTESIAN_POINT('Ctrl Pts',(-0.329478459166605,-0.189619233745584,
-1.36488810913924));
#52489=CARTESIAN_POINT('Ctrl Pts',(-0.0216513306458494,-0.379529615109383,
-1.34516104611055));
#52490=CARTESIAN_POINT('Ctrl Pts',(0.305776331751614,-0.225859123798109,
-1.32543398308186));
#52491=CARTESIAN_POINT('Ctrl Pts',(0.356390552660915,0.132277295241747,
-1.30570692005317));
#52492=CARTESIAN_POINT('Ctrl Pts',(0.0843712498095106,0.370665618945638,
-1.28597985702447));
#52493=CARTESIAN_POINT('Ctrl Pts',(-0.264027725361984,0.273497475496068,
-1.26625279399578));
#52494=CARTESIAN_POINT('Ctrl Pts',(-0.37340747073584,-0.0712626807048641,
-1.24652573096709));
#52495=CARTESIAN_POINT('Ctrl Pts',(-0.144748603181605,-0.351510100480195,
-1.2267986679384));
#52496=CARTESIAN_POINT('Ctrl Pts',(0.214948395308735,-0.313542176137101,
-1.20707160490971));
#52497=CARTESIAN_POINT('Ctrl Pts',(0.380056739056546,0.00826945949266903,
-1.18734454188101));
#52498=CARTESIAN_POINT('Ctrl Pts',(0.201107014947573,0.322594912237434,
-1.16761747885232));
#52499=CARTESIAN_POINT('Ctrl Pts',(-0.15990102805103,0.344881385538304,
-1.14789041582363));
#52500=CARTESIAN_POINT('Ctrl Pts',(-0.376153740842564,0.0549533630703619,
-1.12816335279494));
#52501=CARTESIAN_POINT('Ctrl Pts',(-0.251881695113395,-0.28472288374734,
-1.10843628976625));
#52502=CARTESIAN_POINT('Ctrl Pts',(0.100414012462523,-0.366644971278448,
-1.08870922673756));
#52503=CARTESIAN_POINT('Ctrl Pts',(0.361806842748681,-0.116650406783812,
-1.06898216370886));
#52504=CARTESIAN_POINT('Ctrl Pts',(0.295662885863291,0.2389455310015,-1.04925510068017));
#52505=CARTESIAN_POINT('Ctrl Pts',(-0.0381390041496891,0.378228667904838,
-1.02952803765148));
#52506=CARTESIAN_POINT('Ctrl Pts',(-0.337414386067329,0.175108654661627,
-1.00980097462279));
#52507=CARTESIAN_POINT('Ctrl Pts',(-0.331235003452725,-0.186533861135912,
-0.990073911594096));
#52508=CARTESIAN_POINT('Ctrl Pts',(-0.0251949327277424,-0.379310854349625,
-0.970346848565404));
#52509=CARTESIAN_POINT('Ctrl Pts',(0.303653626791853,-0.228705014808928,
-0.950619785536712));
#52510=CARTESIAN_POINT('Ctrl Pts',(0.357610388862838,0.128943082947354,
-0.930892722508019));
#52511=CARTESIAN_POINT('Ctrl Pts',(0.0878293328830358,0.3698614837313,-0.911165659479328));
#52512=CARTESIAN_POINT('Ctrl Pts',(-0.261461931619583,0.275951385530775,
-0.891438596450636));
#52513=CARTESIAN_POINT('Ctrl Pts',(-0.374056730130178,-0.0677722030549249,
-0.871711533421944));
#52514=CARTESIAN_POINT('Ctrl Pts',(-0.148025153650298,-0.350142917605659,
-0.851984470393253));
#52515=CARTESIAN_POINT('Ctrl Pts',(0.212010751987255,-0.315535972441172,
-0.832257407364559));
#52516=CARTESIAN_POINT('Ctrl Pts',(0.380117394971352,0.00471962951840088,
-0.81253034433587));
#52517=CARTESIAN_POINT('Ctrl Pts',(0.204111059463726,0.320702641503297,
-0.792803281307175));
#52518=CARTESIAN_POINT('Ctrl Pts',(-0.156673098749063,0.346359710403747,
-0.773076218278485));
#52519=CARTESIAN_POINT('Ctrl Pts',(-0.37562410916778,0.0584639844220986,
-0.753349155249791));
#52520=CARTESIAN_POINT('Ctrl Pts',(-0.254529826450768,-0.282358064006557,
-0.733622092221101));
#52521=CARTESIAN_POINT('Ctrl Pts',(0.0969854205621785,-0.36756677904974,
-0.713895029192408));
#52522=CARTESIAN_POINT('Ctrl Pts',(0.36070162869546,-0.120024347192654,
-0.694167966163718));
#52523=CARTESIAN_POINT('Ctrl Pts',(0.297881578716796,0.236173821419171,
-0.674440903135024));
#52524=CARTESIAN_POINT('Ctrl Pts',(-0.0346049444254762,0.378568364610783,
-0.654713840106333));
#52525=CARTESIAN_POINT('Ctrl Pts',(-0.335764275878176,0.178252236750144,
-0.63498677707764));
#52526=CARTESIAN_POINT('Ctrl Pts',(-0.332962655866839,-0.18343221816361,
-0.615259714048949));
#52527=CARTESIAN_POINT('Ctrl Pts',(-0.0287363371895775,-0.37905900832026,
-0.595532651020257));
#52528=CARTESIAN_POINT('Ctrl Pts',(0.30150443573772,-0.231530957091147,
-0.575805587991564));
#52529=CARTESIAN_POINT('Ctrl Pts',(0.358799032608658,0.125597623625804,
-0.556078524962874));
#52530=CARTESIAN_POINT('Ctrl Pts',(0.0912797550693568,0.36902508747417,
-0.53635146193418));
#52531=CARTESIAN_POINT('Ctrl Pts',(-0.258873331939256,0.278381225768779,
-0.516624398905489));
#52532=CARTESIAN_POINT('Ctrl Pts',(-0.374673362543473,-0.0642758139537041,
-0.496897335876797));
#52533=CARTESIAN_POINT('Ctrl Pts',(-0.151288792665831,-0.348745193702454,
-0.477170272848105));
#52534=CARTESIAN_POINT('Ctrl Pts',(0.209054616084237,-0.317502246064031,
-0.457443209819413));
#52535=CARTESIAN_POINT('Ctrl Pts',(0.380144895279971,0.00116938758285907,
-0.437716146790722));
#52536=CARTESIAN_POINT('Ctrl Pts',(0.207097300423056,0.318782398141369,
-0.41798908376203));
#52537=CARTESIAN_POINT('Ctrl Pts',(-0.15343150362219,0.34780782307336,-0.398262020733337));
#52538=CARTESIAN_POINT('Ctrl Pts',(-0.3750617139142,0.0619695083338889,
-0.378534957704646));
#52539=CARTESIAN_POINT('Ctrl Pts',(-0.257155756274518,-0.279968619624628,
-0.358807894675954));
#52540=CARTESIAN_POINT('Ctrl Pts',(0.093548368701956,-0.368456518342696,
-0.339080831647262));
#52541=CARTESIAN_POINT('Ctrl Pts',(0.359564953389757,-0.12338783304061,
-0.319353768618569));
#52542=CARTESIAN_POINT('Ctrl Pts',(0.300074287338146,0.233381539488646,
-0.299626705589878));
#52543=CARTESIAN_POINT('Ctrl Pts',(-0.0310678632234075,0.378874987446754,
-0.279899642561186));
#52544=CARTESIAN_POINT('Ctrl Pts',(-0.334084884641434,0.18138037311459,
-0.260172579532494));
#52545=CARTESIAN_POINT('Ctrl Pts',(-0.334661254429897,-0.180314771391009,
-0.240445516503802));
#52546=CARTESIAN_POINT('Ctrl Pts',(-0.032275256763624,-0.378773723290174,
-0.22071845347511));
#52547=CARTESIAN_POINT('Ctrl Pts',(0.299328987509231,-0.234337424225216,
-0.200991390446418));
#52548=CARTESIAN_POINT('Ctrl Pts',(0.359956300760417,0.122242589194944,
-0.181264327417726));
#52549=CARTESIAN_POINT('Ctrl Pts',(0.0947223676997066,0.368153857966175,
-0.161537264389034));
#52550=CARTESIAN_POINT('Ctrl Pts',(-0.256262443999497,0.280791854072041,
-0.141810201360342));
#52551=CARTESIAN_POINT('Ctrl Pts',(-0.37525675475801,-0.0607835353733978,
-0.122083138331651));
#52552=CARTESIAN_POINT('Ctrl Pts',(-0.154540307687754,-0.347298426219855,
-0.102356075302959));
#52553=CARTESIAN_POINT('Ctrl Pts',(0.206082299461314,-0.319476526910996,
-0.0826290122742663));
#52554=CARTESIAN_POINT('Ctrl Pts',(0.380135308624816,-0.00231248299897462,
-0.0629019492455747));
#52555=CARTESIAN_POINT('Ctrl Pts',(0.210072936662614,0.316702681952579,
-0.0431748862168826));
#52556=CARTESIAN_POINT('Ctrl Pts',(-0.15019017750421,0.3494818508312,-0.0234478231881909));
#52557=CARTESIAN_POINT('Ctrl Pts',(-0.374446208306403,0.0649432109668261,
-0.00372076015949865));
#52558=CARTESIAN_POINT('Ctrl Pts',(-0.297988881011587,-0.162513544214055,
0.00943061519296265));
#52559=CARTESIAN_POINT('Ctrl Pts',(-0.220214763532331,-0.235301155006514,
0.0160063028691932));
#52560=CARTESIAN_POINT('Ctrl Pts',(-0.268747084003623,-0.287158309717044,
-0.0249999999999999));
#52561=CARTESIAN_POINT('Ctrl Pts',(-0.347093960934679,-0.213834662086023,
-0.030427882598834));
#52562=CARTESIAN_POINT('Ctrl Pts',(-0.392557762364837,-0.106467699857906,
-0.035855765197668));
#52563=CARTESIAN_POINT('Ctrl Pts',(-0.393507845663966,0.000361442601786235,
-0.041283647796502));
#52564=CARTESIAN_POINT('Origin',(0.,0.,-0.025));
#52565=CARTESIAN_POINT('',(-0.4183,5.12269756083338E-17,0.));
#52566=CARTESIAN_POINT('Origin',(-0.4183,-5.12269756083338E-17,-0.025));
#52567=CARTESIAN_POINT('Origin',(0.,0.,0.));
#52568=CARTESIAN_POINT('Origin',(0.,0.,-0.025));
#52569=CARTESIAN_POINT('Origin',(0.,0.,-0.975));
#52570=CARTESIAN_POINT('Origin',(0.62,0.,0.));
#52571=CARTESIAN_POINT('',(-0.62,-7.59281015471359E-17,8.67361737988404E-18));
#52572=CARTESIAN_POINT('Origin',(0.,0.,0.));
#52573=CARTESIAN_POINT('Origin',(0.,0.,0.32));
#52574=CARTESIAN_POINT('',(0.173205080756888,0.3,0.32));
#52575=CARTESIAN_POINT('',(0.346410161513775,0.,0.32));
#52576=CARTESIAN_POINT('',(0.346410161513775,0.,0.32));
#52577=CARTESIAN_POINT('Origin',(0.,0.,0.32));
#52578=CARTESIAN_POINT('Origin',(0.,0.,0.32));
#52579=CARTESIAN_POINT('',(0.173205080756888,-0.3,0.32));
#52580=CARTESIAN_POINT('',(0.173205080756888,-0.3,0.32));
#52581=CARTESIAN_POINT('Origin',(0.,0.,0.32));
#52582=CARTESIAN_POINT('Origin',(0.,0.,0.32));
#52583=CARTESIAN_POINT('',(-0.173205080756888,-0.3,0.32));
#52584=CARTESIAN_POINT('',(-0.173205080756888,-0.3,0.32));
#52585=CARTESIAN_POINT('Origin',(0.,0.,0.32));
#52586=CARTESIAN_POINT('Origin',(0.,0.,0.32));
#52587=CARTESIAN_POINT('',(-0.346410161513775,5.55111512312578E-17,0.32));
#52588=CARTESIAN_POINT('',(-0.346410161513775,4.24230095489963E-17,0.32));
#52589=CARTESIAN_POINT('Origin',(0.,0.,0.32));
#52590=CARTESIAN_POINT('Origin',(0.,0.,0.32));
#52591=CARTESIAN_POINT('',(-0.173205080756888,0.3,0.32));
#52592=CARTESIAN_POINT('',(-0.173205080756888,0.3,0.32));
#52593=CARTESIAN_POINT('Origin',(0.,0.,0.32));
#52594=CARTESIAN_POINT('Origin',(0.,0.,0.32));
#52595=CARTESIAN_POINT('',(0.173205080756888,0.3,0.32));
#52596=CARTESIAN_POINT('Origin',(0.,0.,0.32));
#52597=CARTESIAN_POINT('Origin',(0.,0.,0.216076951545867));
#52598=CARTESIAN_POINT('',(0.,0.,0.112153903091735));
#52599=CARTESIAN_POINT('',(-0.173205080756888,-2.12115047744981E-17,0.216076951545867));
#52600=CARTESIAN_POINT('Origin',(0.173205080756888,0.3,0.8));
#52601=CARTESIAN_POINT('',(0.173205080756888,0.3,0.8));
#52602=CARTESIAN_POINT('',(0.346410161513775,0.,0.8));
#52603=CARTESIAN_POINT('',(0.21650635094611,0.225,0.8));
#52604=CARTESIAN_POINT('',(0.173205080756888,0.3,0.8));
#52605=CARTESIAN_POINT('',(0.346410161513775,0.,0.8));
#52606=CARTESIAN_POINT('Origin',(-0.173205080756888,0.3,0.8));
#52607=CARTESIAN_POINT('',(-0.173205080756888,0.3,0.8));
#52608=CARTESIAN_POINT('',(-0.0866025403784438,0.3,0.8));
#52609=CARTESIAN_POINT('',(-0.173205080756888,0.3,0.8));
#52610=CARTESIAN_POINT('Origin',(-0.346410161513775,5.55111512312578E-17,
0.8));
#52611=CARTESIAN_POINT('',(-0.346410161513775,4.24230095489963E-17,0.8));
#52612=CARTESIAN_POINT('',(-0.303108891324554,0.0750000000000001,0.8));
#52613=CARTESIAN_POINT('',(-0.346410161513775,4.24230095489963E-17,0.8));
#52614=CARTESIAN_POINT('Origin',(-0.173205080756888,-0.3,0.8));
#52615=CARTESIAN_POINT('',(-0.173205080756888,-0.3,0.8));
#52616=CARTESIAN_POINT('',(-0.21650635094611,-0.225,0.8));
#52617=CARTESIAN_POINT('',(-0.173205080756888,-0.3,0.8));
#52618=CARTESIAN_POINT('Origin',(0.173205080756888,-0.3,0.8));
#52619=CARTESIAN_POINT('',(0.173205080756888,-0.3,0.8));
#52620=CARTESIAN_POINT('',(0.0866025403784439,-0.3,0.8));
#52621=CARTESIAN_POINT('',(0.173205080756888,-0.3,0.8));
#52622=CARTESIAN_POINT('Origin',(0.346410161513775,0.,0.8));
#52623=CARTESIAN_POINT('',(0.303108891324554,-0.075,0.8));
#52624=CARTESIAN_POINT('Origin',(0.635148348882184,-0.269604478657599,0.75));
#52625=CARTESIAN_POINT('',(0.606534182632106,-0.23370127363539,0.0499999999999999));
#52626=CARTESIAN_POINT('',(0.606534182632106,-0.23370127363539,0.75));
#52627=CARTESIAN_POINT('',(0.606534182632106,-0.23370127363539,0.39));
#52628=CARTESIAN_POINT('',(0.592006351095122,-0.215472690295171,0.0499999999999999));
#52629=CARTESIAN_POINT('',(0.635148348882184,-0.269604478657599,0.0499999999999999));
#52630=CARTESIAN_POINT('',(0.592006351095122,-0.215472690295171,0.75));
#52631=CARTESIAN_POINT('',(0.592006351095122,-0.215472690295171,0.75));
#52632=CARTESIAN_POINT('',(0.635148348882184,-0.269604478657599,0.75));
#52633=CARTESIAN_POINT('Origin',(0.625928316354808,-0.235670477458144,0.75));
#52634=CARTESIAN_POINT('',(0.614852423227828,-0.210847095429052,0.75));
#52635=CARTESIAN_POINT('Origin',(0.,0.,0.75));
#52636=CARTESIAN_POINT('',(0.592006351095122,-0.215472690295171,0.75));
#52637=CARTESIAN_POINT('Origin',(0.592006351095122,-0.215472690295171,0.75));
#52638=CARTESIAN_POINT('',(0.614852423227828,-0.210847095429052,0.0499999999999999));
#52639=CARTESIAN_POINT('',(0.614852423227828,-0.210847095429052,0.39));
#52640=CARTESIAN_POINT('',(0.592006351095122,-0.215472690295171,0.0499999999999999));
#52641=CARTESIAN_POINT('Origin',(0.625928316354808,-0.235670477458144,0.0499999999999999));
#52642=CARTESIAN_POINT('Origin',(0.,0.,0.0499999999999999));
#52643=CARTESIAN_POINT('Origin',(0.504634054117228,-0.470578868443124,0.75));
#52644=CARTESIAN_POINT('',(0.490025152569635,-0.427054270379195,0.0499999999999999));
#52645=CARTESIAN_POINT('',(0.490025152569635,-0.427054270379195,0.75));
#52646=CARTESIAN_POINT('',(0.490025152569635,-0.427054270379195,0.39));
#52647=CARTESIAN_POINT('',(0.482607999164956,-0.40495619410252,0.0499999999999999));
#52648=CARTESIAN_POINT('',(0.504634054117228,-0.470578868443124,0.0499999999999999));
#52649=CARTESIAN_POINT('',(0.482607999164956,-0.40495619410252,0.75));
#52650=CARTESIAN_POINT('',(0.482607999164956,-0.40495619410252,0.75));
#52651=CARTESIAN_POINT('',(0.504634054117228,-0.470578868443124,0.75));
#52652=CARTESIAN_POINT('Origin',(0.516833250548794,-0.437767531272822,0.75));
#52653=CARTESIAN_POINT('',(0.505658331181079,-0.408423373605339,0.75));
#52654=CARTESIAN_POINT('Origin',(0.,0.,0.75));
#52655=CARTESIAN_POINT('',(0.482607999164956,-0.40495619410252,0.75));
#52656=CARTESIAN_POINT('Origin',(0.482607999164956,-0.40495619410252,0.75));
#52657=CARTESIAN_POINT('',(0.505658331181079,-0.408423373605339,0.0499999999999999));
#52658=CARTESIAN_POINT('',(0.505658331181079,-0.408423373605339,0.39));
#52659=CARTESIAN_POINT('',(0.482607999164956,-0.40495619410252,0.0499999999999999));
#52660=CARTESIAN_POINT('Origin',(0.516833250548794,-0.437767531272822,0.0499999999999999));
#52661=CARTESIAN_POINT('Origin',(0.,0.,0.0499999999999999));
#52662=CARTESIAN_POINT('Origin',(0.313253444820287,-0.614794501689974,0.75));
#52663=CARTESIAN_POINT('',(0.314411857106244,-0.568898219465488,0.0499999999999999));
#52664=CARTESIAN_POINT('',(0.314411857106244,-0.568898219465488,0.75));
#52665=CARTESIAN_POINT('',(0.314411857106244,-0.568898219465488,0.39));
#52666=CARTESIAN_POINT('',(0.315,-0.545596004384196,0.0499999999999999));
#52667=CARTESIAN_POINT('',(0.313253444820287,-0.614794501689974,0.0499999999999999));
#52668=CARTESIAN_POINT('',(0.315,-0.545596004384196,0.75));
#52669=CARTESIAN_POINT('',(0.315,-0.545596004384196,0.75));
#52670=CARTESIAN_POINT('',(0.313253444820287,-0.614794501689974,0.75));
#52671=CARTESIAN_POINT('Origin',(0.344527189490328,-0.580195253037085,0.75));
#52672=CARTESIAN_POINT('',(0.335474381671726,-0.556737765237794,0.75));
#52673=CARTESIAN_POINT('Origin',(0.,0.,0.75));
#52674=CARTESIAN_POINT('',(0.315,-0.545596004384196,0.75));
#52675=CARTESIAN_POINT('Origin',(0.315,-0.545596004384196,0.75));
#52676=CARTESIAN_POINT('',(0.335474381671726,-0.556737765237794,0.0499999999999999));
#52677=CARTESIAN_POINT('',(0.335474381671726,-0.556737765237794,0.39));
#52678=CARTESIAN_POINT('',(0.315,-0.545596004384196,0.0499999999999999));
#52679=CARTESIAN_POINT('Origin',(0.344527189490328,-0.580195253037085,0.0499999999999999));
#52680=CARTESIAN_POINT('Origin',(0.,0.,0.0499999999999999));
#52681=CARTESIAN_POINT('Origin',(0.0840898469495519,-0.684856844632512,
0.75));
#52682=CARTESIAN_POINT('',(0.100875851451026,-0.642124647240729,0.0499999999999999));
#52683=CARTESIAN_POINT('',(0.100875851451026,-0.642124647240729,0.75));
#52684=CARTESIAN_POINT('',(0.100875851451026,-0.642124647240729,0.39));
#52685=CARTESIAN_POINT('',(0.109398351930166,-0.620428884397691,0.0499999999999999));
#52686=CARTESIAN_POINT('',(0.0840898469495519,-0.684856844632512,0.0499999999999999));
#52687=CARTESIAN_POINT('',(0.109398351930166,-0.620428884397691,0.75));
#52688=CARTESIAN_POINT('',(0.109398351930166,-0.620428884397691,0.75));
#52689=CARTESIAN_POINT('',(0.0840898469495519,-0.684856844632512,0.75));
#52690=CARTESIAN_POINT('Origin',(0.119653037223409,-0.652642864515102,0.75));
#52691=CARTESIAN_POINT('',(0.124827270658193,-0.637901365808246,0.75));
#52692=CARTESIAN_POINT('Origin',(0.,0.,0.75));
#52693=CARTESIAN_POINT('',(0.109398351930166,-0.620428884397691,0.75));
#52694=CARTESIAN_POINT('Origin',(0.109398351930166,-0.620428884397691,0.75));
#52695=CARTESIAN_POINT('',(0.124827270658193,-0.637901365808246,0.0499999999999999));
#52696=CARTESIAN_POINT('',(0.124827270658193,-0.637901365808246,0.39));
#52697=CARTESIAN_POINT('',(0.109398351930166,-0.620428884397691,0.0499999999999999));
#52698=CARTESIAN_POINT('Origin',(0.119653037223409,-0.652642864515102,0.0499999999999999));
#52699=CARTESIAN_POINT('Origin',(0.,0.,0.0499999999999999));
#52700=CARTESIAN_POINT('Origin',(-0.155216227497267,-0.672315344701812,
0.75));
#52701=CARTESIAN_POINT('',(-0.124827270658194,-0.637901365808246,0.0499999999999999));
#52702=CARTESIAN_POINT('',(-0.124827270658194,-0.637901365808246,0.75));
#52703=CARTESIAN_POINT('',(-0.124827270658194,-0.637901365808246,0.39));
#52704=CARTESIAN_POINT('',(-0.109398351930166,-0.620428884397691,0.0499999999999999));
#52705=CARTESIAN_POINT('',(-0.155216227497267,-0.672315344701812,0.0499999999999999));
#52706=CARTESIAN_POINT('',(-0.109398351930166,-0.620428884397691,0.75));
#52707=CARTESIAN_POINT('',(-0.109398351930166,-0.620428884397691,0.75));
#52708=CARTESIAN_POINT('',(-0.155216227497267,-0.672315344701812,0.75));
#52709=CARTESIAN_POINT('Origin',(-0.119653037223409,-0.652642864515102,
0.75));
#52710=CARTESIAN_POINT('',(-0.100875851451026,-0.642124647240729,0.75));
#52711=CARTESIAN_POINT('Origin',(0.,0.,0.75));
#52712=CARTESIAN_POINT('',(-0.109398351930166,-0.620428884397691,0.75));
#52713=CARTESIAN_POINT('Origin',(-0.109398351930166,-0.620428884397691,
0.75));
#52714=CARTESIAN_POINT('',(-0.100875851451026,-0.642124647240729,0.0499999999999999));
#52715=CARTESIAN_POINT('',(-0.100875851451026,-0.642124647240729,0.39));
#52716=CARTESIAN_POINT('',(-0.109398351930166,-0.620428884397691,0.0499999999999999));
#52717=CARTESIAN_POINT('Origin',(-0.119653037223409,-0.652642864515102,
0.0499999999999999));
#52718=CARTESIAN_POINT('Origin',(0.,0.,0.0499999999999999));
#52719=CARTESIAN_POINT('Origin',(-0.375800934160369,-0.578682691882343,
0.75));
#52720=CARTESIAN_POINT('',(-0.335474381671726,-0.556737765237794,0.0499999999999999));
#52721=CARTESIAN_POINT('',(-0.335474381671726,-0.556737765237794,0.75));
#52722=CARTESIAN_POINT('',(-0.335474381671726,-0.556737765237794,0.39));
#52723=CARTESIAN_POINT('',(-0.315,-0.545596004384196,0.0499999999999999));
#52724=CARTESIAN_POINT('',(-0.375800934160369,-0.578682691882343,0.0499999999999999));
#52725=CARTESIAN_POINT('',(-0.315,-0.545596004384196,0.75));
#52726=CARTESIAN_POINT('',(-0.315,-0.545596004384196,0.75));
#52727=CARTESIAN_POINT('',(-0.375800934160369,-0.578682691882343,0.75));
#52728=CARTESIAN_POINT('Origin',(-0.344527189490328,-0.580195253037085,
0.75));
#52729=CARTESIAN_POINT('',(-0.314411857106244,-0.568898219465488,0.75));
#52730=CARTESIAN_POINT('Origin',(0.,0.,0.75));
#52731=CARTESIAN_POINT('',(-0.315,-0.545596004384196,0.75));
#52732=CARTESIAN_POINT('Origin',(-0.315,-0.545596004384196,0.75));
#52733=CARTESIAN_POINT('',(-0.314411857106244,-0.568898219465488,0.0499999999999999));
#52734=CARTESIAN_POINT('',(-0.314411857106244,-0.568898219465488,0.39));
#52735=CARTESIAN_POINT('',(-0.315,-0.545596004384196,0.0499999999999999));
#52736=CARTESIAN_POINT('Origin',(-0.344527189490328,-0.580195253037085,
0.0499999999999999));
#52737=CARTESIAN_POINT('Origin',(0.,0.,0.0499999999999999));
#52738=CARTESIAN_POINT('Origin',(-0.551058501932632,-0.415252365974913,
0.75));
#52739=CARTESIAN_POINT('',(-0.505658331181079,-0.408423373605339,0.0499999999999999));
#52740=CARTESIAN_POINT('',(-0.505658331181079,-0.408423373605339,0.75));
#52741=CARTESIAN_POINT('',(-0.505658331181079,-0.408423373605339,0.39));
#52742=CARTESIAN_POINT('',(-0.482607999164956,-0.40495619410252,0.0499999999999999));
#52743=CARTESIAN_POINT('',(-0.551058501932632,-0.415252365974913,0.0499999999999999));
#52744=CARTESIAN_POINT('',(-0.482607999164956,-0.40495619410252,0.75));
#52745=CARTESIAN_POINT('',(-0.482607999164956,-0.40495619410252,0.75));
#52746=CARTESIAN_POINT('',(-0.551058501932632,-0.415252365974913,0.75));
#52747=CARTESIAN_POINT('Origin',(-0.516833250548794,-0.437767531272822,
0.75));
#52748=CARTESIAN_POINT('',(-0.490025152569635,-0.427054270379195,0.75));
#52749=CARTESIAN_POINT('Origin',(0.,0.,0.75));
#52750=CARTESIAN_POINT('',(-0.482607999164956,-0.40495619410252,0.75));
#52751=CARTESIAN_POINT('Origin',(-0.482607999164956,-0.40495619410252,0.75));
#52752=CARTESIAN_POINT('',(-0.490025152569635,-0.427054270379195,0.0499999999999999));
#52753=CARTESIAN_POINT('',(-0.490025152569635,-0.427054270379195,0.39));
#52754=CARTESIAN_POINT('',(-0.482607999164956,-0.40495619410252,0.0499999999999999));
#52755=CARTESIAN_POINT('Origin',(-0.516833250548794,-0.437767531272822,
0.0499999999999999));
#52756=CARTESIAN_POINT('Origin',(0.,0.,0.0499999999999999));
#52757=CARTESIAN_POINT('Origin',(-0.659850281614495,-0.201736476258688,
0.75));
#52758=CARTESIAN_POINT('',(-0.614852423227828,-0.210847095429052,0.0499999999999999));
#52759=CARTESIAN_POINT('',(-0.614852423227828,-0.210847095429052,0.75));
#52760=CARTESIAN_POINT('',(-0.614852423227828,-0.210847095429052,0.39));
#52761=CARTESIAN_POINT('',(-0.592006351095122,-0.215472690295171,0.0499999999999999));
#52762=CARTESIAN_POINT('',(-0.659850281614495,-0.201736476258688,0.0499999999999999));
#52763=CARTESIAN_POINT('',(-0.592006351095122,-0.215472690295171,0.75));
#52764=CARTESIAN_POINT('',(-0.592006351095122,-0.215472690295171,0.75));
#52765=CARTESIAN_POINT('',(-0.659850281614495,-0.201736476258688,0.75));
#52766=CARTESIAN_POINT('Origin',(-0.625928316354808,-0.235670477458144,
0.75));
#52767=CARTESIAN_POINT('',(-0.606534182632106,-0.23370127363539,0.75));
#52768=CARTESIAN_POINT('Origin',(0.,0.,0.75));
#52769=CARTESIAN_POINT('',(-0.592006351095122,-0.215472690295171,0.75));
#52770=CARTESIAN_POINT('Origin',(-0.592006351095122,-0.215472690295171,
0.75));
#52771=CARTESIAN_POINT('',(-0.606534182632106,-0.23370127363539,0.0499999999999999));
#52772=CARTESIAN_POINT('',(-0.606534182632106,-0.23370127363539,0.39));
#52773=CARTESIAN_POINT('',(-0.592006351095122,-0.215472690295171,0.0499999999999999));
#52774=CARTESIAN_POINT('Origin',(-0.625928316354808,-0.235670477458144,
0.0499999999999999));
#52775=CARTESIAN_POINT('Origin',(0.,0.,0.0499999999999999));
#52776=CARTESIAN_POINT('Origin',(-0.689054378980656,0.0361118098076312,
0.75));
#52777=CARTESIAN_POINT('',(-0.64988623877797,0.0121604542276944,0.0499999999999999));
#52778=CARTESIAN_POINT('',(-0.64988623877797,0.0121604542276944,0.75));
#52779=CARTESIAN_POINT('',(-0.64988623877797,0.0121604542276944,0.39));
#52780=CARTESIAN_POINT('',(-0.63,7.71527483462833E-17,0.0499999999999999));
#52781=CARTESIAN_POINT('',(-0.689054378980656,0.0361118098076312,0.0499999999999999));
#52782=CARTESIAN_POINT('',(-0.63,7.71527483462833E-17,0.75));
#52783=CARTESIAN_POINT('',(-0.63,7.71527483462833E-17,0.75));
#52784=CARTESIAN_POINT('',(-0.689054378980656,0.0361118098076312,0.75));
#52785=CARTESIAN_POINT('Origin',(-0.659527189490328,8.32667268468867E-17,
0.75));
#52786=CARTESIAN_POINT('',(-0.65,-7.9602041944578E-17,0.75));
#52787=CARTESIAN_POINT('Origin',(0.,0.,0.75));
#52788=CARTESIAN_POINT('',(-0.64988623877797,-0.0121604542276942,0.75));
#52789=CARTESIAN_POINT('',(-0.63,7.71527483462833E-17,0.75));
#52790=CARTESIAN_POINT('Origin',(0.,0.,0.75));
#52791=CARTESIAN_POINT('Origin',(-0.63,7.71527483462833E-17,0.75));
#52792=CARTESIAN_POINT('',(-0.64988623877797,-0.0121604542276942,0.0499999999999999));
#52793=CARTESIAN_POINT('',(-0.64988623877797,-0.0121604542276942,0.39));
#52794=CARTESIAN_POINT('',(-0.63,7.71527483462833E-17,0.0499999999999999));
#52795=CARTESIAN_POINT('Origin',(-0.659527189490328,8.32667268468867E-17,
0.0499999999999999));
#52796=CARTESIAN_POINT('',(-0.65,-7.9602041944578E-17,0.0499999999999999));
#52797=CARTESIAN_POINT('Origin',(0.,0.,0.0499999999999999));
#52798=CARTESIAN_POINT('Origin',(0.,0.,0.0499999999999999));
#52799=CARTESIAN_POINT('Origin',(-0.672315344701812,0.155216227497267,0.75));
#52800=CARTESIAN_POINT('',(-0.637901365808246,0.124827270658193,0.0499999999999999));
#52801=CARTESIAN_POINT('',(-0.637901365808246,0.124827270658193,0.75));
#52802=CARTESIAN_POINT('',(-0.637901365808246,0.124827270658193,0.39));
#52803=CARTESIAN_POINT('',(-0.620428884397691,0.109398351930166,0.0499999999999999));
#52804=CARTESIAN_POINT('',(-0.672315344701812,0.155216227497267,0.0499999999999999));
#52805=CARTESIAN_POINT('',(-0.620428884397691,0.109398351930166,0.75));
#52806=CARTESIAN_POINT('',(-0.620428884397691,0.109398351930166,0.75));
#52807=CARTESIAN_POINT('',(-0.672315344701812,0.155216227497267,0.75));
#52808=CARTESIAN_POINT('Origin',(-0.652642864515102,0.119653037223409,0.75));
#52809=CARTESIAN_POINT('',(-0.642124647240729,0.100875851451027,0.75));
#52810=CARTESIAN_POINT('Origin',(0.,0.,0.75));
#52811=CARTESIAN_POINT('',(-0.620428884397691,0.109398351930166,0.75));
#52812=CARTESIAN_POINT('Origin',(-0.620428884397691,0.109398351930166,0.75));
#52813=CARTESIAN_POINT('',(-0.642124647240729,0.100875851451027,0.0499999999999999));
#52814=CARTESIAN_POINT('',(-0.642124647240729,0.100875851451027,0.39));
#52815=CARTESIAN_POINT('',(-0.620428884397691,0.109398351930166,0.0499999999999999));
#52816=CARTESIAN_POINT('Origin',(-0.652642864515102,0.119653037223409,0.0499999999999999));
#52817=CARTESIAN_POINT('Origin',(0.,0.,0.0499999999999999));
#52818=CARTESIAN_POINT('Origin',(-0.578682691882343,0.375800934160369,0.75));
#52819=CARTESIAN_POINT('',(-0.556737765237794,0.335474381671726,0.0499999999999999));
#52820=CARTESIAN_POINT('',(-0.556737765237794,0.335474381671726,0.75));
#52821=CARTESIAN_POINT('',(-0.556737765237794,0.335474381671726,0.39));
#52822=CARTESIAN_POINT('',(-0.545596004384196,0.315,0.0499999999999999));
#52823=CARTESIAN_POINT('',(-0.578682691882343,0.375800934160369,0.0499999999999999));
#52824=CARTESIAN_POINT('',(-0.545596004384196,0.315,0.75));
#52825=CARTESIAN_POINT('',(-0.545596004384196,0.315,0.75));
#52826=CARTESIAN_POINT('',(-0.578682691882343,0.375800934160369,0.75));
#52827=CARTESIAN_POINT('Origin',(-0.580195253037085,0.344527189490328,0.75));
#52828=CARTESIAN_POINT('',(-0.568898219465488,0.314411857106244,0.75));
#52829=CARTESIAN_POINT('Origin',(0.,0.,0.75));
#52830=CARTESIAN_POINT('',(-0.545596004384196,0.315,0.75));
#52831=CARTESIAN_POINT('Origin',(-0.545596004384196,0.315,0.75));
#52832=CARTESIAN_POINT('',(-0.568898219465488,0.314411857106244,0.0499999999999999));
#52833=CARTESIAN_POINT('',(-0.568898219465488,0.314411857106244,0.39));
#52834=CARTESIAN_POINT('',(-0.545596004384196,0.315,0.0499999999999999));
#52835=CARTESIAN_POINT('Origin',(-0.580195253037085,0.344527189490328,0.0499999999999999));
#52836=CARTESIAN_POINT('Origin',(0.,0.,0.0499999999999999));
#52837=CARTESIAN_POINT('Origin',(-0.415252365974913,0.551058501932632,0.75));
#52838=CARTESIAN_POINT('',(-0.408423373605339,0.505658331181079,0.0499999999999999));
#52839=CARTESIAN_POINT('',(-0.408423373605339,0.505658331181079,0.75));
#52840=CARTESIAN_POINT('',(-0.408423373605339,0.505658331181079,0.39));
#52841=CARTESIAN_POINT('',(-0.40495619410252,0.482607999164956,0.0499999999999999));
#52842=CARTESIAN_POINT('',(-0.415252365974913,0.551058501932632,0.0499999999999999));
#52843=CARTESIAN_POINT('',(-0.40495619410252,0.482607999164956,0.75));
#52844=CARTESIAN_POINT('',(-0.40495619410252,0.482607999164956,0.75));
#52845=CARTESIAN_POINT('',(-0.415252365974913,0.551058501932632,0.75));
#52846=CARTESIAN_POINT('Origin',(-0.437767531272822,0.516833250548794,0.75));
#52847=CARTESIAN_POINT('',(-0.427054270379195,0.490025152569635,0.75));
#52848=CARTESIAN_POINT('Origin',(0.,0.,0.75));
#52849=CARTESIAN_POINT('',(-0.40495619410252,0.482607999164956,0.75));
#52850=CARTESIAN_POINT('Origin',(-0.40495619410252,0.482607999164956,0.75));
#52851=CARTESIAN_POINT('',(-0.427054270379195,0.490025152569635,0.0499999999999999));
#52852=CARTESIAN_POINT('',(-0.427054270379195,0.490025152569635,0.39));
#52853=CARTESIAN_POINT('',(-0.40495619410252,0.482607999164956,0.0499999999999999));
#52854=CARTESIAN_POINT('Origin',(-0.437767531272822,0.516833250548794,0.0499999999999999));
#52855=CARTESIAN_POINT('Origin',(0.,0.,0.0499999999999999));
#52856=CARTESIAN_POINT('Origin',(-0.201736476258688,0.659850281614495,0.75));
#52857=CARTESIAN_POINT('',(-0.210847095429052,0.614852423227828,0.0499999999999999));
#52858=CARTESIAN_POINT('',(-0.210847095429052,0.614852423227828,0.75));
#52859=CARTESIAN_POINT('',(-0.210847095429052,0.614852423227828,0.39));
#52860=CARTESIAN_POINT('',(-0.215472690295171,0.592006351095122,0.0499999999999999));
#52861=CARTESIAN_POINT('',(-0.201736476258688,0.659850281614495,0.0499999999999999));
#52862=CARTESIAN_POINT('',(-0.215472690295171,0.592006351095122,0.75));
#52863=CARTESIAN_POINT('',(-0.215472690295171,0.592006351095122,0.75));
#52864=CARTESIAN_POINT('',(-0.201736476258688,0.659850281614495,0.75));
#52865=CARTESIAN_POINT('Origin',(-0.235670477458144,0.625928316354808,0.75));
#52866=CARTESIAN_POINT('',(-0.23370127363539,0.606534182632106,0.75));
#52867=CARTESIAN_POINT('Origin',(0.,0.,0.75));
#52868=CARTESIAN_POINT('',(-0.215472690295171,0.592006351095122,0.75));
#52869=CARTESIAN_POINT('Origin',(-0.215472690295171,0.592006351095122,0.75));
#52870=CARTESIAN_POINT('',(-0.23370127363539,0.606534182632106,0.0499999999999999));
#52871=CARTESIAN_POINT('',(-0.23370127363539,0.606534182632106,0.39));
#52872=CARTESIAN_POINT('',(-0.215472690295171,0.592006351095122,0.0499999999999999));
#52873=CARTESIAN_POINT('Origin',(-0.235670477458144,0.625928316354808,0.0499999999999999));
#52874=CARTESIAN_POINT('Origin',(0.,0.,0.0499999999999999));
#52875=CARTESIAN_POINT('Origin',(0.0361118098076313,0.689054378980656,0.75));
#52876=CARTESIAN_POINT('',(0.0121604542276944,0.64988623877797,0.0499999999999999));
#52877=CARTESIAN_POINT('',(0.0121604542276944,0.64988623877797,0.75));
#52878=CARTESIAN_POINT('',(0.0121604542276944,0.64988623877797,0.39));
#52879=CARTESIAN_POINT('',(3.85763741731416E-17,0.63,0.0499999999999999));
#52880=CARTESIAN_POINT('',(0.0361118098076313,0.689054378980656,0.0499999999999999));
#52881=CARTESIAN_POINT('',(3.85763741731416E-17,0.63,0.75));
#52882=CARTESIAN_POINT('',(3.85763741731416E-17,0.63,0.75));
#52883=CARTESIAN_POINT('',(0.0361118098076313,0.689054378980656,0.75));
#52884=CARTESIAN_POINT('Origin',(4.16333634234434E-17,0.659527189490328,
0.75));
#52885=CARTESIAN_POINT('',(-0.0121604542276943,0.64988623877797,0.75));
#52886=CARTESIAN_POINT('Origin',(0.,0.,0.75));
#52887=CARTESIAN_POINT('',(3.85763741731416E-17,0.63,0.75));
#52888=CARTESIAN_POINT('Origin',(3.85763741731416E-17,0.63,0.75));
#52889=CARTESIAN_POINT('',(-0.0121604542276943,0.64988623877797,0.0499999999999999));
#52890=CARTESIAN_POINT('',(-0.0121604542276943,0.64988623877797,0.39));
#52891=CARTESIAN_POINT('',(3.85763741731416E-17,0.63,0.0499999999999999));
#52892=CARTESIAN_POINT('Origin',(4.16333634234434E-17,0.659527189490328,
0.0499999999999999));
#52893=CARTESIAN_POINT('Origin',(0.,0.,0.0499999999999999));
#52894=CARTESIAN_POINT('Origin',(0.269604478657599,0.635148348882184,0.75));
#52895=CARTESIAN_POINT('',(0.23370127363539,0.606534182632106,0.0499999999999999));
#52896=CARTESIAN_POINT('',(0.23370127363539,0.606534182632106,0.75));
#52897=CARTESIAN_POINT('',(0.23370127363539,0.606534182632106,0.39));
#52898=CARTESIAN_POINT('',(0.215472690295171,0.592006351095122,0.0499999999999999));
#52899=CARTESIAN_POINT('',(0.269604478657599,0.635148348882184,0.0499999999999999));
#52900=CARTESIAN_POINT('',(0.215472690295171,0.592006351095122,0.75));
#52901=CARTESIAN_POINT('',(0.215472690295171,0.592006351095122,0.75));
#52902=CARTESIAN_POINT('',(0.269604478657599,0.635148348882184,0.75));
#52903=CARTESIAN_POINT('Origin',(0.235670477458144,0.625928316354808,0.75));
#52904=CARTESIAN_POINT('',(0.210847095429052,0.614852423227828,0.75));
#52905=CARTESIAN_POINT('Origin',(0.,0.,0.75));
#52906=CARTESIAN_POINT('',(0.215472690295171,0.592006351095122,0.75));
#52907=CARTESIAN_POINT('Origin',(0.215472690295171,0.592006351095122,0.75));
#52908=CARTESIAN_POINT('',(0.210847095429052,0.614852423227828,0.0499999999999999));
#52909=CARTESIAN_POINT('',(0.210847095429052,0.614852423227828,0.39));
#52910=CARTESIAN_POINT('',(0.215472690295171,0.592006351095122,0.0499999999999999));
#52911=CARTESIAN_POINT('Origin',(0.235670477458144,0.625928316354808,0.0499999999999999));
#52912=CARTESIAN_POINT('Origin',(0.,0.,0.0499999999999999));
#52913=CARTESIAN_POINT('Origin',(0.470578868443124,0.504634054117228,0.75));
#52914=CARTESIAN_POINT('',(0.427054270379195,0.490025152569635,0.0499999999999999));
#52915=CARTESIAN_POINT('',(0.427054270379195,0.490025152569635,0.75));
#52916=CARTESIAN_POINT('',(0.427054270379195,0.490025152569635,0.39));
#52917=CARTESIAN_POINT('',(0.40495619410252,0.482607999164956,0.0499999999999999));
#52918=CARTESIAN_POINT('',(0.470578868443124,0.504634054117228,0.0499999999999999));
#52919=CARTESIAN_POINT('',(0.40495619410252,0.482607999164956,0.75));
#52920=CARTESIAN_POINT('',(0.40495619410252,0.482607999164956,0.75));
#52921=CARTESIAN_POINT('',(0.470578868443124,0.504634054117228,0.75));
#52922=CARTESIAN_POINT('Origin',(0.437767531272822,0.516833250548794,0.75));
#52923=CARTESIAN_POINT('',(0.408423373605339,0.505658331181079,0.75));
#52924=CARTESIAN_POINT('Origin',(0.,0.,0.75));
#52925=CARTESIAN_POINT('',(0.40495619410252,0.482607999164956,0.75));
#52926=CARTESIAN_POINT('Origin',(0.40495619410252,0.482607999164956,0.75));
#52927=CARTESIAN_POINT('',(0.408423373605339,0.505658331181079,0.0499999999999999));
#52928=CARTESIAN_POINT('',(0.408423373605339,0.505658331181079,0.39));
#52929=CARTESIAN_POINT('',(0.40495619410252,0.482607999164956,0.0499999999999999));
#52930=CARTESIAN_POINT('Origin',(0.437767531272822,0.516833250548794,0.0499999999999999));
#52931=CARTESIAN_POINT('Origin',(0.,0.,0.0499999999999999));
#52932=CARTESIAN_POINT('Origin',(0.614794501689974,0.313253444820287,0.75));
#52933=CARTESIAN_POINT('',(0.568898219465489,0.314411857106244,0.0499999999999999));
#52934=CARTESIAN_POINT('',(0.568898219465489,0.314411857106244,0.75));
#52935=CARTESIAN_POINT('',(0.568898219465489,0.314411857106244,0.39));
#52936=CARTESIAN_POINT('',(0.545596004384196,0.315,0.0499999999999999));
#52937=CARTESIAN_POINT('',(0.614794501689974,0.313253444820287,0.0499999999999999));
#52938=CARTESIAN_POINT('',(0.545596004384196,0.315,0.75));
#52939=CARTESIAN_POINT('',(0.545596004384196,0.315,0.75));
#52940=CARTESIAN_POINT('',(0.614794501689974,0.313253444820287,0.75));
#52941=CARTESIAN_POINT('Origin',(0.580195253037085,0.344527189490328,0.75));
#52942=CARTESIAN_POINT('',(0.556737765237794,0.335474381671726,0.75));
#52943=CARTESIAN_POINT('Origin',(0.,0.,0.75));
#52944=CARTESIAN_POINT('',(0.545596004384196,0.315,0.75));
#52945=CARTESIAN_POINT('Origin',(0.545596004384196,0.315,0.75));
#52946=CARTESIAN_POINT('',(0.556737765237794,0.335474381671726,0.0499999999999999));
#52947=CARTESIAN_POINT('',(0.556737765237794,0.335474381671726,0.39));
#52948=CARTESIAN_POINT('',(0.545596004384196,0.315,0.0499999999999999));
#52949=CARTESIAN_POINT('Origin',(0.580195253037085,0.344527189490328,0.0499999999999999));
#52950=CARTESIAN_POINT('Origin',(0.,0.,0.0499999999999999));
#52951=CARTESIAN_POINT('Origin',(0.684856844632512,0.0840898469495518,0.75));
#52952=CARTESIAN_POINT('',(0.642124647240729,0.100875851451026,0.0499999999999999));
#52953=CARTESIAN_POINT('',(0.642124647240729,0.100875851451026,0.75));
#52954=CARTESIAN_POINT('',(0.642124647240729,0.100875851451026,0.39));
#52955=CARTESIAN_POINT('',(0.620428884397691,0.109398351930166,0.0499999999999999));
#52956=CARTESIAN_POINT('',(0.684856844632512,0.0840898469495518,0.0499999999999999));
#52957=CARTESIAN_POINT('',(0.620428884397691,0.109398351930166,0.75));
#52958=CARTESIAN_POINT('',(0.620428884397691,0.109398351930166,0.75));
#52959=CARTESIAN_POINT('',(0.684856844632512,0.0840898469495518,0.75));
#52960=CARTESIAN_POINT('Origin',(0.652642864515102,0.119653037223409,0.75));
#52961=CARTESIAN_POINT('',(0.637901365808246,0.124827270658193,0.75));
#52962=CARTESIAN_POINT('Origin',(0.,0.,0.75));
#52963=CARTESIAN_POINT('',(0.620428884397691,0.109398351930166,0.75));
#52964=CARTESIAN_POINT('Origin',(0.620428884397691,0.109398351930166,0.75));
#52965=CARTESIAN_POINT('',(0.637901365808246,0.124827270658193,0.0499999999999999));
#52966=CARTESIAN_POINT('',(0.637901365808246,0.124827270658193,0.39));
#52967=CARTESIAN_POINT('',(0.620428884397691,0.109398351930166,0.0499999999999999));
#52968=CARTESIAN_POINT('Origin',(0.652642864515102,0.119653037223409,0.0499999999999999));
#52969=CARTESIAN_POINT('Origin',(0.,0.,0.0499999999999999));
#52970=CARTESIAN_POINT('Origin',(0.659850281614495,0.201736476258688,0.75));
#52971=CARTESIAN_POINT('',(0.614852423227828,0.210847095429052,0.0499999999999999));
#52972=CARTESIAN_POINT('',(0.614852423227828,0.210847095429052,0.75));
#52973=CARTESIAN_POINT('',(0.614852423227828,0.210847095429052,0.39));
#52974=CARTESIAN_POINT('',(0.592006351095122,0.215472690295171,0.0499999999999999));
#52975=CARTESIAN_POINT('',(0.659850281614495,0.201736476258688,0.0499999999999999));
#52976=CARTESIAN_POINT('',(0.592006351095122,0.215472690295171,0.75));
#52977=CARTESIAN_POINT('',(0.592006351095122,0.215472690295171,0.75));
#52978=CARTESIAN_POINT('',(0.659850281614495,0.201736476258688,0.75));
#52979=CARTESIAN_POINT('Origin',(0.625928316354808,0.235670477458144,0.75));
#52980=CARTESIAN_POINT('',(0.606534182632106,0.23370127363539,0.75));
#52981=CARTESIAN_POINT('Origin',(0.,0.,0.75));
#52982=CARTESIAN_POINT('',(0.592006351095122,0.215472690295171,0.75));
#52983=CARTESIAN_POINT('Origin',(0.592006351095122,0.215472690295171,0.75));
#52984=CARTESIAN_POINT('',(0.606534182632106,0.23370127363539,0.0499999999999999));
#52985=CARTESIAN_POINT('',(0.606534182632106,0.23370127363539,0.39));
#52986=CARTESIAN_POINT('',(0.592006351095122,0.215472690295171,0.0499999999999999));
#52987=CARTESIAN_POINT('Origin',(0.625928316354808,0.235670477458144,0.0499999999999999));
#52988=CARTESIAN_POINT('Origin',(0.,0.,0.0499999999999999));
#52989=CARTESIAN_POINT('Origin',(0.551058501932632,0.415252365974913,0.75));
#52990=CARTESIAN_POINT('',(0.505658331181079,0.408423373605339,0.0499999999999999));
#52991=CARTESIAN_POINT('',(0.505658331181079,0.408423373605339,0.75));
#52992=CARTESIAN_POINT('',(0.505658331181079,0.408423373605339,0.39));
#52993=CARTESIAN_POINT('',(0.482607999164956,0.40495619410252,0.0499999999999999));
#52994=CARTESIAN_POINT('',(0.551058501932632,0.415252365974913,0.0499999999999999));
#52995=CARTESIAN_POINT('',(0.482607999164956,0.40495619410252,0.75));
#52996=CARTESIAN_POINT('',(0.482607999164956,0.40495619410252,0.75));
#52997=CARTESIAN_POINT('',(0.551058501932632,0.415252365974913,0.75));
#52998=CARTESIAN_POINT('Origin',(0.516833250548794,0.437767531272822,0.75));
#52999=CARTESIAN_POINT('',(0.490025152569635,0.427054270379194,0.75));
#53000=CARTESIAN_POINT('Origin',(0.,0.,0.75));
#53001=CARTESIAN_POINT('',(0.482607999164956,0.40495619410252,0.75));
#53002=CARTESIAN_POINT('Origin',(0.482607999164956,0.40495619410252,0.75));
#53003=CARTESIAN_POINT('',(0.490025152569635,0.427054270379194,0.0499999999999999));
#53004=CARTESIAN_POINT('',(0.490025152569635,0.427054270379194,0.39));
#53005=CARTESIAN_POINT('',(0.482607999164956,0.40495619410252,0.0499999999999999));
#53006=CARTESIAN_POINT('Origin',(0.516833250548794,0.437767531272822,0.0499999999999999));
#53007=CARTESIAN_POINT('Origin',(0.,0.,0.0499999999999999));
#53008=CARTESIAN_POINT('Origin',(0.375800934160369,0.578682691882343,0.75));
#53009=CARTESIAN_POINT('',(0.335474381671726,0.556737765237794,0.0499999999999999));
#53010=CARTESIAN_POINT('',(0.335474381671726,0.556737765237794,0.75));
#53011=CARTESIAN_POINT('',(0.335474381671726,0.556737765237794,0.39));
#53012=CARTESIAN_POINT('',(0.315,0.545596004384196,0.0499999999999999));
#53013=CARTESIAN_POINT('',(0.375800934160369,0.578682691882343,0.0499999999999999));
#53014=CARTESIAN_POINT('',(0.315,0.545596004384196,0.75));
#53015=CARTESIAN_POINT('',(0.315,0.545596004384196,0.75));
#53016=CARTESIAN_POINT('',(0.375800934160369,0.578682691882343,0.75));
#53017=CARTESIAN_POINT('Origin',(0.344527189490328,0.580195253037085,0.75));
#53018=CARTESIAN_POINT('',(0.314411857106244,0.568898219465488,0.75));
#53019=CARTESIAN_POINT('Origin',(0.,0.,0.75));
#53020=CARTESIAN_POINT('',(0.315,0.545596004384196,0.75));
#53021=CARTESIAN_POINT('Origin',(0.315,0.545596004384196,0.75));
#53022=CARTESIAN_POINT('',(0.314411857106244,0.568898219465488,0.0499999999999999));
#53023=CARTESIAN_POINT('',(0.314411857106244,0.568898219465488,0.39));
#53024=CARTESIAN_POINT('',(0.315,0.545596004384196,0.0499999999999999));
#53025=CARTESIAN_POINT('Origin',(0.344527189490328,0.580195253037085,0.0499999999999999));
#53026=CARTESIAN_POINT('Origin',(0.,0.,0.0499999999999999));
#53027=CARTESIAN_POINT('Origin',(0.155216227497267,0.672315344701812,0.75));
#53028=CARTESIAN_POINT('',(0.124827270658193,0.637901365808246,0.0499999999999999));
#53029=CARTESIAN_POINT('',(0.124827270658193,0.637901365808246,0.75));
#53030=CARTESIAN_POINT('',(0.124827270658193,0.637901365808246,0.39));
#53031=CARTESIAN_POINT('',(0.109398351930166,0.620428884397691,0.0499999999999999));
#53032=CARTESIAN_POINT('',(0.155216227497267,0.672315344701812,0.0499999999999999));
#53033=CARTESIAN_POINT('',(0.109398351930166,0.620428884397691,0.75));
#53034=CARTESIAN_POINT('',(0.109398351930166,0.620428884397691,0.75));
#53035=CARTESIAN_POINT('',(0.155216227497267,0.672315344701812,0.75));
#53036=CARTESIAN_POINT('Origin',(0.119653037223409,0.652642864515102,0.75));
#53037=CARTESIAN_POINT('',(0.100875851451027,0.642124647240729,0.75));
#53038=CARTESIAN_POINT('Origin',(0.,0.,0.75));
#53039=CARTESIAN_POINT('',(0.109398351930166,0.620428884397691,0.75));
#53040=CARTESIAN_POINT('Origin',(0.109398351930166,0.620428884397691,0.75));
#53041=CARTESIAN_POINT('',(0.100875851451027,0.642124647240729,0.0499999999999999));
#53042=CARTESIAN_POINT('',(0.100875851451027,0.642124647240729,0.39));
#53043=CARTESIAN_POINT('',(0.109398351930166,0.620428884397691,0.0499999999999999));
#53044=CARTESIAN_POINT('Origin',(0.119653037223409,0.652642864515102,0.0499999999999999));
#53045=CARTESIAN_POINT('Origin',(0.,0.,0.0499999999999999));
#53046=CARTESIAN_POINT('Origin',(-0.0840898469495517,0.684856844632512,
0.75));
#53047=CARTESIAN_POINT('',(-0.100875851451027,0.642124647240729,0.0499999999999999));
#53048=CARTESIAN_POINT('',(-0.100875851451027,0.642124647240729,0.75));
#53049=CARTESIAN_POINT('',(-0.100875851451026,0.642124647240729,0.39));
#53050=CARTESIAN_POINT('',(-0.109398351930166,0.620428884397691,0.0499999999999999));
#53051=CARTESIAN_POINT('',(-0.0840898469495517,0.684856844632512,0.0499999999999999));
#53052=CARTESIAN_POINT('',(-0.109398351930166,0.620428884397691,0.75));
#53053=CARTESIAN_POINT('',(-0.109398351930166,0.620428884397691,0.75));
#53054=CARTESIAN_POINT('',(-0.0840898469495517,0.684856844632512,0.75));
#53055=CARTESIAN_POINT('Origin',(-0.119653037223409,0.652642864515102,0.75));
#53056=CARTESIAN_POINT('',(-0.124827270658193,0.637901365808246,0.75));
#53057=CARTESIAN_POINT('Origin',(0.,0.,0.75));
#53058=CARTESIAN_POINT('',(-0.109398351930166,0.620428884397691,0.75));
#53059=CARTESIAN_POINT('Origin',(-0.109398351930166,0.620428884397691,0.75));
#53060=CARTESIAN_POINT('',(-0.124827270658193,0.637901365808246,0.0499999999999999));
#53061=CARTESIAN_POINT('',(-0.124827270658193,0.637901365808246,0.39));
#53062=CARTESIAN_POINT('',(-0.109398351930166,0.620428884397691,0.0499999999999999));
#53063=CARTESIAN_POINT('Origin',(-0.119653037223409,0.652642864515102,0.0499999999999999));
#53064=CARTESIAN_POINT('Origin',(0.,0.,0.0499999999999999));
#53065=CARTESIAN_POINT('Origin',(-0.313253444820287,0.614794501689974,0.75));
#53066=CARTESIAN_POINT('',(-0.314411857106243,0.568898219465489,0.0499999999999999));
#53067=CARTESIAN_POINT('',(-0.314411857106243,0.568898219465489,0.75));
#53068=CARTESIAN_POINT('',(-0.314411857106243,0.568898219465489,0.39));
#53069=CARTESIAN_POINT('',(-0.315,0.545596004384196,0.0499999999999999));
#53070=CARTESIAN_POINT('',(-0.313253444820287,0.614794501689974,0.0499999999999999));
#53071=CARTESIAN_POINT('',(-0.315,0.545596004384196,0.75));
#53072=CARTESIAN_POINT('',(-0.315,0.545596004384196,0.75));
#53073=CARTESIAN_POINT('',(-0.313253444820287,0.614794501689974,0.75));
#53074=CARTESIAN_POINT('Origin',(-0.344527189490328,0.580195253037085,0.75));
#53075=CARTESIAN_POINT('',(-0.335474381671726,0.556737765237794,0.75));
#53076=CARTESIAN_POINT('Origin',(0.,0.,0.75));
#53077=CARTESIAN_POINT('',(-0.315,0.545596004384196,0.75));
#53078=CARTESIAN_POINT('Origin',(-0.315,0.545596004384196,0.75));
#53079=CARTESIAN_POINT('',(-0.335474381671726,0.556737765237794,0.0499999999999999));
#53080=CARTESIAN_POINT('',(-0.335474381671726,0.556737765237794,0.39));
#53081=CARTESIAN_POINT('',(-0.315,0.545596004384196,0.0499999999999999));
#53082=CARTESIAN_POINT('Origin',(-0.344527189490328,0.580195253037085,0.0499999999999999));
#53083=CARTESIAN_POINT('Origin',(0.,0.,0.0499999999999999));
#53084=CARTESIAN_POINT('Origin',(-0.504634054117228,0.470578868443124,0.75));
#53085=CARTESIAN_POINT('',(-0.490025152569635,0.427054270379195,0.0499999999999999));
#53086=CARTESIAN_POINT('',(-0.490025152569635,0.427054270379195,0.75));
#53087=CARTESIAN_POINT('',(-0.490025152569635,0.427054270379195,0.39));
#53088=CARTESIAN_POINT('',(-0.482607999164956,0.40495619410252,0.0499999999999999));
#53089=CARTESIAN_POINT('',(-0.504634054117228,0.470578868443124,0.0499999999999999));
#53090=CARTESIAN_POINT('',(-0.482607999164956,0.40495619410252,0.75));
#53091=CARTESIAN_POINT('',(-0.482607999164956,0.40495619410252,0.75));
#53092=CARTESIAN_POINT('',(-0.504634054117228,0.470578868443124,0.75));
#53093=CARTESIAN_POINT('Origin',(-0.516833250548794,0.437767531272822,0.75));
#53094=CARTESIAN_POINT('',(-0.505658331181079,0.408423373605339,0.75));
#53095=CARTESIAN_POINT('Origin',(0.,0.,0.75));
#53096=CARTESIAN_POINT('',(-0.482607999164956,0.40495619410252,0.75));
#53097=CARTESIAN_POINT('Origin',(-0.482607999164956,0.40495619410252,0.75));
#53098=CARTESIAN_POINT('',(-0.505658331181079,0.408423373605339,0.0499999999999999));
#53099=CARTESIAN_POINT('',(-0.505658331181079,0.408423373605339,0.39));
#53100=CARTESIAN_POINT('',(-0.482607999164956,0.40495619410252,0.0499999999999999));
#53101=CARTESIAN_POINT('Origin',(-0.516833250548794,0.437767531272822,0.0499999999999999));
#53102=CARTESIAN_POINT('Origin',(0.,0.,0.0499999999999999));
#53103=CARTESIAN_POINT('Origin',(-0.635148348882184,0.269604478657599,0.75));
#53104=CARTESIAN_POINT('',(-0.606534182632106,0.23370127363539,0.0499999999999999));
#53105=CARTESIAN_POINT('',(-0.606534182632106,0.23370127363539,0.75));
#53106=CARTESIAN_POINT('',(-0.606534182632106,0.23370127363539,0.39));
#53107=CARTESIAN_POINT('',(-0.592006351095122,0.215472690295171,0.0499999999999999));
#53108=CARTESIAN_POINT('',(-0.635148348882184,0.269604478657599,0.0499999999999999));
#53109=CARTESIAN_POINT('',(-0.592006351095122,0.215472690295171,0.75));
#53110=CARTESIAN_POINT('',(-0.592006351095122,0.215472690295171,0.75));
#53111=CARTESIAN_POINT('',(-0.635148348882184,0.269604478657599,0.75));
#53112=CARTESIAN_POINT('Origin',(-0.625928316354808,0.235670477458144,0.75));
#53113=CARTESIAN_POINT('',(-0.614852423227828,0.210847095429052,0.75));
#53114=CARTESIAN_POINT('Origin',(0.,0.,0.75));
#53115=CARTESIAN_POINT('',(-0.592006351095122,0.215472690295171,0.75));
#53116=CARTESIAN_POINT('Origin',(-0.592006351095122,0.215472690295171,0.75));
#53117=CARTESIAN_POINT('',(-0.614852423227828,0.210847095429052,0.0499999999999999));
#53118=CARTESIAN_POINT('',(-0.614852423227828,0.210847095429052,0.39));
#53119=CARTESIAN_POINT('',(-0.592006351095122,0.215472690295171,0.0499999999999999));
#53120=CARTESIAN_POINT('Origin',(-0.625928316354808,0.235670477458144,0.0499999999999999));
#53121=CARTESIAN_POINT('Origin',(0.,0.,0.0499999999999999));
#53122=CARTESIAN_POINT('Origin',(0.659527189490328,0.,0.75));
#53123=CARTESIAN_POINT('',(0.64988623877797,-0.0121604542276943,0.75));
#53124=CARTESIAN_POINT('',(0.64988623877797,0.0121604542276944,0.75));
#53125=CARTESIAN_POINT('Origin',(0.,0.,0.75));
#53126=CARTESIAN_POINT('',(0.63,0.,0.75));
#53127=CARTESIAN_POINT('',(0.689054378980656,-0.0361118098076312,0.75));
#53128=CARTESIAN_POINT('',(0.63,0.,0.75));
#53129=CARTESIAN_POINT('Origin',(0.689054378980656,-0.0361118098076312,
0.75));
#53130=CARTESIAN_POINT('',(0.64988623877797,-0.0121604542276943,0.0499999999999999));
#53131=CARTESIAN_POINT('',(0.64988623877797,-0.0121604542276943,0.39));
#53132=CARTESIAN_POINT('',(0.63,0.,0.0499999999999999));
#53133=CARTESIAN_POINT('',(0.689054378980656,-0.0361118098076312,0.0499999999999999));
#53134=CARTESIAN_POINT('',(0.63,0.,0.75));
#53135=CARTESIAN_POINT('Origin',(0.63,0.,0.75));
#53136=CARTESIAN_POINT('',(0.64988623877797,0.0121604542276944,0.0499999999999999));
#53137=CARTESIAN_POINT('',(0.64988623877797,0.0121604542276944,0.39));
#53138=CARTESIAN_POINT('',(0.63,0.,0.0499999999999999));
#53139=CARTESIAN_POINT('Origin',(0.659527189490328,0.,0.0499999999999999));
#53140=CARTESIAN_POINT('Origin',(0.,0.,0.0499999999999999));
#53141=CARTESIAN_POINT('Origin',(-0.684856844632512,-0.0840898469495517,
0.75));
#53142=CARTESIAN_POINT('',(-0.642124647240729,-0.100875851451027,0.0499999999999999));
#53143=CARTESIAN_POINT('',(-0.642124647240729,-0.100875851451027,0.75));
#53144=CARTESIAN_POINT('',(-0.642124647240729,-0.100875851451027,0.39));
#53145=CARTESIAN_POINT('',(-0.620428884397691,-0.109398351930166,0.0499999999999999));
#53146=CARTESIAN_POINT('',(-0.684856844632512,-0.0840898469495517,0.0499999999999999));
#53147=CARTESIAN_POINT('',(-0.620428884397691,-0.109398351930166,0.75));
#53148=CARTESIAN_POINT('',(-0.620428884397691,-0.109398351930166,0.75));
#53149=CARTESIAN_POINT('',(-0.684856844632512,-0.0840898469495517,0.75));
#53150=CARTESIAN_POINT('Origin',(-0.652642864515102,-0.119653037223409,
0.75));
#53151=CARTESIAN_POINT('',(-0.637901365808246,-0.124827270658193,0.75));
#53152=CARTESIAN_POINT('Origin',(0.,0.,0.75));
#53153=CARTESIAN_POINT('',(-0.620428884397691,-0.109398351930166,0.75));
#53154=CARTESIAN_POINT('Origin',(-0.620428884397691,-0.109398351930166,
0.75));
#53155=CARTESIAN_POINT('',(-0.637901365808246,-0.124827270658193,0.0499999999999999));
#53156=CARTESIAN_POINT('',(-0.637901365808246,-0.124827270658193,0.39));
#53157=CARTESIAN_POINT('',(-0.620428884397691,-0.109398351930166,0.0499999999999999));
#53158=CARTESIAN_POINT('Origin',(-0.652642864515102,-0.119653037223409,
0.0499999999999999));
#53159=CARTESIAN_POINT('Origin',(0.,0.,0.0499999999999999));
#53160=CARTESIAN_POINT('Origin',(-0.614794501689974,-0.313253444820287,
0.75));
#53161=CARTESIAN_POINT('',(-0.568898219465488,-0.314411857106244,0.0499999999999999));
#53162=CARTESIAN_POINT('',(-0.568898219465488,-0.314411857106244,0.75));
#53163=CARTESIAN_POINT('',(-0.568898219465488,-0.314411857106244,0.39));
#53164=CARTESIAN_POINT('',(-0.545596004384196,-0.315,0.0499999999999999));
#53165=CARTESIAN_POINT('',(-0.614794501689974,-0.313253444820287,0.0499999999999999));
#53166=CARTESIAN_POINT('',(-0.545596004384196,-0.315,0.75));
#53167=CARTESIAN_POINT('',(-0.545596004384196,-0.315,0.75));
#53168=CARTESIAN_POINT('',(-0.614794501689974,-0.313253444820287,0.75));
#53169=CARTESIAN_POINT('Origin',(-0.580195253037085,-0.344527189490328,
0.75));
#53170=CARTESIAN_POINT('',(-0.556737765237794,-0.335474381671726,0.75));
#53171=CARTESIAN_POINT('Origin',(0.,0.,0.75));
#53172=CARTESIAN_POINT('',(-0.545596004384196,-0.315,0.75));
#53173=CARTESIAN_POINT('Origin',(-0.545596004384196,-0.315,0.75));
#53174=CARTESIAN_POINT('',(-0.556737765237794,-0.335474381671726,0.0499999999999999));
#53175=CARTESIAN_POINT('',(-0.556737765237794,-0.335474381671726,0.39));
#53176=CARTESIAN_POINT('',(-0.545596004384196,-0.315,0.0499999999999999));
#53177=CARTESIAN_POINT('Origin',(-0.580195253037085,-0.344527189490328,
0.0499999999999999));
#53178=CARTESIAN_POINT('Origin',(0.,0.,0.0499999999999999));
#53179=CARTESIAN_POINT('Origin',(-0.470578868443124,-0.504634054117228,
0.75));
#53180=CARTESIAN_POINT('',(-0.427054270379195,-0.490025152569635,0.0499999999999999));
#53181=CARTESIAN_POINT('',(-0.427054270379195,-0.490025152569635,0.75));
#53182=CARTESIAN_POINT('',(-0.427054270379195,-0.490025152569635,0.39));
#53183=CARTESIAN_POINT('',(-0.40495619410252,-0.482607999164956,0.0499999999999999));
#53184=CARTESIAN_POINT('',(-0.470578868443124,-0.504634054117228,0.0499999999999999));
#53185=CARTESIAN_POINT('',(-0.40495619410252,-0.482607999164956,0.75));
#53186=CARTESIAN_POINT('',(-0.40495619410252,-0.482607999164956,0.75));
#53187=CARTESIAN_POINT('',(-0.470578868443124,-0.504634054117228,0.75));
#53188=CARTESIAN_POINT('Origin',(-0.437767531272822,-0.516833250548794,
0.75));
#53189=CARTESIAN_POINT('',(-0.408423373605339,-0.505658331181079,0.75));
#53190=CARTESIAN_POINT('Origin',(0.,0.,0.75));
#53191=CARTESIAN_POINT('',(-0.40495619410252,-0.482607999164956,0.75));
#53192=CARTESIAN_POINT('Origin',(-0.40495619410252,-0.482607999164956,0.75));
#53193=CARTESIAN_POINT('',(-0.408423373605339,-0.505658331181079,0.0499999999999999));
#53194=CARTESIAN_POINT('',(-0.408423373605339,-0.505658331181079,0.39));
#53195=CARTESIAN_POINT('',(-0.40495619410252,-0.482607999164956,0.0499999999999999));
#53196=CARTESIAN_POINT('Origin',(-0.437767531272822,-0.516833250548794,
0.0499999999999999));
#53197=CARTESIAN_POINT('Origin',(0.,0.,0.0499999999999999));
#53198=CARTESIAN_POINT('Origin',(-0.269604478657599,-0.635148348882184,
0.75));
#53199=CARTESIAN_POINT('',(-0.23370127363539,-0.606534182632106,0.0499999999999999));
#53200=CARTESIAN_POINT('',(-0.23370127363539,-0.606534182632106,0.75));
#53201=CARTESIAN_POINT('',(-0.23370127363539,-0.606534182632106,0.39));
#53202=CARTESIAN_POINT('',(-0.215472690295171,-0.592006351095122,0.0499999999999999));
#53203=CARTESIAN_POINT('',(-0.269604478657599,-0.635148348882184,0.0499999999999999));
#53204=CARTESIAN_POINT('',(-0.215472690295171,-0.592006351095122,0.75));
#53205=CARTESIAN_POINT('',(-0.215472690295171,-0.592006351095122,0.75));
#53206=CARTESIAN_POINT('',(-0.269604478657599,-0.635148348882184,0.75));
#53207=CARTESIAN_POINT('Origin',(-0.235670477458144,-0.625928316354808,
0.75));
#53208=CARTESIAN_POINT('',(-0.210847095429052,-0.614852423227828,0.75));
#53209=CARTESIAN_POINT('Origin',(0.,0.,0.75));
#53210=CARTESIAN_POINT('',(-0.215472690295171,-0.592006351095122,0.75));
#53211=CARTESIAN_POINT('Origin',(-0.215472690295171,-0.592006351095122,
0.75));
#53212=CARTESIAN_POINT('',(-0.210847095429052,-0.614852423227828,0.0499999999999999));
#53213=CARTESIAN_POINT('',(-0.210847095429052,-0.614852423227828,0.39));
#53214=CARTESIAN_POINT('',(-0.215472690295171,-0.592006351095122,0.0499999999999999));
#53215=CARTESIAN_POINT('Origin',(-0.235670477458144,-0.625928316354808,
0.0499999999999999));
#53216=CARTESIAN_POINT('Origin',(0.,0.,0.0499999999999999));
#53217=CARTESIAN_POINT('Origin',(-0.0361118098076316,-0.689054378980656,
0.75));
#53218=CARTESIAN_POINT('',(-0.0121604542276945,-0.64988623877797,0.0499999999999999));
#53219=CARTESIAN_POINT('',(-0.0121604542276945,-0.64988623877797,0.75));
#53220=CARTESIAN_POINT('',(-0.0121604542276945,-0.64988623877797,0.39));
#53221=CARTESIAN_POINT('',(-1.15729122519425E-16,-0.63,0.0499999999999999));
#53222=CARTESIAN_POINT('',(-0.0361118098076316,-0.689054378980656,0.0499999999999999));
#53223=CARTESIAN_POINT('',(-1.15729122519425E-16,-0.63,0.75));
#53224=CARTESIAN_POINT('',(-1.15729122519425E-16,-0.63,0.75));
#53225=CARTESIAN_POINT('',(-0.0361118098076316,-0.689054378980656,0.75));
#53226=CARTESIAN_POINT('Origin',(-1.2490009027033E-16,-0.659527189490328,
0.75));
#53227=CARTESIAN_POINT('',(0.0121604542276944,-0.64988623877797,0.75));
#53228=CARTESIAN_POINT('Origin',(0.,0.,0.75));
#53229=CARTESIAN_POINT('',(-1.15729122519425E-16,-0.63,0.75));
#53230=CARTESIAN_POINT('Origin',(-1.15729122519425E-16,-0.63,0.75));
#53231=CARTESIAN_POINT('',(0.0121604542276944,-0.64988623877797,0.0499999999999999));
#53232=CARTESIAN_POINT('',(0.0121604542276944,-0.64988623877797,0.39));
#53233=CARTESIAN_POINT('',(-1.15729122519425E-16,-0.63,0.0499999999999999));
#53234=CARTESIAN_POINT('Origin',(-1.2490009027033E-16,-0.659527189490328,
0.0499999999999999));
#53235=CARTESIAN_POINT('Origin',(0.,0.,0.0499999999999999));
#53236=CARTESIAN_POINT('Origin',(0.201736476258688,-0.659850281614495,0.75));
#53237=CARTESIAN_POINT('',(0.210847095429052,-0.614852423227828,0.0499999999999999));
#53238=CARTESIAN_POINT('',(0.210847095429052,-0.614852423227828,0.75));
#53239=CARTESIAN_POINT('',(0.210847095429052,-0.614852423227828,0.39));
#53240=CARTESIAN_POINT('',(0.215472690295171,-0.592006351095122,0.0499999999999999));
#53241=CARTESIAN_POINT('',(0.201736476258688,-0.659850281614495,0.0499999999999999));
#53242=CARTESIAN_POINT('',(0.215472690295171,-0.592006351095122,0.75));
#53243=CARTESIAN_POINT('',(0.215472690295171,-0.592006351095122,0.75));
#53244=CARTESIAN_POINT('',(0.201736476258688,-0.659850281614495,0.75));
#53245=CARTESIAN_POINT('Origin',(0.235670477458144,-0.625928316354808,0.75));
#53246=CARTESIAN_POINT('',(0.23370127363539,-0.606534182632106,0.75));
#53247=CARTESIAN_POINT('Origin',(0.,0.,0.75));
#53248=CARTESIAN_POINT('',(0.215472690295171,-0.592006351095122,0.75));
#53249=CARTESIAN_POINT('Origin',(0.215472690295171,-0.592006351095122,0.75));
#53250=CARTESIAN_POINT('',(0.23370127363539,-0.606534182632106,0.0499999999999999));
#53251=CARTESIAN_POINT('',(0.23370127363539,-0.606534182632106,0.39));
#53252=CARTESIAN_POINT('',(0.215472690295171,-0.592006351095122,0.0499999999999999));
#53253=CARTESIAN_POINT('Origin',(0.235670477458144,-0.625928316354808,0.0499999999999999));
#53254=CARTESIAN_POINT('Origin',(0.,0.,0.0499999999999999));
#53255=CARTESIAN_POINT('Origin',(0.415252365974913,-0.551058501932632,0.75));
#53256=CARTESIAN_POINT('',(0.408423373605339,-0.505658331181079,0.0499999999999999));
#53257=CARTESIAN_POINT('',(0.408423373605339,-0.505658331181079,0.75));
#53258=CARTESIAN_POINT('',(0.408423373605339,-0.505658331181079,0.39));
#53259=CARTESIAN_POINT('',(0.40495619410252,-0.482607999164956,0.0499999999999999));
#53260=CARTESIAN_POINT('',(0.415252365974913,-0.551058501932632,0.0499999999999999));
#53261=CARTESIAN_POINT('',(0.40495619410252,-0.482607999164956,0.75));
#53262=CARTESIAN_POINT('',(0.40495619410252,-0.482607999164956,0.75));
#53263=CARTESIAN_POINT('',(0.415252365974913,-0.551058501932632,0.75));
#53264=CARTESIAN_POINT('Origin',(0.437767531272822,-0.516833250548794,0.75));
#53265=CARTESIAN_POINT('',(0.427054270379194,-0.490025152569635,0.75));
#53266=CARTESIAN_POINT('Origin',(0.,0.,0.75));
#53267=CARTESIAN_POINT('',(0.40495619410252,-0.482607999164956,0.75));
#53268=CARTESIAN_POINT('Origin',(0.40495619410252,-0.482607999164956,0.75));
#53269=CARTESIAN_POINT('',(0.427054270379194,-0.490025152569635,0.0499999999999999));
#53270=CARTESIAN_POINT('',(0.427054270379194,-0.490025152569635,0.39));
#53271=CARTESIAN_POINT('',(0.40495619410252,-0.482607999164956,0.0499999999999999));
#53272=CARTESIAN_POINT('Origin',(0.437767531272822,-0.516833250548794,0.0499999999999999));
#53273=CARTESIAN_POINT('Origin',(0.,0.,0.0499999999999999));
#53274=CARTESIAN_POINT('Origin',(0.578682691882343,-0.375800934160369,0.75));
#53275=CARTESIAN_POINT('',(0.556737765237794,-0.335474381671726,0.0499999999999999));
#53276=CARTESIAN_POINT('',(0.556737765237794,-0.335474381671726,0.75));
#53277=CARTESIAN_POINT('',(0.556737765237794,-0.335474381671726,0.39));
#53278=CARTESIAN_POINT('',(0.545596004384196,-0.315,0.0499999999999999));
#53279=CARTESIAN_POINT('',(0.578682691882343,-0.375800934160369,0.0499999999999999));
#53280=CARTESIAN_POINT('',(0.545596004384196,-0.315,0.75));
#53281=CARTESIAN_POINT('',(0.545596004384196,-0.315,0.75));
#53282=CARTESIAN_POINT('',(0.578682691882343,-0.375800934160369,0.75));
#53283=CARTESIAN_POINT('Origin',(0.580195253037085,-0.344527189490328,0.75));
#53284=CARTESIAN_POINT('',(0.568898219465488,-0.314411857106244,0.75));
#53285=CARTESIAN_POINT('Origin',(0.,0.,0.75));
#53286=CARTESIAN_POINT('',(0.545596004384196,-0.315,0.75));
#53287=CARTESIAN_POINT('Origin',(0.545596004384196,-0.315,0.75));
#53288=CARTESIAN_POINT('',(0.568898219465488,-0.314411857106244,0.0499999999999999));
#53289=CARTESIAN_POINT('',(0.568898219465488,-0.314411857106244,0.39));
#53290=CARTESIAN_POINT('',(0.545596004384196,-0.315,0.0499999999999999));
#53291=CARTESIAN_POINT('Origin',(0.580195253037085,-0.344527189490328,0.0499999999999999));
#53292=CARTESIAN_POINT('Origin',(0.,0.,0.0499999999999999));
#53293=CARTESIAN_POINT('Origin',(0.672315344701812,-0.155216227497267,0.75));
#53294=CARTESIAN_POINT('',(0.637901365808246,-0.124827270658194,0.0499999999999999));
#53295=CARTESIAN_POINT('',(0.637901365808246,-0.124827270658194,0.75));
#53296=CARTESIAN_POINT('',(0.637901365808246,-0.124827270658194,0.39));
#53297=CARTESIAN_POINT('',(0.620428884397691,-0.109398351930166,0.0499999999999999));
#53298=CARTESIAN_POINT('',(0.672315344701812,-0.155216227497267,0.0499999999999999));
#53299=CARTESIAN_POINT('',(0.620428884397691,-0.109398351930166,0.75));
#53300=CARTESIAN_POINT('',(0.620428884397691,-0.109398351930166,0.75));
#53301=CARTESIAN_POINT('',(0.672315344701812,-0.155216227497267,0.75));
#53302=CARTESIAN_POINT('Origin',(0.652642864515102,-0.119653037223409,0.75));
#53303=CARTESIAN_POINT('',(0.642124647240729,-0.100875851451027,0.75));
#53304=CARTESIAN_POINT('Origin',(0.,0.,0.75));
#53305=CARTESIAN_POINT('',(0.620428884397691,-0.109398351930166,0.75));
#53306=CARTESIAN_POINT('Origin',(0.620428884397691,-0.109398351930166,0.75));
#53307=CARTESIAN_POINT('',(0.642124647240729,-0.100875851451027,0.0499999999999999));
#53308=CARTESIAN_POINT('',(0.642124647240729,-0.100875851451027,0.39));
#53309=CARTESIAN_POINT('',(0.620428884397691,-0.109398351930166,0.0499999999999999));
#53310=CARTESIAN_POINT('Origin',(0.652642864515102,-0.119653037223409,0.0499999999999999));
#53311=CARTESIAN_POINT('Origin',(0.,0.,0.0499999999999999));
#53312=CARTESIAN_POINT('Origin',(0.35,0.,-2.));
#53313=CARTESIAN_POINT('',(-0.35,-4.28626379701574E-17,-2.));
#53314=CARTESIAN_POINT('Origin',(0.,0.,-2.));
#53315=CARTESIAN_POINT('Origin',(0.,0.,-1.975));
#53316=CARTESIAN_POINT('',(-0.375,-4.59242549680257E-17,-1.975));
#53317=CARTESIAN_POINT('Origin',(0.,0.,0.015));
#53318=CARTESIAN_POINT('',(-0.65,-7.9602041944578E-17,0.03));
#53319=CARTESIAN_POINT('Origin',(0.,0.,0.03));
#53320=CARTESIAN_POINT('',(-0.635,-7.77650717458569E-17,0.015));
#53321=CARTESIAN_POINT('Origin',(0.,0.,0.39));
#53322=CARTESIAN_POINT('Origin',(0.,0.,0.75));
#53323=CARTESIAN_POINT('Origin',(0.,0.,0.75));
#53324=CARTESIAN_POINT('Origin',(0.,0.,0.75));
#53325=CARTESIAN_POINT('Origin',(0.,0.,0.75));
#53326=CARTESIAN_POINT('Origin',(0.,0.,0.75));
#53327=CARTESIAN_POINT('Origin',(0.,0.,0.75));
#53328=CARTESIAN_POINT('Origin',(0.,0.,0.75));
#53329=CARTESIAN_POINT('Origin',(0.,0.,0.75));
#53330=CARTESIAN_POINT('Origin',(0.,0.,0.75));
#53331=CARTESIAN_POINT('Origin',(0.,0.,0.75));
#53332=CARTESIAN_POINT('Origin',(0.,0.,0.75));
#53333=CARTESIAN_POINT('Origin',(0.,0.,0.75));
#53334=CARTESIAN_POINT('Origin',(0.,0.,0.75));
#53335=CARTESIAN_POINT('Origin',(0.,0.,0.75));
#53336=CARTESIAN_POINT('Origin',(0.,0.,0.75));
#53337=CARTESIAN_POINT('Origin',(0.,0.,0.75));
#53338=CARTESIAN_POINT('',(-0.65,-7.9602041944578E-17,0.39));
#53339=CARTESIAN_POINT('Origin',(0.,0.,0.75));
#53340=CARTESIAN_POINT('Origin',(0.,0.,0.75));
#53341=CARTESIAN_POINT('Origin',(0.,0.,0.75));
#53342=CARTESIAN_POINT('Origin',(0.,0.,0.75));
#53343=CARTESIAN_POINT('Origin',(0.,0.,0.75));
#53344=CARTESIAN_POINT('Origin',(0.,0.,0.75));
#53345=CARTESIAN_POINT('Origin',(0.,0.,0.75));
#53346=CARTESIAN_POINT('Origin',(0.,0.,0.75));
#53347=CARTESIAN_POINT('Origin',(0.,0.,0.75));
#53348=CARTESIAN_POINT('Origin',(0.,0.,0.75));
#53349=CARTESIAN_POINT('Origin',(0.,0.,0.75));
#53350=CARTESIAN_POINT('Origin',(0.,0.,0.75));
#53351=CARTESIAN_POINT('Origin',(0.,0.,0.75));
#53352=CARTESIAN_POINT('Origin',(0.,0.,0.75));
#53353=CARTESIAN_POINT('Origin',(0.,0.,0.75));
#53354=CARTESIAN_POINT('Origin',(0.,0.,0.75));
#53355=CARTESIAN_POINT('Origin',(0.,0.,0.75));
#53356=CARTESIAN_POINT('Origin',(0.,0.,0.75));
#53357=CARTESIAN_POINT('Origin',(0.,0.,0.75));
#53358=CARTESIAN_POINT('Origin',(0.,0.,0.75));
#53359=CARTESIAN_POINT('Origin',(0.,0.,0.775));
#53360=CARTESIAN_POINT('',(-0.6,-7.34788079488412E-17,0.8));
#53361=CARTESIAN_POINT('Origin',(0.,0.,0.8));
#53362=CARTESIAN_POINT('',(-0.625,-7.65404249467096E-17,0.775));
#53363=CARTESIAN_POINT('Origin',(0.,0.,0.8));
#53364=CARTESIAN_POINT('',(0.,0.,0.));
#53365=CARTESIAN_POINT('Origin',(3.375,0.24,27.21));
#53366=CARTESIAN_POINT('',(2.25,0.23,27.2));
#53367=CARTESIAN_POINT('',(2.25,0.25,27.22));
#53368=CARTESIAN_POINT('',(2.25,0.23,27.2));
#53369=CARTESIAN_POINT('',(3.75,0.25,27.22));
#53370=CARTESIAN_POINT('',(3.375,0.25,27.22));
#53371=CARTESIAN_POINT('',(3.75,0.23,27.2));
#53372=CARTESIAN_POINT('',(3.75,0.25,27.22));
#53373=CARTESIAN_POINT('',(3.375,0.23,27.2));
#53374=CARTESIAN_POINT('Origin',(2.25,0.,27.21));
#53375=CARTESIAN_POINT('',(2.25,-0.23,27.2));
#53376=CARTESIAN_POINT('',(2.25,-0.25,27.22));
#53377=CARTESIAN_POINT('',(2.25,-0.23,27.2));
#53378=CARTESIAN_POINT('Origin',(2.25,0.,27.22));
#53379=CARTESIAN_POINT('Origin',(2.25,0.,27.2));
#53380=CARTESIAN_POINT('Origin',(2.625,-0.24,27.21));
#53381=CARTESIAN_POINT('',(3.75,-0.23,27.2));
#53382=CARTESIAN_POINT('',(3.75,-0.25,27.22));
#53383=CARTESIAN_POINT('',(3.75,-0.23,27.2));
#53384=CARTESIAN_POINT('',(2.625,-0.25,27.22));
#53385=CARTESIAN_POINT('',(2.625,-0.23,27.2));
#53386=CARTESIAN_POINT('Origin',(3.75,0.,27.21));
#53387=CARTESIAN_POINT('Origin',(3.75,0.,27.22));
#53388=CARTESIAN_POINT('Origin',(3.75,0.,27.2));
#53389=CARTESIAN_POINT('Origin',(3.75,0.,27.2));
#53390=CARTESIAN_POINT('',(3.75,0.25,27.675));
#53391=CARTESIAN_POINT('',(3.75,0.25,27.2));
#53392=CARTESIAN_POINT('',(3.75,-0.25,27.675));
#53393=CARTESIAN_POINT('Origin',(3.75,0.,27.675));
#53394=CARTESIAN_POINT('',(3.75,-0.25,27.2));
#53395=CARTESIAN_POINT('Origin',(3.75,0.25,27.2));
#53396=CARTESIAN_POINT('',(2.25,0.25,27.675));
#53397=CARTESIAN_POINT('',(2.25,0.25,27.2));
#53398=CARTESIAN_POINT('',(3.375,0.25,27.675));
#53399=CARTESIAN_POINT('Origin',(3.,0.,27.2));
#53400=CARTESIAN_POINT('Origin',(3.375,0.2375,27.6875));
#53401=CARTESIAN_POINT('',(2.25,0.225,27.7));
#53402=CARTESIAN_POINT('',(2.25,0.25,27.675));
#53403=CARTESIAN_POINT('',(3.75,0.225,27.7));
#53404=CARTESIAN_POINT('',(3.375,0.225,27.7));
#53405=CARTESIAN_POINT('',(3.75,0.225,27.7));
#53406=CARTESIAN_POINT('Origin',(2.25,0.,27.6875));
#53407=CARTESIAN_POINT('',(2.25,-0.25,27.675));
#53408=CARTESIAN_POINT('',(2.25,-0.225,27.7));
#53409=CARTESIAN_POINT('',(2.25,-0.25,27.675));
#53410=CARTESIAN_POINT('Origin',(2.25,0.,27.7));
#53411=CARTESIAN_POINT('Origin',(2.25,0.,27.675));
#53412=CARTESIAN_POINT('Origin',(2.625,-0.2375,27.6875));
#53413=CARTESIAN_POINT('',(3.75,-0.225,27.7));
#53414=CARTESIAN_POINT('',(3.75,-0.25,27.675));
#53415=CARTESIAN_POINT('',(2.625,-0.225,27.7));
#53416=CARTESIAN_POINT('',(2.625,-0.25,27.675));
#53417=CARTESIAN_POINT('Origin',(3.75,0.,27.6875));
#53418=CARTESIAN_POINT('Origin',(3.75,0.,27.7));
#53419=CARTESIAN_POINT('Origin',(2.25,0.,27.2));
#53420=CARTESIAN_POINT('',(2.25,-0.25,27.2));
#53421=CARTESIAN_POINT('Origin',(3.,0.,27.7));
#53422=CARTESIAN_POINT('Origin',(2.25,-0.25,27.2));
#53423=CARTESIAN_POINT('',(0.,0.,0.));
#53424=CARTESIAN_POINT('Origin',(33.5,0.,32.675));
#53425=CARTESIAN_POINT('',(32.9083243043092,1.51088532809041E-5,31.8980125192205));
#53426=CARTESIAN_POINT('',(32.9083297324002,6.33379116770168E-6,31.8728374807795));
#53427=CARTESIAN_POINT('',(32.908325,-7.2459289488551E-17,32.675));
#53428=CARTESIAN_POINT('',(33.7584027379629,0.532279281158053,31.841675));
#53429=CARTESIAN_POINT('Ctrl Pts',(32.9083243043092,1.51088532809041E-5,
31.8980125192205));
#53430=CARTESIAN_POINT('Ctrl Pts',(32.9083008607279,0.0232268401770754,
31.8969198589752));
#53431=CARTESIAN_POINT('Ctrl Pts',(32.9096409746213,0.0464358794039322,
31.8958271987299));
#53432=CARTESIAN_POINT('Ctrl Pts',(32.9123658196052,0.069481186711505,31.8947345384845));
#53433=CARTESIAN_POINT('Ctrl Pts',(32.9238691680684,0.166770464436772,31.8901217066986));
#53434=CARTESIAN_POINT('Ctrl Pts',(32.9600516776961,0.261141654707062,31.8855088749126));
#53435=CARTESIAN_POINT('Ctrl Pts',(33.0165384573284,0.341184074808894,31.8808960431267));
#53436=CARTESIAN_POINT('Ctrl Pts',(33.0730252369608,0.421226494910727,31.8762832113407));
#53437=CARTESIAN_POINT('Ctrl Pts',(33.1498162865978,0.486940144844102,31.8716703795547));
#53438=CARTESIAN_POINT('Ctrl Pts',(33.237626207759,0.530378954117449,31.8670575477688));
#53439=CARTESIAN_POINT('Ctrl Pts',(33.3254361289203,0.573817763390796,31.8624447159828));
#53440=CARTESIAN_POINT('Ctrl Pts',(33.4242649216058,0.594981732004116,31.8578318841968));
#53441=CARTESIAN_POINT('Ctrl Pts',(33.5221632259087,0.591312650760069,31.8532190524109));
#53442=CARTESIAN_POINT('Ctrl Pts',(33.6038298469235,0.588251908599479,31.8493710349406));
#53443=CARTESIAN_POINT('Ctrl Pts',(33.6848489530031,0.567910165439557,31.8455230174703));
#53444=CARTESIAN_POINT('Ctrl Pts',(33.7584134942914,0.532287118922753,31.841675));
#53445=CARTESIAN_POINT('',(33.2416080183656,0.532271443393358,31.841675));
#53446=CARTESIAN_POINT('Origin',(33.5,0.,31.841675));
#53447=CARTESIAN_POINT('Ctrl Pts',(33.2416080183656,0.532271443393365,31.841675));
#53448=CARTESIAN_POINT('Ctrl Pts',(33.1534539004746,0.4894768928049,31.846287831786));
#53449=CARTESIAN_POINT('Ctrl Pts',(33.0761864930348,0.42436482186366,31.8509006635719));
#53450=CARTESIAN_POINT('Ctrl Pts',(33.0191062520769,0.344757517693961,31.8555134953579));
#53451=CARTESIAN_POINT('Ctrl Pts',(32.962026011119,0.265150213524262,31.8601263271438));
#53452=CARTESIAN_POINT('Ctrl Pts',(32.925132936643,0.171047676126103,31.8647391589298));
#53453=CARTESIAN_POINT('Ctrl Pts',(32.9129020489814,0.0738474299101955,
31.8693519907158));
#53454=CARTESIAN_POINT('Ctrl Pts',(32.9098214657017,0.0493656865113986,
31.870513820737));
#53455=CARTESIAN_POINT('Ctrl Pts',(32.9083054039246,0.0246874304476675,
31.8716756507583));
#53456=CARTESIAN_POINT('Ctrl Pts',(32.9083297324002,6.33379116770168E-6,
31.8728374807795));
#53457=CARTESIAN_POINT('Origin',(33.5,0.,32.675));
#53458=CARTESIAN_POINT('',(32.908289309907,-1.06508462919264E-5,32.0730125192205));
#53459=CARTESIAN_POINT('',(32.9082856845956,-9.55217830049818E-6,32.0478374807795));
#53460=CARTESIAN_POINT('',(32.908325,-7.2459289488551E-17,32.675));
#53461=CARTESIAN_POINT('Ctrl Pts',(32.908289309907,-1.06508462919264E-5,
32.0730125192205));
#53462=CARTESIAN_POINT('Ctrl Pts',(32.9083616633977,0.0864776372948188,
32.0689405070734));
#53463=CARTESIAN_POINT('Ctrl Pts',(32.9275556115765,0.172996985137614,32.0648684949263));
#53464=CARTESIAN_POINT('Ctrl Pts',(32.9642820299513,0.251292277390749,32.0607964827792));
#53465=CARTESIAN_POINT('Ctrl Pts',(33.0058862256033,0.339986269390676,32.0561836509933));
#53466=CARTESIAN_POINT('Ctrl Pts',(33.0699892657986,0.418126600317315,32.0515708192073));
#53467=CARTESIAN_POINT('Ctrl Pts',(33.1488401604359,0.476264967414407,32.0469579874214));
#53468=CARTESIAN_POINT('Ctrl Pts',(33.2276910550732,0.534403334511499,32.0423451556354));
#53469=CARTESIAN_POINT('Ctrl Pts',(33.3212898041525,0.572539737779045,32.0377323238494));
#53470=CARTESIAN_POINT('Ctrl Pts',(33.4183189572484,0.586062931239154,32.0331194920635));
#53471=CARTESIAN_POINT('Ctrl Pts',(33.5153481103443,0.599586124699262,32.0285066602775));
#53472=CARTESIAN_POINT('Ctrl Pts',(33.6158076674569,0.588496108351934,32.0238938284915));
#53473=CARTESIAN_POINT('Ctrl Pts',(33.7075506067178,0.554133826567958,32.0192809967056));
#53474=CARTESIAN_POINT('Ctrl Pts',(33.7992935459788,0.519771544783983,32.0146681649196));
#53475=CARTESIAN_POINT('Ctrl Pts',(33.8823198673881,0.462136997563359,32.0100553331336));
#53476=CARTESIAN_POINT('Ctrl Pts',(33.9465904807604,0.38819903998265,32.0054425013477));
#53477=CARTESIAN_POINT('Ctrl Pts',(34.0108610941327,0.31426108240194,32.0008296695617));
#53478=CARTESIAN_POINT('Ctrl Pts',(34.0563759994678,0.224019714461143,31.9962168377758));
#53479=CARTESIAN_POINT('Ctrl Pts',(34.0776317827638,0.128386430639952,31.9916040059898));
#53480=CARTESIAN_POINT('Ctrl Pts',(34.0988875660599,0.032753146818763,31.9869911742038));
#53481=CARTESIAN_POINT('Ctrl Pts',(34.0958842273168,-0.0682720528828202,
31.9823783424179));
#53482=CARTESIAN_POINT('Ctrl Pts',(34.0689849134539,-0.16247375277057,31.9777655106319));
#53483=CARTESIAN_POINT('Ctrl Pts',(34.042085599591,-0.256675452658321,31.9731526788459));
#53484=CARTESIAN_POINT('Ctrl Pts',(33.9912903106084,-0.344053652732237,
31.96853984706));
#53485=CARTESIAN_POINT('Ctrl Pts',(33.9227409368074,-0.414043056023174,
31.963927015274));
#53486=CARTESIAN_POINT('Ctrl Pts',(33.8541915630064,-0.484032459314111,
31.9593141834881));
#53487=CARTESIAN_POINT('Ctrl Pts',(33.767888104387,-0.536633065822067,31.9547013517021));
#53488=CARTESIAN_POINT('Ctrl Pts',(33.6742659025346,-0.565484700043603,
31.9500885199161));
#53489=CARTESIAN_POINT('Ctrl Pts',(33.5806437006822,-0.594336334265139,
31.9454756881302));
#53490=CARTESIAN_POINT('Ctrl Pts',(33.4797027555968,-0.599438996200255,
31.9408628563442));
#53491=CARTESIAN_POINT('Ctrl Pts',(33.3836483003762,-0.580175692813326,
31.9362500245582));
#53492=CARTESIAN_POINT('Ctrl Pts',(33.2875938451557,-0.560912389426397,
31.9316371927722));
#53493=CARTESIAN_POINT('Ctrl Pts',(33.1964258798001,-0.517283120717423,
31.9270243609863));
#53494=CARTESIAN_POINT('Ctrl Pts',(33.1211679274723,-0.45456331459057,31.9224115292003));
#53495=CARTESIAN_POINT('Ctrl Pts',(33.0459099751446,-0.391843508463717,
31.9177986974144));
#53496=CARTESIAN_POINT('Ctrl Pts',(32.9865620358447,-0.310033164918984,
31.9131858656284));
#53497=CARTESIAN_POINT('Ctrl Pts',(32.9503001598441,-0.219024310556495,
31.9085730338424));
#53498=CARTESIAN_POINT('Ctrl Pts',(32.9226277820443,-0.149573094050218,
31.9050528623018));
#53499=CARTESIAN_POINT('Ctrl Pts',(32.9083998313799,-0.0747650219016244,
31.9015326907611));
#53500=CARTESIAN_POINT('Ctrl Pts',(32.9083243043092,1.51088532809041E-5,
31.8980125192205));
#53501=CARTESIAN_POINT('Ctrl Pts',(32.9083297324002,6.33379116770168E-6,
31.8728374807795));
#53502=CARTESIAN_POINT('Ctrl Pts',(32.9084019956493,-0.0733043111048681,
31.8762884825442));
#53503=CARTESIAN_POINT('Ctrl Pts',(32.9220647745795,-0.146640017910053,
31.879739484309));
#53504=CARTESIAN_POINT('Ctrl Pts',(32.9486856754287,-0.214925334208059,
31.8831904860737));
#53505=CARTESIAN_POINT('Ctrl Pts',(32.9842688903849,-0.306199897076748,
31.8878033178596));
#53506=CARTESIAN_POINT('Ctrl Pts',(33.0430040211446,-0.38845106778047,31.8924161496456));
#53507=CARTESIAN_POINT('Ctrl Pts',(33.1177920474854,-0.451729845779465,
31.8970289814316));
#53508=CARTESIAN_POINT('Ctrl Pts',(33.1925800738261,-0.515008623778459,
31.9016418132175));
#53509=CARTESIAN_POINT('Ctrl Pts',(33.2834209957479,-0.559315009072727,
31.9062546450035));
#53510=CARTESIAN_POINT('Ctrl Pts',(33.3793293742516,-0.579293076033512,
31.9108674767895));
#53511=CARTESIAN_POINT('Ctrl Pts',(33.4752377527552,-0.599271142994297,
31.9154803085754));
#53512=CARTESIAN_POINT('Ctrl Pts',(33.5762135878407,-0.5949208916216,31.9200931403614));
#53513=CARTESIAN_POINT('Ctrl Pts',(33.6700480416488,-0.566767599976771,
31.9247059721474));
#53514=CARTESIAN_POINT('Ctrl Pts',(33.7638824954568,-0.538614308331942,
31.9293188039333));
#53515=CARTESIAN_POINT('Ctrl Pts',(33.8505755679873,-0.486657976414981,
31.9339316357193));
#53516=CARTESIAN_POINT('Ctrl Pts',(33.9196445096566,-0.417181169157836,
31.9385444675052));
#53517=CARTESIAN_POINT('Ctrl Pts',(33.9887134513259,-0.34770436190069,31.9431572992912));
#53518=CARTESIAN_POINT('Ctrl Pts',(34.040158262134,-0.26070707930336,31.9477701310772));
#53519=CARTESIAN_POINT('Ctrl Pts',(34.0677586431681,-0.166708410595722,
31.9523829628631));
#53520=CARTESIAN_POINT('Ctrl Pts',(34.0953590242022,-0.0727097418880827,
31.9569957946491));
#53521=CARTESIAN_POINT('Ctrl Pts',(34.0991149754623,0.0282903129298638,
31.961608626435));
#53522=CARTESIAN_POINT('Ctrl Pts',(34.0785722872182,0.124079317210986,31.966221458221));
#53523=CARTESIAN_POINT('Ctrl Pts',(34.0580295989741,0.219868321492108,31.970834290007));
#53524=CARTESIAN_POINT('Ctrl Pts',(34.0131882712259,0.310446275236406,31.9754471217929));
#53525=CARTESIAN_POINT('Ctrl Pts',(33.9494702992662,0.384861016213016,31.9800599535789));
#53526=CARTESIAN_POINT('Ctrl Pts',(33.8857523273065,0.459275757189627,31.9846727853649));
#53527=CARTESIAN_POINT('Ctrl Pts',(33.8031577111352,0.517527285398551,31.9892856171508));
#53528=CARTESIAN_POINT('Ctrl Pts',(33.7116733289766,0.55257213095512,31.9938984489368));
#53529=CARTESIAN_POINT('Ctrl Pts',(33.620188946818,0.587616976511689,31.9985112807228));
#53530=CARTESIAN_POINT('Ctrl Pts',(33.519814798672,0.599455139415905,32.0031241125087));
#53531=CARTESIAN_POINT('Ctrl Pts',(33.4226875847438,0.586655219696921,32.0077369442947));
#53532=CARTESIAN_POINT('Ctrl Pts',(33.3255603708156,0.573855299977937,32.0123497760807));
#53533=CARTESIAN_POINT('Ctrl Pts',(33.2316800911052,0.536417297635754,32.0169626078666));
#53534=CARTESIAN_POINT('Ctrl Pts',(33.1523982346142,0.478868009142385,32.0215754396526));
#53535=CARTESIAN_POINT('Ctrl Pts',(33.0731163781232,0.421318720649017,32.0261882714386));
#53536=CARTESIAN_POINT('Ctrl Pts',(33.0084329448517,0.343658146004464,32.0308011032245));
#53537=CARTESIAN_POINT('Ctrl Pts',(32.9661691040117,0.255276579721552,32.0354139350105));
#53538=CARTESIAN_POINT('Ctrl Pts',(32.928226629236,0.175931795085864,32.0395551169335));
#53539=CARTESIAN_POINT('Ctrl Pts',(32.9083534448324,0.0879463221066194,
32.0436962988565));
#53540=CARTESIAN_POINT('Ctrl Pts',(32.9082856845956,-9.55217830049818E-6,
32.0478374807795));
#53541=CARTESIAN_POINT('Origin',(33.5,0.,32.675));
#53542=CARTESIAN_POINT('',(32.9083715657093,-2.56487800331939E-6,32.2480125192205));
#53543=CARTESIAN_POINT('',(32.9083706917437,-3.8834067794807E-6,32.2228374807795));
#53544=CARTESIAN_POINT('',(32.908325,-7.2459289488551E-17,32.675));
#53545=CARTESIAN_POINT('Ctrl Pts',(32.9083715657093,-2.56487800331939E-6,
32.2480125192205));
#53546=CARTESIAN_POINT('Ctrl Pts',(32.9083794549289,0.051811826723419,32.2455739869576));
#53547=CARTESIAN_POINT('Ctrl Pts',(32.9151197717928,0.103628232274518,32.2431354546947));
#53548=CARTESIAN_POINT('Ctrl Pts',(32.9285668248986,0.15364139579779,32.2406969224319));
#53549=CARTESIAN_POINT('Ctrl Pts',(32.95400384492,0.248248432140261,32.2360840906459));
#53550=CARTESIAN_POINT('Ctrl Pts',(33.0034396607516,0.336402905617286,32.2314712588599));
#53551=CARTESIAN_POINT('Ctrl Pts',(33.0708967630834,0.407445657943371,32.2268584270739));
#53552=CARTESIAN_POINT('Ctrl Pts',(33.1383538654153,0.478488410269457,32.222245595288));
#53553=CARTESIAN_POINT('Ctrl Pts',(33.2238322542474,0.532419441444603,32.217632763502));
#53554=CARTESIAN_POINT('Ctrl Pts',(33.3169963488586,0.562717705228931,32.2130199317161));
#53555=CARTESIAN_POINT('Ctrl Pts',(33.4101604434698,0.59301596901326,32.2084070999301));
#53556=CARTESIAN_POINT('Ctrl Pts',(33.5110102438602,0.599681465406771,32.2037942681441));
#53557=CARTESIAN_POINT('Ctrl Pts',(33.6073515420329,0.581908238928051,32.1991814363582));
#53558=CARTESIAN_POINT('Ctrl Pts',(33.7036928402057,0.564135012449331,32.1945686045722));
#53559=CARTESIAN_POINT('Ctrl Pts',(33.7955256361608,0.521923063098379,32.1899557727862));
#53560=CARTESIAN_POINT('Ctrl Pts',(33.8717460089143,0.460376429637208,32.1853429410003));
#53561=CARTESIAN_POINT('Ctrl Pts',(33.9479663816677,0.398829796176036,32.1807301092143));
#53562=CARTESIAN_POINT('Ctrl Pts',(34.0085743312194,0.317948478604645,32.1761172774283));
#53563=CARTESIAN_POINT('Ctrl Pts',(34.0462414747642,0.227512204852059,32.1715044456424));
#53564=CARTESIAN_POINT('Ctrl Pts',(34.083908618309,0.137075931099472,32.1668916138564));
#53565=CARTESIAN_POINT('Ctrl Pts',(34.0986349558468,0.0370847011656908,
32.1622787820704));
#53566=CARTESIAN_POINT('Ctrl Pts',(34.0886398589355,-0.0603710906109303,
32.1576659502845));
#53567=CARTESIAN_POINT('Ctrl Pts',(34.0786447620242,-0.157826882387551,
32.1530531184985));
#53568=CARTESIAN_POINT('Ctrl Pts',(34.0439282306638,-0.252747236007011,
32.1484402867126));
#53569=CARTESIAN_POINT('Ctrl Pts',(33.9886879985403,-0.33365489984686,32.1438274549266));
#53570=CARTESIAN_POINT('Ctrl Pts',(33.9334477664169,-0.414562563686709,
32.1392146231406));
#53571=CARTESIAN_POINT('Ctrl Pts',(33.8576838335303,-0.481457537746947,
32.1346017913547));
#53572=CARTESIAN_POINT('Ctrl Pts',(33.7705571615554,-0.526251246497627,
32.1299889595687));
#53573=CARTESIAN_POINT('Ctrl Pts',(33.6834304895804,-0.571044955248308,
32.1253761277827));
#53574=CARTESIAN_POINT('Ctrl Pts',(33.5849410785171,-0.59373739868943,32.1207632959968));
#53575=CARTESIAN_POINT('Ctrl Pts',(33.4869977309542,-0.59158473028704,32.1161504642108));
#53576=CARTESIAN_POINT('Ctrl Pts',(33.3890543833913,-0.58943206188465,32.1115376324249));
#53577=CARTESIAN_POINT('Ctrl Pts',(33.2916570993287,-0.562434281638749,
32.1069248006389));
#53578=CARTESIAN_POINT('Ctrl Pts',(33.2065826273135,-0.513855813935313,
32.1023119688529));
#53579=CARTESIAN_POINT('Ctrl Pts',(33.1215081552984,-0.465277346231876,
32.097699137067));
#53580=CARTESIAN_POINT('Ctrl Pts',(33.0487564953306,-0.395118191070904,
32.093086305281));
#53581=CARTESIAN_POINT('Ctrl Pts',(32.9971243814666,-0.311861610964698,
32.088473473495));
#53582=CARTESIAN_POINT('Ctrl Pts',(32.9454922676025,-0.228605030858492,
32.0838606417091));
#53583=CARTESIAN_POINT('Ctrl Pts',(32.9149796998423,-0.132251025807052,
32.0792478099231));
#53584=CARTESIAN_POINT('Ctrl Pts',(32.9092760915165,-0.0344501967447237,
32.0746349781371));
#53585=CARTESIAN_POINT('Ctrl Pts',(32.9086073865782,-0.0229837892296867,
32.0740941584983));
#53586=CARTESIAN_POINT('Ctrl Pts',(32.9082797003609,-0.0114974939771132,
32.0735533388594));
#53587=CARTESIAN_POINT('Ctrl Pts',(32.908289309907,-1.06508462919264E-5,
32.0730125192205));
#53588=CARTESIAN_POINT('Ctrl Pts',(32.9082856845956,-9.55217830049818E-6,
32.0478374807795));
#53589=CARTESIAN_POINT('Ctrl Pts',(32.908277967208,-0.0100270729788548,
32.0483091306425));
#53590=CARTESIAN_POINT('Ctrl Pts',(32.9085271562383,-0.02004420983941,32.0487807805054));
#53591=CARTESIAN_POINT('Ctrl Pts',(32.9090358165807,-0.0300481536284575,
32.0492524303684));
#53592=CARTESIAN_POINT('Ctrl Pts',(32.9140106183982,-0.127888762774285,
32.0538652621543));
#53593=CARTESIAN_POINT('Ctrl Pts',(32.9438044704417,-0.224467423144669,
32.0584780939403));
#53594=CARTESIAN_POINT('Ctrl Pts',(32.9948148628033,-0.308106369448236,
32.0630909257263));
#53595=CARTESIAN_POINT('Ctrl Pts',(33.0458252551648,-0.391745315751803,
32.0677037575122));
#53596=CARTESIAN_POINT('Ctrl Pts',(33.1180521878445,-0.462444547988551,
32.0723165892982));
#53597=CARTESIAN_POINT('Ctrl Pts',(33.2027623738394,-0.511655500586126,
32.0769294210842));
#53598=CARTESIAN_POINT('Ctrl Pts',(33.2874725598343,-0.560866453183702,
32.0815422528701));
#53599=CARTESIAN_POINT('Ctrl Pts',(33.3846659991445,-0.588589126142103,
32.0861550846561));
#53600=CARTESIAN_POINT('Ctrl Pts',(33.482590591068,-0.591471444947309,32.090767916442));
#53601=CARTESIAN_POINT('Ctrl Pts',(33.5805151829916,-0.594353763752514,
32.095380748228));
#53602=CARTESIAN_POINT('Ctrl Pts',(33.6791709275285,-0.572395728404524,
32.099993580014));
#53603=CARTESIAN_POINT('Ctrl Pts',(33.7666289099307,-0.528252384838784,
32.1046064117999));
#53604=CARTESIAN_POINT('Ctrl Pts',(33.854086892333,-0.484109041273043,32.1092192435859));
#53605=CARTESIAN_POINT('Ctrl Pts',(33.9303471126006,-0.417780389489552,
32.1138320753719));
#53606=CARTESIAN_POINT('Ctrl Pts',(33.9861886007049,-0.337286528405296,
32.1184449071578));
#53607=CARTESIAN_POINT('Ctrl Pts',(34.0420300888091,-0.256792667321041,
32.1230577389438));
#53608=CARTESIAN_POINT('Ctrl Pts',(34.07745284475,-0.162133596936023,32.1276705707298));
#53609=CARTESIAN_POINT('Ctrl Pts',(34.0881737420111,-0.0647549759335278,
32.1322834025157));
#53610=CARTESIAN_POINT('Ctrl Pts',(34.0988946392722,0.0326236450689678,
32.1368962343017));
#53611=CARTESIAN_POINT('Ctrl Pts',(34.0849136778535,0.132721816688942,32.1415090660877));
#53612=CARTESIAN_POINT('Ctrl Pts',(34.0479213593831,0.223436213784697,32.1461218978736));
#53613=CARTESIAN_POINT('Ctrl Pts',(34.0109290409127,0.314150610880454,32.1507347296596));
#53614=CARTESIAN_POINT('Ctrl Pts',(33.9509253653904,0.395481233451992,32.1553475614456));
#53615=CARTESIAN_POINT('Ctrl Pts',(33.8751656500997,0.457594026058407,32.1599603932315));
#53616=CARTESIAN_POINT('Ctrl Pts',(33.7994059348091,0.519706818664821,32.1645732250175));
#53617=CARTESIAN_POINT('Ctrl Pts',(33.7078901797499,0.562601781306112,32.1691860568034));
#53618=CARTESIAN_POINT('Ctrl Pts',(33.6116839710503,0.581092288977684,32.1737988885894));
#53619=CARTESIAN_POINT('Ctrl Pts',(33.5154777623508,0.599582796649255,32.1784117203754));
#53620=CARTESIAN_POINT('Ctrl Pts',(33.4145811000107,0.593668849351107,32.1830245521613));
#53621=CARTESIAN_POINT('Ctrl Pts',(33.3211938583182,0.564065529345526,32.1876373839473));
#53622=CARTESIAN_POINT('Ctrl Pts',(33.2278066166257,0.534462209339944,32.1922502157332));
#53623=CARTESIAN_POINT('Ctrl Pts',(33.1419287955807,0.481169516626928,32.1968630475192));
#53624=CARTESIAN_POINT('Ctrl Pts',(33.0739442730699,0.410631313040044,32.2014758793052));
#53625=CARTESIAN_POINT('Ctrl Pts',(33.005959750559,0.34009310945316,32.2060887110911));
#53626=CARTESIAN_POINT('Ctrl Pts',(32.9558685265822,0.252309394992407,32.2107015428771));
#53627=CARTESIAN_POINT('Ctrl Pts',(32.9297273588288,0.157894497784488,32.2153143746631));
#53628=CARTESIAN_POINT('Ctrl Pts',(32.9155160754537,0.106567148076506,32.2178220767019));
#53629=CARTESIAN_POINT('Ctrl Pts',(32.9083829975906,0.0532800169870548,
32.2203297787407));
#53630=CARTESIAN_POINT('Ctrl Pts',(32.9083706917437,-3.8834067794807E-6,
32.2228374807795));
#53631=CARTESIAN_POINT('Origin',(33.5,0.,32.675));
#53632=CARTESIAN_POINT('',(32.9083052712772,1.37854762840214E-5,32.4230125192205));
#53633=CARTESIAN_POINT('',(32.9083097907792,1.43029731956186E-5,32.3978374807795));
#53634=CARTESIAN_POINT('',(32.908325,-7.2459289488551E-17,32.675));
#53635=CARTESIAN_POINT('Ctrl Pts',(32.9083052712772,1.37854762840214E-5,
32.4230125192205));
#53636=CARTESIAN_POINT('Ctrl Pts',(32.9082882892976,0.017114184346715,32.4222074668418));
#53637=CARTESIAN_POINT('Ctrl Pts',(32.9090149389792,0.0342131447793152,
32.4214024144631));
#53638=CARTESIAN_POINT('Ctrl Pts',(32.9104956801375,0.0512465508369966,
32.4205973620844));
#53639=CARTESIAN_POINT('Ctrl Pts',(32.9189801093039,0.148845463611661,32.4159845302985));
#53640=CARTESIAN_POINT('Ctrl Pts',(32.9522222781642,0.244292146583959,32.4113716985125));
#53641=CARTESIAN_POINT('Ctrl Pts',(33.006202724907,0.326045707255768,32.4067588667265));
#53642=CARTESIAN_POINT('Ctrl Pts',(33.0601831716498,0.407799267927575,32.4021460349406));
#53643=CARTESIAN_POINT('Ctrl Pts',(33.1349018962753,0.475859706298894,32.3975332031546));
#53644=CARTESIAN_POINT('Ctrl Pts',(33.2213243179928,0.521997525249887,32.3929203713687));
#53645=CARTESIAN_POINT('Ctrl Pts',(33.3077467397103,0.56813534420088,32.3883075395827));
#53646=CARTESIAN_POINT('Ctrl Pts',(33.4058728585199,0.592350543731546,32.3836947077967));
#53647=CARTESIAN_POINT('Ctrl Pts',(33.5038377991512,0.591715153943916,32.3790818760108));
#53648=CARTESIAN_POINT('Ctrl Pts',(33.6018027397825,0.591079764156285,32.3744690442248));
#53649=CARTESIAN_POINT('Ctrl Pts',(33.6996065022355,0.565593785050359,32.3698562124388));
#53650=CARTESIAN_POINT('Ctrl Pts',(33.7854231888128,0.518338842261637,32.3652433806529));
#53651=CARTESIAN_POINT('Ctrl Pts',(33.8712398753901,0.471083899472915,32.3606305488669));
#53652=CARTESIAN_POINT('Ctrl Pts',(33.9450694860918,0.402059993001396,32.3560177170809));
#53653=CARTESIAN_POINT('Ctrl Pts',(33.9979849469352,0.319613117276449,32.351404885295));
#53654=CARTESIAN_POINT('Ctrl Pts',(34.0509004077786,0.2371662415515,32.346792053509));
#53655=CARTESIAN_POINT('Ctrl Pts',(34.0829017187637,0.141296396573124,32.342179221723));
#53656=CARTESIAN_POINT('Ctrl Pts',(34.0901194558481,0.0435956412819957,
32.3375663899371));
#53657=CARTESIAN_POINT('Ctrl Pts',(34.0973371929324,-0.0541051140091329,
32.3329535581511));
#53658=CARTESIAN_POINT('Ctrl Pts',(34.0797713561159,-0.153636779613012,
32.3283407263652));
#53659=CARTESIAN_POINT('Ctrl Pts',(34.0395459106116,-0.242964529204384,
32.3237278945792));
#53660=CARTESIAN_POINT('Ctrl Pts',(33.9993204651073,-0.332292278795755,
32.3191150627932));
#53661=CARTESIAN_POINT('Ctrl Pts',(33.9364354109153,-0.411416112374621,
32.3145022310073));
#53662=CARTESIAN_POINT('Ctrl Pts',(33.8584944659184,-0.470768807393935,
32.3098893992213));
#53663=CARTESIAN_POINT('Ctrl Pts',(33.7805535209214,-0.530121502413249,
32.3052765674353));
#53664=CARTESIAN_POINT('Ctrl Pts',(33.6875566851195,-0.569703058873012,
32.3006637356494));
#53665=CARTESIAN_POINT('Ctrl Pts',(33.5907486288483,-0.584727490777849,
32.2960509038634));
#53666=CARTESIAN_POINT('Ctrl Pts',(33.493940572577,-0.599751922682685,32.2914380720775));
#53667=CARTESIAN_POINT('Ctrl Pts',(33.3933212958365,-0.590219230032596,
32.2868252402915));
#53668=CARTESIAN_POINT('Ctrl Pts',(33.3010571329606,-0.557282054047435,
32.2822124085055));
#53669=CARTESIAN_POINT('Ctrl Pts',(33.2087929700846,-0.524344878062274,
32.2775995767196));
#53670=CARTESIAN_POINT('Ctrl Pts',(33.1248839210733,-0.468003218742042,
32.2729867449336));
#53671=CARTESIAN_POINT('Ctrl Pts',(33.0594758106331,-0.395069602338378,
32.2683739131476));
#53672=CARTESIAN_POINT('Ctrl Pts',(32.9940677001929,-0.322135985934715,
32.2637610813617));
#53673=CARTESIAN_POINT('Ctrl Pts',(32.9471605283238,-0.232610412447618,
32.2591482495757));
#53674=CARTESIAN_POINT('Ctrl Pts',(32.9244260544949,-0.137317826100111,
32.2545354177897));
#53675=CARTESIAN_POINT('Ctrl Pts',(32.9137099569007,-0.0924008131539427,
32.2523611182666));
#53676=CARTESIAN_POINT('Ctrl Pts',(32.9083645313442,-0.0462024895878838,
32.2501868187436));
#53677=CARTESIAN_POINT('Ctrl Pts',(32.9083715657093,-2.56487800331939E-6,
32.2480125192205));
#53678=CARTESIAN_POINT('Ctrl Pts',(32.9083706917437,-3.8834067794807E-6,
32.2228374807795));
#53679=CARTESIAN_POINT('Ctrl Pts',(32.9083603614078,-0.0447338880195855,
32.2249426105267));
#53680=CARTESIAN_POINT('Ctrl Pts',(32.9133680575856,-0.0894616159528088,
32.2270477402738));
#53681=CARTESIAN_POINT('Ctrl Pts',(32.9234189614985,-0.133025801029227,
32.229152870021));
#53682=CARTESIAN_POINT('Ctrl Pts',(32.9454428434515,-0.22848512267994,32.2337657018069));
#53683=CARTESIAN_POINT('Ctrl Pts',(32.9916817188874,-0.318357686026281,
32.2383785335929));
#53684=CARTESIAN_POINT('Ctrl Pts',(33.0565446350982,-0.391776590723363,
32.2429913653788));
#53685=CARTESIAN_POINT('Ctrl Pts',(33.1214075513091,-0.465195495420446,
32.2476041971648));
#53686=CARTESIAN_POINT('Ctrl Pts',(33.2048945082948,-0.52216074146827,32.2522170289508));
#53687=CARTESIAN_POINT('Ctrl Pts',(33.2969107184152,-0.555784401908092,
32.2568298607367));
#53688=CARTESIAN_POINT('Ctrl Pts',(33.3889269285356,-0.589408062347915,
32.2614426925227));
#53689=CARTESIAN_POINT('Ctrl Pts',(33.4894723917907,-0.599690137179735,
32.2660555243087));
#53690=CARTESIAN_POINT('Ctrl Pts',(33.5863896989707,-0.585387373976165,
32.2706683560946));
#53691=CARTESIAN_POINT('Ctrl Pts',(33.6833070061508,-0.571084610772594,
32.2752811878806));
#53692=CARTESIAN_POINT('Ctrl Pts',(33.7765961572559,-0.532197009533633,
32.2798940196666));
#53693=CARTESIAN_POINT('Ctrl Pts',(33.8549771367776,-0.473426646973031,
32.2845068514525));
#53694=CARTESIAN_POINT('Ctrl Pts',(33.9333581162994,-0.414656284412429,
32.2891196832385));
#53695=CARTESIAN_POINT('Ctrl Pts',(33.9968309242378,-0.336003160530186,
32.2937325150245));
#53696=CARTESIAN_POINT('Ctrl Pts',(34.0377207747317,-0.246977582223296,
32.2983453468104));
#53697=CARTESIAN_POINT('Ctrl Pts',(34.0786106252257,-0.157952003916404,
32.3029581785964));
#53698=CARTESIAN_POINT('Ctrl Pts',(34.0969175182751,-0.0585539711848644,
32.3075710103824));
#53699=CARTESIAN_POINT('Ctrl Pts',(34.0904278841878,0.0391978478043787,
32.3121838421683));
#53700=CARTESIAN_POINT('Ctrl Pts',(34.0839382501004,0.13694966679362,32.3167966739543));
#53701=CARTESIAN_POINT('Ctrl Pts',(34.0526520888763,0.233055272040565,32.3214095057402));
#53702=CARTESIAN_POINT('Ctrl Pts',(34.0003523525481,0.315894097758303,32.3260223375262));
#53703=CARTESIAN_POINT('Ctrl Pts',(33.9480526162199,0.398732923476041,32.3306351693122));
#53704=CARTESIAN_POINT('Ctrl Pts',(33.8747393047876,0.468304969664571,32.3352480010981));
#53705=CARTESIAN_POINT('Ctrl Pts',(33.7892770641413,0.516197963828584,32.3398608328841));
#53706=CARTESIAN_POINT('Ctrl Pts',(33.7038148234949,0.564090957992597,32.3444736646701));
#53707=CARTESIAN_POINT('Ctrl Pts',(33.6062036536344,0.590304900132093,32.349086496456));
#53708=CARTESIAN_POINT('Ctrl Pts',(33.508246165011,0.591670143290649,32.353699328242));
#53709=CARTESIAN_POINT('Ctrl Pts',(33.4102886763875,0.593035386449204,32.3583121600279));
#53710=CARTESIAN_POINT('Ctrl Pts',(33.3119848690011,0.569551930626819,32.3629249918139));
#53711=CARTESIAN_POINT('Ctrl Pts',(33.2252211032561,0.524059267261966,32.3675378235999));
#53712=CARTESIAN_POINT('Ctrl Pts',(33.138457337511,0.478566603897114,32.3721506553859));
#53713=CARTESIAN_POINT('Ctrl Pts',(33.0632336134073,0.411064732989794,32.3767634871718));
#53714=CARTESIAN_POINT('Ctrl Pts',(33.0086455735188,0.329715612727591,32.3813763189578));
#53715=CARTESIAN_POINT('Ctrl Pts',(32.9540575336304,0.248366492465389,32.3859891507437));
#53716=CARTESIAN_POINT('Ctrl Pts',(32.9201051779573,0.153170122848304,32.3906019825297));
#53717=CARTESIAN_POINT('Ctrl Pts',(32.9108938402281,0.0556371298483394,
32.3952148143157));
#53718=CARTESIAN_POINT('Ctrl Pts',(32.9091481109472,0.0371527134979093,
32.3960890364703));
#53719=CARTESIAN_POINT('Ctrl Pts',(32.9082910218449,0.0185843710363966,
32.3969632586249));
#53720=CARTESIAN_POINT('Ctrl Pts',(32.9083097907792,1.43029731956186E-5,
32.3978374807795));
#53721=CARTESIAN_POINT('Origin',(33.5,0.,32.675));
#53722=CARTESIAN_POINT('',(32.9083067908048,-1.39749957427382E-5,32.5980125192205));
#53723=CARTESIAN_POINT('',(32.9083023250225,-1.33713639708521E-5,32.5728374807795));
#53724=CARTESIAN_POINT('',(32.908325,-7.2459289488551E-17,32.675));
#53725=CARTESIAN_POINT('Ctrl Pts',(32.9083067908048,-1.39749957427382E-5,
32.5980125192205));
#53726=CARTESIAN_POINT('Ctrl Pts',(32.9083871816409,0.0803724744095247,
32.59422811494));
#53727=CARTESIAN_POINT('Ctrl Pts',(32.9248933708252,0.160790928549149,32.5904437106596));
#53728=CARTESIAN_POINT('Ctrl Pts',(32.9567555944583,0.234578489970505,32.5866593063791));
#53729=CARTESIAN_POINT('Ctrl Pts',(32.9955926390906,0.324518566006179,32.5820464745932));
#53730=CARTESIAN_POINT('Ctrl Pts',(33.0572446201524,0.40460691916758,32.5774336428072));
#53731=CARTESIAN_POINT('Ctrl Pts',(33.1342569162406,0.465159702458623,32.5728208110212));
#53732=CARTESIAN_POINT('Ctrl Pts',(33.2112692123289,0.525712485749666,32.5682079792353));
#53733=CARTESIAN_POINT('Ctrl Pts',(33.3036418234436,0.566729699170351,32.5635951474493));
#53734=CARTESIAN_POINT('Ctrl Pts',(33.4002055570948,0.583251764913266,32.5589823156634));
#53735=CARTESIAN_POINT('Ctrl Pts',(33.496769290746,0.599773830656181,32.5543694838774));
#53736=CARTESIAN_POINT('Ctrl Pts',(33.5975241469337,0.591800748721324,32.5497566520914));
#53737=CARTESIAN_POINT('Ctrl Pts',(33.6902873977965,0.560296580704379,32.5451438203055));
#53738=CARTESIAN_POINT('Ctrl Pts',(33.7830506486593,0.528792412687434,32.5405309885195));
#53739=CARTESIAN_POINT('Ctrl Pts',(33.8678222941972,0.473757158588402,32.5359181567335));
#53740=CARTESIAN_POINT('Ctrl Pts',(33.9343522092348,0.401845381262527,32.5313053249476));
#53741=CARTESIAN_POINT('Ctrl Pts',(34.0008821242724,0.329933603936652,32.5266924931616));
#53742=CARTESIAN_POINT('Ctrl Pts',(34.0491703088097,0.241145303383935,32.5220796613756));
#53743=CARTESIAN_POINT('Ctrl Pts',(34.0733780188556,0.146216276804027,32.5174668295897));
#53744=CARTESIAN_POINT('Ctrl Pts',(34.0975857289015,0.0512872502241166,
32.5128539978037));
#53745=CARTESIAN_POINT('Ctrl Pts',(34.097712964456,-0.0497825023829855,
32.5082411660178));
#53746=CARTESIAN_POINT('Ctrl Pts',(34.0737443408896,-0.144772177597751,
32.5036283342318));
#53747=CARTESIAN_POINT('Ctrl Pts',(34.0497757173232,-0.239761852812517,
32.4990155024458));
#53748=CARTESIAN_POINT('Ctrl Pts',(34.0017112346358,-0.328671450634946,
32.4944026706599));
#53749=CARTESIAN_POINT('Ctrl Pts',(33.9353625880107,-0.400750507260887,
32.4897898388739));
#53750=CARTESIAN_POINT('Ctrl Pts',(33.8690139413855,-0.472829563886829,
32.4851770070879));
#53751=CARTESIAN_POINT('Ctrl Pts',(33.7843811308225,-0.528078079316282,
32.480564175302));
#53752=CARTESIAN_POINT('Ctrl Pts',(33.6916974943289,-0.559815704296698,
32.475951343516));
#53753=CARTESIAN_POINT('Ctrl Pts',(33.5990138578353,-0.591553329277114,
32.4713385117301));
#53754=CARTESIAN_POINT('Ctrl Pts',(33.4982793954111,-0.599780063808494,
32.4667256799441));
#53755=CARTESIAN_POINT('Ctrl Pts',(33.401674369015,-0.58350117600618,32.4621128481581));
#53756=CARTESIAN_POINT('Ctrl Pts',(33.3050693426189,-0.567222288203867,
32.4575000163721));
#53757=CARTESIAN_POINT('Ctrl Pts',(33.2125937522508,-0.526437778067861,
32.4528871845862));
#53758=CARTESIAN_POINT('Ctrl Pts',(33.1354292420907,-0.466079086193168,
32.4482743528002));
#53759=CARTESIAN_POINT('Ctrl Pts',(33.0582647319306,-0.405720394318476,
32.4436615210143));
#53760=CARTESIAN_POINT('Ctrl Pts',(32.9964113019784,-0.325787520705097,
32.4390486892283));
#53761=CARTESIAN_POINT('Ctrl Pts',(32.9573479317385,-0.235945512609894,
32.4344358574423));
#53762=CARTESIAN_POINT('Ctrl Pts',(32.9251020785013,-0.161783140295638,
32.430628078035));
#53763=CARTESIAN_POINT('Ctrl Pts',(32.9083855935444,-0.0808685873969588,
32.4268202986278));
#53764=CARTESIAN_POINT('Ctrl Pts',(32.9083052712772,1.37854762840214E-5,
32.4230125192205));
#53765=CARTESIAN_POINT('Ctrl Pts',(32.9083097907792,1.43029731956186E-5,
32.3978374807795));
#53766=CARTESIAN_POINT('Ctrl Pts',(32.9083900560961,-0.0794005630875795,
32.4015760904109));
#53767=CARTESIAN_POINT('Ctrl Pts',(32.924488397185,-0.158846987708581,32.4053147000422));
#53768=CARTESIAN_POINT('Ctrl Pts',(32.9556051166133,-0.231896029809362,
32.4090533096736));
#53769=CARTESIAN_POINT('Ctrl Pts',(32.9939980505131,-0.322026580084256,
32.4136661414595));
#53770=CARTESIAN_POINT('Ctrl Pts',(33.0552542380982,-0.402418064251198,
32.4182789732455));
#53771=CARTESIAN_POINT('Ctrl Pts',(33.1319669151548,-0.463349982365688,
32.4228918050314));
#53772=CARTESIAN_POINT('Ctrl Pts',(33.2086795922113,-0.524281900480177,
32.4275046368174));
#53773=CARTESIAN_POINT('Ctrl Pts',(33.3008487587393,-0.565754252542212,
32.4321174686034));
#53774=CARTESIAN_POINT('Ctrl Pts',(33.397329821659,-0.582752427861434,32.4367303003893));
#53775=CARTESIAN_POINT('Ctrl Pts',(33.4938108845787,-0.599750603180655,
32.4413431321753));
#53776=CARTESIAN_POINT('Ctrl Pts',(33.59460384389,-0.592274601757063,32.4459559639613));
#53777=CARTESIAN_POINT('Ctrl Pts',(33.6875213645097,-0.561228380921165,
32.4505687957472));
#53778=CARTESIAN_POINT('Ctrl Pts',(33.7804388851293,-0.530182160085267,
32.4551816275332));
#53779=CARTESIAN_POINT('Ctrl Pts',(33.8654809670573,-0.475565719837063,
32.4597944593192));
#53780=CARTESIAN_POINT('Ctrl Pts',(33.9323647854243,-0.403982982344468,
32.4644072911051));
#53781=CARTESIAN_POINT('Ctrl Pts',(33.9992486037914,-0.332400244851874,
32.4690201228911));
#53782=CARTESIAN_POINT('Ctrl Pts',(34.0479741585976,-0.24385121011489,32.4736329546771));
#53783=CARTESIAN_POINT('Ctrl Pts',(34.0726498214236,-0.149042744615283,
32.478245786463));
#53784=CARTESIAN_POINT('Ctrl Pts',(34.0973254842496,-0.0542342791156765,
32.482858618249));
#53785=CARTESIAN_POINT('Ctrl Pts',(34.0979512550954,0.0468336171465515,
32.4874714500349));
#53786=CARTESIAN_POINT('Ctrl Pts',(34.0744514691623,0.141940365210975,32.4920842818209));
#53787=CARTESIAN_POINT('Ctrl Pts',(34.0509516832292,0.2370471132754,32.4966971136069));
#53788=CARTESIAN_POINT('Ctrl Pts',(34.0033263405171,0.326192713142021,32.5013099453928));
#53789=CARTESIAN_POINT('Ctrl Pts',(33.9373340377976,0.39859816492626,32.5059227771788));
#53790=CARTESIAN_POINT('Ctrl Pts',(33.8713417350782,0.471003616710499,32.5105356089648));
#53791=CARTESIAN_POINT('Ctrl Pts',(33.7869824723514,0.526668920412358,32.5151484407507));
#53792=CARTESIAN_POINT('Ctrl Pts',(33.6944565117116,0.558863331013858,32.5197612725367));
#53793=CARTESIAN_POINT('Ctrl Pts',(33.6019305510718,0.591057741615356,32.5243741043227));
#53794=CARTESIAN_POINT('Ctrl Pts',(33.501237892519,0.599781259116496,32.5289869361086));
#53795=CARTESIAN_POINT('Ctrl Pts',(33.4045537433157,0.583979083344541,32.5335997678946));
#53796=CARTESIAN_POINT('Ctrl Pts',(33.3078695941124,0.568176907572586,32.5382125996805));
#53797=CARTESIAN_POINT('Ctrl Pts',(33.2151939542587,0.527849038527536,32.5428254314665));
#53798=CARTESIAN_POINT('Ctrl Pts',(33.1377326568273,0.467871702253438,32.5474382632525));
#53799=CARTESIAN_POINT('Ctrl Pts',(33.0602713593959,0.40789436597934,32.5520510950384));
#53800=CARTESIAN_POINT('Ctrl Pts',(32.9980244043868,0.328267562476194,32.5566639268244));
#53801=CARTESIAN_POINT('Ctrl Pts',(32.9585183542089,0.238619330671929,32.5612767586104));
#53802=CARTESIAN_POINT('Ctrl Pts',(32.925514876714,0.163726918307737,32.5651303326667));
#53803=CARTESIAN_POINT('Ctrl Pts',(32.9083822396197,0.0818405674730361,
32.5689839067231));
#53804=CARTESIAN_POINT('Ctrl Pts',(32.9083023250225,-1.33713639708521E-5,
32.5728374807795));
#53805=CARTESIAN_POINT('Origin',(33.5,0.,32.675));
#53806=CARTESIAN_POINT('',(32.9083713119041,3.01319602050154E-6,32.7730125192205));
#53807=CARTESIAN_POINT('',(32.9083719392501,1.68036311726623E-6,32.7478374807795));
#53808=CARTESIAN_POINT('',(32.908325,-7.2459289488551E-17,32.675));
#53809=CARTESIAN_POINT('Ctrl Pts',(32.9083713119041,3.01319602050154E-6,
32.7730125192205));
#53810=CARTESIAN_POINT('Ctrl Pts',(32.9083631325366,0.0457062027160928,
32.7708615948242));
#53811=CARTESIAN_POINT('Ctrl Pts',(32.9135931597386,0.0914075504572254,
32.768710670428));
#53812=CARTESIAN_POINT('Ctrl Pts',(32.924082143701,0.135868226253254,32.7665597460317));
#53813=CARTESIAN_POINT('Ctrl Pts',(32.946576620359,0.231217750808743,32.7619469142458));
#53814=CARTESIAN_POINT('Ctrl Pts',(32.9932582384694,0.320861142152127,32.7573340824598));
#53815=CARTESIAN_POINT('Ctrl Pts',(33.0584825112939,0.393959210167586,32.7527212506738));
#53816=CARTESIAN_POINT('Ctrl Pts',(33.1237067841184,0.467057278183043,32.7481084188879));
#53817=CARTESIAN_POINT('Ctrl Pts',(33.207473711657,0.523610022870575,32.7434955871019));
#53818=CARTESIAN_POINT('Ctrl Pts',(33.2996546537567,0.556779394686837,32.7388827553159));
#53819=CARTESIAN_POINT('Ctrl Pts',(33.3918355958564,0.589948766503101,32.73426992353));
#53820=CARTESIAN_POINT('Ctrl Pts',(33.4924305525172,0.599734765448092,32.729657091744));
#53821=CARTESIAN_POINT('Ctrl Pts',(33.5892761300567,0.584954121885886,32.7250442599581));
#53822=CARTESIAN_POINT('Ctrl Pts',(33.6861217075963,0.57017347832368,32.7204314281721));
#53823=CARTESIAN_POINT('Ctrl Pts',(33.7792179060145,0.530826192254278,32.7158185963861));
#53824=CARTESIAN_POINT('Ctrl Pts',(33.8573080405899,0.471669922974772,32.7112057646002));
#53825=CARTESIAN_POINT('Ctrl Pts',(33.9353981751653,0.412513653695266,32.7065929328142));
#53826=CARTESIAN_POINT('Ctrl Pts',(33.9984822458979,0.333548401205659,32.7019801010282));
#53827=CARTESIAN_POINT('Ctrl Pts',(34.03893247091,0.244322213292315,32.6973672692423));
#53828=CARTESIAN_POINT('Ctrl Pts',(34.0793826959221,0.155096025378972,32.6927544374563));
#53829=CARTESIAN_POINT('Ctrl Pts',(34.0971990752136,0.0556089020418922,
32.6881416056703));
#53830=CARTESIAN_POINT('Ctrl Pts',(34.0902273493414,-0.0421097162017081,
32.6835287738844));
#53831=CARTESIAN_POINT('Ctrl Pts',(34.0832556234693,-0.139828334445311,
32.6789159420984));
#53832=CARTESIAN_POINT('Ctrl Pts',(34.0514957924334,-0.235778447595435,
32.6743031103125));
#53833=CARTESIAN_POINT('Ctrl Pts',(33.9987880818376,-0.318358291121721,
32.6696902785265));
#53834=CARTESIAN_POINT('Ctrl Pts',(33.9460803712418,-0.400938134648005,
32.6650774467405));
#53835=CARTESIAN_POINT('Ctrl Pts',(33.8724247810861,-0.470147708550451,
32.6604646149546));
#53836=CARTESIAN_POINT('Ctrl Pts',(33.7867273437374,-0.517618568506266,
32.6558517831686));
#53837=CARTESIAN_POINT('Ctrl Pts',(33.7010299063888,-0.565089428462083,
32.6512389513826));
#53838=CARTESIAN_POINT('Ctrl Pts',(33.6032906218471,-0.590821574471267,
32.6466261195967));
#53839=CARTESIAN_POINT('Ctrl Pts',(33.5053275914924,-0.591703615738561,
32.6420132878107));
#53840=CARTESIAN_POINT('Ctrl Pts',(33.4073645611377,-0.592585657005855,
32.6374004560247));
#53841=CARTESIAN_POINT('Ctrl Pts',(33.3091777849699,-0.568617593531258,
32.6327876242388));
#53842=CARTESIAN_POINT('Ctrl Pts',(33.2226394726165,-0.522697512868307,
32.6281747924528));
#53843=CARTESIAN_POINT('Ctrl Pts',(33.136101160263,-0.476777432205359,32.6235619606669));
#53844=CARTESIAN_POINT('Ctrl Pts',(33.0612113117239,-0.408905334354059,
32.6189491288809));
#53845=CARTESIAN_POINT('Ctrl Pts',(33.0070251991603,-0.327287943325459,
32.6143362970949));
#53846=CARTESIAN_POINT('Ctrl Pts',(32.9528390865966,-0.245670552296858,
32.609723465309));
#53847=CARTESIAN_POINT('Ctrl Pts',(32.9193567100084,-0.150307868090957,
32.605110633523));
#53848=CARTESIAN_POINT('Ctrl Pts',(32.9106265758158,-0.0527306265330337,
32.600497801737));
#53849=CARTESIAN_POINT('Ctrl Pts',(32.9090587138976,-0.0352065383872344,
32.5996693742315));
#53850=CARTESIAN_POINT('Ctrl Pts',(32.908289192796,-0.01761102351991,32.598840946726));
#53851=CARTESIAN_POINT('Ctrl Pts',(32.9083067908048,-1.39749957427382E-5,
32.5980125192205));
#53852=CARTESIAN_POINT('Ctrl Pts',(32.9083023250225,-1.33713639708521E-5,
32.5728374807795));
#53853=CARTESIAN_POINT('Ctrl Pts',(32.9082865796976,-0.0161407987469254,
32.5735967385091));
#53854=CARTESIAN_POINT('Ctrl Pts',(32.9089328141914,-0.0322669679091847,
32.5743559962387));
#53855=CARTESIAN_POINT('Ctrl Pts',(32.9102500681346,-0.0483381377762423,
32.5751152539682));
#53856=CARTESIAN_POINT('Ctrl Pts',(32.918252977585,-0.145977714314759,32.5797280857542));
#53857=CARTESIAN_POINT('Ctrl Pts',(32.9510239418328,-0.241587207286407,
32.5843409175402));
#53858=CARTESIAN_POINT('Ctrl Pts',(33.0046004745592,-0.323606038095636,
32.5889537493262));
#53859=CARTESIAN_POINT('Ctrl Pts',(33.0581770072855,-0.405624868904866,
32.5935665811121));
#53860=CARTESIAN_POINT('Ctrl Pts',(33.1325591084905,-0.474053037551677,
32.5981794128981));
#53861=CARTESIAN_POINT('Ctrl Pts',(33.2187529000522,-0.520616582976306,
32.602792244684));
#53862=CARTESIAN_POINT('Ctrl Pts',(33.3049466916139,-0.567180128400934,
32.60740507647));
#53863=CARTESIAN_POINT('Ctrl Pts',(33.4029521735323,-0.591879050603381,
32.612017908256));
#53864=CARTESIAN_POINT('Ctrl Pts',(33.5009190572922,-0.59172689057762,32.6166307400419));
#53865=CARTESIAN_POINT('Ctrl Pts',(33.5988859410521,-0.591574730551859,
32.6212435718279));
#53866=CARTESIAN_POINT('Ctrl Pts',(33.6968142266534,-0.56657148829789,32.6258564036139));
#53867=CARTESIAN_POINT('Ctrl Pts',(33.7828629597387,-0.519740419543116,
32.6304692353998));
#53868=CARTESIAN_POINT('Ctrl Pts',(33.8689116928239,-0.472909350788342,
32.6350820671858));
#53869=CARTESIAN_POINT('Ctrl Pts',(33.9430808733931,-0.404250455532762,
32.6396948989717));
#53870=CARTESIAN_POINT('Ctrl Pts',(33.9964023685267,-0.322065593039673,
32.6443077307577));
#53871=CARTESIAN_POINT('Ctrl Pts',(34.0497238636604,-0.239880730546585,
32.6489205625437));
#53872=CARTESIAN_POINT('Ctrl Pts',(34.0821976733584,-0.144169900815988,
32.6535333943296));
#53873=CARTESIAN_POINT('Ctrl Pts',(34.0898972416102,-0.0465059355318047,
32.6581462261156));
#53874=CARTESIAN_POINT('Ctrl Pts',(34.0975968098619,0.0511580297523774,
32.6627590579016));
#53875=CARTESIAN_POINT('Ctrl Pts',(34.0805221366673,0.150775130590147,32.6673718896875));
#53876=CARTESIAN_POINT('Ctrl Pts',(34.0407377984123,0.240300210293585,32.6719847214735));
#53877=CARTESIAN_POINT('Ctrl Pts',(34.0009534601573,0.329825289997023,32.6765975532595));
#53878=CARTESIAN_POINT('Ctrl Pts',(33.938459456842,0.40925834856613,32.6812103850454));
#53879=CARTESIAN_POINT('Ctrl Pts',(33.8608122226091,0.468994773654039,32.6858232168314));
#53880=CARTESIAN_POINT('Ctrl Pts',(33.7831649883763,0.528731198741949,32.6904360486174));
#53881=CARTESIAN_POINT('Ctrl Pts',(33.690364523226,0.568770990348661,32.6950488804033));
#53882=CARTESIAN_POINT('Ctrl Pts',(33.5936317534254,0.584272755183279,32.6996617121893));
#53883=CARTESIAN_POINT('Ctrl Pts',(33.4968989836247,0.599774520017897,32.7042745439753));
#53884=CARTESIAN_POINT('Ctrl Pts',(33.3962339091737,0.590738258080421,32.7088873757612));
#53885=CARTESIAN_POINT('Ctrl Pts',(33.3038084020157,0.558256584895642,32.7135002075472));
#53886=CARTESIAN_POINT('Ctrl Pts',(33.2113828948578,0.525774911710863,32.7181130393332));
#53887=CARTESIAN_POINT('Ctrl Pts',(33.1271969549928,0.469847827278781,32.7227258711191));
#53888=CARTESIAN_POINT('Ctrl Pts',(33.0614298872597,0.39723772971596,32.7273387029051));
#53889=CARTESIAN_POINT('Ctrl Pts',(32.9956628195266,0.324627632153138,32.731951534691));
#53890=CARTESIAN_POINT('Ctrl Pts',(32.9483146239253,0.235334521459577,32.736564366477));
#53891=CARTESIAN_POINT('Ctrl Pts',(32.9251103861101,0.140155233724766,32.741177198263));
#53892=CARTESIAN_POINT('Ctrl Pts',(32.9139424971573,0.0943467170008,32.7433972924351));
#53893=CARTESIAN_POINT('Ctrl Pts',(32.9083672373457,0.0471747450578055,
32.7456173866073));
#53894=CARTESIAN_POINT('Ctrl Pts',(32.9083719392501,1.68036311726623E-6,
32.7478374807795));
#53895=CARTESIAN_POINT('Origin',(33.5,0.,32.675));
#53896=CARTESIAN_POINT('',(32.9082880531064,1.02913734114571E-5,32.9480125192205));
#53897=CARTESIAN_POINT('',(32.9082918568422,1.13186425445232E-5,32.9228374807795));
#53898=CARTESIAN_POINT('',(32.908325,-7.2459289488551E-17,32.675));
#53899=CARTESIAN_POINT('Ctrl Pts',(32.9082880531064,1.02913734114571E-5,
32.9480125192205));
#53900=CARTESIAN_POINT('Ctrl Pts',(32.9082790912156,0.011000586374815,32.9474950747084));
#53901=CARTESIAN_POINT('Ctrl Pts',(32.9085790477372,0.0219903924153702,
32.9469776301964));
#53902=CARTESIAN_POINT('Ctrl Pts',(32.9091912260938,0.0329627787767829,
32.9464601856843));
#53903=CARTESIAN_POINT('Ctrl Pts',(32.914648576044,0.130777658240983,32.9418473538984));
#53904=CARTESIAN_POINT('Ctrl Pts',(32.9449184495677,0.227208181613048,32.9372345221124));
#53905=CARTESIAN_POINT('Ctrl Pts',(32.9963407785996,0.310594495777936,32.9326216903264));
#53906=CARTESIAN_POINT('Ctrl Pts',(33.0477631076316,0.393980809942825,32.9280088585405));
#53907=CARTESIAN_POINT('Ctrl Pts',(33.1203378921718,0.464322914900539,32.9233960267545));
#53908=CARTESIAN_POINT('Ctrl Pts',(33.2052897849755,0.513115426848012,32.9187831949685));
#53909=CARTESIAN_POINT('Ctrl Pts',(33.2902416777792,0.561907938795485,32.9141703631826));
#53910=CARTESIAN_POINT('Ctrl Pts',(33.3875706788463,0.589150857732719,32.9095575313966));
#53911=CARTESIAN_POINT('Ctrl Pts',(33.4855082960378,0.591550118439231,32.9049446996106));
#53912=CARTESIAN_POINT('Ctrl Pts',(33.5834459132292,0.593949379145743,32.9003318678247));
#53913=CARTESIAN_POINT('Ctrl Pts',(33.681992146545,0.571504981621529,32.8957190360387));
#53914=CARTESIAN_POINT('Ctrl Pts',(33.7692313227591,0.526930780040939,32.8911062042528));
#53915=CARTESIAN_POINT('Ctrl Pts',(33.8564704989733,0.48235657846035,32.8864933724668));
#53916=CARTESIAN_POINT('Ctrl Pts',(33.9324026180859,0.415652572823385,32.8818805406808));
#53917=CARTESIAN_POINT('Ctrl Pts',(33.9878463822609,0.334884247799363,32.8772677088949));
#53918=CARTESIAN_POINT('Ctrl Pts',(34.0432901464359,0.254115922775342,32.8726548771089));
#53919=CARTESIAN_POINT('Ctrl Pts',(34.0782455556732,0.159283278364265,32.8680420453229));
#53920=CARTESIAN_POINT('Ctrl Pts',(34.0884859924764,0.0618529608693727,
32.863429213537));
#53921=CARTESIAN_POINT('Ctrl Pts',(34.0987264292795,-0.0355773566255206,
32.858816381751));
#53922=CARTESIAN_POINT('Ctrl Pts',(34.0842518936485,-0.135605347204229,
32.854203549965));
#53923=CARTESIAN_POINT('Ctrl Pts',(34.0468125675119,-0.226136171631666,
32.8495907181791));
#53924=CARTESIAN_POINT('Ctrl Pts',(34.0093732413753,-0.316666996059103,
32.8449778863931));
#53925=CARTESIAN_POINT('Ctrl Pts',(33.9489691247331,-0.397700654335268,
32.8403650546072));
#53926=CARTESIAN_POINT('Ctrl Pts',(33.8729039540264,-0.459438998323717,
32.8357522228212));
#53927=CARTESIAN_POINT('Ctrl Pts',(33.7968387833197,-0.521177342312166,
32.8311393910352));
#53928=CARTESIAN_POINT('Ctrl Pts',(33.7051125585485,-0.563620372012898,
32.8265265592493));
#53929=CARTESIAN_POINT('Ctrl Pts',(33.6088163146905,-0.58163610768794,32.8219137274633));
#53930=CARTESIAN_POINT('Ctrl Pts',(33.5125200708325,-0.599651843362981,
32.8173008956773));
#53931=CARTESIAN_POINT('Ctrl Pts',(33.4116538078876,-0.593240285012332,
32.8126880638914));
#53932=CARTESIAN_POINT('Ctrl Pts',(33.318413724415,-0.563176683313814,32.8080752321054));
#53933=CARTESIAN_POINT('Ctrl Pts',(33.2251736409423,-0.533113081615296,
32.8034624003194));
#53934=CARTESIAN_POINT('Ctrl Pts',(33.1395597369418,-0.479397436568909,
32.7988495685335));
#53935=CARTESIAN_POINT('Ctrl Pts',(33.07192397889,-0.408524751098197,32.7942367367475));
#53936=CARTESIAN_POINT('Ctrl Pts',(33.0042882208382,-0.337652065627488,
32.7896239049616));
#53937=CARTESIAN_POINT('Ctrl Pts',(32.954630608735,-0.249622339732455,32.7850110731756));
#53938=CARTESIAN_POINT('Ctrl Pts',(32.9289554702862,-0.155079647901143,
32.7803982413896));
#53939=CARTESIAN_POINT('Ctrl Pts',(32.9152524314563,-0.104621412599548,
32.7779363339999));
#53940=CARTESIAN_POINT('Ctrl Pts',(32.9083806738534,-0.0523079932758981,
32.7754744266102));
#53941=CARTESIAN_POINT('Ctrl Pts',(32.9083713119041,3.01319602050154E-6,
32.7730125192205));
#53942=CARTESIAN_POINT('Ctrl Pts',(32.9083719392501,1.68036311726623E-6,
32.7478374807795));
#53943=CARTESIAN_POINT('Ctrl Pts',(32.9083770067935,-0.0508397513504451,
32.7502302183933));
#53944=CARTESIAN_POINT('Ctrl Pts',(32.9148636199127,-0.101682452377359,
32.7526229560071));
#53945=CARTESIAN_POINT('Ctrl Pts',(32.9278159202069,-0.150820875645032,
32.7550156936208));
#53946=CARTESIAN_POINT('Ctrl Pts',(32.9527859721484,-0.245552232503963,
32.7596285254068));
#53947=CARTESIAN_POINT('Ctrl Pts',(33.0017863560606,-0.333949481445767,
32.7642413571928));
#53948=CARTESIAN_POINT('Ctrl Pts',(33.0688922126872,-0.405324109099441,
32.7688541889788));
#53949=CARTESIAN_POINT('Ctrl Pts',(33.1359980693138,-0.476698736753116,
32.7734670207647));
#53950=CARTESIAN_POINT('Ctrl Pts',(33.2212093986549,-0.531050743118661,
32.7780798525507));
#53951=CARTESIAN_POINT('Ctrl Pts',(33.3142229113667,-0.561808179931472,
32.7826926843366));
#53952=CARTESIAN_POINT('Ctrl Pts',(33.4072364240786,-0.592565616744283,
32.7873055161226));
#53953=CARTESIAN_POINT('Ctrl Pts',(33.5080521201613,-0.599728484004359,
32.7919183479086));
#53954=CARTESIAN_POINT('Ctrl Pts',(33.604479915325,-0.582430686856934,32.7965311796945));
#53955=CARTESIAN_POINT('Ctrl Pts',(33.7009077104888,-0.565132889709509,
32.8011440114805));
#53956=CARTESIAN_POINT('Ctrl Pts',(33.7929476047335,-0.523374428154583,
32.8057568432665));
#53957=CARTESIAN_POINT('Ctrl Pts',(33.8694706358792,-0.462204507682433,
32.8103696750524));
#53958=CARTESIAN_POINT('Ctrl Pts',(33.9459936670249,-0.401034587210282,
32.8149825068384));
#53959=CARTESIAN_POINT('Ctrl Pts',(34.0069998350715,-0.320453207820907,
32.8195953386244));
#53960=CARTESIAN_POINT('Ctrl Pts',(34.0451126068046,-0.230203830553735,
32.8242081704103));
#53961=CARTESIAN_POINT('Ctrl Pts',(34.0832253785378,-0.139954453286563,
32.8288210021963));
#53962=CARTESIAN_POINT('Ctrl Pts',(34.0984447539574,-0.0400370781415953,
32.8334338339822));
#53963=CARTESIAN_POINT('Ctrl Pts',(34.0889304891689,0.0574668306612187,
32.8380466657682));
#53964=CARTESIAN_POINT('Ctrl Pts',(34.0794162243804,0.154970739464031,32.8426594975542));
#53965=CARTESIAN_POINT('Ctrl Pts',(34.0451683193837,0.25006118192469,32.8472723293401));
#53966=CARTESIAN_POINT('Ctrl Pts',(33.9903278441202,0.331240340205398,32.8518851611261));
#53967=CARTESIAN_POINT('Ctrl Pts',(33.9354873688567,0.412419498486108,32.8564979929121));
#53968=CARTESIAN_POINT('Ctrl Pts',(33.8600543233263,0.479687372586867,32.861110824698));
#53969=CARTESIAN_POINT('Ctrl Pts',(33.7731496601087,0.52491029793811,32.865723656484));
#53970=CARTESIAN_POINT('Ctrl Pts',(33.686244996891,0.570133223289354,32.87033648827));
#53971=CARTESIAN_POINT('Ctrl Pts',(33.5878687159862,0.593311199891084,32.8749493200559));
#53972=CARTESIAN_POINT('Ctrl Pts',(33.4899159409011,0.591641673186612,32.8795621518419));
#53973=CARTESIAN_POINT('Ctrl Pts',(33.3919631658159,0.589972146482141,32.8841749836278));
#53974=CARTESIAN_POINT('Ctrl Pts',(33.2944338965506,0.56345511647147,32.8887878154138));
#53975=CARTESIAN_POINT('Ctrl Pts',(33.2091208405827,0.51529687784387,32.8934006471998));
#53976=CARTESIAN_POINT('Ctrl Pts',(33.1238077846148,0.467138639216271,32.8980134789857));
#53977=CARTESIAN_POINT('Ctrl Pts',(33.0507109419444,0.397339191971745,32.9026263107717));
#53978=CARTESIAN_POINT('Ctrl Pts',(32.998668784239,0.314338304701424,32.9072391425577));
#53979=CARTESIAN_POINT('Ctrl Pts',(32.9466266265336,0.2313374174311,32.9118519743436));
#53980=CARTESIAN_POINT('Ctrl Pts',(32.9156391537933,0.13513509013498,32.9164648061296));
#53981=CARTESIAN_POINT('Ctrl Pts',(32.9094532022677,0.0373635837028018,
32.9210776379156));
#53982=CARTESIAN_POINT('Ctrl Pts',(32.9086665341823,0.0249299712729768,
32.9216642522035));
#53983=CARTESIAN_POINT('Ctrl Pts',(32.9082809621213,0.012470981709718,32.9222508664915));
#53984=CARTESIAN_POINT('Ctrl Pts',(32.9082918568422,1.13186425445232E-5,
32.9228374807795));
#53985=CARTESIAN_POINT('Origin',(33.5,0.,32.675));
#53986=CARTESIAN_POINT('',(32.9083258423465,-1.50708354626494E-5,33.1230125192205));
#53987=CARTESIAN_POINT('',(32.9083212660424,-1.50170003654025E-5,33.0978374807795));
#53988=CARTESIAN_POINT('',(32.908325,-7.2459289488551E-17,32.675));
#53989=CARTESIAN_POINT('Ctrl Pts',(32.9083258423465,-1.50708354626494E-5,
33.1230125192205));
#53990=CARTESIAN_POINT('Ctrl Pts',(32.9084005096858,0.0742690450598342,
33.1195157228067));
#53991=CARTESIAN_POINT('Ctrl Pts',(32.922435621069,0.148580580320246,33.1160189263928));
#53992=CARTESIAN_POINT('Ctrl Pts',(32.9497504595365,0.217639599634083,33.112522129979));
#53993=CARTESIAN_POINT('Ctrl Pts',(32.9857830848885,0.308739452670834,33.1079092981931));
#53994=CARTESIAN_POINT('Ctrl Pts',(33.0449248452043,0.390698974800284,33.1032964664071));
#53995=CARTESIAN_POINT('Ctrl Pts',(33.1200246412871,0.453608067476981,33.0986836346211));
#53996=CARTESIAN_POINT('Ctrl Pts',(33.1951244373698,0.516517160153676,33.0940708028352));
#53997=CARTESIAN_POINT('Ctrl Pts',(33.2861822692195,0.560375823377616,33.0894579710492));
#53998=CARTESIAN_POINT('Ctrl Pts',(33.3821879202862,0.579880906723698,33.0848451392632));
#53999=CARTESIAN_POINT('Ctrl Pts',(33.4781935713528,0.59938599006978,33.0802323074773));
#54000=CARTESIAN_POINT('Ctrl Pts',(33.5791470416366,0.594537493538001,33.0756194756913));
#54001=CARTESIAN_POINT('Ctrl Pts',(33.6728415879424,0.565921670893381,33.0710066439053));
#54002=CARTESIAN_POINT('Ctrl Pts',(33.7665361342481,0.537305848248762,33.0663938121194));
#54003=CARTESIAN_POINT('Ctrl Pts',(33.852971756576,0.484922699491301,33.0617809803334));
#54004=CARTESIAN_POINT('Ctrl Pts',(33.9216971307496,0.415106109358497,33.0571681485475));
#54005=CARTESIAN_POINT('Ctrl Pts',(33.9904225049232,0.345289519225692,33.0525553167615));
#54006=CARTESIAN_POINT('Ctrl Pts',(34.0414376309426,0.258039487717542,33.0479424849755));
#54007=CARTESIAN_POINT('Ctrl Pts',(34.0685740379208,0.163905812927982,33.0433296531896));
#54008=CARTESIAN_POINT('Ctrl Pts',(34.0957104448991,0.0697721381384229,
33.0387168214036));
#54009=CARTESIAN_POINT('Ctrl Pts',(34.0989681328362,-0.0312451799325463,
33.0341039896176));
#54010=CARTESIAN_POINT('Ctrl Pts',(34.0779531998687,-0.126931677963617,
33.0294911578317));
#54011=CARTESIAN_POINT('Ctrl Pts',(34.0569382669013,-0.22261817599469,33.0248783260457));
#54012=CARTESIAN_POINT('Ctrl Pts',(34.0116507130294,-0.31297385398586,33.0202654942598));
#54013=CARTESIAN_POINT('Ctrl Pts',(33.9475664623444,-0.387073396003486,
33.0156526624738));
#54014=CARTESIAN_POINT('Ctrl Pts',(33.8834822116595,-0.461172938021111,
33.0110398306878));
#54015=CARTESIAN_POINT('Ctrl Pts',(33.8006012641615,-0.519016344065188,
33.0064269989019));
#54016=CARTESIAN_POINT('Ctrl Pts',(33.7089451321275,-0.55360950485825,33.0018141671159));
#54017=CARTESIAN_POINT('Ctrl Pts',(33.6172890000936,-0.588202665651312,
32.9972013353299));
#54018=CARTESIAN_POINT('Ctrl Pts',(33.5168576835238,-0.59954558119336,32.992588503544));
#54019=CARTESIAN_POINT('Ctrl Pts',(33.4197947896329,-0.586266727982377,
32.987975671758));
#54020=CARTESIAN_POINT('Ctrl Pts',(33.322731895742,-0.572987874771394,32.983362839972));
#54021=CARTESIAN_POINT('Ctrl Pts',(33.22903742453,-0.535087252807379,32.9787500081861));
#54022=CARTESIAN_POINT('Ctrl Pts',(33.1500404006027,-0.477147598651493,
32.9741371764001));
#54023=CARTESIAN_POINT('Ctrl Pts',(33.0710433766754,-0.419207944495608,
32.9695243446141));
#54024=CARTESIAN_POINT('Ctrl Pts',(33.0067438000327,-0.341229258147852,
32.9649115128282));
#54025=CARTESIAN_POINT('Ctrl Pts',(32.9649164248998,-0.252640297195804,
32.9602986810422));
#54026=CARTESIAN_POINT('Ctrl Pts',(32.9277810365377,-0.17398880498314,32.9562032937683));
#54027=CARTESIAN_POINT('Ctrl Pts',(32.90835898325,-0.0869739421761365,32.9521079064944));
#54028=CARTESIAN_POINT('Ctrl Pts',(32.9082880531064,1.02913734114571E-5,
32.9480125192205));
#54029=CARTESIAN_POINT('Ctrl Pts',(32.9082918568422,1.13186425445232E-5,
32.9228374807795));
#54030=CARTESIAN_POINT('Ctrl Pts',(32.9083666325799,-0.0855053734799262,
32.9268636982775));
#54031=CARTESIAN_POINT('Ctrl Pts',(32.9271179299873,-0.171053792624762,
32.9308899157755));
#54032=CARTESIAN_POINT('Ctrl Pts',(32.9630490181471,-0.248646738941268,
32.9349161332734));
#54033=CARTESIAN_POINT('Ctrl Pts',(33.0042152158626,-0.337544869584926,
32.9395289650594));
#54034=CARTESIAN_POINT('Ctrl Pts',(33.0679320416044,-0.416000445304007,
32.9441417968454));
#54035=CARTESIAN_POINT('Ctrl Pts',(33.146495204209,-0.474527045648313,32.9487546286313));
#54036=CARTESIAN_POINT('Ctrl Pts',(33.2250583668135,-0.533053645992619,
32.9533674604173));
#54037=CARTESIAN_POINT('Ctrl Pts',(33.3184678662809,-0.571651270962148,
32.9579802922033));
#54038=CARTESIAN_POINT('Ctrl Pts',(33.4154291352348,-0.585652906192602,
32.9625931239892));
#54039=CARTESIAN_POINT('Ctrl Pts',(33.5123904041888,-0.599654541423056,
32.9672059557752));
#54040=CARTESIAN_POINT('Ctrl Pts',(33.6129034426295,-0.589060186914436,
32.9718187875611));
#54041=CARTESIAN_POINT('Ctrl Pts',(33.7048147619789,-0.555150854249999,
32.9764316193471));
#54042=CARTESIAN_POINT('Ctrl Pts',(33.7967260813282,-0.521241521585563,
32.9810444511331));
#54043=CARTESIAN_POINT('Ctrl Pts',(33.8800356815864,-0.46401721076531,32.985657282919));
#54044=CARTESIAN_POINT('Ctrl Pts',(33.9446702201216,-0.390397173447754,
32.990270114705));
#54045=CARTESIAN_POINT('Ctrl Pts',(34.0093047586567,-0.316777136130199,
32.994882946491));
#54046=CARTESIAN_POINT('Ctrl Pts',(34.0552642354689,-0.226761372315337,
32.9994957782769));
#54047=CARTESIAN_POINT('Ctrl Pts',(34.0769914812083,-0.13123409736795,33.0041086100629));
#54048=CARTESIAN_POINT('Ctrl Pts',(34.0987187269477,-0.0357068224205606,
33.0087214418489));
#54049=CARTESIAN_POINT('Ctrl Pts',(34.0962137416143,0.0653319636593577,
33.0133342736348));
#54050=CARTESIAN_POINT('Ctrl Pts',(34.0697794143765,0.159665201755905,33.0179471054208));
#54051=CARTESIAN_POINT('Ctrl Pts',(34.0433450871387,0.253998439852452,33.0225599372068));
#54052=CARTESIAN_POINT('Ctrl Pts',(33.9929814179966,0.341626129965624,33.0271727689927));
#54053=CARTESIAN_POINT('Ctrl Pts',(33.9247781072235,0.411952809582094,33.0317856007787));
#54054=CARTESIAN_POINT('Ctrl Pts',(33.8565747964504,0.482279489198563,33.0363984325647));
#54055=CARTESIAN_POINT('Ctrl Pts',(33.7705318440462,0.53530515831833,33.0410112643506));
#54056=CARTESIAN_POINT('Ctrl Pts',(33.6770530946811,0.564618242144916,33.0456240961366));
#54057=CARTESIAN_POINT('Ctrl Pts',(33.583574345316,0.593931325971504,33.0502369279225));
#54058=CARTESIAN_POINT('Ctrl Pts',(33.4826597989899,0.599531824504911,33.0548497597085));
#54059=CARTESIAN_POINT('Ctrl Pts',(33.3865114924251,0.580742555998248,33.0594625914945));
#54060=CARTESIAN_POINT('Ctrl Pts',(33.2903631858603,0.561953287491587,33.0640754232804));
#54061=CARTESIAN_POINT('Ctrl Pts',(33.1989811190568,0.518774251944856,33.0686882550664));
#54062=CARTESIAN_POINT('Ctrl Pts',(33.1234147132872,0.456426422909986,33.0733010868524));
#54063=CARTESIAN_POINT('Ctrl Pts',(33.0478483075176,0.394078593875114,33.0779139186383));
#54064=CARTESIAN_POINT('Ctrl Pts',(32.988097562782,0.312561971352099,33.0825267504243));
#54065=CARTESIAN_POINT('Ctrl Pts',(32.9513872133529,0.221733100880836,33.0871395822103));
#54066=CARTESIAN_POINT('Ctrl Pts',(32.9230081457969,0.151517516141978,33.0907055484));
#54067=CARTESIAN_POINT('Ctrl Pts',(32.9083982917097,0.075736821596309,33.0942715145898));
#54068=CARTESIAN_POINT('Ctrl Pts',(32.9083212660424,-1.50170003654025E-5,
33.0978374807795));
#54069=CARTESIAN_POINT('Origin',(33.5,0.,32.675));
#54070=CARTESIAN_POINT('',(32.9083649252952,8.19085268685682E-6,33.2980125192205));
#54071=CARTESIAN_POINT('',(32.9083669931439,7.02104240262066E-6,33.2728374807795));
#54072=CARTESIAN_POINT('',(32.908325,-7.2459289488551E-17,32.675));
#54073=CARTESIAN_POINT('Ctrl Pts',(32.9083649252952,8.19085268685682E-6,
33.2980125192205));
#54074=CARTESIAN_POINT('Ctrl Pts',(32.9083454014238,0.0395990184514228,
33.2961492026909));
#54075=CARTESIAN_POINT('Ctrl Pts',(32.9122609890038,0.0791860361356371,
33.2942858861612));
#54076=CARTESIAN_POINT('Ctrl Pts',(32.9201501167737,0.11796467672071,33.2924225696316));
#54077=CARTESIAN_POINT('Ctrl Pts',(32.9396804642814,0.213965191428613,33.2878097378457));
#54078=CARTESIAN_POINT('Ctrl Pts',(32.983563088619,0.305011478429999,33.2831969060597));
#54079=CARTESIAN_POINT('Ctrl Pts',(33.0464919423082,0.380094716824501,33.2785840742737));
#54080=CARTESIAN_POINT('Ctrl Pts',(33.1094207959975,0.455177955219004,33.2739712424878));
#54081=CARTESIAN_POINT('Ctrl Pts',(33.1913958790385,0.514298145006622,33.2693584107018));
#54082=CARTESIAN_POINT('Ctrl Pts',(33.2825052112551,0.550306795310209,33.2647455789158));
#54083=CARTESIAN_POINT('Ctrl Pts',(33.3736145434717,0.586315445613794,33.2601327471299));
#54084=CARTESIAN_POINT('Ctrl Pts',(33.4738581248639,0.599212556433349,33.2555199153439));
#54085=CARTESIAN_POINT('Ctrl Pts',(33.5711150481712,0.587438679388093,33.2509070835579));
#54086=CARTESIAN_POINT('Ctrl Pts',(33.6683719714784,0.575664802342838,33.246294251772));
#54087=CARTESIAN_POINT('Ctrl Pts',(33.7626422367007,0.539219937432771,33.241681419986));
#54088=CARTESIAN_POINT('Ctrl Pts',(33.8425271973415,0.482510799040096,33.2370685882001));
#54089=CARTESIAN_POINT('Ctrl Pts',(33.9224121579823,0.42580166064742,33.2324557564141));
#54090=CARTESIAN_POINT('Ctrl Pts',(33.9879118140415,0.348828248772135,33.2278429246281));
#54091=CARTESIAN_POINT('Ctrl Pts',(34.0311063042427,0.260897768681385,33.2232300928422));
#54092=CARTESIAN_POINT('Ctrl Pts',(34.0743007944439,0.172967288590632,33.2186172610562));
#54093=CARTESIAN_POINT('Ctrl Pts',(34.095190118787,0.0740797402844121,33.2140044292702));
#54094=CARTESIAN_POINT('Ctrl Pts',(34.0912484540641,-0.0238079330581781,
33.2093915974843));
#54095=CARTESIAN_POINT('Ctrl Pts',(34.0873067893412,-0.121695606400766,
33.2047787656983));
#54096=CARTESIAN_POINT('Ctrl Pts',(34.0585341355524,-0.218583404779724,
33.2001659339123));
#54097=CARTESIAN_POINT('Ctrl Pts',(34.0084095251174,-0.302756183881931,
33.1955531021264));
#54098=CARTESIAN_POINT('Ctrl Pts',(33.9582849146825,-0.386928962984141,
33.1909402703404));
#54099=CARTESIAN_POINT('Ctrl Pts',(33.8868083476014,-0.4583867228096,33.1863274385545));
#54100=CARTESIAN_POINT('Ctrl Pts',(33.8026223806509,-0.508489180650413,
33.1817146067685));
#54101=CARTESIAN_POINT('Ctrl Pts',(33.7184364137004,-0.558591638491224,
33.1771017749825));
#54102=CARTESIAN_POINT('Ctrl Pts',(33.6215410468806,-0.58733879434739,33.1724889431966));
#54103=CARTESIAN_POINT('Ctrl Pts',(33.5236523396421,-0.59125469887231,33.1678761114106));
#54104=CARTESIAN_POINT('Ctrl Pts',(33.4257636324035,-0.595170603397229,
33.1632632796246));
#54105=CARTESIAN_POINT('Ctrl Pts',(33.3268815847462,-0.574255256590902,
33.1586504478387));
#54106=CARTESIAN_POINT('Ctrl Pts',(33.2389624747351,-0.531037628151524,
33.1540376160527));
#54107=CARTESIAN_POINT('Ctrl Pts',(33.151043364724,-0.487819999712145,33.1494247842667));
#54108=CARTESIAN_POINT('Ctrl Pts',(33.0740871923591,-0.422300089639714,
33.1448119524808));
#54109=CARTESIAN_POINT('Ctrl Pts',(33.0173990784123,-0.342400208224076,
33.1401991206948));
#54110=CARTESIAN_POINT('Ctrl Pts',(32.9607109644655,-0.262500326808438,
33.1355862889089));
#54111=CARTESIAN_POINT('Ctrl Pts',(32.9242909089368,-0.168220474049594,
33.1309734571229));
#54112=CARTESIAN_POINT('Ctrl Pts',(32.9125426263666,-0.0709604556981504,
33.1263606253369));
#54113=CARTESIAN_POINT('Ctrl Pts',(32.9097002294358,-0.0474292224314332,
33.1252445899648));
#54114=CARTESIAN_POINT('Ctrl Pts',(32.9083020115649,-0.0237235431388561,
33.1241285545926));
#54115=CARTESIAN_POINT('Ctrl Pts',(32.9083258423465,-1.50708354626494E-5,
33.1230125192205));
#54116=CARTESIAN_POINT('Ctrl Pts',(32.9083212660424,-1.50170003654025E-5,
33.0978374807795));
#54117=CARTESIAN_POINT('Ctrl Pts',(32.9082986535113,-0.0222535883881241,
33.0988843463757));
#54118=CARTESIAN_POINT('Ctrl Pts',(32.9095285404738,-0.0444896728503885,
33.0999312119719));
#54119=CARTESIAN_POINT('Ctrl Pts',(32.9120302473045,-0.0665817363409164,
33.1009780775682));
#54120=CARTESIAN_POINT('Ctrl Pts',(32.9230535848078,-0.163926584671891,
33.1055909093541));
#54121=CARTESIAN_POINT('Ctrl Pts',(32.9587702139371,-0.258475162914329,
33.1102037411401));
#54122=CARTESIAN_POINT('Ctrl Pts',(33.0148614746369,-0.338795172497278,
33.114816572926));
#54123=CARTESIAN_POINT('Ctrl Pts',(33.0709527353366,-0.419115182080227,
33.119429404712));
#54124=CARTESIAN_POINT('Ctrl Pts',(33.1474186276069,-0.485206623003687,
33.124042236498));
#54125=CARTESIAN_POINT('Ctrl Pts',(33.2350133126716,-0.529078078583591,
33.1286550682839));
#54126=CARTESIAN_POINT('Ctrl Pts',(33.3226079977364,-0.572949534163495,
33.1332679000699));
#54127=CARTESIAN_POINT('Ctrl Pts',(33.4213314755957,-0.594601004399844,
33.1378807318559));
#54128=CARTESIAN_POINT('Ctrl Pts',(33.5192466415797,-0.591414511562632,
33.1424935636418));
#54129=CARTESIAN_POINT('Ctrl Pts',(33.6171618075638,-0.58822801872542,33.1471063954278));
#54130=CARTESIAN_POINT('Ctrl Pts',(33.7142686616727,-0.560203562814648,
33.1517192272138));
#54131=CARTESIAN_POINT('Ctrl Pts',(33.7988255725663,-0.510729708240448,
33.1563320589997));
#54132=CARTESIAN_POINT('Ctrl Pts',(33.8833824834599,-0.461255853666247,
33.1609448907857));
#54133=CARTESIAN_POINT('Ctrl Pts',(33.9553894511381,-0.390332600428618,
33.1655577225716));
#54134=CARTESIAN_POINT('Ctrl Pts',(34.0061397856752,-0.306535601612007,
33.1701705543576));
#54135=CARTESIAN_POINT('Ctrl Pts',(34.0568901202122,-0.222738602795397,
33.1747833861436));
#54136=CARTESIAN_POINT('Ctrl Pts',(34.0863838216081,-0.12606785839981,33.1793962179295));
#54137=CARTESIAN_POINT('Ctrl Pts',(34.0910546722994,-0.0282122677567023,
33.1840090497155));
#54138=CARTESIAN_POINT('Ctrl Pts',(34.0957255229907,0.069643322886404,33.1886218815015));
#54139=CARTESIAN_POINT('Ctrl Pts',(34.0755735229775,0.168683759777027,33.1932347132874));
#54140=CARTESIAN_POINT('Ctrl Pts',(34.0330353422259,0.256933613287628,33.1978475450734));
#54141=CARTESIAN_POINT('Ctrl Pts',(33.9904971614744,0.34518346679823,33.2024603768593));
#54142=CARTESIAN_POINT('Ctrl Pts',(33.9255727999844,0.42264273692881,33.2070732086453));
#54143=CARTESIAN_POINT('Ctrl Pts',(33.8461125575585,0.479945471068623,33.2116860404313));
#54144=CARTESIAN_POINT('Ctrl Pts',(33.7666523151326,0.537248205208437,33.2162988722173));
#54145=CARTESIAN_POINT('Ctrl Pts',(33.6726561917706,0.574394403357483,33.2209117040032));
#54146=CARTESIAN_POINT('Ctrl Pts',(33.5754896862115,0.586892549769198,33.2255245357892));
#54147=CARTESIAN_POINT('Ctrl Pts',(33.4783231806524,0.599390696180913,33.2301373675751));
#54148=CARTESIAN_POINT('Ctrl Pts',(33.377986292896,0.587240790855296,33.2347501993611));
#54149=CARTESIAN_POINT('Ctrl Pts',(33.2866112123404,0.551911934098445,33.2393630311471));
#54150=CARTESIAN_POINT('Ctrl Pts',(33.1952361317848,0.516583077341593,33.243975862933));
#54151=CARTESIAN_POINT('Ctrl Pts',(33.1128228584299,0.458075269153507,33.248588694719));
#54152=CARTESIAN_POINT('Ctrl Pts',(33.0493363559447,0.383462954697623,33.253201526505));
#54153=CARTESIAN_POINT('Ctrl Pts',(32.9858498534595,0.308850640241739,33.2578143582909));
#54154=CARTESIAN_POINT('Ctrl Pts',(32.9412901218441,0.218133819518058,33.2624271900769));
#54155=CARTESIAN_POINT('Ctrl Pts',(32.9210450808922,0.122281475867587,33.2670400218629));
#54156=CARTESIAN_POINT('Ctrl Pts',(32.9125636824346,0.0821253743546122,
33.2689725081684));
#54157=CARTESIAN_POINT('Ctrl Pts',(32.9083497135586,0.0410679460364483,
33.270904994474));
#54158=CARTESIAN_POINT('Ctrl Pts',(32.9083669931439,7.02104240262066E-6,
33.2728374807795));
#54159=CARTESIAN_POINT('Origin',(33.5,0.,32.675));
#54160=CARTESIAN_POINT('',(32.9082801122102,1.43778562331377E-5,33.4730125192205));
#54161=CARTESIAN_POINT('',(32.9082781605688,6.35800992875699E-6,33.4478374807795));
#54162=CARTESIAN_POINT('',(32.908325,-7.2459289488551E-17,32.675));
#54163=CARTESIAN_POINT('Ctrl Pts',(32.9082801122102,1.43778562331377E-5,
33.4730125192205));
#54164=CARTESIAN_POINT('Ctrl Pts',(32.9082777494417,0.0048957297300282,
33.4727826825751));
#54165=CARTESIAN_POINT('Ctrl Pts',(32.9083367376185,0.00977701899879359,
33.4725528459296));
#54166=CARTESIAN_POINT('Ctrl Pts',(32.9084574135329,0.0146567689798401,
33.4723230092842));
#54167=CARTESIAN_POINT('Ctrl Pts',(32.9108793845494,0.112593570044052,33.4677101774982));
#54168=CARTESIAN_POINT('Ctrl Pts',(32.9381495896478,0.209910335700311,33.4630973457123));
#54169=CARTESIAN_POINT('Ctrl Pts',(32.9869645530622,0.29484743325453,33.4584845139263));
#54170=CARTESIAN_POINT('Ctrl Pts',(33.0357795164767,0.379784530808754,33.4538716821404));
#54171=CARTESIAN_POINT('Ctrl Pts',(33.1061392382071,0.452341960260935,33.4492588503544));
#54172=CARTESIAN_POINT('Ctrl Pts',(33.1895385394219,0.503742439857524,33.4446460185684));
#54173=CARTESIAN_POINT('Ctrl Pts',(33.2729378406366,0.555142919454111,33.4400331867825));
#54174=CARTESIAN_POINT('Ctrl Pts',(33.3693767213356,0.585386449195107,33.4354203549965));
#54175=CARTESIAN_POINT('Ctrl Pts',(33.4671930878207,0.590817709657423,33.4308075232105));
#54176=CARTESIAN_POINT('Ctrl Pts',(33.5650094543058,0.59624897011974,33.4261946914246));
#54177=CARTESIAN_POINT('Ctrl Pts',(33.664203306577,0.576867961303377,33.4215818596386));
#54178=CARTESIAN_POINT('Ctrl Pts',(33.7527811584451,0.535017315384049,33.4169690278527));
#54179=CARTESIAN_POINT('Ctrl Pts',(33.8413590103132,0.493166669464721,33.4123561960667));
#54180=CARTESIAN_POINT('Ctrl Pts',(33.9193208617782,0.428846386442427,33.4077433642807));
#54181=CARTESIAN_POINT('Ctrl Pts',(33.9772397414075,0.349834054041184,33.4031305324948));
#54182=CARTESIAN_POINT('Ctrl Pts',(34.0351586210367,0.27082172163994,33.3985177007088));
#54183=CARTESIAN_POINT('Ctrl Pts',(34.0730345288302,0.177117339859746,33.3939048689228));
#54184=CARTESIAN_POINT('Ctrl Pts',(34.0862878201468,0.0800509664060832,
33.3892920371369));
#54185=CARTESIAN_POINT('Ctrl Pts',(34.0995411114634,-0.01701540704758,33.3846792053509));
#54186=CARTESIAN_POINT('Ctrl Pts',(34.0881717863031,-0.117443772174712,
33.3800663735649));
#54187=CARTESIAN_POINT('Ctrl Pts',(34.0535545106543,-0.209090809497847,
33.375453541779));
#54188=CARTESIAN_POINT('Ctrl Pts',(34.0189372350054,-0.300737846820983,
33.370840709993));
#54189=CARTESIAN_POINT('Ctrl Pts',(33.961072008868,-0.383603556340122,33.3662278782071));
#54190=CARTESIAN_POINT('Ctrl Pts',(33.8869556015323,-0.447668301971417,
33.3616150464211));
#54191=CARTESIAN_POINT('Ctrl Pts',(33.8128391941966,-0.511733047602713,
33.3570022146351));
#54192=CARTESIAN_POINT('Ctrl Pts',(33.7224716056626,-0.556996829346165,
33.3523893828492));
#54193=CARTESIAN_POINT('Ctrl Pts',(33.6267795816305,-0.577986583078156,
33.3477765510632));
#54194=CARTESIAN_POINT('Ctrl Pts',(33.5310875575984,-0.598976336810146,
33.3431637192772));
#54195=CARTESIAN_POINT('Ctrl Pts',(33.4300710980682,-0.595692062530675,
33.3385508874913));
#54196=CARTESIAN_POINT('Ctrl Pts',(33.3359445670576,-0.568530883674471,
33.3339380557053));
#54197=CARTESIAN_POINT('Ctrl Pts',(33.241818036047,-0.541369704818268,33.3293252239193));
#54198=CARTESIAN_POINT('Ctrl Pts',(33.154581433556,-0.490331621385331,33.3247123921334));
#54199=CARTESIAN_POINT('Ctrl Pts',(33.0847829317848,-0.421587877146135,
33.3200995603474));
#54200=CARTESIAN_POINT('Ctrl Pts',(33.0149844300136,-0.352844132906939,
33.3154867285614));
#54201=CARTESIAN_POINT('Ctrl Pts',(32.9626240289621,-0.266394727861483,
33.3108738967755));
#54202=CARTESIAN_POINT('Ctrl Pts',(32.9340328637752,-0.172692654131546,
33.3062610649895));
#54203=CARTESIAN_POINT('Ctrl Pts',(32.9169908712366,-0.11684078412505,33.3035115497332));
#54204=CARTESIAN_POINT('Ctrl Pts',(32.9083937347762,-0.0584121487748326,
33.3007620344768));
#54205=CARTESIAN_POINT('Ctrl Pts',(32.9083649252952,8.19085268685682E-6,
33.2980125192205));
#54206=CARTESIAN_POINT('Ctrl Pts',(32.9083669931439,7.02104240262066E-6,
33.2728374807795));
#54207=CARTESIAN_POINT('Ctrl Pts',(32.9083909598124,-0.0569442051646274,
33.2755178262599));
#54208=CARTESIAN_POINT('Ctrl Pts',(32.916554791989,-0.113902158102944,33.2781981717403));
#54209=CARTESIAN_POINT('Ctrl Pts',(32.9327619501703,-0.168471221650837,
33.2808785172207));
#54210=CARTESIAN_POINT('Ctrl Pts',(32.9606542106887,-0.262383708941532,
33.2854913490067));
#54211=CARTESIAN_POINT('Ctrl Pts',(33.0123690820137,-0.349220816945665,
33.2901041807927));
#54212=CARTESIAN_POINT('Ctrl Pts',(33.0816534838775,-0.418482676041528,
33.2947170125786));
#54213=CARTESIAN_POINT('Ctrl Pts',(33.1509378857413,-0.487744535137393,
33.2993298443646));
#54214=CARTESIAN_POINT('Ctrl Pts',(33.2377918181438,-0.539431145324988,
33.3039426761506));
#54215=CARTESIAN_POINT('Ctrl Pts',(33.3317133771216,-0.567292843483501,
33.3085555079365));
#54216=CARTESIAN_POINT('Ctrl Pts',(33.4256349360993,-0.595154541642011,
33.3131683397225));
#54217=CARTESIAN_POINT('Ctrl Pts',(33.5266241216523,-0.599191327771441,
33.3177811715085));
#54218=CARTESIAN_POINT('Ctrl Pts',(33.6224698721195,-0.578915095768528,
33.3223940032944));
#54219=CARTESIAN_POINT('Ctrl Pts',(33.7183156225867,-0.558638863765614,
33.3270068350804));
#54220=CARTESIAN_POINT('Ctrl Pts',(33.8090179379681,-0.514049613630359,
33.3316196668663));
#54221=CARTESIAN_POINT('Ctrl Pts',(33.8836095887596,-0.45053883423155,33.3362324986523));
#54222=CARTESIAN_POINT('Ctrl Pts',(33.9582012395511,-0.387028054832742,
33.3408453304383));
#54223=CARTESIAN_POINT('Ctrl Pts',(34.0166822257528,-0.304595746170383,
33.3454581622242));
#54224=CARTESIAN_POINT('Ctrl Pts',(34.0519813455136,-0.213209173878463,
33.3500709940102));
#54225=CARTESIAN_POINT('Ctrl Pts',(34.0872804652743,-0.121822601586543,
33.3546838257962));
#54226=CARTESIAN_POINT('Ctrl Pts',(34.0993977185941,-0.0214817656650577,
33.3592966575821));
#54227=CARTESIAN_POINT('Ctrl Pts',(34.0868679529414,0.0756806677846,33.3639094893681));
#54228=CARTESIAN_POINT('Ctrl Pts',(34.0743381872887,0.172843101234259,33.3685223211541));
#54229=CARTESIAN_POINT('Ctrl Pts',(34.0371614026635,0.26682713221209,33.37313515294));
#54230=CARTESIAN_POINT('Ctrl Pts',(33.9798328138488,0.346268722574251,33.377747984726));
#54231=CARTESIAN_POINT('Ctrl Pts',(33.9225042250342,0.425710312936409,33.382360816512));
#54232=CARTESIAN_POINT('Ctrl Pts',(33.8450238320301,0.490609462682893,33.3869736482979));
#54233=CARTESIAN_POINT('Ctrl Pts',(33.7567601399104,0.533118923790534,33.3915864800839));
#54234=CARTESIAN_POINT('Ctrl Pts',(33.6684964477907,0.575628384898177,33.3961993118699));
#54235=CARTESIAN_POINT('Ctrl Pts',(33.5694494565553,0.595748157366975,33.4008121436558));
#54236=CARTESIAN_POINT('Ctrl Pts',(33.471595391638,0.591045460461492,33.4054249754418));
#54237=CARTESIAN_POINT('Ctrl Pts',(33.3737413267206,0.586342763556009,33.4100378072277));
#54238=CARTESIAN_POINT('Ctrl Pts',(33.2770801881214,0.556817597276246,33.4146506390137));
#54239=CARTESIAN_POINT('Ctrl Pts',(33.1932997058521,0.506039999696235,33.4192634707997));
#54240=CARTESIAN_POINT('Ctrl Pts',(33.1095192235828,0.455262402116224,33.4238763025856));
#54241=CARTESIAN_POINT('Ctrl Pts',(33.0386193976434,0.383232373235965,33.4284891343716));
#54242=CARTESIAN_POINT('Ctrl Pts',(32.9891730641268,0.298659354587987,33.4331019661576));
#54243=CARTESIAN_POINT('Ctrl Pts',(32.9397267306103,0.214086335940007,33.4377147979435));
#54244=CARTESIAN_POINT('Ctrl Pts',(32.9117338895166,0.116970327524307,33.4423276297295));
#54245=CARTESIAN_POINT('Ctrl Pts',(32.9085792439848,0.0190541441652503,
33.4469404615155));
#54246=CARTESIAN_POINT('Ctrl Pts',(32.9083747580389,0.0127071605905036,
33.4472394679368));
#54247=CARTESIAN_POINT('Ctrl Pts',(32.9082746349205,0.00635681491485789,
33.4475384743582));
#54248=CARTESIAN_POINT('Ctrl Pts',(32.9082781605688,6.35800992875699E-6,
33.4478374807795));
#54249=CARTESIAN_POINT('Origin',(33.5,0.,31.5181609435991));
#54250=CARTESIAN_POINT('',(33.0082081875748,6.80857923756794E-6,33.3556609435991));
#54251=CARTESIAN_POINT('',(33.0081360651062,5.28504368550037E-6,33.3901890564009));
#54252=CARTESIAN_POINT('',(33.008175,-2.33277202951234E-14,31.5181609435991));
#54253=CARTESIAN_POINT('',(33.2772637232776,0.4385197762278,33.5));
#54254=CARTESIAN_POINT('Ctrl Pts',(33.0082081875748,6.8085792375612E-6,
33.3556609435991));
#54255=CARTESIAN_POINT('Ctrl Pts',(33.00823213522,-0.0485546204777694,33.3584104588554));
#54256=CARTESIAN_POINT('Ctrl Pts',(33.0273677029933,-0.178605494601613,
33.3657728058977));
#54257=CARTESIAN_POINT('Ctrl Pts',(33.1403589327563,-0.365159157144441,
33.377747984726));
#54258=CARTESIAN_POINT('Ctrl Pts',(33.3579030677296,-0.492434124234837,
33.3915864800839));
#54259=CARTESIAN_POINT('Ctrl Pts',(33.609810382768,-0.500624202559088,33.4054249754418));
#54260=CARTESIAN_POINT('Ctrl Pts',(33.8351623372906,-0.3877487584928,33.4192634707997));
#54261=CARTESIAN_POINT('Ctrl Pts',(33.9794623238291,-0.181104430520942,
33.4331019661576));
#54262=CARTESIAN_POINT('Ctrl Pts',(34.0078142992225,0.069336338543082,33.4469404615154));
#54263=CARTESIAN_POINT('Ctrl Pts',(33.9133621843763,0.303009339273432,33.4607789568733));
#54264=CARTESIAN_POINT('Ctrl Pts',(33.7189467319906,0.463406465385431,33.4746174522312));
#54265=CARTESIAN_POINT('Ctrl Pts',(33.4852555067653,0.509066267809633,33.4876911332735));
#54266=CARTESIAN_POINT('Ctrl Pts',(33.3378705446427,0.469227417544844,33.4961519825297));
#54267=CARTESIAN_POINT('Ctrl Pts',(33.2772637232776,0.4385197762278,33.5));
#54268=CARTESIAN_POINT('',(33.8422870473583,0.353173339644655,33.5));
#54269=CARTESIAN_POINT('Origin',(33.5,0.,33.5));
#54270=CARTESIAN_POINT('Ctrl Pts',(33.0081360651062,5.28504368550904E-6,
33.3901890564009));
#54271=CARTESIAN_POINT('Ctrl Pts',(33.0081783464134,-0.0761525165286589,
33.3945028817655));
#54272=CARTESIAN_POINT('Ctrl Pts',(33.0453750663556,-0.233786708256313,
33.4034295389161));
#54273=CARTESIAN_POINT('Ctrl Pts',(33.2066887031424,-0.420299550020602,
33.4169690278527));
#54274=CARTESIAN_POINT('Ctrl Pts',(33.4424952770395,-0.509289505109944,
33.4308075232105));
#54275=CARTESIAN_POINT('Ctrl Pts',(33.6922091923902,-0.47512167024108,33.4446460185684));
#54276=CARTESIAN_POINT('Ctrl Pts',(33.8954376101786,-0.326050114606906,
33.4584845139263));
#54277=CARTESIAN_POINT('Ctrl Pts',(34.003042111098,-0.0981464483443762,
33.4723230092842));
#54278=CARTESIAN_POINT('Ctrl Pts',(33.9889768845264,0.153516958914333,33.4861615046421));
#54279=CARTESIAN_POINT('Ctrl Pts',(33.9007791656288,0.296484195224244,33.495387168214));
#54280=CARTESIAN_POINT('Ctrl Pts',(33.8422870473583,0.35317333964466,33.5));
#54281=CARTESIAN_POINT('Origin',(33.5,0.,31.5181609435991));
#54282=CARTESIAN_POINT('',(33.0081757001937,-1.25275086047875E-5,33.1806609435991));
#54283=CARTESIAN_POINT('',(33.0082099064571,5.83618400502861E-6,33.2151890564009));
#54284=CARTESIAN_POINT('',(33.008175,-2.33277202951234E-14,31.5181609435991));
#54285=CARTESIAN_POINT('Ctrl Pts',(33.0081757001937,-1.25275086048302E-5,
33.1806609435991));
#54286=CARTESIAN_POINT('Ctrl Pts',(33.0081558910515,-0.0197200010212862,
33.1817769789712));
#54287=CARTESIAN_POINT('Ctrl Pts',(33.0141220253085,-0.120871093602866,
33.1875058461293));
#54288=CARTESIAN_POINT('Ctrl Pts',(33.0819942771093,-0.29657060348279,33.1978475450734));
#54289=CARTESIAN_POINT('Ctrl Pts',(33.2739018419382,-0.459959270088812,
33.2116860404313));
#54290=CARTESIAN_POINT('Ctrl Pts',(33.5204865197886,-0.512116402516352,
33.2255245357892));
#54291=CARTESIAN_POINT('Ctrl Pts',(33.7621169610925,-0.440428888616189,
33.2393630311471));
#54292=CARTESIAN_POINT('Ctrl Pts',(33.9403598948212,-0.262232855019252,
33.253201526505));
#54293=CARTESIAN_POINT('Ctrl Pts',(34.0121109935648,-0.0206212873288921,
33.2670400218628));
#54294=CARTESIAN_POINT('Ctrl Pts',(33.9600187540159,0.225977107629683,33.2808785172207));
#54295=CARTESIAN_POINT('Ctrl Pts',(33.7966805953577,0.417927663064147,33.2947170125786));
#54296=CARTESIAN_POINT('Ctrl Pts',(33.5615964366915,0.50881114986548,33.3085555079365));
#54297=CARTESIAN_POINT('Ctrl Pts',(33.3116164675281,0.476649296505977,33.3223940032944));
#54298=CARTESIAN_POINT('Ctrl Pts',(33.1071931174629,0.329219775186188,33.3362324986523));
#54299=CARTESIAN_POINT('Ctrl Pts',(33.0195043512237,0.14728588453292,33.3473214787539));
#54300=CARTESIAN_POINT('Ctrl Pts',(33.0081919585165,0.0329163599102017,
33.3537976270694));
#54301=CARTESIAN_POINT('Ctrl Pts',(33.0082081875748,6.8085792375612E-6,
33.3556609435991));
#54302=CARTESIAN_POINT('Ctrl Pts',(33.0082099064571,5.83618400500432E-6,
33.2151890564009));
#54303=CARTESIAN_POINT('Ctrl Pts',(33.0082298285541,-0.0473344043691201,
33.2178694018813));
#54304=CARTESIAN_POINT('Ctrl Pts',(33.0266947491123,-0.176161657723165,
33.2251625791477));
#54305=CARTESIAN_POINT('Ctrl Pts',(33.1376483548415,-0.362469580324392,
33.2370685882));
#54306=CARTESIAN_POINT('Ctrl Pts',(33.35423821568,-0.491361795081716,33.2509070835579));
#54307=CARTESIAN_POINT('Ctrl Pts',(33.6060775169075,-0.501428431350477,
33.2647455789158));
#54308=CARTESIAN_POINT('Ctrl Pts',(33.8322641882851,-0.390235083915959,
33.2785840742737));
#54309=CARTESIAN_POINT('Ctrl Pts',(33.978099711361,-0.184671538686574,33.2924225696316));
#54310=CARTESIAN_POINT('Ctrl Pts',(34.0083168142334,0.0655509565705277,
33.3062610649895));
#54311=CARTESIAN_POINT('Ctrl Pts',(33.915608120618,0.299921325619444,33.3200995603474));
#54312=CARTESIAN_POINT('Ctrl Pts',(33.7223932934449,0.461761986408213,33.3339380557053));
#54313=CARTESIAN_POINT('Ctrl Pts',(33.4753972915975,0.511935174870455,33.3477765510632));
#54314=CARTESIAN_POINT('Ctrl Pts',(33.2343509511662,0.438307516584007,33.3616150464211));
#54315=CARTESIAN_POINT('Ctrl Pts',(33.057546251495,0.258684401086308,33.375453541779));
#54316=CARTESIAN_POINT('Ctrl Pts',(33.0095003131485,0.0919978637254616,
33.3849782117723));
#54317=CARTESIAN_POINT('Ctrl Pts',(33.00813313444,0.00528405035786898,33.3898900499796));
#54318=CARTESIAN_POINT('Ctrl Pts',(33.0081360651062,5.28504368550904E-6,
33.3901890564009));
#54319=CARTESIAN_POINT('Origin',(33.5,0.,31.5181609435991));
#54320=CARTESIAN_POINT('',(33.0081442881972,8.55461989747011E-6,33.0056609435991));
#54321=CARTESIAN_POINT('',(33.0081718961783,-1.24827586314713E-5,33.0401890564009));
#54322=CARTESIAN_POINT('',(33.008175,-2.33277202951234E-14,31.5181609435991));
#54323=CARTESIAN_POINT('Ctrl Pts',(33.0081442881972,8.55461989746759E-6,
33.0056609435991));
#54324=CARTESIAN_POINT('Ctrl Pts',(33.0082032482984,-0.072296377421353,
33.009756330873));
#54325=CARTESIAN_POINT('Ctrl Pts',(33.0425319114762,-0.226095971754384,
33.0184645499329));
#54326=CARTESIAN_POINT('Ctrl Pts',(33.1968818152122,-0.413282316667997,
33.0317856007787));
#54327=CARTESIAN_POINT('Ctrl Pts',(33.4305301017064,-0.507796061869929,
33.0456240961366));
#54328=CARTESIAN_POINT('Ctrl Pts',(33.6809782308582,-0.47950994481343,33.0594625914945));
#54329=CARTESIAN_POINT('Ctrl Pts',(33.8876605581656,-0.33526437159691,33.0733010868524));
#54330=CARTESIAN_POINT('Ctrl Pts',(34.0005952833934,-0.109942118697895,
33.0871395822102));
#54331=CARTESIAN_POINT('Ctrl Pts',(33.9924715041075,0.141967337305424,33.1009780775682));
#54332=CARTESIAN_POINT('Ctrl Pts',(33.8652537865034,0.359544960560564,33.114816572926));
#54333=CARTESIAN_POINT('Ctrl Pts',(33.6497070761401,0.490174151269844,33.1286550682839));
#54334=CARTESIAN_POINT('Ctrl Pts',(33.3979568389882,0.502264970419248,33.1424935636418));
#54335=CARTESIAN_POINT('Ctrl Pts',(33.1708836071492,0.392893506151966,33.1563320589997));
#54336=CARTESIAN_POINT('Ctrl Pts',(33.0352944053819,0.20499199420157,33.1690545189855));
#54337=CARTESIAN_POINT('Ctrl Pts',(33.0082377668081,0.0617355357021187,
33.1771641471852));
#54338=CARTESIAN_POINT('Ctrl Pts',(33.0081757001937,-1.25275086048302E-5,
33.1806609435991));
#54339=CARTESIAN_POINT('Ctrl Pts',(33.0081718961783,-1.24827586314418E-5,
33.0401890564009));
#54340=CARTESIAN_POINT('Ctrl Pts',(33.008153099697,-0.0184981131685394,
33.0412359219971));
#54341=CARTESIAN_POINT('Ctrl Pts',(33.0136801683864,-0.118426293523507,
33.0468956193793));
#54342=CARTESIAN_POINT('Ctrl Pts',(33.0797963266846,-0.293448094806149,
33.0571681485475));
#54343=CARTESIAN_POINT('Ctrl Pts',(33.2704812675685,-0.458262002435405,
33.0710066439053));
#54344=CARTESIAN_POINT('Ctrl Pts',(33.5166705158794,-0.512254824587727,
33.0848451392633));
#54345=CARTESIAN_POINT('Ctrl Pts',(33.7588283484165,-0.442369525927234,
33.0986836346211));
#54346=CARTESIAN_POINT('Ctrl Pts',(33.938393955608,-0.265506405006475,33.112522129979));
#54347=CARTESIAN_POINT('Ctrl Pts',(34.011943149113,-0.0244361103564004,
33.1263606253369));
#54348=CARTESIAN_POINT('Ctrl Pts',(33.9616895940033,0.222543546754668,33.1401991206948));
#54349=CARTESIAN_POINT('Ctrl Pts',(33.7997860620486,0.41570569928083,33.1540376160527));
#54350=CARTESIAN_POINT('Ctrl Pts',(33.5653855379137,0.508338118622465,33.1678761114106));
#54351=CARTESIAN_POINT('Ctrl Pts',(33.3151728882965,0.478039590612468,33.1817146067685));
#54352=CARTESIAN_POINT('Ctrl Pts',(33.1096568118975,0.332137180866717,33.1955531021264));
#54353=CARTESIAN_POINT('Ctrl Pts',(33.0200595948244,0.149730905427,33.2067112520039));
#54354=CARTESIAN_POINT('Ctrl Pts',(33.0081955429432,0.034137393939865,33.2132565700954));
#54355=CARTESIAN_POINT('Ctrl Pts',(33.0082099064571,5.83618400500432E-6,
33.2151890564009));
#54356=CARTESIAN_POINT('Origin',(33.5,0.,31.5181609435991));
#54357=CARTESIAN_POINT('',(33.0082134963911,2.50469452055408E-6,32.8306609435991));
#54358=CARTESIAN_POINT('',(33.0081474500214,9.4085289371465E-6,32.8651890564009));
#54359=CARTESIAN_POINT('',(33.008175,-2.33277202951234E-14,31.5181609435991));
#54360=CARTESIAN_POINT('Ctrl Pts',(33.0082134963911,2.50469452055951E-6,
32.8306609435991));
#54361=CARTESIAN_POINT('Ctrl Pts',(33.0082212784349,-0.0434805911909761,
32.8331228509888));
#54362=CARTESIAN_POINT('Ctrl Pts',(33.0246360156411,-0.168442948739724,
32.8401975901645));
#54363=CARTESIAN_POINT('Ctrl Pts',(33.1292211252569,-0.353844504357231,
32.8518851611261));
#54364=CARTESIAN_POINT('Ctrl Pts',(33.3427186957223,-0.487796574961559,
32.865723656484));
#54365=CARTESIAN_POINT('Ctrl Pts',(33.5942514617147,-0.503785241133738,
32.8795621518419));
#54366=CARTESIAN_POINT('Ctrl Pts',(33.8229914819863,-0.397943978197684,
32.8934006471998));
#54367=CARTESIAN_POINT('Ctrl Pts',(33.9736227643672,-0.195868283018701,
32.9072391425577));
#54368=CARTESIAN_POINT('Ctrl Pts',(34.0097182821095,0.0535740618481902,
32.9210776379156));
#54369=CARTESIAN_POINT('Ctrl Pts',(33.9225490888117,0.290060639804727,32.9349161332734));
#54370=CARTESIAN_POINT('Ctrl Pts',(33.7331952316305,0.456402115643996,32.9487546286313));
#54371=CARTESIAN_POINT('Ctrl Pts',(33.4874479825469,0.512372280746522,32.9625931239892));
#54372=CARTESIAN_POINT('Ctrl Pts',(33.2447361764886,0.44443592071962,32.9764316193471));
#54373=CARTESIAN_POINT('Ctrl Pts',(33.0637545899428,0.269022024049182,32.990270114705));
#54374=CARTESIAN_POINT('Ctrl Pts',(33.0106089194897,0.0997162351515044,
33.000013222789));
#54375=CARTESIAN_POINT('Ctrl Pts',(33.0081368386988,0.00914414736771318,
33.005143499087));
#54376=CARTESIAN_POINT('Ctrl Pts',(33.0081442881972,8.55461989746759E-6,
33.0056609435991));
#54377=CARTESIAN_POINT('Ctrl Pts',(33.0081474500215,9.40852893713609E-6,
32.8651890564009));
#54378=CARTESIAN_POINT('Ctrl Pts',(33.0082096067412,-0.0710756417150838,
32.8692152738989));
#54379=CARTESIAN_POINT('Ctrl Pts',(33.0416543158414,-0.223659323266138,
32.8778543231829));
#54380=CARTESIAN_POINT('Ctrl Pts',(33.1938111364897,-0.411012519609046,
32.8911062042528));
#54381=CARTESIAN_POINT('Ctrl Pts',(33.4267487816945,-0.507264398937922,
32.9049446996107));
#54382=CARTESIAN_POINT('Ctrl Pts',(33.6774007027546,-0.480844987574239,
32.9187831949685));
#54383=CARTESIAN_POINT('Ctrl Pts',(33.8851519723551,-0.338143267867451,
32.9326216903264));
#54384=CARTESIAN_POINT('Ctrl Pts',(33.9997622889131,-0.113668667597491,
32.9464601856843));
#54385=CARTESIAN_POINT('Ctrl Pts',(33.9935155432591,0.138294323725898,32.9602986810422));
#54386=CARTESIAN_POINT('Ctrl Pts',(33.8679223802432,0.35681372385221,32.9741371764001));
#54387=CARTESIAN_POINT('Ctrl Pts',(33.6533548808583,0.489045183934999,32.987975671758));
#54388=CARTESIAN_POINT('Ctrl Pts',(33.4017017093698,0.503011289607162,33.0018141671159));
#54389=CARTESIAN_POINT('Ctrl Pts',(33.1738199245776,0.395334630168599,33.0156526624738));
#54390=CARTESIAN_POINT('Ctrl Pts',(33.0360897915344,0.207432448948863,33.0284442922355));
#54391=CARTESIAN_POINT('Ctrl Pts',(33.0082359231337,0.0629556129320961,
33.0366230902112));
#54392=CARTESIAN_POINT('Ctrl Pts',(33.0081718961783,-1.24827586314418E-5,
33.0401890564009));
#54393=CARTESIAN_POINT('Origin',(33.5,0.,31.5181609435991));
#54394=CARTESIAN_POINT('',(33.0081598637556,-1.16166009309924E-5,32.6556609435991));
#54395=CARTESIAN_POINT('',(33.0082140178674,1.39678807051236E-6,32.6901890564009));
#54396=CARTESIAN_POINT('',(33.008175,-2.33277202951234E-14,31.5181609435991));
#54397=CARTESIAN_POINT('Ctrl Pts',(33.0081598637556,-1.16166009310036E-5,
32.6556609435991));
#54398=CARTESIAN_POINT('Ctrl Pts',(33.0081452355548,-0.0146390191282887,
32.6564893711046));
#54399=CARTESIAN_POINT('Ctrl Pts',(33.0123466239008,-0.110706028793147,
32.6619306303961));
#54400=CARTESIAN_POINT('Ctrl Pts',(33.073008921504,-0.283481085972825,32.6719847214735));
#54401=CARTESIAN_POINT('Ctrl Pts',(33.2597636420402,-0.452735463083817,
32.6858232168314));
#54402=CARTESIAN_POINT('Ctrl Pts',(33.5046145036892,-0.512505232729617,
32.6996617121893));
#54403=CARTESIAN_POINT('Ctrl Pts',(33.7483494440856,-0.448336325588192,
32.7135002075472));
#54404=CARTESIAN_POINT('Ctrl Pts',(33.932026263091,-0.27574665042241,32.7273387029051));
#54405=CARTESIAN_POINT('Ctrl Pts',(34.0112265617306,-0.0364734122423689,
32.741177198263));
#54406=CARTESIAN_POINT('Ctrl Pts',(33.966797403434,0.211620158224149,32.7550156936209));
#54407=CARTESIAN_POINT('Ctrl Pts',(33.8094830513586,0.408537817271942,32.7688541889788));
#54408=CARTESIAN_POINT('Ctrl Pts',(33.5773266929505,0.506659145557318,32.7826926843366));
#54409=CARTESIAN_POINT('Ctrl Pts',(33.3264704903407,0.482255551027616,32.7965311796945));
#54410=CARTESIAN_POINT('Ctrl Pts',(33.1175787720664,0.341228532870962,32.8103696750524));
#54411=CARTESIAN_POINT('Ctrl Pts',(33.0218775035777,0.157451992758215,32.8217462630206));
#54412=CARTESIAN_POINT('Ctrl Pts',(33.0082066973589,0.0379929068337176,
32.8285100192028));
#54413=CARTESIAN_POINT('Ctrl Pts',(33.0082134963911,2.50469452055951E-6,
32.8306609435991));
#54414=CARTESIAN_POINT('Ctrl Pts',(33.0082140178674,1.39678807050542E-6,
32.6901890564009));
#54415=CARTESIAN_POINT('Ctrl Pts',(33.0082182302214,-0.0422601271102193,
32.6925817940147));
#54416=CARTESIAN_POINT('Ctrl Pts',(33.024005016889,-0.16599848794156,32.6995873634144));
#54417=CARTESIAN_POINT('Ctrl Pts',(33.1265951550888,-0.351072262091296,
32.7112057646002));
#54418=CARTESIAN_POINT('Ctrl Pts',(33.3390888148842,-0.486611243106551,
32.7250442599581));
#54419=CARTESIAN_POINT('Ctrl Pts',(33.590495481006,-0.504473467419831,32.7388827553159));
#54420=CARTESIAN_POINT('Ctrl Pts',(33.8200177068239,-0.400339329484723,
32.7527212506738));
#54421=CARTESIAN_POINT('Ctrl Pts',(33.9721503401083,-0.199391493671923,
32.7665597460317));
#54422=CARTESIAN_POINT('Ctrl Pts',(34.0101032837806,0.0497750066737403,
32.7803982413896));
#54423=CARTESIAN_POINT('Ctrl Pts',(33.924698411807,0.286904462185027,32.7942367367475));
#54424=CARTESIAN_POINT('Ctrl Pts',(33.7365891071145,0.454652071157545,32.8080752321054));
#54425=CARTESIAN_POINT('Ctrl Pts',(33.4912656726816,0.512451581068282,32.8219137274633));
#54426=CARTESIAN_POINT('Ctrl Pts',(33.2480544527224,0.446325388724518,32.8357522228212));
#54427=CARTESIAN_POINT('Ctrl Pts',(33.065770996536,0.272264731398925,32.8495907181791));
#54428=CARTESIAN_POINT('Ctrl Pts',(33.0109791724204,0.102160475369954,32.859402996039));
#54429=CARTESIAN_POINT('Ctrl Pts',(33.0081383938739,0.010366401452443,32.8646024421129));
#54430=CARTESIAN_POINT('Ctrl Pts',(33.0081474500215,9.40852893713609E-6,
32.8651890564009));
#54431=CARTESIAN_POINT('Origin',(33.5,0.,31.5181609435991));
#54432=CARTESIAN_POINT('',(33.0081586006607,1.14590643093381E-5,32.4806609435991));
#54433=CARTESIAN_POINT('',(33.0081561516106,-1.11148368504288E-5,32.5151890564009));
#54434=CARTESIAN_POINT('',(33.008175,-2.33277202951234E-14,31.5181609435991));
#54435=CARTESIAN_POINT('Ctrl Pts',(33.0081586006607,1.14590643093392E-5,
32.4806609435991));
#54436=CARTESIAN_POINT('Ctrl Pts',(33.0082253678877,-0.067221351242673,
32.4844687230064));
#54437=CARTESIAN_POINT('Ctrl Pts',(33.0389540671597,-0.215960692626971,
32.4928893341996));
#54438=CARTESIAN_POINT('Ctrl Pts',(33.1842263319695,-0.403695303165732,
32.5059227771788));
#54439=CARTESIAN_POINT('Ctrl Pts',(33.4148350642942,-0.505400673669678,
32.5197612725367));
#54440=CARTESIAN_POINT('Ctrl Pts',(33.6660391559753,-0.484885456476644,
32.5335997678946));
#54441=CARTESIAN_POINT('Ctrl Pts',(33.877090148776,-0.347110828001091,32.5474382632525));
#54442=CARTESIAN_POINT('Ctrl Pts',(33.9969497720373,-0.125394702007854,
32.5612767586104));
#54443=CARTESIAN_POINT('Ctrl Pts',(33.9966324814981,0.126645511332176,32.5751152539683));
#54444=CARTESIAN_POINT('Ctrl Pts',(33.8762150072425,0.348059155238069,32.5889537493262));
#54445=CARTESIAN_POINT('Ctrl Pts',(33.6648177981328,0.485301968508477,32.6027922446841));
#54446=CARTESIAN_POINT('Ctrl Pts',(33.4135628500049,0.505184645768512,32.616630740042));
#54447=CARTESIAN_POINT('Ctrl Pts',(33.1832109196639,0.402898977163472,32.6304692353998));
#54448=CARTESIAN_POINT('Ctrl Pts',(33.0386714817818,0.215136550920342,32.6434793032522));
#54449=CARTESIAN_POINT('Ctrl Pts',(33.0082266879799,0.066808961383216,32.6518765393186));
#54450=CARTESIAN_POINT('Ctrl Pts',(33.0081598637556,-1.16166009310036E-5,
32.6556609435991));
#54451=CARTESIAN_POINT('Ctrl Pts',(33.0081561516106,-1.11148368504149E-5,
32.5151890564009));
#54452=CARTESIAN_POINT('Ctrl Pts',(33.0081430634381,-0.0134169068216723,
32.5159483141305));
#54453=CARTESIAN_POINT('Ctrl Pts',(33.0119438329651,-0.108261507241117,
32.5213204036461));
#54454=CARTESIAN_POINT('Ctrl Pts',(33.0709087415947,-0.280291996627235,
32.5313053249476));
#54455=CARTESIAN_POINT('Ctrl Pts',(33.2563972796865,-0.450933061627702,
32.5451438203055));
#54456=CARTESIAN_POINT('Ctrl Pts',(33.5007960432536,-0.512525392276544,
32.5589823156633));
#54457=CARTESIAN_POINT('Ctrl Pts',(33.7450023004009,-0.450174170973167,
32.5728208110213));
#54458=CARTESIAN_POINT('Ctrl Pts',(33.9299598728863,-0.278957737158612,
32.5866593063791));
#54459=CARTESIAN_POINT('Ctrl Pts',(34.0109406382799,-0.0402812061293292,
32.600497801737));
#54460=CARTESIAN_POINT('Ctrl Pts',(33.9683610913465,0.208136492537349,32.6143362970949));
#54461=CARTESIAN_POINT('Ctrl Pts',(33.8125182054012,0.406220731506804,32.6281747924528));
#54462=CARTESIAN_POINT('Ctrl Pts',(33.5810993245668,0.506068978468246,32.6420132878107));
#54463=CARTESIAN_POINT('Ctrl Pts',(33.3300682674399,0.483535022187859,32.6558517831686));
#54464=CARTESIAN_POINT('Ctrl Pts',(33.1201316474673,0.344068228927324,32.6696902785265));
#54465=CARTESIAN_POINT('Ctrl Pts',(33.0224736653896,0.159896796562307,32.6811360362706));
#54466=CARTESIAN_POINT('Ctrl Pts',(33.0082101094478,0.039213620633031,32.6879689622287));
#54467=CARTESIAN_POINT('Ctrl Pts',(33.0082140178674,1.39678807050542E-6,
32.6901890564009));
#54468=CARTESIAN_POINT('Origin',(33.5,0.,31.5181609435991));
#54469=CARTESIAN_POINT('',(33.0082137073647,-2.13203384507228E-6,32.3056609435991));
#54470=CARTESIAN_POINT('',(33.0081623574597,1.1889229359581E-5,32.3401890564009));
#54471=CARTESIAN_POINT('',(33.008175,-2.33277202951234E-14,31.5181609435991));
#54472=CARTESIAN_POINT('Ctrl Pts',(33.0082137073647,-2.13203384506061E-6,
32.3056609435991));
#54473=CARTESIAN_POINT('Ctrl Pts',(33.0082078601063,-0.0384054412330459,
32.3078352431222));
#54474=CARTESIAN_POINT('Ctrl Pts',(33.0220778628738,-0.158278193915492,
32.3146223744312));
#54475=CARTESIAN_POINT('Ctrl Pts',(33.1184391202127,-0.342190301200207,
32.3260223375262));
#54476=CARTESIAN_POINT('Ctrl Pts',(33.3276852504194,-0.482690930406304,
32.3398608328841));
#54477=CARTESIAN_POINT('Ctrl Pts',(33.5786021006306,-0.506462848584172,
32.353699328242));
#54478=CARTESIAN_POINT('Ctrl Pts',(33.8105106759546,-0.407757314266396,
32.3675378235999));
#54479=CARTESIAN_POINT('Ctrl Pts',(33.9673287354196,-0.210444197521941,
32.3813763189578));
#54480=CARTESIAN_POINT('Ctrl Pts',(34.0111331095724,0.0377604491284709,
32.3952148143157));
#54481=CARTESIAN_POINT('Ctrl Pts',(33.9313306262398,0.27683352052657,32.4090533096735));
#54482=CARTESIAN_POINT('Ctrl Pts',(33.7472198477718,0.448960192096371,32.4228918050315));
#54483=CARTESIAN_POINT('Ctrl Pts',(33.5033241171675,0.512515226568531,32.4367303003893));
#54484=CARTESIAN_POINT('Ctrl Pts',(33.2586245183158,0.452129167452444,32.4505687957472));
#54485=CARTESIAN_POINT('Ctrl Pts',(33.0722965338366,0.282405120795205,32.4644072911051));
#54486=CARTESIAN_POINT('Ctrl Pts',(33.0122094610991,0.109879922261234,32.4744380070557));
#54487=CARTESIAN_POINT('Ctrl Pts',(33.0081444845291,0.014226025632863,32.4798558912204));
#54488=CARTESIAN_POINT('Ctrl Pts',(33.0081586006607,1.14590643093392E-5,
32.4806609435991));
#54489=CARTESIAN_POINT('Ctrl Pts',(33.0081623574597,1.18892293595862E-5,
32.3401890564009));
#54490=CARTESIAN_POINT('Ctrl Pts',(33.0082290773473,-0.0660010680535029,
32.3439276660323));
#54491=CARTESIAN_POINT('Ctrl Pts',(33.0381214112422,-0.213521799438744,
32.3522791074496));
#54492=CARTESIAN_POINT('Ctrl Pts',(33.1812274307884,-0.40133148460008,32.3652433806529));
#54493=CARTESIAN_POINT('Ctrl Pts',(33.4110720261877,-0.504752144013999,
32.3790818760108));
#54494=CARTESIAN_POINT('Ctrl Pts',(33.6624219930444,-0.486109049070869,
32.3929203713686));
#54495=CARTESIAN_POINT('Ctrl Pts',(33.87449359626,-0.349910642555099,32.4067588667265));
#54496=CARTESIAN_POINT('Ctrl Pts',(33.9960017518821,-0.129093661900934,
32.4205973620844));
#54497=CARTESIAN_POINT('Ctrl Pts',(33.9975622525602,0.122941922224663,32.4344358574423));
#54498=CARTESIAN_POINT('Ctrl Pts',(33.8787977238271,0.345246572519499,32.4482743528002));
#54499=CARTESIAN_POINT('Ctrl Pts',(33.6684288842247,0.484060556513244,32.4621128481581));
#54500=CARTESIAN_POINT('Ctrl Pts',(33.4173290399213,0.505814614036365,32.475951343516));
#54501=CARTESIAN_POINT('Ctrl Pts',(33.1862214391045,0.405247981038107,32.4897898388739));
#54502=CARTESIAN_POINT('Ctrl Pts',(33.0395112404108,0.217575119584883,32.5028690765022));
#54503=CARTESIAN_POINT('Ctrl Pts',(33.0082225799653,0.0680293017237828,
32.5113354823445));
#54504=CARTESIAN_POINT('Ctrl Pts',(33.0081561516106,-1.11148368504149E-5,
32.5151890564009));
#54505=CARTESIAN_POINT('Origin',(33.5,0.,31.5181609435991));
#54506=CARTESIAN_POINT('',(33.0081453329024,-8.85342879087196E-6,32.1306609435991));
#54507=CARTESIAN_POINT('',(33.0082129808879,-3.22805011532257E-6,32.1651890564009));
#54508=CARTESIAN_POINT('',(33.008175,-2.33277202951234E-14,31.5181609435991));
#54509=CARTESIAN_POINT('Ctrl Pts',(33.0081453329024,-8.85342879090173E-6,
32.1306609435991));
#54510=CARTESIAN_POINT('Ctrl Pts',(33.0081373450458,-0.00955719774419399,
32.1312017632379));
#54511=CARTESIAN_POINT('Ctrl Pts',(33.0107330070713,-0.100542228012466,
32.1363554146628));
#54512=CARTESIAN_POINT('Ctrl Pts',(33.064433309084,-0.27011953832155,32.1461218978736));
#54513=CARTESIAN_POINT('Ctrl Pts',(33.2458559743834,-0.44507720842952,32.1599603932315));
#54514=CARTESIAN_POINT('Ctrl Pts',(33.4887380594845,-0.512402259865394,
32.1737988885894));
#54515=CARTESIAN_POINT('Ctrl Pts',(33.7343436094716,-0.455813536349459,
32.1876373839473));
#54516=CARTESIAN_POINT('Ctrl Pts',(33.9232780563821,-0.288995837694741,
32.2014758793052));
#54517=CARTESIAN_POINT('Ctrl Pts',(34.0098515538411,-0.0522905370538949,
32.2153143746631));
#54518=CARTESIAN_POINT('Ctrl Pts',(33.9731281112777,0.197060136857534,32.229152870021));
#54519=CARTESIAN_POINT('Ctrl Pts',(33.8219885255849,0.398755936145399,32.2429913653789));
#54520=CARTESIAN_POINT('Ctrl Pts',(33.5929827460405,0.504020948134402,32.2568298607368));
#54521=CARTESIAN_POINT('Ctrl Pts',(33.3414910331391,0.487399030204428,32.2706683560946));
#54522=CARTESIAN_POINT('Ctrl Pts',(33.1283314002966,0.352909845731284,32.2845068514525));
#54523=CARTESIAN_POINT('Ctrl Pts',(33.024421657049,0.167616884524029,32.2961710472873));
#54524=CARTESIAN_POINT('Ctrl Pts',(33.0082202652138,0.0430681568060907,
32.3032224113362));
#54525=CARTESIAN_POINT('Ctrl Pts',(33.0082137073647,-2.13203384506061E-6,
32.3056609435991));
#54526=CARTESIAN_POINT('Ctrl Pts',(33.0082129808879,-3.22805011533298E-6,
32.1651890564009));
#54527=CARTESIAN_POINT('Ctrl Pts',(33.0082043938807,-0.037184678202124,
32.1672941861481));
#54528=CARTESIAN_POINT('Ctrl Pts',(33.0214882449411,-0.155833345181072,
32.1740121476812));
#54529=CARTESIAN_POINT('Ctrl Pts',(33.1159002768464,-0.339338052812254,
32.1853429410003));
#54530=CARTESIAN_POINT('Ctrl Pts',(33.3240938254305,-0.481393736105298,
32.1991814363582));
#54531=CARTESIAN_POINT('Ctrl Pts',(33.5748266050752,-0.507034407694395,
32.2130199317161));
#54532=CARTESIAN_POINT('Ctrl Pts',(33.8074641345073,-0.410059407165293,
32.2268584270739));
#54533=CARTESIAN_POINT('Ctrl Pts',(33.9657478904425,-0.213920111166386,
32.2406969224318));
#54534=CARTESIAN_POINT('Ctrl Pts',(34.0114002553762,0.033951291790587,32.2545354177897));
#54535=CARTESIAN_POINT('Ctrl Pts',(33.9333811591964,0.273612284568271,32.2683739131476));
#54536=CARTESIAN_POINT('Ctrl Pts',(33.7505578893514,0.447105866095324,32.2822124085055));
#54537=CARTESIAN_POINT('Ctrl Pts',(33.5071424317946,0.512476240504031,32.2960509038634));
#54538=CARTESIAN_POINT('Ctrl Pts',(33.2619997264185,0.4539149492892,32.3098893992213));
#54539=CARTESIAN_POINT('Ctrl Pts',(33.0744124118928,0.285583816527163,32.3237278945792));
#54540=CARTESIAN_POINT('Ctrl Pts',(33.0126184365385,0.112324494712205,32.3338277803057));
#54541=CARTESIAN_POINT('Ctrl Pts',(33.0081467559368,0.0154481062829558,
32.3393148342463));
#54542=CARTESIAN_POINT('Ctrl Pts',(33.0081623574597,1.18892293595862E-5,
32.3401890564009));
#54543=CARTESIAN_POINT('Origin',(33.5,0.,31.5181609435991));
#54544=CARTESIAN_POINT('',(33.0081744217127,1.25591105979769E-5,31.9556609435991));
#54545=CARTESIAN_POINT('',(33.008142319392,-7.94017003039049E-6,31.9901890564009));
#54546=CARTESIAN_POINT('',(33.008175,-2.33277202951234E-14,31.5181609435991));
#54547=CARTESIAN_POINT('Ctrl Pts',(33.0081744217127,1.25591105979584E-5,
31.9556609435991));
#54548=CARTESIAN_POINT('Ctrl Pts',(33.008237202972,-0.0621478123915464,
31.9591811151397));
#54549=CARTESIAN_POINT('Ctrl Pts',(33.0355619943102,-0.205816778506115,
31.9673141184663));
#54550=CARTESIAN_POINT('Ctrl Pts',(33.1718738729398,-0.393720886912672,
31.9800599535789));
#54551=CARTESIAN_POINT('Ctrl Pts',(33.3992217475045,-0.502520304242071,
31.9938984489368));
#54552=CARTESIAN_POINT('Ctrl Pts',(33.6509407502508,-0.489795666360267,
32.0077369442947));
#54553=CARTESIAN_POINT('Ctrl Pts',(33.866157880612,-0.358624195726342,32.0215754396526));
#54554=CARTESIAN_POINT('Ctrl Pts',(33.9928273850048,-0.140726955258076,
32.0354139350105));
#54555=CARTESIAN_POINT('Ctrl Pts',(34.0003168872349,0.11120215536802,32.0492524303684));
#54556=CARTESIAN_POINT('Ctrl Pts',(33.8868152098793,0.336239350386304,32.0630909257263));
#54557=CARTESIAN_POINT('Ctrl Pts',(33.6797703599508,0.479964087041306,32.0769294210842));
#54558=CARTESIAN_POINT('Ctrl Pts',(33.4292518066392,0.507619542942049,32.090767916442));
#54559=CARTESIAN_POINT('Ctrl Pts',(33.1958422248624,0.412517823905107,32.1046064117999));
#54560=CARTESIAN_POINT('Ctrl Pts',(33.0422341208915,0.225272600578221,32.1179040875189));
#54561=CARTESIAN_POINT('Ctrl Pts',(33.0082054761492,0.0718838280517542,
32.126588931452));
#54562=CARTESIAN_POINT('Ctrl Pts',(33.0081453329024,-8.85342879090173E-6,
32.1306609435991));
#54563=CARTESIAN_POINT('Ctrl Pts',(33.008142319392,-7.94017003037054E-6,
31.9901890564009));
#54564=CARTESIAN_POINT('Ctrl Pts',(33.0081359043766,-0.00833492232700847,
31.9906607062639));
#54565=CARTESIAN_POINT('Ctrl Pts',(33.0103688763545,-0.0980980466196527,
31.9957451879128));
#54566=CARTESIAN_POINT('Ctrl Pts',(33.0624329149555,-0.26686692867671,32.0054425013477));
#54567=CARTESIAN_POINT('Ctrl Pts',(33.242547054467,-0.443171402728369,32.0192809967056));
#54568=CARTESIAN_POINT('Ctrl Pts',(33.4849208067233,-0.512304137563027,
32.0331194920635));
#54569=CARTESIAN_POINT('Ctrl Pts',(33.7309411467251,-0.457546826192634,
32.0469579874214));
#54570=CARTESIAN_POINT('Ctrl Pts',(33.9211131981036,-0.292141379806954,
32.0607964827792));
#54571=CARTESIAN_POINT('Ctrl Pts',(34.0094478257655,-0.0560876478150095,
32.0746349781371));
#54572=CARTESIAN_POINT('Ctrl Pts',(33.9745831465933,0.193529709299927,32.088473473495));
#54573=CARTESIAN_POINT('Ctrl Pts',(33.8249504544208,0.396345951897195,32.1023119688529));
#54574=CARTESIAN_POINT('Ctrl Pts',(33.5967352878245,0.503314211504509,32.1161504642108));
#54575=CARTESIAN_POINT('Ctrl Pts',(33.3451267140869,0.488566450673417,32.1299889595687));
#54576=CARTESIAN_POINT('Ctrl Pts',(33.1309710069735,0.355669107062927,32.1438274549266));
#54577=CARTESIAN_POINT('Ctrl Pts',(33.0250592894773,0.170061265436977,32.1555608205373));
#54578=CARTESIAN_POINT('Ctrl Pts',(33.0082232100224,0.0442885779433792,
32.1626813543621));
#54579=CARTESIAN_POINT('Ctrl Pts',(33.0082129808879,-3.22805011533298E-6,
32.1651890564009));
#54580=CARTESIAN_POINT('Origin',(33.5,-4.22503145705836E-17,35.68));
#54581=CARTESIAN_POINT('',(33.8267137838479,-1.25827584552983,35.7));
#54582=CARTESIAN_POINT('',(33.9134877274014,-1.31659709097673,35.6599999998357));
#54583=CARTESIAN_POINT('Ctrl Pts',(33.9134877272219,-1.31659709118071,35.6599999998064));
#54584=CARTESIAN_POINT('Ctrl Pts',(33.8947808196116,-1.30162996643187,35.6699423003901));
#54585=CARTESIAN_POINT('Ctrl Pts',(33.8753602716944,-1.28781826555715,35.6793436587508));
#54586=CARTESIAN_POINT('Ctrl Pts',(33.8461616023478,-1.26945105345498,35.6921094317771));
#54587=CARTESIAN_POINT('Ctrl Pts',(33.8365913002958,-1.2637714493812,35.6960991898629));
#54588=CARTESIAN_POINT('Ctrl Pts',(33.8267137838479,-1.25827584552984,35.7));
#54589=CARTESIAN_POINT('',(33.0865122725986,-1.31659709097673,35.6599999998357));
#54590=CARTESIAN_POINT('Origin',(33.5,-8.45006291411672E-17,35.66));
#54591=CARTESIAN_POINT('',(33.1732862161521,-1.25827584552983,35.7));
#54592=CARTESIAN_POINT('Ctrl Pts',(33.1732862161521,-1.25827584552984,35.7));
#54593=CARTESIAN_POINT('Ctrl Pts',(33.1634086997042,-1.2637714493812,35.6960991898629));
#54594=CARTESIAN_POINT('Ctrl Pts',(33.1538383976522,-1.26945105345497,35.6921094317771));
#54595=CARTESIAN_POINT('Ctrl Pts',(33.1246397283056,-1.28781826555714,35.6793436587508));
#54596=CARTESIAN_POINT('Ctrl Pts',(33.1052191803884,-1.30162996643187,35.6699423003901));
#54597=CARTESIAN_POINT('Ctrl Pts',(33.0865122727781,-1.31659709118072,35.6599999998064));
#54598=CARTESIAN_POINT('Origin',(33.5,0.,35.7));
#54599=CARTESIAN_POINT('Origin',(33.5,0.,35.6));
#54600=CARTESIAN_POINT('',(34.1036927352867,-1.3731551556041,35.5));
#54601=CARTESIAN_POINT('Ctrl Pts',(33.9134877273301,-1.31659709096526,35.6599999997146));
#54602=CARTESIAN_POINT('Ctrl Pts',(33.9319903902625,-1.31957316966569,35.6488222986488));
#54603=CARTESIAN_POINT('Ctrl Pts',(33.9497355251395,-1.32290966342206,35.6370817153252));
#54604=CARTESIAN_POINT('Ctrl Pts',(34.0157704341502,-1.33736376647548,35.5896872944202));
#54605=CARTESIAN_POINT('Ctrl Pts',(34.063005068998,-1.35253774255393,35.5469988938483));
#54606=CARTESIAN_POINT('Ctrl Pts',(34.1036927352866,-1.37315515560417,35.5));
#54607=CARTESIAN_POINT('',(32.,-1.83697019872103E-16,35.5));
#54608=CARTESIAN_POINT('Origin',(33.5,0.,35.5));
#54609=CARTESIAN_POINT('',(32.8963072647133,-1.3731551556041,35.5));
#54610=CARTESIAN_POINT('Origin',(33.5,0.,35.5));
#54611=CARTESIAN_POINT('Ctrl Pts',(32.8963072647134,-1.37315515560417,35.5));
#54612=CARTESIAN_POINT('Ctrl Pts',(32.9369949310021,-1.35253774255393,35.5469988938483));
#54613=CARTESIAN_POINT('Ctrl Pts',(32.9842295658498,-1.33736376647548,35.5896872944202));
#54614=CARTESIAN_POINT('Ctrl Pts',(33.0502644748605,-1.32290966342206,35.6370817153252));
#54615=CARTESIAN_POINT('Ctrl Pts',(33.0680096097375,-1.31957316966569,35.6488222986487));
#54616=CARTESIAN_POINT('Ctrl Pts',(33.0865122726699,-1.31659709096526,35.6599999997146));
#54617=CARTESIAN_POINT('Ctrl Pts',(33.2852137805935,0.44244627987821,31.7840265756214));
#54618=CARTESIAN_POINT('Ctrl Pts',(33.2119363917707,0.406873660039325,31.7886394074074));
#54619=CARTESIAN_POINT('Ctrl Pts',(33.0834805920019,0.298625908180025,31.7978650709793));
#54620=CARTESIAN_POINT('Ctrl Pts',(32.9914793936034,0.0639600166558817,
31.8117035663372));
#54621=CARTESIAN_POINT('Ctrl Pts',(33.0224796405589,-0.186155545440344,
31.8255420616951));
#54622=CARTESIAN_POINT('Ctrl Pts',(33.1689489303847,-0.391267382334031,
31.839380557053));
#54623=CARTESIAN_POINT('Ctrl Pts',(33.3954812484184,-0.501755342518352,
31.8532190524109));
#54624=CARTESIAN_POINT('Ctrl Pts',(33.6472872572454,-0.490907009997742,
31.8670575477688));
#54625=CARTESIAN_POINT('Ctrl Pts',(33.8634759777288,-0.361342183302042,
31.8808960431267));
#54626=CARTESIAN_POINT('Ctrl Pts',(33.991765211222,-0.144394846435863,31.8947345384845));
#54627=CARTESIAN_POINT('Ctrl Pts',(34.0011315224325,0.107471559754204,31.9085730338424));
#54628=CARTESIAN_POINT('Ctrl Pts',(33.8893095626415,0.33334810735359,31.9224115292003));
#54629=CARTESIAN_POINT('Ctrl Pts',(33.6833412670481,0.478611425195411,31.9362500245582));
#54630=CARTESIAN_POINT('Ctrl Pts',(33.4330357002492,0.508132553198278,31.9500885199161));
#54631=CARTESIAN_POINT('Ctrl Pts',(33.1989240583753,0.414772454316571,31.963927015274));
#54632=CARTESIAN_POINT('Ctrl Pts',(33.0376213352481,0.221108303602627,31.9777655106319));
#54633=CARTESIAN_POINT('Ctrl Pts',(32.9881352281445,-0.0260262663029543,
31.9916040059898));
#54634=CARTESIAN_POINT('Ctrl Pts',(33.0624329149555,-0.26686692867671,32.0054425013477));
#54635=CARTESIAN_POINT('Ctrl Pts',(33.242547054467,-0.443171402728369,32.0192809967056));
#54636=CARTESIAN_POINT('Ctrl Pts',(33.4849208067233,-0.512304137563027,
32.0331194920635));
#54637=CARTESIAN_POINT('Ctrl Pts',(33.7309411467251,-0.457546826192634,
32.0469579874214));
#54638=CARTESIAN_POINT('Ctrl Pts',(33.9211131981036,-0.292141379806954,
32.0607964827792));
#54639=CARTESIAN_POINT('Ctrl Pts',(34.0094478257655,-0.0560876478150095,
32.0746349781371));
#54640=CARTESIAN_POINT('Ctrl Pts',(33.9745831465933,0.193529709299927,32.088473473495));
#54641=CARTESIAN_POINT('Ctrl Pts',(33.8249504544208,0.396345951897195,32.1023119688529));
#54642=CARTESIAN_POINT('Ctrl Pts',(33.5967352878245,0.503314211504509,32.1161504642108));
#54643=CARTESIAN_POINT('Ctrl Pts',(33.3451267140869,0.488566450673417,32.1299889595687));
#54644=CARTESIAN_POINT('Ctrl Pts',(33.1309710069735,0.355669107062927,32.1438274549266));
#54645=CARTESIAN_POINT('Ctrl Pts',(33.0060572473975,0.136760625051723,32.1576659502845));
#54646=CARTESIAN_POINT('Ctrl Pts',(33.0005932168323,-0.115220555193728,
32.1715044456424));
#54647=CARTESIAN_POINT('Ctrl Pts',(33.1159002768464,-0.339338052812254,
32.1853429410003));
#54648=CARTESIAN_POINT('Ctrl Pts',(33.3240938254305,-0.481393736105298,
32.1991814363582));
#54649=CARTESIAN_POINT('Ctrl Pts',(33.5748266050752,-0.507034407694395,
32.2130199317161));
#54650=CARTESIAN_POINT('Ctrl Pts',(33.8074641345073,-0.410059407165293,
32.2268584270739));
#54651=CARTESIAN_POINT('Ctrl Pts',(33.9657478904425,-0.213920111166386,
32.2406969224318));
#54652=CARTESIAN_POINT('Ctrl Pts',(34.0114002553762,0.033951291790587,32.2545354177897));
#54653=CARTESIAN_POINT('Ctrl Pts',(33.9333811591964,0.273612284568271,32.2683739131476));
#54654=CARTESIAN_POINT('Ctrl Pts',(33.7505578893514,0.447105866095324,32.2822124085055));
#54655=CARTESIAN_POINT('Ctrl Pts',(33.5071424317946,0.512476240504031,32.2960509038634));
#54656=CARTESIAN_POINT('Ctrl Pts',(33.2619997264185,0.4539149492892,32.3098893992213));
#54657=CARTESIAN_POINT('Ctrl Pts',(33.0744124118928,0.285583816527163,32.3237278945792));
#54658=CARTESIAN_POINT('Ctrl Pts',(32.9897445587864,0.0481902077710606,
32.3375663899371));
#54659=CARTESIAN_POINT('Ctrl Pts',(33.0284713174202,-0.200857195334489,
32.351404885295));
#54660=CARTESIAN_POINT('Ctrl Pts',(33.1812274307884,-0.40133148460008,32.3652433806529));
#54661=CARTESIAN_POINT('Ctrl Pts',(33.4110720261877,-0.504752144013999,
32.3790818760108));
#54662=CARTESIAN_POINT('Ctrl Pts',(33.6624219930444,-0.486109049070869,
32.3929203713686));
#54663=CARTESIAN_POINT('Ctrl Pts',(33.87449359626,-0.349910642555099,32.4067588667265));
#54664=CARTESIAN_POINT('Ctrl Pts',(33.9960017518821,-0.129093661900934,
32.4205973620844));
#54665=CARTESIAN_POINT('Ctrl Pts',(33.9975622525602,0.122941922224663,32.4344358574423));
#54666=CARTESIAN_POINT('Ctrl Pts',(33.8787977238271,0.345246572519499,32.4482743528002));
#54667=CARTESIAN_POINT('Ctrl Pts',(33.6684288842247,0.484060556513244,32.4621128481581));
#54668=CARTESIAN_POINT('Ctrl Pts',(33.4173290399213,0.505814614036365,32.475951343516));
#54669=CARTESIAN_POINT('Ctrl Pts',(33.1862214391045,0.405247981038107,32.4897898388739));
#54670=CARTESIAN_POINT('Ctrl Pts',(33.0309946238057,0.20668059539767,32.5036283342318));
#54671=CARTESIAN_POINT('Ctrl Pts',(32.9891869543408,-0.0418681716517971,
32.5174668295897));
#54672=CARTESIAN_POINT('Ctrl Pts',(33.0709087415947,-0.280291996627235,
32.5313053249476));
#54673=CARTESIAN_POINT('Ctrl Pts',(33.2563972796865,-0.450933061627702,
32.5451438203055));
#54674=CARTESIAN_POINT('Ctrl Pts',(33.5007960432536,-0.512525392276544,
32.5589823156633));
#54675=CARTESIAN_POINT('Ctrl Pts',(33.7450023004009,-0.450174170973167,
32.5728208110213));
#54676=CARTESIAN_POINT('Ctrl Pts',(33.9299598728863,-0.278957737158612,
32.5866593063791));
#54677=CARTESIAN_POINT('Ctrl Pts',(34.0109406382799,-0.0402812061293292,
32.600497801737));
#54678=CARTESIAN_POINT('Ctrl Pts',(33.9683610913465,0.208136492537349,32.6143362970949));
#54679=CARTESIAN_POINT('Ctrl Pts',(33.8125182054012,0.406220731506804,32.6281747924528));
#54680=CARTESIAN_POINT('Ctrl Pts',(33.5810993245668,0.506068978468246,32.6420132878107));
#54681=CARTESIAN_POINT('Ctrl Pts',(33.3300682674399,0.483535022187859,32.6558517831686));
#54682=CARTESIAN_POINT('Ctrl Pts',(33.1201316474673,0.344068228927324,32.6696902785265));
#54683=CARTESIAN_POINT('Ctrl Pts',(33.0020582475354,0.121395727130593,32.6835287738844));
#54684=CARTESIAN_POINT('Ctrl Pts',(33.0044016511332,-0.130633793536081,
32.6973672692423));
#54685=CARTESIAN_POINT('Ctrl Pts',(33.1265951550888,-0.351072262091296,
32.7112057646002));
#54686=CARTESIAN_POINT('Ctrl Pts',(33.3390888148842,-0.486611243106551,
32.7250442599581));
#54687=CARTESIAN_POINT('Ctrl Pts',(33.590495481006,-0.504473467419831,32.7388827553159));
#54688=CARTESIAN_POINT('Ctrl Pts',(33.8200177068239,-0.400339329484723,
32.7527212506738));
#54689=CARTESIAN_POINT('Ctrl Pts',(33.9721503401083,-0.199391493671923,
32.7665597460317));
#54690=CARTESIAN_POINT('Ctrl Pts',(34.0101032837806,0.0497750066737403,
32.7803982413896));
#54691=CARTESIAN_POINT('Ctrl Pts',(33.924698411807,0.286904462185027,32.7942367367475));
#54692=CARTESIAN_POINT('Ctrl Pts',(33.7365891071145,0.454652071157545,32.8080752321054));
#54693=CARTESIAN_POINT('Ctrl Pts',(33.4912656726816,0.512451581068282,32.8219137274633));
#54694=CARTESIAN_POINT('Ctrl Pts',(33.2480544527224,0.446325388724518,32.8357522228212));
#54695=CARTESIAN_POINT('Ctrl Pts',(33.065770996536,0.272264731398925,32.8495907181791));
#54696=CARTESIAN_POINT('Ctrl Pts',(32.9884967474269,0.0323625403865631,
32.863429213537));
#54697=CARTESIAN_POINT('Ctrl Pts',(33.0349188671503,-0.215365854490337,
32.8772677088949));
#54698=CARTESIAN_POINT('Ctrl Pts',(33.1938111364897,-0.411012519609046,
32.8911062042528));
#54699=CARTESIAN_POINT('Ctrl Pts',(33.4267487816945,-0.507264398937922,
32.9049446996107));
#54700=CARTESIAN_POINT('Ctrl Pts',(33.6774007027546,-0.480844987574239,
32.9187831949685));
#54701=CARTESIAN_POINT('Ctrl Pts',(33.8851519723551,-0.338143267867451,
32.9326216903264));
#54702=CARTESIAN_POINT('Ctrl Pts',(33.9997622889131,-0.113668667597491,
32.9464601856843));
#54703=CARTESIAN_POINT('Ctrl Pts',(33.9935155432591,0.138294323725898,32.9602986810422));
#54704=CARTESIAN_POINT('Ctrl Pts',(33.8679223802432,0.35681372385221,32.9741371764001));
#54705=CARTESIAN_POINT('Ctrl Pts',(33.6533548808583,0.489045183934999,32.987975671758));
#54706=CARTESIAN_POINT('Ctrl Pts',(33.4017017093698,0.503011289607162,33.0018141671159));
#54707=CARTESIAN_POINT('Ctrl Pts',(33.1738199245776,0.395334630168599,33.0156526624738));
#54708=CARTESIAN_POINT('Ctrl Pts',(33.0248179723423,0.192054554760403,33.0294911578317));
#54709=CARTESIAN_POINT('Ctrl Pts',(32.9907288599765,-0.0576698998811294,
33.0433296531896));
#54710=CARTESIAN_POINT('Ctrl Pts',(33.0797963266846,-0.293448094806149,
33.0571681485475));
#54711=CARTESIAN_POINT('Ctrl Pts',(33.2704812675685,-0.458262002435405,
33.0710066439053));
#54712=CARTESIAN_POINT('Ctrl Pts',(33.5166705158794,-0.512254824587727,
33.0848451392633));
#54713=CARTESIAN_POINT('Ctrl Pts',(33.7588283484165,-0.442369525927234,
33.0986836346211));
#54714=CARTESIAN_POINT('Ctrl Pts',(33.938393955608,-0.265506405006475,33.112522129979));
#54715=CARTESIAN_POINT('Ctrl Pts',(34.011943149113,-0.0244361103564004,
33.1263606253369));
#54716=CARTESIAN_POINT('Ctrl Pts',(33.9616895940033,0.222543546754668,33.1401991206948));
#54717=CARTESIAN_POINT('Ctrl Pts',(33.7997860620486,0.41570569928083,33.1540376160527));
#54718=CARTESIAN_POINT('Ctrl Pts',(33.5653855379137,0.508338118622465,33.1678761114106));
#54719=CARTESIAN_POINT('Ctrl Pts',(33.3151728882965,0.478039590612468,33.1817146067685));
#54720=CARTESIAN_POINT('Ctrl Pts',(33.1096568118975,0.332137180866717,33.1955531021264));
#54721=CARTESIAN_POINT('Ctrl Pts',(32.9985370755469,0.105914337147998,33.2093915974843));
#54722=CARTESIAN_POINT('Ctrl Pts',(33.0086856645668,-0.145921674916193,
33.2232300928422));
#54723=CARTESIAN_POINT('Ctrl Pts',(33.1376483548415,-0.362469580324392,
33.2370685882));
#54724=CARTESIAN_POINT('Ctrl Pts',(33.35423821568,-0.491361795081716,33.2509070835579));
#54725=CARTESIAN_POINT('Ctrl Pts',(33.6060775169075,-0.501428431350477,
33.2647455789158));
#54726=CARTESIAN_POINT('Ctrl Pts',(33.8322641882851,-0.390235083915959,
33.2785840742737));
#54727=CARTESIAN_POINT('Ctrl Pts',(33.978099711361,-0.184671538686574,33.2924225696316));
#54728=CARTESIAN_POINT('Ctrl Pts',(34.0083168142334,0.0655509565705277,
33.3062610649895));
#54729=CARTESIAN_POINT('Ctrl Pts',(33.915608120618,0.299921325619444,33.3200995603474));
#54730=CARTESIAN_POINT('Ctrl Pts',(33.7223932934449,0.461761986408213,33.3339380557053));
#54731=CARTESIAN_POINT('Ctrl Pts',(33.4753972915975,0.511935174870455,33.3477765510632));
#54732=CARTESIAN_POINT('Ctrl Pts',(33.2343509511662,0.438307516584007,33.3616150464211));
#54733=CARTESIAN_POINT('Ctrl Pts',(33.057546251495,0.258684401086308,33.375453541779));
#54734=CARTESIAN_POINT('Ctrl Pts',(32.9877397915081,0.016503740221554,33.3892920371369));
#54735=CARTESIAN_POINT('Ctrl Pts',(33.0418126118584,-0.229667753869374,
33.4031305324948));
#54736=CARTESIAN_POINT('Ctrl Pts',(33.2066887031424,-0.420299550020602,
33.4169690278527));
#54737=CARTESIAN_POINT('Ctrl Pts',(33.4424952770395,-0.509289505109944,
33.4308075232105));
#54738=CARTESIAN_POINT('Ctrl Pts',(33.6922091923902,-0.47512167024108,33.4446460185684));
#54739=CARTESIAN_POINT('Ctrl Pts',(33.8954376101786,-0.326050114606906,
33.4584845139263));
#54740=CARTESIAN_POINT('Ctrl Pts',(34.003042111098,-0.0981464483443762,
33.4723230092842));
#54741=CARTESIAN_POINT('Ctrl Pts',(33.9889768845264,0.153516958914333,33.4861615046421));
#54742=CARTESIAN_POINT('Ctrl Pts',(33.9007791656288,0.296484195224244,33.495387168214));
#54743=CARTESIAN_POINT('Ctrl Pts',(33.8422870473583,0.35317333964466,33.5));
#54744=CARTESIAN_POINT('Ctrl Pts',(33.2706785265175,0.472388001049928,31.8032427170809));
#54745=CARTESIAN_POINT('Ctrl Pts',(33.1924422280053,0.434408070961184,31.8078555488669));
#54746=CARTESIAN_POINT('Ctrl Pts',(33.0552934231996,0.318834855760824,31.8170812124388));
#54747=CARTESIAN_POINT('Ctrl Pts',(32.957066216458,0.068288390679903,31.8309197077967));
#54748=CARTESIAN_POINT('Ctrl Pts',(32.9901643469143,-0.198753272417905,
31.8447582031546));
#54749=CARTESIAN_POINT('Ctrl Pts',(33.1465456708912,-0.417745667717418,
31.8585966985125));
#54750=CARTESIAN_POINT('Ctrl Pts',(33.3884081381688,-0.535710693134566,
31.8724351938704));
#54751=CARTESIAN_POINT('Ctrl Pts',(33.6572546458057,-0.524128220081462,
31.8862736892283));
#54752=CARTESIAN_POINT('Ctrl Pts',(33.8880735319918,-0.385795337034035,
31.9001121845862));
#54753=CARTESIAN_POINT('Ctrl Pts',(34.0250444984621,-0.154166496525918,
31.9139506799441));
#54754=CARTESIAN_POINT('Ctrl Pts',(34.0350446571958,0.114744495752073,31.927789175302));
#54755=CARTESIAN_POINT('Ctrl Pts',(33.9156553562536,0.355906814562628,31.9416276706599));
#54756=CARTESIAN_POINT('Ctrl Pts',(33.6957485430201,0.511000554666099,31.9554661660177));
#54757=CARTESIAN_POINT('Ctrl Pts',(33.4285040170082,0.542519469572225,31.9693046613756));
#54758=CARTESIAN_POINT('Ctrl Pts',(33.1785493093818,0.442841401308904,31.9831431567335));
#54759=CARTESIAN_POINT('Ctrl Pts',(33.0063307273588,0.236071392855055,31.9969816520914));
#54760=CARTESIAN_POINT('Ctrl Pts',(32.9534957408812,-0.0277875450032694,
32.0108201474493));
#54761=CARTESIAN_POINT('Ctrl Pts',(33.0328213841321,-0.284926646956158,
32.0246586428072));
#54762=CARTESIAN_POINT('Ctrl Pts',(33.2251244098194,-0.473162195227346,
32.0384971381651));
#54763=CARTESIAN_POINT('Ctrl Pts',(33.4839003506337,-0.546973358075519,
32.052335633523));
#54764=CARTESIAN_POINT('Ctrl Pts',(33.7465696551718,-0.488510448480601,
32.0661741288809));
#54765=CARTESIAN_POINT('Ctrl Pts',(33.9496112430251,-0.311911499106656,
32.0800126242388));
#54766=CARTESIAN_POINT('Ctrl Pts',(34.0439237507406,-0.0598832740603414,
32.0938511195967));
#54767=CARTESIAN_POINT('Ctrl Pts',(34.0066996698738,0.20662646896959,32.1076896149546));
#54768=CARTESIAN_POINT('Ctrl Pts',(33.8469408662366,0.423167919939306,32.1215281103125));
#54769=CARTESIAN_POINT('Ctrl Pts',(33.6032816667799,0.53737505565214,32.1353666056703));
#54770=CARTESIAN_POINT('Ctrl Pts',(33.3346459552815,0.521629267799931,32.1492051010282));
#54771=CARTESIAN_POINT('Ctrl Pts',(33.1059976628276,0.379738346013256,32.1630435963861));
#54772=CARTESIAN_POINT('Ctrl Pts',(32.9726305991335,0.146015643545033,32.176882091744));
#54773=CARTESIAN_POINT('Ctrl Pts',(32.96679680056,-0.123017889907018,32.1907205871019));
#54774=CARTESIAN_POINT('Ctrl Pts',(33.0899070493387,-0.362302118332377,
32.2045590824598));
#54775=CARTESIAN_POINT('Ctrl Pts',(33.3121897053805,-0.51397115324223,32.2183975778177));
#54776=CARTESIAN_POINT('Ctrl Pts',(33.5798903550654,-0.541347009133448,
32.2322360731756));
#54777=CARTESIAN_POINT('Ctrl Pts',(33.8282711924585,-0.437809407541753,
32.2460745685335));
#54778=CARTESIAN_POINT('Ctrl Pts',(33.9972665043537,-0.228396752993572,
32.2599130638914));
#54779=CARTESIAN_POINT('Ctrl Pts',(34.046008307359,0.036248881709283,32.2737515592493));
#54780=CARTESIAN_POINT('Ctrl Pts',(33.9627094153483,0.292128482141352,32.2875900546072));
#54781=CARTESIAN_POINT('Ctrl Pts',(33.7675139240194,0.477362916014583,32.301428549965));
#54782=CARTESIAN_POINT('Ctrl Pts',(33.5076257824544,0.547157107759884,32.3152670453229));
#54783=CARTESIAN_POINT('Ctrl Pts',(33.2458935048172,0.484632791127611,32.3291055406808));
#54784=CARTESIAN_POINT('Ctrl Pts',(33.0456115710297,0.3049101650456,32.3429440360387));
#54785=CARTESIAN_POINT('Ctrl Pts',(32.9552139799524,0.0514513895911138,
32.3567825313966));
#54786=CARTESIAN_POINT('Ctrl Pts',(32.9965614992561,-0.214449828862097,
32.3706210267545));
#54787=CARTESIAN_POINT('Ctrl Pts',(33.1596550957534,-0.428490839206101,
32.3844595221124));
#54788=CARTESIAN_POINT('Ctrl Pts',(33.4050539925476,-0.538910297544081,
32.3982980174703));
#54789=CARTESIAN_POINT('Ctrl Pts',(33.67341359643,-0.519005566158403,32.4121365128282));
#54790=CARTESIAN_POINT('Ctrl Pts',(33.8998367471684,-0.37359018823302,32.4259750081861));
#54791=CARTESIAN_POINT('Ctrl Pts',(34.029567739056,-0.137829833059924,32.439813503544));
#54792=CARTESIAN_POINT('Ctrl Pts',(34.0312338436872,0.131261785952703,32.4536519989019));
#54793=CARTESIAN_POINT('Ctrl Pts',(33.9044321484864,0.368610486015879,32.4674904942597));
#54794=CARTESIAN_POINT('Ctrl Pts',(33.6798269926913,0.516818445713568,32.4813289896176));
#54795=CARTESIAN_POINT('Ctrl Pts',(33.4117344379363,0.540044668230122,32.4951674849755));
#54796=CARTESIAN_POINT('Ctrl Pts',(33.1649870642046,0.432672377186234,32.5090059803334));
#54797=CARTESIAN_POINT('Ctrl Pts',(32.9992555656631,0.220667316589463,32.5228444756913));
#54798=CARTESIAN_POINT('Ctrl Pts',(32.9546186406729,-0.0447015215489012,
32.5366829710492));
#54799=CARTESIAN_POINT('Ctrl Pts',(33.0418707964234,-0.299260231170842,
32.5505214664071));
#54800=CARTESIAN_POINT('Ctrl Pts',(33.2399119230228,-0.481449109817964,
32.564359961765));
#54801=CARTESIAN_POINT('Ctrl Pts',(33.500849913986,-0.547209585786305,32.5781984571229));
#54802=CARTESIAN_POINT('Ctrl Pts',(33.7615823710188,-0.480638862663418,
32.5920369524808));
#54803=CARTESIAN_POINT('Ctrl Pts',(33.9590565999117,-0.297835678198135,
32.6058754478387));
#54804=CARTESIAN_POINT('Ctrl Pts',(34.0455175865387,-0.043007161114684,
32.6197139431966));
#54805=CARTESIAN_POINT('Ctrl Pts',(34.0000565487219,0.222221738834205,32.6335524385544));
#54806=CARTESIAN_POINT('Ctrl Pts',(33.8336672881097,0.433710956716281,32.6473909339123));
#54807=CARTESIAN_POINT('Ctrl Pts',(33.5865875690698,0.540316246297288,32.6612294292702));
#54808=CARTESIAN_POINT('Ctrl Pts',(33.3185684565342,0.516257346839555,32.6750679246281));
#54809=CARTESIAN_POINT('Ctrl Pts',(33.0944247700208,0.367352400233783,32.688906419986));
#54810=CARTESIAN_POINT('Ctrl Pts',(32.968360974465,0.129610955009068,32.7027449153439));
#54811=CARTESIAN_POINT('Ctrl Pts',(32.9708629635009,-0.139474190211441,
32.7165834107018));
#54812=CARTESIAN_POINT('Ctrl Pts',(33.1013256833835,-0.374830418190054,
32.7304219060597));
#54813=CARTESIAN_POINT('Ctrl Pts',(33.3281994525881,-0.519541745232436,
32.7442604014176));
#54814=CARTESIAN_POINT('Ctrl Pts',(33.596619592752,-0.538612762034699,32.7580988967755));
#54815=CARTESIAN_POINT('Ctrl Pts',(33.8416743042087,-0.427431541856367,
32.7719373921334));
#54816=CARTESIAN_POINT('Ctrl Pts',(34.0041022277782,-0.212884938591792,
32.7857758874913));
#54817=CARTESIAN_POINT('Ctrl Pts',(34.044623565646,0.0531434367836172,32.7996143828491));
#54818=CARTESIAN_POINT('Ctrl Pts',(33.9534390793337,0.306320182918468,32.813452878207));
#54819=CARTESIAN_POINT('Ctrl Pts',(33.752599830675,0.485419796334239,32.8272913735649));
#54820=CARTESIAN_POINT('Ctrl Pts',(33.4906745934815,0.547130779543125,32.8411298689228));
#54821=CARTESIAN_POINT('Ctrl Pts',(33.23100451091,0.476529621303278,32.8549683642807));
#54822=CARTESIAN_POINT('Ctrl Pts',(33.0363853641153,0.290689735841688,32.8688068596386));
#54823=CARTESIAN_POINT('Ctrl Pts',(32.9538817253023,0.0345526145373283,
32.8826453549965));
#54824=CARTESIAN_POINT('Ctrl Pts',(33.0034453748071,-0.229940334282172,
32.8964838503544));
#54825=CARTESIAN_POINT('Ctrl Pts',(33.1730903801086,-0.438827020080395,
32.9103223457123));
#54826=CARTESIAN_POINT('Ctrl Pts',(33.4217916430457,-0.541592564602507,
32.9241608410702));
#54827=CARTESIAN_POINT('Ctrl Pts',(33.6894059621931,-0.513385269184764,
32.9379993364281));
#54828=CARTESIAN_POINT('Ctrl Pts',(33.9112164088516,-0.361026478559986,
32.951837831786));
#54829=CARTESIAN_POINT('Ctrl Pts',(34.0335827633691,-0.12136098123182,32.9656763271439));
#54830=CARTESIAN_POINT('Ctrl Pts',(34.026913280933,0.147653132397023,32.9795148225017));
#54831=CARTESIAN_POINT('Ctrl Pts',(33.892820836447,0.380960422594407,32.9933533178596));
#54832=CARTESIAN_POINT('Ctrl Pts',(33.6637328844529,0.522140398436032,33.0071918132175));
#54833=CARTESIAN_POINT('Ctrl Pts',(33.3950495571344,0.537051634084214,33.0210303085754));
#54834=CARTESIAN_POINT('Ctrl Pts',(33.1517463004695,0.422088158911775,33.0348688039333));
#54835=CARTESIAN_POINT('Ctrl Pts',(32.9926609209103,0.20505148611663,33.0487072992912));
#54836=CARTESIAN_POINT('Ctrl Pts',(32.9562648918772,-0.0615726020639032,
33.0625457946491));
#54837=CARTESIAN_POINT('Ctrl Pts',(33.0513598321452,-0.313306643589688,
33.076384290007));
#54838=CARTESIAN_POINT('Ctrl Pts',(33.254949018338,-0.489274022932652,33.0902227853649));
#54839=CARTESIAN_POINT('Ctrl Pts',(33.5177986617379,-0.546920707937215,
33.1040612807228));
#54840=CARTESIAN_POINT('Ctrl Pts',(33.7763440708715,-0.472306052919448,
33.1178997760807));
#54841=CARTESIAN_POINT('Ctrl Pts',(33.9680614433441,-0.283474052401314,
33.1317382714386));
#54842=CARTESIAN_POINT('Ctrl Pts',(34.04658794041,-0.026089778239007,33.1455767667965));
#54843=CARTESIAN_POINT('Ctrl Pts',(33.9929335703236,0.237603763392328,33.1594152621543));
#54844=CARTESIAN_POINT('Ctrl Pts',(33.8200735208639,0.443837801873684,33.1732537575122));
#54845=CARTESIAN_POINT('Ctrl Pts',(33.569810381412,0.542738946250486,33.1870922528701));
#54846=CARTESIAN_POINT('Ctrl Pts',(33.3026650605776,0.510390022251539,33.200930748228));
#54847=CARTESIAN_POINT('Ctrl Pts',(33.0832410696233,0.354613940899618,33.2147692435859));
#54848=CARTESIAN_POINT('Ctrl Pts',(32.9646015137741,0.113081891030125,33.2286077389438));
#54849=CARTESIAN_POINT('Ctrl Pts',(32.9754368894991,-0.155796650256595,
33.2424462343017));
#54850=CARTESIAN_POINT('Ctrl Pts',(33.1131268876739,-0.386999028532861,
33.2562847296596));
#54851=CARTESIAN_POINT('Ctrl Pts',(33.3443740606355,-0.524613781892005,
33.2701232250175));
#54852=CARTESIAN_POINT('Ctrl Pts',(33.6132561136734,-0.535361658867275,
33.2839617203754));
#54853=CARTESIAN_POINT('Ctrl Pts',(33.8547495433066,-0.41664351044234,33.2978002157333));
#54854=CARTESIAN_POINT('Ctrl Pts',(34.0104542115589,-0.197168838293723,
33.3116387110912));
#54855=CARTESIAN_POINT('Ctrl Pts',(34.0427162001269,0.0699869944658259,
33.325477206449));
#54856=CARTESIAN_POINT('Ctrl Pts',(33.9437336197581,0.320217938142937,33.3393157018069));
#54857=CARTESIAN_POINT('Ctrl Pts',(33.7374433419719,0.493010861748602,33.3531541971648));
#54858=CARTESIAN_POINT('Ctrl Pts',(33.4737323495049,0.54657942652556,33.3669926925227));
#54859=CARTESIAN_POINT('Ctrl Pts',(33.2163736506182,0.467969154721499,33.3808311878806));
#54860=CARTESIAN_POINT('Ctrl Pts',(33.027604024898,0.276190382176106,33.3946696832385));
#54861=CARTESIAN_POINT('Ctrl Pts',(32.953073543813,0.0176205998505714,33.4085081785964));
#54862=CARTESIAN_POINT('Ctrl Pts',(33.0108056407434,-0.245210087845792,
33.4223466739543));
#54863=CARTESIAN_POINT('Ctrl Pts',(33.1868394119032,-0.448742532836006,
33.4361851693122));
#54864=CARTESIAN_POINT('Ctrl Pts',(33.4386037528947,-0.543754716032006,
33.4500236646701));
#54865=CARTESIAN_POINT('Ctrl Pts',(33.7052165885577,-0.507274637098244,
33.463862160028));
#54866=CARTESIAN_POINT('Ctrl Pts',(33.9221981079006,-0.348114943860877,
33.4777006553858));
#54867=CARTESIAN_POINT('Ctrl Pts',(34.0370845413616,-0.104788324938144,
33.4915391507438));
#54868=CARTESIAN_POINT('Ctrl Pts',(34.0220674769932,0.163905930836998,33.5053776461016));
#54869=CARTESIAN_POINT('Ctrl Pts',(33.9279011430856,0.316548206402434,33.5146033096736));
#54870=CARTESIAN_POINT('Ctrl Pts',(33.8654506805467,0.37707368222147,33.5192161414595));
#54871=CARTESIAN_POINT('Ctrl Pts',(33.2561432724416,0.502329722221647,31.8224588585405));
#54872=CARTESIAN_POINT('Ctrl Pts',(33.17294806424,0.461942481883043,31.8270716903264));
#54873=CARTESIAN_POINT('Ctrl Pts',(33.0271062543972,0.339043803341623,31.8362973538983));
#54874=CARTESIAN_POINT('Ctrl Pts',(32.9226530393125,0.0726167647039235,
31.8501358492563));
#54875=CARTESIAN_POINT('Ctrl Pts',(32.9578490532698,-0.211350999395466,
31.8639743446142));
#54876=CARTESIAN_POINT('Ctrl Pts',(33.1241424113978,-0.444223953100805,
31.877812839972));
#54877=CARTESIAN_POINT('Ctrl Pts',(33.3813350279193,-0.56966604375078,31.8916513353299));
#54878=CARTESIAN_POINT('Ctrl Pts',(33.667222034366,-0.557349430165183,31.9054898306878));
#54879=CARTESIAN_POINT('Ctrl Pts',(33.9126710862548,-0.410248490766028,
31.9193283260457));
#54880=CARTESIAN_POINT('Ctrl Pts',(34.0583237857021,-0.163938146615973,
31.9331668214036));
#54881=CARTESIAN_POINT('Ctrl Pts',(34.0689577919591,0.122017431749941,31.9470053167615));
#54882=CARTESIAN_POINT('Ctrl Pts',(33.9420011498656,0.378465521771666,31.9608438121194));
#54883=CARTESIAN_POINT('Ctrl Pts',(33.708155818992,0.543389684136786,31.9746823074773));
#54884=CARTESIAN_POINT('Ctrl Pts',(33.4239723337671,0.576906385946173,31.9885208028352));
#54885=CARTESIAN_POINT('Ctrl Pts',(33.1581745603883,0.470910348301238,32.0023592981931));
#54886=CARTESIAN_POINT('Ctrl Pts',(32.9750401194695,0.251034482107482,32.0161977935509));
#54887=CARTESIAN_POINT('Ctrl Pts',(32.9188562536179,-0.029548823703585,
32.0300362889088));
#54888=CARTESIAN_POINT('Ctrl Pts',(33.0032098533087,-0.302986365235606,
32.0438747842667));
#54889=CARTESIAN_POINT('Ctrl Pts',(33.2077017651717,-0.503152987726324,
32.0577132796246));
#54890=CARTESIAN_POINT('Ctrl Pts',(33.4828798945442,-0.581642578588012,
32.0715517749825));
#54891=CARTESIAN_POINT('Ctrl Pts',(33.7621981636186,-0.519474070768568,
32.0853902703404));
#54892=CARTESIAN_POINT('Ctrl Pts',(33.9781092879467,-0.331681618406357,
32.0992287656983));
#54893=CARTESIAN_POINT('Ctrl Pts',(34.0783996757157,-0.0636789003056738,
32.1130672610562));
#54894=CARTESIAN_POINT('Ctrl Pts',(34.0388161931543,0.219723228639253,32.1269057564141));
#54895=CARTESIAN_POINT('Ctrl Pts',(33.8689312780524,0.449989887981418,32.140744251772));
#54896=CARTESIAN_POINT('Ctrl Pts',(33.6098280457354,0.571435899799772,32.1545827471299));
#54897=CARTESIAN_POINT('Ctrl Pts',(33.3241651964761,0.554692084926445,32.1684212424878));
#54898=CARTESIAN_POINT('Ctrl Pts',(33.0810243186817,0.403807584963584,32.1822597378457));
#54899=CARTESIAN_POINT('Ctrl Pts',(32.9392039508694,0.155270662038344,32.1960982332035));
#54900=CARTESIAN_POINT('Ctrl Pts',(32.9330003842878,-0.130815224620308,
32.2099367285614));
#54901=CARTESIAN_POINT('Ctrl Pts',(33.063913821831,-0.3852661838525,32.2237752239193));
#54902=CARTESIAN_POINT('Ctrl Pts',(33.3002855853305,-0.546548570379162,
32.2376137192772));
#54903=CARTESIAN_POINT('Ctrl Pts',(33.5849541050556,-0.575659610572502,
32.2514522146351));
#54904=CARTESIAN_POINT('Ctrl Pts',(33.8490782504097,-0.465559407918213,
32.265290709993));
#54905=CARTESIAN_POINT('Ctrl Pts',(34.028785118265,-0.242873394820758,32.2791292053509));
#54906=CARTESIAN_POINT('Ctrl Pts',(34.0806163593418,0.0385464716279787,
32.2929677007088));
#54907=CARTESIAN_POINT('Ctrl Pts',(33.9920376715003,0.310644679714432,32.3068061960667));
#54908=CARTESIAN_POINT('Ctrl Pts',(33.7844699586874,0.507619965933842,32.3206446914246));
#54909=CARTESIAN_POINT('Ctrl Pts',(33.5081091331142,0.581837975015737,32.3344831867824));
#54910=CARTESIAN_POINT('Ctrl Pts',(33.229787283216,0.515350632966022,32.3483216821404));
#54911=CARTESIAN_POINT('Ctrl Pts',(33.0168107301666,0.324236513564037,32.3621601774982));
#54912=CARTESIAN_POINT('Ctrl Pts',(32.9206834011183,0.0547125714111669,
32.3759986728561));
#54913=CARTESIAN_POINT('Ctrl Pts',(32.9646516810921,-0.228042462389705,
32.389837168214));
#54914=CARTESIAN_POINT('Ctrl Pts',(33.1380827607183,-0.455650193812121,
32.4036756635719));
#54915=CARTESIAN_POINT('Ctrl Pts',(33.3990359589075,-0.573068451074164,
32.4175141589298));
#54916=CARTESIAN_POINT('Ctrl Pts',(33.6844051998157,-0.551902083245937,
32.4313526542877));
#54917=CARTESIAN_POINT('Ctrl Pts',(33.9251798980768,-0.39726973391094,32.4451911496456));
#54918=CARTESIAN_POINT('Ctrl Pts',(34.0631337262299,-0.146566004218914,
32.4590296450035));
#54919=CARTESIAN_POINT('Ctrl Pts',(34.0649054348142,0.139581649680744,32.4728681403614));
#54920=CARTESIAN_POINT('Ctrl Pts',(33.9300665731457,0.39197439951226,32.4867066357193));
#54921=CARTESIAN_POINT('Ctrl Pts',(33.691225101158,0.549576334913893,32.5005451310771));
#54922=CARTESIAN_POINT('Ctrl Pts',(33.4061398359513,0.574274722423879,32.514383626435));
#54923=CARTESIAN_POINT('Ctrl Pts',(33.1437526893048,0.460096773334361,32.5282221217929));
#54924=CARTESIAN_POINT('Ctrl Pts',(32.9675165075204,0.234654037781256,32.5420606171508));
#54925=CARTESIAN_POINT('Ctrl Pts',(32.9200503270051,-0.0475348714460054,
32.5558991125087));
#54926=CARTESIAN_POINT('Ctrl Pts',(33.012832851252,-0.318228465714449,32.5697376078666));
#54927=CARTESIAN_POINT('Ctrl Pts',(33.2234265663591,-0.511965158008226,
32.5835761032245));
#54928=CARTESIAN_POINT('Ctrl Pts',(33.5009037847184,-0.581893779296067,
32.5974145985824));
#54929=CARTESIAN_POINT('Ctrl Pts',(33.7781624416367,-0.511103554353669,
32.6112530939403));
#54930=CARTESIAN_POINT('Ctrl Pts',(33.988153326937,-0.316713619237659,32.6250915892982));
#54931=CARTESIAN_POINT('Ctrl Pts',(34.0800945347976,-0.0457331161000383,
32.6389300846561));
#54932=CARTESIAN_POINT('Ctrl Pts',(34.0317520060973,0.23630698513106,32.652768580014));
#54933=CARTESIAN_POINT('Ctrl Pts',(33.8548163708181,0.461201181925759,32.6666070753719));
#54934=CARTESIAN_POINT('Ctrl Pts',(33.5920758135727,0.574563514126331,32.6804455707298));
#54935=CARTESIAN_POINT('Ctrl Pts',(33.3070686456285,0.54897967149125,32.6942840660877));
#54936=CARTESIAN_POINT('Ctrl Pts',(33.0687178925743,0.390636571540241,32.7081225614455));
#54937=CARTESIAN_POINT('Ctrl Pts',(32.9346637013945,0.137826182887542,32.7219610568034));
#54938=CARTESIAN_POINT('Ctrl Pts',(32.9373242758685,-0.1483145868868,32.7357995521613));
#54939=CARTESIAN_POINT('Ctrl Pts',(33.0760562116781,-0.398588574288813,
32.7496380475192));
#54940=CARTESIAN_POINT('Ctrl Pts',(33.317310090292,-0.552472247358322,32.7634765428771));
#54941=CARTESIAN_POINT('Ctrl Pts',(33.602743704498,-0.572752056649567,32.777315038235));
#54942=CARTESIAN_POINT('Ctrl Pts',(33.8633309015935,-0.454523754228012,
32.7911535335929));
#54943=CARTESIAN_POINT('Ctrl Pts',(34.0360541154482,-0.226378383511662,
32.8049920289508));
#54944=CARTESIAN_POINT('Ctrl Pts',(34.0791438475116,0.0565118668934944,
32.8188305243087));
#54945=CARTESIAN_POINT('Ctrl Pts',(33.9821797468604,0.32573590365191,32.8326690196666));
#54946=CARTESIAN_POINT('Ctrl Pts',(33.7686105542355,0.516187521510932,32.8465075150245));
#54947=CARTESIAN_POINT('Ctrl Pts',(33.4900835142814,0.581809978017969,32.8603460103823));
#54948=CARTESIAN_POINT('Ctrl Pts',(33.2139545690976,0.506733853882039,32.8741845057402));
#54949=CARTESIAN_POINT('Ctrl Pts',(33.0069997316946,0.309114740284451,32.8880230010981));
#54950=CARTESIAN_POINT('Ctrl Pts',(32.9192667031776,0.0367426886880944,
32.901861496456));
#54951=CARTESIAN_POINT('Ctrl Pts',(32.971971882464,-0.244514814074009,32.9156999918139));
#54952=CARTESIAN_POINT('Ctrl Pts',(33.1523696237274,-0.466641520551743,
32.9295384871718));
#54953=CARTESIAN_POINT('Ctrl Pts',(33.416834504397,-0.575920730267091,32.9433769825297));
#54954=CARTESIAN_POINT('Ctrl Pts',(33.7014112216316,-0.54592555079529,32.9572154778876));
#54955=CARTESIAN_POINT('Ctrl Pts',(33.9372808453481,-0.383909689252521,
32.9710539732455));
#54956=CARTESIAN_POINT('Ctrl Pts',(34.0674032378252,-0.12905329486615,32.9848924686034));
#54957=CARTESIAN_POINT('Ctrl Pts',(34.0603110186069,0.157011941068149,32.9987309639613));
#54958=CARTESIAN_POINT('Ctrl Pts',(33.9177192926508,0.405107121336604,33.0125694593192));
#54959=CARTESIAN_POINT('Ctrl Pts',(33.6741108880475,0.555235612937064,33.0264079546771));
#54960=CARTESIAN_POINT('Ctrl Pts',(33.3883974048991,0.571091978561265,33.0402464500349));
#54961=CARTESIAN_POINT('Ctrl Pts',(33.1296726763614,0.448841687654951,33.0540849453928));
#54962=CARTESIAN_POINT('Ctrl Pts',(32.9605038694783,0.218048417472858,33.0679234407507));
#54963=CARTESIAN_POINT('Ctrl Pts',(32.9218009237779,-0.0654753042466776,
33.0817619361086));
#54964=CARTESIAN_POINT('Ctrl Pts',(33.0229233376058,-0.333165192373228,
33.0956004314665));
#54965=CARTESIAN_POINT('Ctrl Pts',(33.2394167691076,-0.5202860434299,33.1094389268244));
#54966=CARTESIAN_POINT('Ctrl Pts',(33.5189268075964,-0.581586591286704,
33.1232774221823));
#54967=CARTESIAN_POINT('Ctrl Pts',(33.7938597933266,-0.502242579911662,
33.1371159175402));
#54968=CARTESIAN_POINT('Ctrl Pts',(33.9977289310803,-0.301441699796153,
33.1509544128981));
#54969=CARTESIAN_POINT('Ctrl Pts',(34.081232731707,-0.0277434461216138,
33.164792908256));
#54970=CARTESIAN_POINT('Ctrl Pts',(34.024177546644,0.25266398002999,33.1786314036138));
#54971=CARTESIAN_POINT('Ctrl Pts',(33.8403609796792,0.471969904466537,33.1924698989718));
#54972=CARTESIAN_POINT('Ctrl Pts',(33.5742352249103,0.577139773878508,33.2063083943296));
#54973=CARTESIAN_POINT('Ctrl Pts',(33.2901572328587,0.542740453890609,33.2201468896875));
#54974=CARTESIAN_POINT('Ctrl Pts',(33.0568253273491,0.377090700932519,33.2339853850454));
#54975=CARTESIAN_POINT('Ctrl Pts',(32.9306659520014,0.120249444912251,33.2478238804033));
#54976=CARTESIAN_POINT('Ctrl Pts',(32.9421881144314,-0.165671625596998,
33.2616623757612));
#54977=CARTESIAN_POINT('Ctrl Pts',(33.0886054205063,-0.411528476741329,
33.2755008711191));
#54978=CARTESIAN_POINT('Ctrl Pts',(33.3345099055909,-0.557865768702293,
33.289339366477));
#54979=CARTESIAN_POINT('Ctrl Pts',(33.6204347104393,-0.569294886384073,
33.3031778618349));
#54980=CARTESIAN_POINT('Ctrl Pts',(33.877234898328,-0.44305193696872,33.3170163571928));
#54981=CARTESIAN_POINT('Ctrl Pts',(34.0428087117567,-0.209666137900871,
33.3308548525507));
#54982=CARTESIAN_POINT('Ctrl Pts',(34.0771155860204,0.0744230323611239,
33.3446933479086));
#54983=CARTESIAN_POINT('Ctrl Pts',(33.9718591188982,0.34051455066643,33.3585318432665));
#54984=CARTESIAN_POINT('Ctrl Pts',(33.752493390499,0.524259737088992,33.3723703386243));
#54985=CARTESIAN_POINT('Ctrl Pts',(33.4720674074124,0.581223678180666,33.3862088339822));
#54986=CARTESIAN_POINT('Ctrl Pts',(33.1983963500702,0.497630792858991,33.4000473293401));
#54987=CARTESIAN_POINT('Ctrl Pts',(32.997661798301,0.293696363265905,33.413885824698));
#54988=CARTESIAN_POINT('Ctrl Pts',(32.9184072961179,0.0187374594795893,
33.4277243200559));
#54989=CARTESIAN_POINT('Ctrl Pts',(32.9797986696284,-0.26075242182221,33.4415628154138));
#54990=CARTESIAN_POINT('Ctrl Pts',(33.1669901206639,-0.477185515651409,
33.4554013107717));
#54991=CARTESIAN_POINT('Ctrl Pts',(33.4347122287498,-0.578219926954068,
33.4692398061296));
#54992=CARTESIAN_POINT('Ctrl Pts',(33.7182239847251,-0.539427603955409,
33.4830783014875));
#54993=CARTESIAN_POINT('Ctrl Pts',(33.9489586056226,-0.370179773114848,
33.4969167968453));
#54994=CARTESIAN_POINT('Ctrl Pts',(34.0711269716252,-0.111430201531911,
33.5107552922033));
#54995=CARTESIAN_POINT('Ctrl Pts',(34.05515806946,0.174294902759664,33.5245937875611));
#54996=CARTESIAN_POINT('Ctrl Pts',(33.9550231205424,0.336612217580624,33.5338194511331));
#54997=CARTESIAN_POINT('Ctrl Pts',(33.8886143137352,0.40097402479828,33.5384322829191));
#54998=CARTESIAN_POINT('Ctrl Pts',(33.2416080183656,0.532271443393366,31.841675));
#54999=CARTESIAN_POINT('Ctrl Pts',(33.1534539004746,0.489476892804901,31.846287831786));
#55000=CARTESIAN_POINT('Ctrl Pts',(32.9989190855949,0.359252750922421,31.8555134953579));
#55001=CARTESIAN_POINT('Ctrl Pts',(32.8882398621671,0.0769451387279448,
31.8693519907158));
#55002=CARTESIAN_POINT('Ctrl Pts',(32.9255337596252,-0.223948726373027,
31.8831904860737));
#55003=CARTESIAN_POINT('Ctrl Pts',(33.1017391519043,-0.470702238484192,
31.8970289814316));
#55004=CARTESIAN_POINT('Ctrl Pts',(33.3742619176698,-0.603621394366995,
31.9108674767895));
#55005=CARTESIAN_POINT('Ctrl Pts',(33.6771894229262,-0.590570640248903,
31.9247059721474));
#55006=CARTESIAN_POINT('Ctrl Pts',(33.9372686405179,-0.43470164449802,31.9385444675052));
#55007=CARTESIAN_POINT('Ctrl Pts',(34.0916030729421,-0.173709796706028,
31.9523829628631));
#55008=CARTESIAN_POINT('Ctrl Pts',(34.1028709267224,0.12929036774781,31.966221458221));
#55009=CARTESIAN_POINT('Ctrl Pts',(33.9683469434777,0.401024228980704,31.9800599535789));
#55010=CARTESIAN_POINT('Ctrl Pts',(33.720563094964,0.575778813607474,31.9938984489368));
#55011=CARTESIAN_POINT('Ctrl Pts',(33.419440650526,0.61129330232012,32.0077369442947));
#55012=CARTESIAN_POINT('Ctrl Pts',(33.1377998113948,0.498979295293571,32.0215754396526));
#55013=CARTESIAN_POINT('Ctrl Pts',(32.9437495115802,0.265997571359909,32.0354139350105));
#55014=CARTESIAN_POINT('Ctrl Pts',(32.8842167663547,-0.0313101024039002,
32.0492524303684));
#55015=CARTESIAN_POINT('Ctrl Pts',(32.9735983224852,-0.321046083515054,
32.0630909257263));
#55016=CARTESIAN_POINT('Ctrl Pts',(33.1902791205241,-0.533143780225301,
32.0769294210842));
#55017=CARTESIAN_POINT('Ctrl Pts',(33.4818594384547,-0.616311799100504,
32.090767916442));
#55018=CARTESIAN_POINT('Ctrl Pts',(33.7778266720653,-0.550437693056534,
32.1046064117999));
#55019=CARTESIAN_POINT('Ctrl Pts',(34.0066073328682,-0.351451737706059,
32.1184449071578));
#55020=CARTESIAN_POINT('Ctrl Pts',(34.1128756006909,-0.0674745265510057,
32.1322834025157));
#55021=CARTESIAN_POINT('Ctrl Pts',(34.0709327164349,0.232819988308916,32.1461218978736));
#55022=CARTESIAN_POINT('Ctrl Pts',(33.8909216898682,0.47681185602353,32.1599603932315));
#55023=CARTESIAN_POINT('Ctrl Pts',(33.6163744246908,0.605496743947403,32.1737988885894));
#55024=CARTESIAN_POINT('Ctrl Pts',(33.3136844376707,0.587754902052959,32.1876373839473));
#55025=CARTESIAN_POINT('Ctrl Pts',(33.0560509745358,0.427876823913913,32.2014758793052));
#55026=CARTESIAN_POINT('Ctrl Pts',(32.9057773026054,0.164525680531654,32.2153143746631));
#55027=CARTESIAN_POINT('Ctrl Pts',(32.8992039680155,-0.138612559333598,
32.229152870021));
#55028=CARTESIAN_POINT('Ctrl Pts',(33.0379205943234,-0.408230249372622,
32.2429913653788));
#55029=CARTESIAN_POINT('Ctrl Pts',(33.2883814652805,-0.579125987516094,
32.2568298607368));
#55030=CARTESIAN_POINT('Ctrl Pts',(33.5900178550457,-0.609972212011555,
32.2706683560946));
#55031=CARTESIAN_POINT('Ctrl Pts',(33.8698853083609,-0.493309408294673,
32.2845068514525));
#55032=CARTESIAN_POINT('Ctrl Pts',(34.0603037321762,-0.257350036647943,
32.2983453468104));
#55033=CARTESIAN_POINT('Ctrl Pts',(34.1152244113246,0.0408440615466747,
32.3121838421683));
#55034=CARTESIAN_POINT('Ctrl Pts',(34.0213659276522,0.329160877287513,32.3260223375262));
#55035=CARTESIAN_POINT('Ctrl Pts',(33.8014259933554,0.537877015853101,32.3398608328841));
#55036=CARTESIAN_POINT('Ctrl Pts',(33.5085924837739,0.61651884227159,32.353699328242));
#55037=CARTESIAN_POINT('Ctrl Pts',(33.2136810616147,0.546068474804433,32.3675378235999));
#55038=CARTESIAN_POINT('Ctrl Pts',(32.9880098893035,0.343562862082473,32.3813763189578));
#55039=CARTESIAN_POINT('Ctrl Pts',(32.8861528222842,0.0579737532312202,
32.3952148143157));
#55040=CARTESIAN_POINT('Ctrl Pts',(32.9327418629281,-0.241635095917313,
32.4090533096736));
#55041=CARTESIAN_POINT('Ctrl Pts',(33.1165104256833,-0.482809548418142,
32.4228918050314));
#55042=CARTESIAN_POINT('Ctrl Pts',(33.3930179252673,-0.607226604604248,
32.4367303003893));
#55043=CARTESIAN_POINT('Ctrl Pts',(33.6953968032014,-0.584798600333471,
32.4505687957472));
#55044=CARTESIAN_POINT('Ctrl Pts',(33.9505230489852,-0.420949279588861,
32.4644072911051));
#55045=CARTESIAN_POINT('Ctrl Pts',(34.0966997134038,-0.155302175377904,
32.478245786463));
#55046=CARTESIAN_POINT('Ctrl Pts',(34.0985770259413,0.147901513408784,32.4920842818209));
#55047=CARTESIAN_POINT('Ctrl Pts',(33.955700997805,0.41533831300864,32.5059227771788));
#55048=CARTESIAN_POINT('Ctrl Pts',(33.7026232096246,0.582334224114217,32.5197612725367));
#55049=CARTESIAN_POINT('Ctrl Pts',(33.4005452339662,0.608504776617635,32.5335997678946));
#55050=CARTESIAN_POINT('Ctrl Pts',(33.1225183144049,0.487521169482489,32.5474382632525));
#55051=CARTESIAN_POINT('Ctrl Pts',(32.9357774493778,0.248640758973048,32.5612767586104));
#55052=CARTESIAN_POINT('Ctrl Pts',(32.8854820133373,-0.0503682213431094,
32.5751152539682));
#55053=CARTESIAN_POINT('Ctrl Pts',(32.9837949060806,-0.337196700258056,
32.5889537493262));
#55054=CARTESIAN_POINT('Ctrl Pts',(33.2069412096955,-0.542481206198488,
32.602792244684));
#55055=CARTESIAN_POINT('Ctrl Pts',(33.5009576554507,-0.616577972805828,
32.6166307400419));
#55056=CARTESIAN_POINT('Ctrl Pts',(33.7947425122547,-0.541568246043921,
32.6304692353998));
#55057=CARTESIAN_POINT('Ctrl Pts',(34.0172500539623,-0.335591560277182,
32.6443077307577));
#55058=CARTESIAN_POINT('Ctrl Pts',(34.1146714830565,-0.048459071085393,
32.6581462261156));
#55059=CARTESIAN_POINT('Ctrl Pts',(34.0634474634727,0.250392231427916,32.6719847214735));
#55060=CARTESIAN_POINT('Ctrl Pts',(33.8759654535266,0.488691407135238,32.6858232168314));
#55061=CARTESIAN_POINT('Ctrl Pts',(33.5975640580757,0.608810781955373,32.6996617121893));
#55062=CARTESIAN_POINT('Ctrl Pts',(33.2955688347228,0.581701996142946,32.7135002075472));
#55063=CARTESIAN_POINT('Ctrl Pts',(33.0430110151278,0.413920742846699,32.7273387029051));
#55064=CARTESIAN_POINT('Ctrl Pts',(32.9009664283241,0.146041410766017,32.741177198263));
#55065=CARTESIAN_POINT('Ctrl Pts',(32.9037855882362,-0.15715498356216,32.7550156936208));
#55066=CARTESIAN_POINT('Ctrl Pts',(33.0507867399728,-0.422346730387571,
32.7688541889787));
#55067=CARTESIAN_POINT('Ctrl Pts',(33.3064207279959,-0.585402749484206,
32.7826926843366));
#55068=CARTESIAN_POINT('Ctrl Pts',(33.608867816244,-0.606891351264435,32.7965311796945));
#55069=CARTESIAN_POINT('Ctrl Pts',(33.8849874989783,-0.481615966599657,
32.8103696750524));
#55070=CARTESIAN_POINT('Ctrl Pts',(34.0680060031181,-0.239871828431531,
32.8242081704103));
#55071=CARTESIAN_POINT('Ctrl Pts',(34.113664129377,0.0598802970033712,32.8380466657682));
#55072=CARTESIAN_POINT('Ctrl Pts',(34.0109204143871,0.345151624385351,32.8518851611261));
#55073=CARTESIAN_POINT('Ctrl Pts',(33.7846212777959,0.546955246687625,32.865723656484));
#55074=CARTESIAN_POINT('Ctrl Pts',(33.4894924350813,0.616489176492813,32.8795621518419));
#55075=CARTESIAN_POINT('Ctrl Pts',(33.1969046272852,0.536938086460799,32.8934006471998));
#55076=CARTESIAN_POINT('Ctrl Pts',(32.977614099274,0.327539744727214,32.9072391425577));
#55077=CARTESIAN_POINT('Ctrl Pts',(32.8846516810529,0.0389327628388598,
32.9210776379156));
#55078=CARTESIAN_POINT('Ctrl Pts',(32.9404983901208,-0.259089293865844,
32.9349161332734));
#55079=CARTESIAN_POINT('Ctrl Pts',(33.1316488673462,-0.494456021023092,
32.9487546286313));
#55080=CARTESIAN_POINT('Ctrl Pts',(33.4118773657482,-0.610248895931676,
32.9625931239892));
#55081=CARTESIAN_POINT('Ctrl Pts',(33.7134164810701,-0.578465832405816,
32.9764316193471));
#55082=CARTESIAN_POINT('Ctrl Pts',(33.9633452818445,-0.406792899945056,
32.990270114705));
#55083=CARTESIAN_POINT('Ctrl Pts',(34.1012237122812,-0.136745608500479,
33.0041086100629));
#55084=CARTESIAN_POINT('Ctrl Pts',(34.0937087562808,0.166370749739275,33.0179471054208));
#55085=CARTESIAN_POINT('Ctrl Pts',(33.9426177488545,0.4292538200788,33.0317856007787));
#55086=CARTESIAN_POINT('Ctrl Pts',(33.684488891642,0.588330827438097,33.0456240961366));
#55087=CARTESIAN_POINT('Ctrl Pts',(33.3817452526638,0.605132323038317,33.0594625914945));
#55088=CARTESIAN_POINT('Ctrl Pts',(33.1075990522533,0.475595216398127,33.0733010868524));
#55089=CARTESIAN_POINT('Ctrl Pts',(32.9283468180463,0.231045348829085,33.0871395822102));
#55090=CARTESIAN_POINT('Ctrl Pts',(32.8873369556786,-0.0693780064294515,
33.1009780775682));
#55091=CARTESIAN_POINT('Ctrl Pts',(32.9944868430664,-0.353023741156768,
33.114816572926));
#55092=CARTESIAN_POINT('Ctrl Pts',(33.2238845198771,-0.551298063927147,
33.1286550682839));
#55093=CARTESIAN_POINT('Ctrl Pts',(33.5200549534549,-0.616252474636192,
33.1424935636418));
#55094=CARTESIAN_POINT('Ctrl Pts',(33.8113755157816,-0.532179106903876,
33.1563320589997));
#55095=CARTESIAN_POINT('Ctrl Pts',(34.0273964188164,-0.319409347190992,
33.1701705543576));
#55096=CARTESIAN_POINT('Ctrl Pts',(34.115877523004,-0.0293971140042204,
33.1840090497155));
#55097=CARTESIAN_POINT('Ctrl Pts',(34.0554215229643,0.26772419666765,33.1978475450734));
#55098=CARTESIAN_POINT('Ctrl Pts',(33.8606484384945,0.500102007059391,33.2116860404313));
#55099=CARTESIAN_POINT('Ctrl Pts',(33.5786600684087,0.611540601506529,33.2255245357892));
#55100=CARTESIAN_POINT('Ctrl Pts',(33.2776494051397,0.57509088552968,33.2393630311471));
#55101=CARTESIAN_POINT('Ctrl Pts',(33.0304095850749,0.39956746096542,33.253201526505));
#55102=CARTESIAN_POINT('Ctrl Pts',(32.8967303902286,0.127416998794378,33.2670400218629));
#55103=CARTESIAN_POINT('Ctrl Pts',(32.9089393393637,-0.1755466009374,33.2808785172207));
#55104=CARTESIAN_POINT('Ctrl Pts',(33.0640839533387,-0.436057924949798,
33.2947170125786));
#55105=CARTESIAN_POINT('Ctrl Pts',(33.3246457505464,-0.591117755512582,
33.3085555079365));
#55106=CARTESIAN_POINT('Ctrl Pts',(33.6276133072053,-0.603228113900871,
33.3223940032944));
#55107=CARTESIAN_POINT('Ctrl Pts',(33.8997202533495,-0.469460363495101,
33.3362324986523));
#55108=CARTESIAN_POINT('Ctrl Pts',(34.0751632119545,-0.22216343750802,33.3500709940102));
#55109=CARTESIAN_POINT('Ctrl Pts',(34.1115149719139,0.0788590702564221,
33.3639094893681));
#55110=CARTESIAN_POINT('Ctrl Pts',(33.9999846180383,0.360811163189923,33.377747984726));
#55111=CARTESIAN_POINT('Ctrl Pts',(33.7675434390261,0.555508612429381,33.3915864800839));
#55112=CARTESIAN_POINT('Ctrl Pts',(33.4704024653199,0.615867929835772,33.4054249754418));
#55113=CARTESIAN_POINT('Ctrl Pts',(33.1804190495222,0.527292430996483,33.4192634707997));
#55114=CARTESIAN_POINT('Ctrl Pts',(32.967719571704,0.311202344355704,33.4331019661576));
#55115=CARTESIAN_POINT('Ctrl Pts',(32.8837410484228,0.0198543191086066,
33.4469404615155));
#55116=CARTESIAN_POINT('Ctrl Pts',(32.9487916985133,-0.276294755798628,
33.4607789568733));
#55117=CARTESIAN_POINT('Ctrl Pts',(33.1471408294247,-0.505628498466812,
33.4746174522312));
#55118=CARTESIAN_POINT('Ctrl Pts',(33.430820704605,-0.61268513787613,33.4884559475891));
#55119=CARTESIAN_POINT('Ctrl Pts',(33.7312313808926,-0.571580570812573,
33.502294442947));
#55120=CARTESIAN_POINT('Ctrl Pts',(33.9757191033446,-0.392244602368818,
33.5161329383049));
#55121=CARTESIAN_POINT('Ctrl Pts',(34.1051694018887,-0.118072078125678,
33.5299714336628));
#55122=CARTESIAN_POINT('Ctrl Pts',(34.0882486619268,0.184683874682329,33.5438099290207));
#55123=CARTESIAN_POINT('Ctrl Pts',(33.9821450979991,0.356676228758814,33.5530355925926));
#55124=CARTESIAN_POINT('Ctrl Pts',(33.9117779469236,0.424874367375091,33.5576484243786));
#55125=CARTESIAN_POINT('',(33.6760249362314,-0.564909144196547,33.5));
#55126=CARTESIAN_POINT('Ctrl Pts',(33.6760249362314,-0.564909144196542,
33.5));
#55127=CARTESIAN_POINT('Ctrl Pts',(33.6911122757525,-0.558840417608856,
33.5));
#55128=CARTESIAN_POINT('Ctrl Pts',(33.7059244375066,-0.552154731533978,
33.5));
#55129=CARTESIAN_POINT('Ctrl Pts',(33.7204203841144,-0.544857622697481,
33.5));
#55130=CARTESIAN_POINT('Ctrl Pts',(33.7417770502642,-0.534106898960881,
33.5));
#55131=CARTESIAN_POINT('Ctrl Pts',(33.7624481830748,-0.52202962717952,33.5));
#55132=CARTESIAN_POINT('Ctrl Pts',(33.7823236701149,-0.508709918934891,
33.5));
#55133=CARTESIAN_POINT('Ctrl Pts',(33.7907449420496,-0.503066339736406,
33.5));
#55134=CARTESIAN_POINT('Ctrl Pts',(33.7990231813029,-0.497199521839695,
33.5));
#55135=CARTESIAN_POINT('Ctrl Pts',(33.8071490502093,-0.49111511150774,33.5));
#55136=CARTESIAN_POINT('Ctrl Pts',(33.8133814475092,-0.486448476719381,
33.5));
#55137=CARTESIAN_POINT('Ctrl Pts',(33.8195200720538,-0.481656796007188,
33.5));
#55138=CARTESIAN_POINT('Ctrl Pts',(33.8255551722681,-0.476747944565078,
33.5));
#55139=CARTESIAN_POINT('Ctrl Pts',(33.8464600611014,-0.459744251162589,
33.5));
#55140=CARTESIAN_POINT('Ctrl Pts',(33.8661480360983,-0.441319459139679,
33.5));
#55141=CARTESIAN_POINT('Ctrl Pts',(33.8844537797586,-0.42159231484267,33.5));
#55142=CARTESIAN_POINT('Ctrl Pts',(33.8921079577626,-0.413343806791768,
33.5));
#55143=CARTESIAN_POINT('Ctrl Pts',(33.8995200933928,-0.40486733827089,33.5));
#55144=CARTESIAN_POINT('Ctrl Pts',(33.9066762790281,-0.396170620269095,
33.5));
#55145=CARTESIAN_POINT('Ctrl Pts',(33.9132917197804,-0.388131054834033,
33.5));
#55146=CARTESIAN_POINT('Ctrl Pts',(33.9196920796633,-0.379897755733789,
33.5));
#55147=CARTESIAN_POINT('Ctrl Pts',(33.9258448740597,-0.37150609087778,33.5));
#55148=CARTESIAN_POINT('Ctrl Pts',(33.9289541933474,-0.367265356715093,
33.5));
#55149=CARTESIAN_POINT('Ctrl Pts',(33.9320012373505,-0.362983155325591,
33.5));
#55150=CARTESIAN_POINT('Ctrl Pts',(33.9349848660807,-0.358660426862662,
33.5));
#55151=CARTESIAN_POINT('Ctrl Pts',(33.9511257768077,-0.335275220281268,
33.5));
#55152=CARTESIAN_POINT('Ctrl Pts',(33.965414668381,-0.310705612220643,33.5));
#55153=CARTESIAN_POINT('Ctrl Pts',(33.9777661289714,-0.285187438614856,
33.5));
#55154=CARTESIAN_POINT('Ctrl Pts',(33.9854825529834,-0.269245271604584,
33.5));
#55155=CARTESIAN_POINT('Ctrl Pts',(33.9924418668927,-0.252932378117298,
33.5));
#55156=CARTESIAN_POINT('Ctrl Pts',(33.998613146102,-0.236304071866443,33.5));
#55157=CARTESIAN_POINT('Ctrl Pts',(34.0036563734748,-0.222715263711188,
33.5));
#55158=CARTESIAN_POINT('Ctrl Pts',(34.0081731898733,-0.208915758312357,
33.5));
#55159=CARTESIAN_POINT('Ctrl Pts',(34.0121425784944,-0.194935980493716,
33.5));
#55160=CARTESIAN_POINT('Ctrl Pts',(34.0136761904768,-0.189534757076068,
33.5));
#55161=CARTESIAN_POINT('Ctrl Pts',(34.0151273441099,-0.184108772924433,
33.5));
#55162=CARTESIAN_POINT('Ctrl Pts',(34.0164930221575,-0.17866833866244,33.5));
#55163=CARTESIAN_POINT('Ctrl Pts',(34.0227201539916,-0.153861392804361,
33.5));
#55164=CARTESIAN_POINT('Ctrl Pts',(34.0271877526469,-0.128703923630915,
33.5));
#55165=CARTESIAN_POINT('Ctrl Pts',(34.029818588611,-0.103366805055813,33.5));
#55166=CARTESIAN_POINT('Ctrl Pts',(34.0320826207061,-0.0815623100458099,
33.5));
#55167=CARTESIAN_POINT('Ctrl Pts',(34.0329856460914,-0.0596242711054819,
33.5));
#55168=CARTESIAN_POINT('Ctrl Pts',(34.0325345483032,-0.0376796328618632,
33.5));
#55169=CARTESIAN_POINT('Ctrl Pts',(34.0322528803194,-0.0239772779168079,
33.5));
#55170=CARTESIAN_POINT('Ctrl Pts',(34.0314428596882,-0.0102724241422518,
33.5));
#55171=CARTESIAN_POINT('Ctrl Pts',(34.0301023506548,0.00340237109113172,
33.5));
#55172=CARTESIAN_POINT('Ctrl Pts',(34.0292916947886,0.0116720303766825,
33.5));
#55173=CARTESIAN_POINT('Ctrl Pts',(34.0282860950337,0.0199351010588,33.5));
#55174=CARTESIAN_POINT('Ctrl Pts',(34.0270894236949,0.0281557507514959,
33.5));
#55175=CARTESIAN_POINT('Ctrl Pts',(34.0232241120248,0.0547088837317084,
33.5));
#55176=CARTESIAN_POINT('Ctrl Pts',(34.0173659683933,0.0808741381588435,
33.5));
#55177=CARTESIAN_POINT('Ctrl Pts',(34.0095386293675,0.106418114041308,33.5));
#55178=CARTESIAN_POINT('Ctrl Pts',(34.0045436985712,0.122718722891032,33.5));
#55179=CARTESIAN_POINT('Ctrl Pts',(33.9987458654949,0.13876610958674,33.5));
#55180=CARTESIAN_POINT('Ctrl Pts',(33.9921415044704,0.154494222574271,33.5));
#55181=CARTESIAN_POINT('Ctrl Pts',(33.9867522237381,0.16732865363659,33.5));
#55182=CARTESIAN_POINT('Ctrl Pts',(33.9808256851105,0.179950413411563,33.5));
#55183=CARTESIAN_POINT('Ctrl Pts',(33.9743780260007,0.19232756964181,33.5));
#55184=CARTESIAN_POINT('Ctrl Pts',(33.9716025348906,0.197655501298915,33.5));
#55185=CARTESIAN_POINT('Ctrl Pts',(33.9687292815229,0.20294011721496,33.5));
#55186=CARTESIAN_POINT('Ctrl Pts',(33.9657632598639,0.208171980084317,33.5));
#55187=CARTESIAN_POINT('Ctrl Pts',(33.9528122203456,0.231016743395765,33.5));
#55188=CARTESIAN_POINT('Ctrl Pts',(33.9381451291001,0.252774726602467,33.5));
#55189=CARTESIAN_POINT('Ctrl Pts',(33.9219062551012,0.273259989548275,33.5));
#55190=CARTESIAN_POINT('Ctrl Pts',(33.9059968779726,0.29332959374667,33.5));
#55191=CARTESIAN_POINT('Ctrl Pts',(33.8885778372857,0.312178402515089,33.5));
#55192=CARTESIAN_POINT('Ctrl Pts',(33.869754609251,0.329593084869071,33.5));
#55193=CARTESIAN_POINT('Ctrl Pts',(33.8609062152635,0.337779351876591,33.5));
#55194=CARTESIAN_POINT('Ctrl Pts',(33.8517471877261,0.345648082814158,33.5));
#55195=CARTESIAN_POINT('Ctrl Pts',(33.8422870473583,0.35317333964466,33.5));
#55196=CARTESIAN_POINT('Ctrl Pts',(32.9082781605688,6.35800992875699E-6,
33.4478374807795));
#55197=CARTESIAN_POINT('Ctrl Pts',(32.9083290258001,-0.0916129522026867,
33.4521513061441));
#55198=CARTESIAN_POINT('Ctrl Pts',(32.9299537694797,-0.183255414133556,
33.4564651315087));
#55199=CARTESIAN_POINT('Ctrl Pts',(32.9710081119835,-0.265158867092123,
33.4607789568733));
#55200=CARTESIAN_POINT('Ctrl Pts',(33.0149080754838,-0.352739336688025,
33.4653917886593));
#55201=CARTESIAN_POINT('Ctrl Pts',(33.0810244524542,-0.429183917577418,
33.4700046204453));
#55202=CARTESIAN_POINT('Ctrl Pts',(33.1613626201362,-0.485248981257002,
33.4746174522312));
#55203=CARTESIAN_POINT('Ctrl Pts',(33.2417007878181,-0.541314044936585,
33.4792302840172));
#55204=CARTESIAN_POINT('Ctrl Pts',(33.3362607462115,-0.576999591406357,
33.4838431158032));
#55205=CARTESIAN_POINT('Ctrl Pts',(33.4336091714562,-0.587991603463984,
33.4884559475891));
#55206=CARTESIAN_POINT('Ctrl Pts',(33.5148170841719,-0.597161123705348,
33.4923039650594));
#55207=CARTESIAN_POINT('Ctrl Pts',(33.5979654552171,-0.589146729956918,
33.4961519825297));
#55208=CARTESIAN_POINT('Ctrl Pts',(33.6760249362314,-0.564909144196547,
33.5));
#55209=CARTESIAN_POINT('',(33.214273727605,-0.400339288800258,31.841675));
#55210=CARTESIAN_POINT('Ctrl Pts',(33.214273727605,-0.400339288800269,31.841675));
#55211=CARTESIAN_POINT('Ctrl Pts',(33.202445536308,-0.393549802407431,31.841675));
#55212=CARTESIAN_POINT('Ctrl Pts',(33.1909188893102,-0.386274380346431,
31.841675));
#55213=CARTESIAN_POINT('Ctrl Pts',(33.1797255998311,-0.378530861128202,
31.841675));
#55214=CARTESIAN_POINT('Ctrl Pts',(33.1623725701358,-0.36652603277173,31.841675));
#55215=CARTESIAN_POINT('Ctrl Pts',(33.1458201190519,-0.353397217584822,
31.841675));
#55216=CARTESIAN_POINT('Ctrl Pts',(33.1301375000556,-0.33925697081958,31.841675));
#55217=CARTESIAN_POINT('Ctrl Pts',(33.1236496305693,-0.333407177775548,
31.841675));
#55218=CARTESIAN_POINT('Ctrl Pts',(33.1173107384902,-0.327384026765024,
31.841675));
#55219=CARTESIAN_POINT('Ctrl Pts',(33.1111262805031,-0.321194485935576,
31.841675));
#55220=CARTESIAN_POINT('Ctrl Pts',(33.1058978843992,-0.31596179275138,31.841675));
#55221=CARTESIAN_POINT('Ctrl Pts',(33.1007867492974,-0.310617016155103,
31.841675));
#55222=CARTESIAN_POINT('Ctrl Pts',(33.0957966844085,-0.305166390094826,
31.841675));
#55223=CARTESIAN_POINT('Ctrl Pts',(33.0798413474256,-0.287738445269293,
31.841675));
#55224=CARTESIAN_POINT('Ctrl Pts',(33.0651186646452,-0.269226640989678,
31.841675));
#55225=CARTESIAN_POINT('Ctrl Pts',(33.0517262526342,-0.249778295685198,
31.841675));
#55226=CARTESIAN_POINT('Ctrl Pts',(33.0448378287756,-0.239774985923105,
31.841675));
#55227=CARTESIAN_POINT('Ctrl Pts',(33.0383016109362,-0.229523445428141,
31.841675));
#55228=CARTESIAN_POINT('Ctrl Pts',(33.0321330309045,-0.219041184108565,
31.841675));
#55229=CARTESIAN_POINT('Ctrl Pts',(33.0287567547832,-0.213303881778108,
31.841675));
#55230=CARTESIAN_POINT('Ctrl Pts',(33.0254915088972,-0.207498587651468,
31.841675));
#55231=CARTESIAN_POINT('Ctrl Pts',(33.0223453246647,-0.201639190709689,
31.841675));
#55232=CARTESIAN_POINT('Ctrl Pts',(33.0200641158264,-0.197390708388766,
31.841675));
#55233=CARTESIAN_POINT('Ctrl Pts',(33.0178446103249,-0.193112292436708,
31.841675));
#55234=CARTESIAN_POINT('Ctrl Pts',(33.0156875281279,-0.188805215535055,
31.841675));
#55235=CARTESIAN_POINT('Ctrl Pts',(33.0036409556039,-0.164751651728364,
31.841675));
#55236=CARTESIAN_POINT('Ctrl Pts',(32.9935380319056,-0.139807256470817,
31.841675));
#55237=CARTESIAN_POINT('Ctrl Pts',(32.985378164183,-0.114227460255648,31.841675));
#55238=CARTESIAN_POINT('Ctrl Pts',(32.9797053372983,-0.0964441136860784,
31.841675));
#55239=CARTESIAN_POINT('Ctrl Pts',(32.9749723925742,-0.078352707342488,
31.841675));
#55240=CARTESIAN_POINT('Ctrl Pts',(32.9711913497449,-0.0600308664810086,
31.841675));
#55241=CARTESIAN_POINT('Ctrl Pts',(32.9690190509139,-0.0495045341224176,
31.841675));
#55242=CARTESIAN_POINT('Ctrl Pts',(32.9671611459791,-0.0389020394357615,
31.841675));
#55243=CARTESIAN_POINT('Ctrl Pts',(32.9656215688667,-0.0282375501046256,
31.841675));
#55244=CARTESIAN_POINT('Ctrl Pts',(32.9647194634728,-0.0219887605696254,
31.841675));
#55245=CARTESIAN_POINT('Ctrl Pts',(32.9639268554194,-0.0157187328581642,
31.841675));
#55246=CARTESIAN_POINT('Ctrl Pts',(32.963245807483,-0.00944500166436709,
31.841675));
#55247=CARTESIAN_POINT('Ctrl Pts',(32.9604541038064,0.0162718348550039,
31.841675));
#55248=CARTESIAN_POINT('Ctrl Pts',(32.9595247742186,0.0421101434159377,
31.841675));
#55249=CARTESIAN_POINT('Ctrl Pts',(32.9604691671461,0.0678642555206383,
31.841675));
#55250=CARTESIAN_POINT('Ctrl Pts',(32.9613139098195,0.0909008506478625,
31.841675));
#55251=CARTESIAN_POINT('Ctrl Pts',(32.9636580310818,0.113870868334692,31.841675));
#55252=CARTESIAN_POINT('Ctrl Pts',(32.9674438169868,0.136645403709817,31.841675));
#55253=CARTESIAN_POINT('Ctrl Pts',(32.970078563272,0.152495513563676,31.841675));
#55254=CARTESIAN_POINT('Ctrl Pts',(32.9734121292935,0.168251080637884,31.841675));
#55255=CARTESIAN_POINT('Ctrl Pts',(32.9774321328346,0.183868477408068,31.841675));
#55256=CARTESIAN_POINT('Ctrl Pts',(32.9789897771462,0.189919802734665,31.841675));
#55257=CARTESIAN_POINT('Ctrl Pts',(32.9806498707955,0.195947306704219,31.841675));
#55258=CARTESIAN_POINT('Ctrl Pts',(32.9824083539019,0.201938602673053,31.841675));
#55259=CARTESIAN_POINT('Ctrl Pts',(32.9904800928408,0.229439678339,31.841675));
#55260=CARTESIAN_POINT('Ctrl Pts',(33.0006358559238,0.25623805384077,31.841675));
#55261=CARTESIAN_POINT('Ctrl Pts',(33.0127580426733,0.282097465557135,31.841675));
#55262=CARTESIAN_POINT('Ctrl Pts',(33.0205590508707,0.298738809808761,31.841675));
#55263=CARTESIAN_POINT('Ctrl Pts',(33.0291755271542,0.314991493911562,31.841675));
#55264=CARTESIAN_POINT('Ctrl Pts',(33.0385874388979,0.330791260825022,31.841675));
#55265=CARTESIAN_POINT('Ctrl Pts',(33.0459626520483,0.343172023828949,31.841675));
#55266=CARTESIAN_POINT('Ctrl Pts',(33.0538264742727,0.355274673381566,31.841675));
#55267=CARTESIAN_POINT('Ctrl Pts',(33.0621563230389,0.367079020916876,31.841675));
#55268=CARTESIAN_POINT('Ctrl Pts',(33.0657154626098,0.372122728383882,31.841675));
#55269=CARTESIAN_POINT('Ctrl Pts',(33.0693597192202,0.377111955976574,31.841675));
#55270=CARTESIAN_POINT('Ctrl Pts',(33.0730874902831,0.38204502655157,31.841675));
#55271=CARTESIAN_POINT('Ctrl Pts',(33.0770323210358,0.387265338684776,31.841675));
#55272=CARTESIAN_POINT('Ctrl Pts',(33.0810655061613,0.392415856119987,31.841675));
#55273=CARTESIAN_POINT('Ctrl Pts',(33.0851820902859,0.397492211415429,31.841675));
#55274=CARTESIAN_POINT('Ctrl Pts',(33.1035198571394,0.420105382203403,31.841675));
#55275=CARTESIAN_POINT('Ctrl Pts',(33.1235223899938,0.441266649917038,31.841675));
#55276=CARTESIAN_POINT('Ctrl Pts',(33.1449735740815,0.460832266340302,31.841675));
#55277=CARTESIAN_POINT('Ctrl Pts',(33.166583666432,0.480542822926494,31.841675));
#55278=CARTESIAN_POINT('Ctrl Pts',(33.1896647511158,0.4986350560007,31.841675));
#55279=CARTESIAN_POINT('Ctrl Pts',(33.2140396640545,0.51493431247186,31.841675));
#55280=CARTESIAN_POINT('Ctrl Pts',(33.223054381113,0.520962362119504,31.841675));
#55281=CARTESIAN_POINT('Ctrl Pts',(33.2322464335979,0.52674481929958,31.841675));
#55282=CARTESIAN_POINT('Ctrl Pts',(33.2416080183656,0.532271443393363,31.841675));
#55283=CARTESIAN_POINT('Ctrl Pts',(33.214273727605,-0.400339288800258,31.841675));
#55284=CARTESIAN_POINT('Ctrl Pts',(33.2696150942638,-0.439753488539296,
31.8455230174703));
#55285=CARTESIAN_POINT('Ctrl Pts',(33.4093978510072,-0.501155786006003,
31.8539838667265));
#55286=CARTESIAN_POINT('Ctrl Pts',(33.6472872572454,-0.490907009997742,
31.8670575477688));
#55287=CARTESIAN_POINT('Ctrl Pts',(33.8634759777288,-0.361342183302042,
31.8808960431267));
#55288=CARTESIAN_POINT('Ctrl Pts',(33.991765211222,-0.144394846435863,31.8947345384845));
#55289=CARTESIAN_POINT('Ctrl Pts',(34.0011315224325,0.107471559754204,31.9085730338424));
#55290=CARTESIAN_POINT('Ctrl Pts',(33.8893095626415,0.33334810735359,31.9224115292003));
#55291=CARTESIAN_POINT('Ctrl Pts',(33.6833412670481,0.478611425195411,31.9362500245582));
#55292=CARTESIAN_POINT('Ctrl Pts',(33.4330357002492,0.508132553198278,31.9500885199161));
#55293=CARTESIAN_POINT('Ctrl Pts',(33.1989240583753,0.414772454316571,31.963927015274));
#55294=CARTESIAN_POINT('Ctrl Pts',(33.0431189276735,0.227708852851754,31.9772938607689));
#55295=CARTESIAN_POINT('Ctrl Pts',(33.008198644534,0.07310466027816,31.9860478744779));
#55296=CARTESIAN_POINT('Ctrl Pts',(33.008142319392,-7.94017003037054E-6,
31.9901890564009));
#55297=CARTESIAN_POINT('Origin',(33.5,0.,31.841675));
#55298=CARTESIAN_POINT('',(32.908325,-7.24592894885513E-17,31.841675));
#55299=CARTESIAN_POINT('Origin',(33.5,0.,31.841675));
#55300=CARTESIAN_POINT('Origin',(33.5,0.,31.841675));
#55301=CARTESIAN_POINT('',(33.7857064634585,-0.400329423553981,31.841675));
#55302=CARTESIAN_POINT('Ctrl Pts',(33.7584134942914,0.532287118922758,31.841675));
#55303=CARTESIAN_POINT('Ctrl Pts',(33.772425355028,0.524033330922347,31.841675));
#55304=CARTESIAN_POINT('Ctrl Pts',(33.7860729882342,0.515210596415881,31.841675));
#55305=CARTESIAN_POINT('Ctrl Pts',(33.7993166435626,0.505830518481214,31.841675));
#55306=CARTESIAN_POINT('Ctrl Pts',(33.818828327284,0.492010986833412,31.841675));
#55307=CARTESIAN_POINT('Ctrl Pts',(33.8374640609541,0.476982159013618,31.841675));
#55308=CARTESIAN_POINT('Ctrl Pts',(33.8551275279765,0.460843647400137,31.841675));
#55309=CARTESIAN_POINT('Ctrl Pts',(33.8626115637645,0.454005737360827,31.841675));
#55310=CARTESIAN_POINT('Ctrl Pts',(33.8699208327767,0.446968452215185,31.841675));
#55311=CARTESIAN_POINT('Ctrl Pts',(33.87704694526,0.439738769381008,31.841675));
#55312=CARTESIAN_POINT('Ctrl Pts',(33.8825125471367,0.434193730882298,31.841675));
#55313=CARTESIAN_POINT('Ctrl Pts',(33.8878667536915,0.428539052549657,31.841675));
#55314=CARTESIAN_POINT('Ctrl Pts',(33.8931010987672,0.422783977549386,31.841675));
#55315=CARTESIAN_POINT('Ctrl Pts',(33.9112322648403,0.402849063231819,31.841675));
#55316=CARTESIAN_POINT('Ctrl Pts',(33.9279479391311,0.381690717831276,31.841675));
#55317=CARTESIAN_POINT('Ctrl Pts',(33.9431023913175,0.359451044338682,31.841675));
#55318=CARTESIAN_POINT('Ctrl Pts',(33.949438920161,0.350151972961984,31.841675));
#55319=CARTESIAN_POINT('Ctrl Pts',(33.9555020776674,0.340663643583745,31.841675));
#55320=CARTESIAN_POINT('Ctrl Pts',(33.961279263717,0.330995757663889,31.841675));
#55321=CARTESIAN_POINT('Ctrl Pts',(33.9666199068549,0.32205840855433,31.841675));
#55322=CARTESIAN_POINT('Ctrl Pts',(33.9717189491627,0.312961618041324,31.841675));
#55323=CARTESIAN_POINT('Ctrl Pts',(33.9765495520735,0.303745208622123,31.841675));
#55324=CARTESIAN_POINT('Ctrl Pts',(33.97899070078,0.299087689395735,31.841675));
#55325=CARTESIAN_POINT('Ctrl Pts',(33.9813640799093,0.294398468025505,31.841675));
#55326=CARTESIAN_POINT('Ctrl Pts',(33.9836687026571,0.289678644366065,31.841675));
#55327=CARTESIAN_POINT('Ctrl Pts',(33.9961363097837,0.264145221532597,31.841675));
#55328=CARTESIAN_POINT('Ctrl Pts',(34.0065957896222,0.237717256001346,31.841675));
#55329=CARTESIAN_POINT('Ctrl Pts',(34.0149979074777,0.210640694239323,31.841675));
#55330=CARTESIAN_POINT('Ctrl Pts',(34.0202470279456,0.193724943116885,31.841675));
#55331=CARTESIAN_POINT('Ctrl Pts',(34.0246921647938,0.176555688160426,31.841675));
#55332=CARTESIAN_POINT('Ctrl Pts',(34.0283110006646,0.159192241006528,31.841675));
#55333=CARTESIAN_POINT('Ctrl Pts',(34.0312683473334,0.145002668880409,31.841675));
#55334=CARTESIAN_POINT('Ctrl Pts',(34.033673720977,0.130683375434189,31.841675));
#55335=CARTESIAN_POINT('Ctrl Pts',(34.0355108840631,0.116267582911012,31.841675));
#55336=CARTESIAN_POINT('Ctrl Pts',(34.0362206899574,0.110697900729543,31.841675));
#55337=CARTESIAN_POINT('Ctrl Pts',(34.0368452644478,0.105116049648021,31.841675));
#55338=CARTESIAN_POINT('Ctrl Pts',(34.0373831639022,0.0995326752541386,
31.841675));
#55339=CARTESIAN_POINT('Ctrl Pts',(34.0398358433799,0.0740739623317904,
31.841675));
#55340=CARTESIAN_POINT('Ctrl Pts',(34.0404963744696,0.048531422070593,31.841675));
#55341=CARTESIAN_POINT('Ctrl Pts',(34.039313911727,0.0230855454553802,31.841675));
#55342=CARTESIAN_POINT('Ctrl Pts',(34.0382963136198,0.00118745518433947,
31.841675));
#55343=CARTESIAN_POINT('Ctrl Pts',(34.0359130277643,-0.0206394314362162,
31.841675));
#55344=CARTESIAN_POINT('Ctrl Pts',(34.0321898180806,-0.0422706211314857,
31.841675));
#55345=CARTESIAN_POINT('Ctrl Pts',(34.0298650251175,-0.0557772570344726,
31.841675));
#55346=CARTESIAN_POINT('Ctrl Pts',(34.0270174311808,-0.0692074605482755,
31.841675));
#55347=CARTESIAN_POINT('Ctrl Pts',(34.023649786498,-0.0825287204060243,
31.841675));
#55348=CARTESIAN_POINT('Ctrl Pts',(34.021613246018,-0.0905845836279709,
31.841675));
#55349=CARTESIAN_POINT('Ctrl Pts',(34.0193849316341,-0.0986048195598047,
31.841675));
#55350=CARTESIAN_POINT('Ctrl Pts',(34.0169740233629,-0.106554575906866,
31.841675));
#55351=CARTESIAN_POINT('Ctrl Pts',(34.0091866628973,-0.132232706853019,
31.841675));
#55352=CARTESIAN_POINT('Ctrl Pts',(33.9994867429401,-0.157229702919544,
31.841675));
#55353=CARTESIAN_POINT('Ctrl Pts',(33.9879324903209,-0.181318311028767,
31.841675));
#55354=CARTESIAN_POINT('Ctrl Pts',(33.980559268656,-0.1966901964327,31.841675));
#55355=CARTESIAN_POINT('Ctrl Pts',(33.9724299636648,-0.211691795026075,
31.841675));
#55356=CARTESIAN_POINT('Ctrl Pts',(33.9635508543046,-0.226257254386194,
31.841675));
#55357=CARTESIAN_POINT('Ctrl Pts',(33.9563053384283,-0.238142936019265,
31.841675));
#55358=CARTESIAN_POINT('Ctrl Pts',(33.948560349239,-0.249738097973514,31.841675));
#55359=CARTESIAN_POINT('Ctrl Pts',(33.9403366119352,-0.261013576093959,
31.841675));
#55360=CARTESIAN_POINT('Ctrl Pts',(33.9367965810775,-0.26586727448038,31.841675));
#55361=CARTESIAN_POINT('Ctrl Pts',(33.9331663529206,-0.270663543200871,
31.841675));
#55362=CARTESIAN_POINT('Ctrl Pts',(33.9294522747798,-0.275393796579051,
31.841675));
#55363=CARTESIAN_POINT('Ctrl Pts',(33.9132348705555,-0.296048297698745,
31.841675));
#55364=CARTESIAN_POINT('Ctrl Pts',(33.8954829555075,-0.315371933379871,
31.841675));
#55365=CARTESIAN_POINT('Ctrl Pts',(33.8763669491027,-0.333202393981228,
31.841675));
#55366=CARTESIAN_POINT('Ctrl Pts',(33.8576388146564,-0.350671066899168,
31.841675));
#55367=CARTESIAN_POINT('Ctrl Pts',(33.8376002565746,-0.366707183478365,
31.841675));
#55368=CARTESIAN_POINT('Ctrl Pts',(33.8163874271366,-0.381115557025756,
31.841675));
#55369=CARTESIAN_POINT('Ctrl Pts',(33.8064157396606,-0.387888618510642,
31.841675));
#55370=CARTESIAN_POINT('Ctrl Pts',(33.7961843225975,-0.394301315777978,
31.841675));
#55371=CARTESIAN_POINT('Ctrl Pts',(33.7857064634585,-0.400329423553973,
31.841675));
#55372=CARTESIAN_POINT('Origin',(33.5,0.,31.841675));
#55373=CARTESIAN_POINT('Origin',(33.5,0.,31.5181609435991));
#55374=CARTESIAN_POINT('Ctrl Pts',(33.7857064634585,-0.400329423553979,
31.841675));
#55375=CARTESIAN_POINT('Ctrl Pts',(33.8520085122293,-0.353011083307552,
31.846287831786));
#55376=CARTESIAN_POINT('Ctrl Pts',(33.9605676688256,-0.224818358029771,
31.8555134953579));
#55377=CARTESIAN_POINT('Ctrl Pts',(34.0120581005265,0.0219224808651154,
31.8693519907158));
#55378=CARTESIAN_POINT('Ctrl Pts',(33.9396949594551,0.263339931378287,31.8831904860737));
#55379=CARTESIAN_POINT('Ctrl Pts',(33.7610075704167,0.441089580123063,31.8970289814316));
#55380=CARTESIAN_POINT('Ctrl Pts',(33.5191964609478,0.512166069558742,31.9108674767895));
#55381=CARTESIAN_POINT('Ctrl Pts',(33.2727445863754,0.459388942606042,31.9247059721473));
#55382=CARTESIAN_POINT('Ctrl Pts',(33.081248792294,0.295517141979944,31.9385444675052));
#55383=CARTESIAN_POINT('Ctrl Pts',(33.0139716396026,0.120044930604756,31.9488627913225));
#55384=CARTESIAN_POINT('Ctrl Pts',(33.0081549344277,0.0193071207505607,
31.9545682833538));
#55385=CARTESIAN_POINT('Ctrl Pts',(33.0081744217127,1.25591105979584E-5,
31.9556609435991));
#55386=CARTESIAN_POINT('Ctrl Pts',(33.8437104087161,-0.481604049573127,
31.7840265756214));
#55387=CARTESIAN_POINT('Ctrl Pts',(33.9234730574357,-0.424679169859196,
31.7886394074074));
#55388=CARTESIAN_POINT('Ctrl Pts',(34.0540718252475,-0.27046083868707,31.7978650709793));
#55389=CARTESIAN_POINT('Ctrl Pts',(34.1160158117807,0.0263731690456256,
31.8117035663372));
#55390=CARTESIAN_POINT('Ctrl Pts',(34.0289615516405,0.316803037458948,31.8255420616951));
#55391=CARTESIAN_POINT('Ctrl Pts',(33.8139971620522,0.530639307313199,31.839380557053));
#55392=CARTESIAN_POINT('Ctrl Pts',(33.5230937142913,0.616145700617437,31.8532190524109));
#55393=CARTESIAN_POINT('Ctrl Pts',(33.2266073362348,0.552653794777477,31.8670575477688));
#55394=CARTESIAN_POINT('Ctrl Pts',(32.9962341873238,0.355512844977353,31.8808960431267));
#55395=CARTESIAN_POINT('Ctrl Pts',(32.8876866584407,0.0723992741664823,
31.8947345384846));
#55396=CARTESIAN_POINT('Ctrl Pts',(32.9272140965448,-0.228222821374253,
31.9085730338424));
#55397=CARTESIAN_POINT('Ctrl Pts',(33.1052579144445,-0.473653852008448,
31.9224115292003));
#55398=CARTESIAN_POINT('Ctrl Pts',(33.3787618105113,-0.60454165813537,31.9362500245582));
#55399=CARTESIAN_POINT('Ctrl Pts',(33.6815846457676,-0.589233672330023,
31.9500885199161));
#55400=CARTESIAN_POINT('Ctrl Pts',(33.9404950216258,-0.431431852806154,
31.963927015274));
#55401=CARTESIAN_POINT('Ctrl Pts',(34.0928808885737,-0.169297252584404,
31.9777655106319));
#55402=CARTESIAN_POINT('Ctrl Pts',(34.101890904803,0.13377834652035,31.9916040059898));
#55403=CARTESIAN_POINT('Ctrl Pts',(33.9653461887975,0.404502450342735,32.0054425013477));
#55404=CARTESIAN_POINT('Ctrl Pts',(33.7162672245694,0.577406092004606,32.0192809967056));
#55405=CARTESIAN_POINT('Ctrl Pts',(33.4148885532318,0.61067614104659,32.0331194920635));
#55406=CARTESIAN_POINT('Ctrl Pts',(33.1340923059939,0.496266931243954,32.0469579874214));
#55407=CARTESIAN_POINT('Ctrl Pts',(32.941783185408,0.261845938464038,32.0607964827792));
#55408=CARTESIAN_POINT('Ctrl Pts',(32.8844671320821,-0.0358970207556132,
32.0746349781371));
#55409=CARTESIAN_POINT('Ctrl Pts',(32.9760048353628,-0.324959035909932,
32.088473473495));
#55410=CARTESIAN_POINT('Ctrl Pts',(33.1942598152662,-0.535436501392846,
32.1023119688529));
#55411=CARTESIAN_POINT('Ctrl Pts',(33.4864516674538,-0.616429842130552,
32.1161504642108));
#55412=CARTESIAN_POINT('Ctrl Pts',(33.7819199006438,-0.548352511807186,
32.1299889595687));
#55413=CARTESIAN_POINT('Ctrl Pts',(34.0092116993034,-0.34766758962647,32.1438274549266));
#55414=CARTESIAN_POINT('Ctrl Pts',(34.1133612933847,-0.06290652876809,32.1576659502845));
#55415=CARTESIAN_POINT('Ctrl Pts',(34.0691822807711,0.237067161033253,32.1715044456424));
#55416=CARTESIAN_POINT('Ctrl Pts',(33.887358432116,0.479711113747428,32.1853429410003));
#55417=CARTESIAN_POINT('Ctrl Pts',(33.6118600442505,0.606346961800283,32.1991814363582));
#55418=CARTESIAN_POINT('Ctrl Pts',(33.3093106430795,0.586350472619748,32.2130199317161));
#55419=CARTESIAN_POINT('Ctrl Pts',(33.0528754765832,0.424557379094313,32.2268584270739));
#55420=CARTESIAN_POINT('Ctrl Pts',(32.9045680290884,0.160093958663236,32.2406969224319));
#55421=CARTESIAN_POINT('Ctrl Pts',(32.9002533564547,-0.143084838960522,
32.2545354177897));
#55422=CARTESIAN_POINT('Ctrl Pts',(33.0409748720619,-0.41166155942181,32.2683739131476));
#55423=CARTESIAN_POINT('Ctrl Pts',(33.292702019096,-0.580686537382506,32.2822124085055));
#55424=CARTESIAN_POINT('Ctrl Pts',(33.5945598493176,-0.609284615332775,
32.2960509038634));
#55425=CARTESIAN_POINT('Ctrl Pts',(33.8735503567233,-0.490539945953485,
32.3098893992213));
#55426=CARTESIAN_POINT('Ctrl Pts',(34.0622055192993,-0.253168445216891,
32.3237278945792));
#55427=CARTESIAN_POINT('Ctrl Pts',(34.1149030297489,0.0454265515947455,
32.3375663899371));
#55428=CARTESIAN_POINT('Ctrl Pts',(34.0188990967934,0.333036086529878,32.351404885295));
#55429=CARTESIAN_POINT('Ctrl Pts',(33.7974102646885,0.540107805944433,32.3652433806529));
#55430=CARTESIAN_POINT('Ctrl Pts',(33.5039989773295,0.616565743262212,32.3790818760108));
#55431=CARTESIAN_POINT('Ctrl Pts',(33.2096206209007,0.543920144670213,32.3929203713687));
#55432=CARTESIAN_POINT('Ctrl Pts',(32.9854644470244,0.339738829556257,32.4067588667266));
#55433=CARTESIAN_POINT('Ctrl Pts',(32.8857379404437,0.0533987806393666,
32.4205973620844));
#55434=CARTESIAN_POINT('Ctrl Pts',(32.9345578720262,-0.245854647091717,
32.4344358574423));
#55435=CARTESIAN_POINT('Ctrl Pts',(33.1201181618828,-0.485653267931855,
32.4482743528002));
#55436=CARTESIAN_POINT('Ctrl Pts',(33.3975449329869,-0.608006798339873,
32.4621128481581));
#55437=CARTESIAN_POINT('Ctrl Pts',(33.6997483202596,-0.583326594745735,
32.475951343516));
#55438=CARTESIAN_POINT('Ctrl Pts',(33.9536467519485,-0.417581048457376,
32.4897898388739));
#55439=CARTESIAN_POINT('Ctrl Pts',(34.0978402000105,-0.150852254990088,
32.5036283342318));
#55440=CARTESIAN_POINT('Ctrl Pts',(34.097458493347,0.152357002831217,32.5174668295897));
#55441=CARTESIAN_POINT('Ctrl Pts',(33.9525939397351,0.41872190448937,32.5313053249476));
#55442=CARTESIAN_POINT('Ctrl Pts',(33.6982790031214,0.583827666786467,32.5451438203055));
#55443=CARTESIAN_POINT('Ctrl Pts',(33.3960144345583,0.607746912591037,32.5589823156634));
#55444=CARTESIAN_POINT('Ctrl Pts',(33.1188966012142,0.48469527232898,32.5728208110212));
#55445=CARTESIAN_POINT('Ctrl Pts',(32.9339406580288,0.244430212844782,32.5866593063791));
#55446=CARTESIAN_POINT('Ctrl Pts',(32.8858743334203,-0.0549451838850536,
32.600497801737));
#55447=CARTESIAN_POINT('Ctrl Pts',(32.9863214631848,-0.34103323650276,32.6143362970949));
#55448=CARTESIAN_POINT('Ctrl Pts',(33.2109910088021,-0.544649530056662,
32.6281747924528));
#55449=CARTESIAN_POINT('Ctrl Pts',(33.5055513373055,-0.616553720480452,
32.6420132878107));
#55450=CARTESIAN_POINT('Ctrl Pts',(33.7987691909304,-0.539357282452898,
32.6558517831686));
#55451=CARTESIAN_POINT('Ctrl Pts',(34.0197359613976,-0.331728560745555,
32.6696902785265));
#55452=CARTESIAN_POINT('Ctrl Pts',(34.1150154545051,-0.0438782212951887,
32.6835287738844));
#55453=CARTESIAN_POINT('Ctrl Pts',(34.0615663166305,0.254583148716051,32.6973672692422));
#55454=CARTESIAN_POINT('Ctrl Pts',(33.8723141044326,0.491478906184875,32.7112057646002));
#55455=CARTESIAN_POINT('Ctrl Pts',(33.5930255091781,0.609520764393083,32.7250442599581));
#55456=CARTESIAN_POINT('Ctrl Pts',(33.2912406391955,0.58016276755811,32.7388827553159));
#55457=CARTESIAN_POINT('Ctrl Pts',(33.0399398565798,0.41050453349551,32.7527212506738));
#55458=CARTESIAN_POINT('Ctrl Pts',(32.8998950022487,0.141574359465359,32.7665597460317));
#55459=CARTESIAN_POINT('Ctrl Pts',(32.9049729966318,-0.161592613837421,
32.7803982413896));
#55460=CARTESIAN_POINT('Ctrl Pts',(33.0539458329414,-0.425681791522521,
32.7942367367475));
#55461=CARTESIAN_POINT('Ctrl Pts',(33.3107875449427,-0.586828726661681,
32.8080752321054));
#55462=CARTESIAN_POINT('Ctrl Pts',(33.6133863337773,-0.606063401713632,
32.8219137274633));
#55463=CARTESIAN_POINT('Ctrl Pts',(33.8885650080908,-0.478734312611433,
32.8357522228212));
#55464=CARTESIAN_POINT('Ctrl Pts',(34.0697773580175,-0.235633337782937,
32.8495907181791));
#55465=CARTESIAN_POINT('Ctrl Pts',(34.1132009649105,0.0644506339531861,
32.863429213537));
#55466=CARTESIAN_POINT('Ctrl Pts',(34.0083347371985,0.34894856718642,32.8772677088949));
#55467=CARTESIAN_POINT('Ctrl Pts',(33.7805383798607,0.549060584097315,32.8911062042528));
#55468=CARTESIAN_POINT('Ctrl Pts',(33.4848996799135,0.616393776669955,32.9049446996106));
#55469=CARTESIAN_POINT('Ctrl Pts',(33.1929126767121,0.534665019858251,32.9187831949685));
#55470=CARTESIAN_POINT('Ctrl Pts',(32.9751883230913,0.323638704985112,32.9326216903264));
#55471=CARTESIAN_POINT('Ctrl Pts',(32.8843787025204,0.0343471348689163,
32.9464601856843));
#55472=CARTESIAN_POINT('Ctrl Pts',(32.9424442233901,-0.263250571800097,
32.9602986810422));
#55473=CARTESIAN_POINT('Ctrl Pts',(33.1353429533181,-0.497186630843364,
32.9741371764001));
#55474=CARTESIAN_POINT('Ctrl Pts',(33.4164263669539,-0.610888496735408,
32.987975671758));
#55475=CARTESIAN_POINT('Ctrl Pts',(33.7177203166635,-0.576859750109264,
33.0018141671159));
#55476=CARTESIAN_POINT('Ctrl Pts',(33.9663631591575,-0.403329531977034,
33.0156526624738));
#55477=CARTESIAN_POINT('Ctrl Pts',(34.1022258207733,-0.132262498003517,
33.0294911578317));
#55478=CARTESIAN_POINT('Ctrl Pts',(34.092452756962,0.170789456209393,33.0433296531896));
#55479=CARTESIAN_POINT('Ctrl Pts',(33.9394073789038,0.432539550733842,33.0571681485475));
#55480=CARTESIAN_POINT('Ctrl Pts',(33.6801005119203,0.589688997006223,33.0710066439053));
#55481=CARTESIAN_POINT('Ctrl Pts',(33.3772401010691,0.604234486601558,33.0848451392632));
#55482=CARTESIAN_POINT('Ctrl Pts',(33.1040666055202,0.472658496929737,33.0986836346211));
#55483=CARTESIAN_POINT('Ctrl Pts',(32.9266413245726,0.226779930541385,33.112522129979));
#55484=CARTESIAN_POINT('Ctrl Pts',(32.8878708534081,-0.0739406212907469,
33.1263606253369));
#55485=CARTESIAN_POINT('Ctrl Pts',(32.9971310199942,-0.356780179567283,
33.1401991206948));
#55486=CARTESIAN_POINT('Ctrl Pts',(33.2279995370889,-0.553339909784574,
33.1540376160527));
#55487=CARTESIAN_POINT('Ctrl Pts',(33.5246456800608,-0.616085950203557,
33.1678761114106));
#55488=CARTESIAN_POINT('Ctrl Pts',(33.8153317805203,-0.529844482635056,
33.1817146067685));
#55489=CARTESIAN_POINT('Ctrl Pts',(34.0297614817636,-0.315471203158683,
33.1955531021264));
#55490=CARTESIAN_POINT('Ctrl Pts',(34.1160794431301,-0.024807808021806,
33.2093915974843));
#55491=CARTESIAN_POINT('Ctrl Pts',(34.0534114701008,0.271854836896847,33.2232300928422));
#55492=CARTESIAN_POINT('Ctrl Pts',(33.856912501923,0.502775072522705,33.2370685882001));
#55493=CARTESIAN_POINT('Ctrl Pts',(33.5741017062561,0.612109667252904,33.2509070835579));
#55494=CARTESIAN_POINT('Ctrl Pts',(33.2733709620794,0.573418334794239,33.2647455789158));
#55495=CARTESIAN_POINT('Ctrl Pts',(33.0274457129566,0.396057765431385,33.2785840742737));
#55496=CARTESIAN_POINT('Ctrl Pts',(32.8957978399437,0.12291890442723,33.2924225696316));
#55497=CARTESIAN_POINT('Ctrl Pts',(32.9102636279106,-0.179945322816027,
33.3062610649895));
#55498=CARTESIAN_POINT('Ctrl Pts',(33.067344831065,-0.439293537952395,33.3200995603474));
#55499=CARTESIAN_POINT('Ctrl Pts',(33.3290546385379,-0.592407788251204,
33.3339380557053));
#55500=CARTESIAN_POINT('Ctrl Pts',(33.6321040171286,-0.602260611089616,
33.3477765510632));
#55501=CARTESIAN_POINT('Ctrl Pts',(33.9032067827305,-0.46646926585926,33.3616150464211));
#55502=CARTESIAN_POINT('Ctrl Pts',(34.0768024611429,-0.217872137301847,
33.375453541779));
#55503=CARTESIAN_POINT('Ctrl Pts',(34.1109104366237,0.0834129580795525,
33.3892920371369));
#55504=CARTESIAN_POINT('Ctrl Pts',(33.9972827132432,0.364526103420134,33.4031305324948));
#55505=CARTESIAN_POINT('Ctrl Pts',(33.7633971588482,0.557486952487014,33.4169690278527));
#55506=CARTESIAN_POINT('Ctrl Pts',(33.4658156020346,0.615629978936103,33.4308075232105));
#55507=CARTESIAN_POINT('Ctrl Pts',(33.1764989599376,0.524899389713111,33.4446460185684));
#55508=CARTESIAN_POINT('Ctrl Pts',(32.9654197947462,0.307227101356573,33.4584845139263));
#55509=CARTESIAN_POINT('Ctrl Pts',(32.883609179451,0.0152768043877929,33.4723230092842));
#55510=CARTESIAN_POINT('Ctrl Pts',(32.9508879686469,-0.280393705028702,
33.4861615046421));
#55511=CARTESIAN_POINT('Ctrl Pts',(33.0842424455853,-0.432235449302045,
33.495387168214));
#55512=CARTESIAN_POINT('Ctrl Pts',(33.1650171622239,-0.487714879843202,
33.5));
#55513=CARTESIAN_POINT('Ctrl Pts',(33.8243757602969,-0.454512507566744,
31.8032427170809));
#55514=CARTESIAN_POINT('Ctrl Pts',(33.8996515423669,-0.400789807675315,
31.8078555488669));
#55515=CARTESIAN_POINT('Ctrl Pts',(34.0229037731069,-0.25524667846797,31.8170812124388));
#55516=CARTESIAN_POINT('Ctrl Pts',(34.0813632413627,0.0248896063187892,
31.8309197077967));
#55517=CARTESIAN_POINT('Ctrl Pts',(33.999206020912,0.298982002098727,31.8447582031546));
#55518=CARTESIAN_POINT('Ctrl Pts',(33.7963339648404,0.50078939824982,31.8585966985125));
#55519=CARTESIAN_POINT('Ctrl Pts',(33.5217946298435,0.581485823597872,31.8724351938704));
#55520=CARTESIAN_POINT('Ctrl Pts',(33.241986419615,0.521565510720332,31.8862736892283));
#55521=CARTESIAN_POINT('Ctrl Pts',(33.0245723889805,0.33551427731155,31.9001121845862));
#55522=CARTESIAN_POINT('Ctrl Pts',(32.9221309548054,0.0683266174289568,
31.9139506799441));
#55523=CARTESIAN_POINT('Ctrl Pts',(32.9594348666523,-0.215384664889574,
31.927789175302));
#55524=CARTESIAN_POINT('Ctrl Pts',(33.1274632339429,-0.447009530309856,
31.9416276706599));
#55525=CARTESIAN_POINT('Ctrl Pts',(33.3855817895091,-0.570534540170937,
31.9554661660177));
#55526=CARTESIAN_POINT('Ctrl Pts',(33.6713700139287,-0.556087670340104,
31.9693046613756));
#55527=CARTESIAN_POINT('Ctrl Pts',(33.9157159746212,-0.40716263377955,31.9831431567335));
#55528=CARTESIAN_POINT('Ctrl Pts',(34.0595297207174,-0.159773820142295,
31.9969816520914));
#55529=CARTESIAN_POINT('Ctrl Pts',(34.0680328989469,0.126252949469573,32.0108201474493));
#55530=CARTESIAN_POINT('Ctrl Pts',(33.9391691958248,0.381748083690591,32.0246586428072));
#55531=CARTESIAN_POINT('Ctrl Pts',(33.7041016030299,0.544925423683506,32.0384971381651));
#55532=CARTESIAN_POINT('Ctrl Pts',(33.4196763043676,0.57632394167841,32.052335633523));
#55533=CARTESIAN_POINT('Ctrl Pts',(33.1546756122834,0.468350562131005,32.0661741288809));
#55534=CARTESIAN_POINT('Ctrl Pts',(32.9731844045103,0.247116389891124,32.0800126242388));
#55535=CARTESIAN_POINT('Ctrl Pts',(32.91909253559,-0.0338777153810717,32.0938511195967));
#55536=CARTESIAN_POINT('Ctrl Pts',(33.0054809932699,-0.306679203380471,
32.1076896149546));
#55537=CARTESIAN_POINT('Ctrl Pts',(33.2114585349719,-0.505316737071738,
32.1215281103124));
#55538=CARTESIAN_POINT('Ctrl Pts',(33.4872137981307,-0.581753981375499,
32.1353666056703));
#55539=CARTESIAN_POINT('Ctrl Pts',(33.7660611369197,-0.517506186654611,
32.1492051010282));
#55540=CARTESIAN_POINT('Ctrl Pts',(33.980567151663,-0.32811033898256,32.1630435963861));
#55541=CARTESIAN_POINT('Ctrl Pts',(34.0788580468701,-0.0593678648633583,
32.176882091744));
#55542=CARTESIAN_POINT('Ctrl Pts',(34.0371642242733,0.223731486308013,32.1907205871019));
#55543=CARTESIAN_POINT('Ctrl Pts',(33.8655684632723,0.452726054546752,32.2045590824598));
#55544=CARTESIAN_POINT('Ctrl Pts',(33.6055676115139,0.572238290578322,32.2183975778177));
#55545=CARTESIAN_POINT('Ctrl Pts',(33.320037439766,0.553366658481309,32.2322360731756));
#55546=CARTESIAN_POINT('Ctrl Pts',(33.0780274511543,0.400674867973303,32.2460745685335));
#55547=CARTESIAN_POINT('Ctrl Pts',(32.9380627022876,0.151088236618461,32.2599130638914));
#55548=CARTESIAN_POINT('Ctrl Pts',(32.9339907417637,-0.135035926314105,
32.2737515592493));
#55549=CARTESIAN_POINT('Ctrl Pts',(33.0667962881122,-0.388504473347942,
32.2875900546072));
#55550=CARTESIAN_POINT('Ctrl Pts',(33.3043630962038,-0.548021335057105,
32.3014285499651));
#55551=CARTESIAN_POINT('Ctrl Pts',(33.5892405997552,-0.57501069308324,32.3152670453229));
#55552=CARTESIAN_POINT('Ctrl Pts',(33.8525371298004,-0.462945735391122,
32.3291055406808));
#55553=CARTESIAN_POINT('Ctrl Pts',(34.0305799246728,-0.238927029318574,
32.3429440360387));
#55554=CARTESIAN_POINT('Ctrl Pts',(34.0803130563567,0.0428711841059874,
32.3567825313966));
#55555=CARTESIAN_POINT('Ctrl Pts',(33.9897096066089,0.314301897862109,32.3706210267545));
#55556=CARTESIAN_POINT('Ctrl Pts',(33.7806801257163,0.509725267995079,32.3844595221124));
#55557=CARTESIAN_POINT('Ctrl Pts',(33.5037740239422,0.581882237697651,32.3982980174703));
#55558=CARTESIAN_POINT('Ctrl Pts',(33.2259552533724,0.51332315226429,32.4121365128282));
#55559=CARTESIAN_POINT('Ctrl Pts',(33.0144084759618,0.320627593302573,32.4259750081861));
#55560=CARTESIAN_POINT('Ctrl Pts',(32.9202918575134,0.0503949535119496,
32.439813503544));
#55561=CARTESIAN_POINT('Ctrl Pts',(32.9663655347229,-0.23202465229609,32.4536519989019));
#55562=CARTESIAN_POINT('Ctrl Pts',(33.1414875519117,-0.458333946343147,
32.4674904942597));
#55563=CARTESIAN_POINT('Ctrl Pts',(33.4033083100893,-0.573804756783141,
32.4813289896176));
#55564=CARTESIAN_POINT('Ctrl Pts',(33.6885119321648,-0.550512881989371,
32.4951674849755));
#55565=CARTESIAN_POINT('Ctrl Pts',(33.9281278842243,-0.394090974971947,
32.5090059803334));
#55566=CARTESIAN_POINT('Ctrl Pts',(34.0642100573527,-0.142366403996009,
32.5228444756913));
#55567=CARTESIAN_POINT('Ctrl Pts',(34.0638498227307,0.14378650566487,32.5366829710492));
#55568=CARTESIAN_POINT('Ctrl Pts',(33.9271342955709,0.395167654738936,32.5505214664071));
#55569=CARTESIAN_POINT('Ctrl Pts',(33.6871252681252,0.55098576736047,32.564359961765));
#55570=CARTESIAN_POINT('Ctrl Pts',(33.4018639063738,0.573559490316862,32.5781984571229));
#55571=CARTESIAN_POINT('Ctrl Pts',(33.1403347073641,0.457429840607144,32.5920369524808));
#55572=CARTESIAN_POINT('Ctrl Pts',(32.9657830406972,0.230680346362589,32.6058754478387));
#55573=CARTESIAN_POINT('Ctrl Pts',(32.9204205780129,-0.0518543673551904,
32.6197139431966));
#55574=CARTESIAN_POINT('Ctrl Pts',(33.0152172826245,-0.321849186326115,
32.6335524385544));
#55575=CARTESIAN_POINT('Ctrl Pts',(33.2272485532148,-0.51401150773238,32.6473909339124));
#55576=CARTESIAN_POINT('Ctrl Pts',(33.5052390594334,-0.581870891230174,
32.6612294292702));
#55577=CARTESIAN_POINT('Ctrl Pts',(33.7819626086488,-0.509016963497996,
32.6750679246281));
#55578=CARTESIAN_POINT('Ctrl Pts',(33.9904993952954,-0.313067923971173,
32.688906419986));
#55579=CARTESIAN_POINT('Ctrl Pts',(34.0804191569136,-0.0414099516109154,
32.7027449153439));
#55580=CARTESIAN_POINT('Ctrl Pts',(34.0299766788984,0.240262151885417,32.7165834107018));
#55581=CARTESIAN_POINT('Ctrl Pts',(33.8513704200746,0.463831876547231,32.7304219060597));
#55582=CARTESIAN_POINT('Ctrl Pts',(33.5877925704356,0.575233558114495,32.7442604014176));
#55583=CARTESIAN_POINT('Ctrl Pts',(33.3029839229106,0.547527028714612,32.7580988967755));
#55584=CARTESIAN_POINT('Ctrl Pts',(33.0658194950753,0.387412533287327,32.7719373921334));
#55585=CARTESIAN_POINT('Ctrl Pts',(32.9336525459596,0.133610415412391,32.7857758874913));
#55586=CARTESIAN_POINT('Ctrl Pts',(32.9384448893016,-0.152502588349518,
32.7996143828492));
#55587=CARTESIAN_POINT('Ctrl Pts',(33.0790375970466,-0.401736029134091,
32.813452878207));
#55588=CARTESIAN_POINT('Ctrl Pts',(33.3214312618693,-0.553818009428307,
32.8272913735649));
#55589=CARTESIAN_POINT('Ctrl Pts',(33.6070080430898,-0.571970681520334,
32.8411298689228));
#55590=CARTESIAN_POINT('Ctrl Pts',(33.866707166056,-0.451804201140183,32.8549683642807));
#55591=CARTESIAN_POINT('Ctrl Pts',(34.0377258268008,-0.222378319528192,
32.8688068596386));
#55592=CARTESIAN_POINT('Ctrl Pts',(34.0787067373102,0.0608251099181874,
32.8826453549965));
#55593=CARTESIAN_POINT('Ctrl Pts',(33.9797395210696,0.329319258059189,32.8964838503544));
#55594=CARTESIAN_POINT('Ctrl Pts',(33.7647573304507,0.518174427946209,32.9103223457123));
#55595=CARTESIAN_POINT('Ctrl Pts',(33.4857491141246,0.581719944695477,32.9241608410702));
#55596=CARTESIAN_POINT('Ctrl Pts',(33.2101871766376,0.504588653478707,32.9379993364281));
#55597=CARTESIAN_POINT('Ctrl Pts',(33.0047104120418,0.305433144673135,32.951837831786));
#55598=CARTESIAN_POINT('Ctrl Pts',(32.9190090804324,0.0324150148048813,
32.9656763271438));
#55599=CARTESIAN_POINT('Ctrl Pts',(32.973808257302,-0.248442008769019,32.9795148225017));
#55600=CARTESIAN_POINT('Ctrl Pts',(33.1558559072828,-0.469218526118242,
32.9933533178596));
#55601=CARTESIAN_POINT('Ctrl Pts',(33.4211276118714,-0.576524351780248,
33.0071918132175));
#55602=CARTESIAN_POINT('Ctrl Pts',(33.7054729547284,-0.544409815010653,
33.0210303085754));
#55603=CARTESIAN_POINT('Ctrl Pts',(33.9401289588269,-0.380641145183659,
33.0348688039333));
#55604=CARTESIAN_POINT('Ctrl Pts',(34.06834897498,-0.124822371568309,33.0487072992912));
#55605=CARTESIAN_POINT('Ctrl Pts',(34.0591256726772,0.161182083241403,33.0625457946491));
#55606=CARTESIAN_POINT('Ctrl Pts',(33.9146895147703,0.408208020676082,33.076384290007));
#55607=CARTESIAN_POINT('Ctrl Pts',(33.6699693666602,0.556517381760763,33.0902227853649));
#55608=CARTESIAN_POINT('Ctrl Pts',(33.3841456803755,0.570244647874121,33.1040612807228));
#55609=CARTESIAN_POINT('Ctrl Pts',(33.1263389393965,0.44607016667048,33.1178997760807));
#55610=CARTESIAN_POINT('Ctrl Pts',(32.9588943146665,0.214022940603463,33.1317382714385));
#55611=CARTESIAN_POINT('Ctrl Pts',(32.9223047883032,-0.0697812595714029,
33.1455767667964));
#55612=CARTESIAN_POINT('Ctrl Pts',(33.0254187723659,-0.336710320872452,
33.1594152621543));
#55613=CARTESIAN_POINT('Ctrl Pts',(33.243300305372,-0.522213029885987,33.1732537575122));
#55614=CARTESIAN_POINT('Ctrl Pts',(33.5232592933034,-0.581429434307822,
33.1870922528701));
#55615=CARTESIAN_POINT('Ctrl Pts',(33.7975935073776,-0.500039284628767,
33.200930748228));
#55616=CARTESIAN_POINT('Ctrl Pts',(33.9999609527828,-0.297725087112206,
33.2147692435859));
#55617=CARTESIAN_POINT('Ctrl Pts',(34.081423293275,-0.0234123011241682,
33.2286077389438));
#55618=CARTESIAN_POINT('Ctrl Pts',(34.0222805647392,0.256562260474459,33.2424462343017));
#55619=CARTESIAN_POINT('Ctrl Pts',(33.8368351997345,0.474492602703185,33.2562847296596));
#55620=CARTESIAN_POINT('Ctrl Pts',(33.5699332830679,0.577676828123762,33.2701232250175));
#55621=CARTESIAN_POINT('Ctrl Pts',(33.2861194638957,0.541161988698152,33.2839617203754));
#55622=CARTESIAN_POINT('Ctrl Pts',(33.0540281811253,0.373778435349653,33.2978002157333));
#55623=CARTESIAN_POINT('Ctrl Pts',(32.9297858602148,0.116004380627812,33.3116387110911));
#55624=CARTESIAN_POINT('Ctrl Pts',(32.9434379081338,-0.169822907366567,
33.325477206449));
#55625=CARTESIAN_POINT('Ctrl Pts',(33.0916828649621,-0.414582077683077,
33.3393157018069));
#55626=CARTESIAN_POINT('Ctrl Pts',(33.3386707816018,-0.559083233579081,
33.3531541971648));
#55627=CARTESIAN_POINT('Ctrl Pts',(33.6246728056751,-0.568381808246107,
33.3669926925227));
#55628=CARTESIAN_POINT('Ctrl Pts',(33.8805253009172,-0.440229096737107,
33.3808311878806));
#55629=CARTESIAN_POINT('Ctrl Pts',(34.044355748705,-0.205616235041545,33.3946696832385));
#55630=CARTESIAN_POINT('Ctrl Pts',(34.07654505749,0.0787207515673956,33.4085081785964));
#55631=CARTESIAN_POINT('Ctrl Pts',(33.9693092036209,0.344020515371233,33.4223466739543));
#55632=CARTESIAN_POINT('Ctrl Pts',(33.7485803498957,0.52612679011982,33.4361851693122));
#55633=CARTESIAN_POINT('Ctrl Pts',(33.4677385677038,0.580999112668433,33.4500236646701));
#55634=CARTESIAN_POINT('Ctrl Pts',(33.194696776222,0.495372366678023,33.463862160028));
#55635=CARTESIAN_POINT('Ctrl Pts',(32.9954913900728,0.289944738533257,33.4777006553859));
#55636=CARTESIAN_POINT('Ctrl Pts',(32.9182828451356,0.0144174424531027,
33.4915391507437));
#55637=CARTESIAN_POINT('Ctrl Pts',(32.9817770188465,-0.264620793972737,
33.5053776461016));
#55638=CARTESIAN_POINT('Ctrl Pts',(33.1076299425548,-0.407921025779667,
33.5146033096736));
#55639=CARTESIAN_POINT('Ctrl Pts',(33.1838608609616,-0.460279586958683,
33.5192161414595));
#55640=CARTESIAN_POINT('Ctrl Pts',(33.8050411118777,-0.427420965560361,
31.8224588585405));
#55641=CARTESIAN_POINT('Ctrl Pts',(33.8758300272981,-0.376900445491433,
31.8270716903264));
#55642=CARTESIAN_POINT('Ctrl Pts',(33.9917357209662,-0.240032518248871,
31.8362973538984));
#55643=CARTESIAN_POINT('Ctrl Pts',(34.0467106709446,0.0234060435919519,
31.8501358492563));
#55644=CARTESIAN_POINT('Ctrl Pts',(33.9694504901836,0.281160966738507,31.8639743446141));
#55645=CARTESIAN_POINT('Ctrl Pts',(33.7786707676286,0.470939489186442,31.877812839972));
#55646=CARTESIAN_POINT('Ctrl Pts',(33.5204955453957,0.546825946578308,31.8916513353299));
#55647=CARTESIAN_POINT('Ctrl Pts',(33.2573655029952,0.490477226663187,31.9054898306878));
#55648=CARTESIAN_POINT('Ctrl Pts',(33.0529105906372,0.315515709645747,31.9193283260457));
#55649=CARTESIAN_POINT('Ctrl Pts',(32.9565752511701,0.0642539606914318,
31.9331668214036));
#55650=CARTESIAN_POINT('Ctrl Pts',(32.9916556367597,-0.202546508404894,
31.9470053167615));
#55651=CARTESIAN_POINT('Ctrl Pts',(33.1496685534414,-0.420365208611264,
31.9608438121194));
#55652=CARTESIAN_POINT('Ctrl Pts',(33.3924017685068,-0.536527422206504,
31.9746823074773));
#55653=CARTESIAN_POINT('Ctrl Pts',(33.6611553820898,-0.522941668350186,
31.9885208028352));
#55654=CARTESIAN_POINT('Ctrl Pts',(33.8909369276166,-0.382893414752947,
32.0023592981931));
#55655=CARTESIAN_POINT('Ctrl Pts',(34.0261785528611,-0.150250387700185,
32.0161977935509));
#55656=CARTESIAN_POINT('Ctrl Pts',(34.0341748930909,0.118727552418796,32.0300362889088));
#55657=CARTESIAN_POINT('Ctrl Pts',(33.912992202852,0.358993717038448,32.0438747842667));
#55658=CARTESIAN_POINT('Ctrl Pts',(33.6919359814903,0.512444755362406,32.0577132796246));
#55659=CARTESIAN_POINT('Ctrl Pts',(33.4244640555034,0.541971742310229,32.0715517749825));
#55660=CARTESIAN_POINT('Ctrl Pts',(33.1752589185729,0.440434193018056,32.0853902703404));
#55661=CARTESIAN_POINT('Ctrl Pts',(33.0045856236125,0.232386841318209,32.0992287656983));
#55662=CARTESIAN_POINT('Ctrl Pts',(32.9537179390979,-0.03185841000653,32.1130672610562));
#55663=CARTESIAN_POINT('Ctrl Pts',(33.0349571511769,-0.288399370851011,
32.1269057564141));
#55664=CARTESIAN_POINT('Ctrl Pts',(33.2286572546776,-0.475196972750629,
32.140744251772));
#55665=CARTESIAN_POINT('Ctrl Pts',(33.4879759288076,-0.547078120620447,
32.1545827471299));
#55666=CARTESIAN_POINT('Ctrl Pts',(33.7502023731957,-0.486659861502035,
32.1684212424878));
#55667=CARTESIAN_POINT('Ctrl Pts',(33.9519226040226,-0.308553088338651,
32.1822597378456));
#55668=CARTESIAN_POINT('Ctrl Pts',(34.0443548003556,-0.0558292009586265,
32.1960982332036));
#55669=CARTESIAN_POINT('Ctrl Pts',(34.0051461677755,0.210395811582773,32.2099367285614));
#55670=CARTESIAN_POINT('Ctrl Pts',(33.8437784944286,0.425740995346075,32.2237752239193));
#55671=CARTESIAN_POINT('Ctrl Pts',(33.5992751787772,0.538129619356363,32.2376137192772));
#55672=CARTESIAN_POINT('Ctrl Pts',(33.3307642364525,0.520382844342869,32.2514522146351));
#55673=CARTESIAN_POINT('Ctrl Pts',(33.1031794257255,0.376792356852294,32.265290709993));
#55674=CARTESIAN_POINT('Ctrl Pts',(32.9715573754869,0.142082514573685,32.2791292053509));
#55675=CARTESIAN_POINT('Ctrl Pts',(32.9677281270726,-0.126987013667689,
32.2929677007088));
#55676=CARTESIAN_POINT('Ctrl Pts',(33.0926177041624,-0.365347387274075,
32.3068061960667));
#55677=CARTESIAN_POINT('Ctrl Pts',(33.3160241733116,-0.515356132731705,
32.3206446914246));
#55678=CARTESIAN_POINT('Ctrl Pts',(33.5839213501929,-0.540736770833706,
32.3344831867825));
#55679=CARTESIAN_POINT('Ctrl Pts',(33.8315239028775,-0.435351524828759,
32.3483216821404));
#55680=CARTESIAN_POINT('Ctrl Pts',(33.9989543300462,-0.224685613420258,
32.3621601774982));
#55681=CARTESIAN_POINT('Ctrl Pts',(34.0457230829646,0.0403158166172291,
32.3759986728561));
#55682=CARTESIAN_POINT('Ctrl Pts',(33.9605201164243,0.29556770919434,32.389837168214));
#55683=CARTESIAN_POINT('Ctrl Pts',(33.763949986744,0.479342730045725,32.4036756635719));
#55684=CARTESIAN_POINT('Ctrl Pts',(33.5035490705548,0.547198732133091,32.4175141589298));
#55685=CARTESIAN_POINT('Ctrl Pts',(33.2422898858441,0.482726159858367,32.4313526542877));
#55686=CARTESIAN_POINT('Ctrl Pts',(33.0433525048992,0.301516357048889,32.4451911496456));
#55687=CARTESIAN_POINT('Ctrl Pts',(32.9548457745831,0.0473911263845326,
32.4590296450035));
#55688=CARTESIAN_POINT('Ctrl Pts',(32.9981731974196,-0.218194657500464,
32.4728681403614));
#55689=CARTESIAN_POINT('Ctrl Pts',(33.1628569419406,-0.43101462475444,32.4867066357193));
#55690=CARTESIAN_POINT('Ctrl Pts',(33.4090716871918,-0.53960271522641,32.5005451310772));
#55691=CARTESIAN_POINT('Ctrl Pts',(33.67727554407,-0.517699169233008,32.5143836264351));
#55692=CARTESIAN_POINT('Ctrl Pts',(33.9026090165002,-0.370600901486519,
32.5282221217929));
#55693=CARTESIAN_POINT('Ctrl Pts',(34.030579914695,-0.133880553001932,32.5420606171509));
#55694=CARTESIAN_POINT('Ctrl Pts',(34.0302411521144,0.135216008498523,32.5558991125087));
#55695=CARTESIAN_POINT('Ctrl Pts',(33.9016746514067,0.371613404988503,32.5697376078666));
#55696=CARTESIAN_POINT('Ctrl Pts',(33.675971533129,0.518143867934474,32.5835761032245));
#55697=CARTESIAN_POINT('Ctrl Pts',(33.4077133781894,0.539372068042687,32.5974145985824));
#55698=CARTESIAN_POINT('Ctrl Pts',(33.161772813514,0.430164408885308,32.6112530939403));
#55699=CARTESIAN_POINT('Ctrl Pts',(32.9976254233655,0.216930479880396,32.6250915892982));
#55700=CARTESIAN_POINT('Ctrl Pts',(32.9549668226055,-0.0487635508253273,
32.6389300846561));
#55701=CARTESIAN_POINT('Ctrl Pts',(33.0441131020642,-0.30266513614947,32.652768580014));
#55702=CARTESIAN_POINT('Ctrl Pts',(33.2435060976275,-0.483373485408099,
32.6666070753719));
#55703=CARTESIAN_POINT('Ctrl Pts',(33.5049267815613,-0.547188061979896,
32.6804455707298));
#55704=CARTESIAN_POINT('Ctrl Pts',(33.7651560263672,-0.478676644543094,
32.6942840660876));
#55705=CARTESIAN_POINT('Ctrl Pts',(33.9612628291932,-0.294407287196792,
32.7081225614455));
#55706=CARTESIAN_POINT('Ctrl Pts',(34.0458228593221,-0.0389416819266422,
32.7219610568034));
#55707=CARTESIAN_POINT('Ctrl Pts',(33.9983870411662,0.225941155054783,32.7357995521613));
#55708=CARTESIAN_POINT('Ctrl Pts',(33.8304267357166,0.436184846909587,32.7496380475192));
#55709=CARTESIAN_POINT('Ctrl Pts',(33.582559631693,0.540946351835907,32.7634765428771));
#55710=CARTESIAN_POINT('Ctrl Pts',(33.3147272066257,0.514891289871114,32.777315038235));
#55711=CARTESIAN_POINT('Ctrl Pts',(33.0916991335709,0.364320533079145,32.7911535335929));
#55712=CARTESIAN_POINT('Ctrl Pts',(32.9674100896705,0.125646471359423,32.8049920289508));
#55713=CARTESIAN_POINT('Ctrl Pts',(32.9719167819715,-0.143412562861615,
32.8188305243087));
#55714=CARTESIAN_POINT('Ctrl Pts',(33.1041293611518,-0.377790266745661,
32.8326690196666));
#55715=CARTESIAN_POINT('Ctrl Pts',(33.3320749787957,-0.520807292194933,
32.8465075150245));
#55716=CARTESIAN_POINT('Ctrl Pts',(33.6006297524022,-0.537877961327036,
32.8603460103823));
#55717=CARTESIAN_POINT('Ctrl Pts',(33.8448493240212,-0.424874089668934,
32.8741845057402));
#55718=CARTESIAN_POINT('Ctrl Pts',(34.005674295584,-0.209123301273446,32.8880230010981));
#55719=CARTESIAN_POINT('Ctrl Pts',(34.0442125097098,0.0571995858831888,
32.901861496456));
#55720=CARTESIAN_POINT('Ctrl Pts',(33.9511443049407,0.309689948931958,32.9156999918139));
#55721=CARTESIAN_POINT('Ctrl Pts',(33.7489762810406,0.487288271795102,32.9295384871718));
#55722=CARTESIAN_POINT('Ctrl Pts',(33.4865985483358,0.547046112721,32.9433769825297));
#55723=CARTESIAN_POINT('Ctrl Pts',(33.2274616765631,0.474512287099164,32.9572154778876));
#55724=CARTESIAN_POINT('Ctrl Pts',(33.0342325009923,0.287227584361159,32.9710539732455));
#55725=CARTESIAN_POINT('Ctrl Pts',(32.9536394583445,0.0304828947408463,
32.9848924686034));
#55726=CARTESIAN_POINT('Ctrl Pts',(33.0051722912139,-0.233633445737942,
32.9987309639613));
#55727=CARTESIAN_POINT('Ctrl Pts',(33.1763688612475,-0.441250421393119,
33.0125694593192));
#55728=CARTESIAN_POINT('Ctrl Pts',(33.4258288567889,-0.542160206825089,
33.026407954677));
#55729=CARTESIAN_POINT('Ctrl Pts',(33.6932255927933,-0.511959879912042,
33.040246450035));
#55730=CARTESIAN_POINT('Ctrl Pts',(33.9138947584962,-0.357952758390285,
33.0540849453928));
#55731=CARTESIAN_POINT('Ctrl Pts',(34.0344721291867,-0.117382245133102,
33.0679234407507));
#55732=CARTESIAN_POINT('Ctrl Pts',(34.0257985883924,0.151574710273414,33.0817619361086));
#55733=CARTESIAN_POINT('Ctrl Pts',(33.8899716506368,0.383876490618324,33.0956004314665));
#55734=CARTESIAN_POINT('Ctrl Pts',(33.6598382214002,0.523345766515303,33.1094389268244));
#55735=CARTESIAN_POINT('Ctrl Pts',(33.3910512596818,0.536254809146684,33.1232774221823));
#55736=CARTESIAN_POINT('Ctrl Pts',(33.1486112732729,0.419481836411223,33.1371159175402));
#55737=CARTESIAN_POINT('Ctrl Pts',(32.9911473047604,0.201265950665541,33.1509544128981));
#55738=CARTESIAN_POINT('Ctrl Pts',(32.9567387231984,-0.0656218978520585,
33.164792908256));
#55739=CARTESIAN_POINT('Ctrl Pts',(33.0537065247376,-0.316640462177621,
33.1786314036139));
#55740=CARTESIAN_POINT('Ctrl Pts',(33.2586010736551,-0.491086149987399,
33.1924698989717));
#55741=CARTESIAN_POINT('Ctrl Pts',(33.521872906546,-0.546772918412087,33.2063083943297));
#55742=CARTESIAN_POINT('Ctrl Pts',(33.779855234235,-0.470234086622478,33.2201468896875));
#55743=CARTESIAN_POINT('Ctrl Pts',(33.970160423802,-0.279978971065729,33.2339853850454));
#55744=CARTESIAN_POINT('Ctrl Pts',(34.0467671434199,-0.02201679422653,33.2478238804033));
#55745=CARTESIAN_POINT('Ctrl Pts',(33.9911496593775,0.241269684052071,33.2616623757612));
#55746=CARTESIAN_POINT('Ctrl Pts',(33.8167578975461,0.446210132883666,33.2755008711191));
#55747=CARTESIAN_POINT('Ctrl Pts',(33.5657648598797,0.543243988994621,33.289339366477));
#55748=CARTESIAN_POINT('Ctrl Pts',(33.2988679657119,0.508905642602065,33.3031778618349));
#55749=CARTESIAN_POINT('Ctrl Pts',(33.0806106492941,0.35149910526792,33.3170163571928));
#55750=CARTESIAN_POINT('Ctrl Pts',(32.9637738804858,0.109089856828395,33.3308548525507));
#55751=CARTESIAN_POINT('Ctrl Pts',(32.9766121883569,-0.159700491917106,
33.3446933479086));
#55752=CARTESIAN_POINT('Ctrl Pts',(33.1160208988592,-0.389870617413759,
33.3585318432665));
#55753=CARTESIAN_POINT('Ctrl Pts',(33.3482869246657,-0.525758678906959,
33.3723703386243));
#55754=CARTESIAN_POINT('Ctrl Pts',(33.6172415942216,-0.534503005402597,
33.3862088339823));
#55755=CARTESIAN_POINT('Ctrl Pts',(33.8578438191039,-0.413988927614954,
33.4000473293401));
#55756=CARTESIAN_POINT('Ctrl Pts',(34.011909036267,-0.193360332781244,33.413885824698));
#55757=CARTESIAN_POINT('Ctrl Pts',(34.0421796783562,0.0740285450552389,
33.4277243200559));
#55758=CARTESIAN_POINT('Ctrl Pts',(33.9413356939986,0.323514927322333,33.4415628154138));
#55759=CARTESIAN_POINT('Ctrl Pts',(33.7337635409431,0.494766627752625,33.4554013107717));
#55760=CARTESIAN_POINT('Ctrl Pts',(33.4696615333729,0.546368246400762,33.4692398061296));
#55761=CARTESIAN_POINT('Ctrl Pts',(33.2128945925064,0.465845343642935,33.4830783014875));
#55762=CARTESIAN_POINT('Ctrl Pts',(33.0255629853994,0.272662375709941,33.4969167968454));
#55763=CARTESIAN_POINT('Ctrl Pts',(32.9529565108202,0.0135580805184124,
33.5107552922033));
#55764=CARTESIAN_POINT('Ctrl Pts',(33.0126660690462,-0.248847882916771,
33.5245937875612));
#55765=CARTESIAN_POINT('Ctrl Pts',(33.1310174395243,-0.383606602257289,
33.5338194511331));
#55766=CARTESIAN_POINT('Ctrl Pts',(33.2027045596994,-0.432844294074163,
33.5384322829191));
#55767=CARTESIAN_POINT('Ctrl Pts',(33.7857064634585,-0.400329423553979,
31.841675));
#55768=CARTESIAN_POINT('Ctrl Pts',(33.8520085122293,-0.353011083307552,
31.846287831786));
#55769=CARTESIAN_POINT('Ctrl Pts',(33.9605676688256,-0.224818358029771,
31.8555134953579));
#55770=CARTESIAN_POINT('Ctrl Pts',(34.0120581005265,0.0219224808651154,
31.8693519907158));
#55771=CARTESIAN_POINT('Ctrl Pts',(33.9396949594551,0.263339931378287,31.8831904860737));
#55772=CARTESIAN_POINT('Ctrl Pts',(33.7610075704167,0.441089580123063,31.8970289814316));
#55773=CARTESIAN_POINT('Ctrl Pts',(33.5191964609478,0.512166069558742,31.9108674767895));
#55774=CARTESIAN_POINT('Ctrl Pts',(33.2727445863754,0.459388942606042,31.9247059721473));
#55775=CARTESIAN_POINT('Ctrl Pts',(33.081248792294,0.295517141979944,31.9385444675052));
#55776=CARTESIAN_POINT('Ctrl Pts',(32.9910195475347,0.0601813039539063,
31.9523829628631));
#55777=CARTESIAN_POINT('Ctrl Pts',(33.0238764068672,-0.189708351920215,
31.966221458221));
#55778=CARTESIAN_POINT('Ctrl Pts',(33.1718738729398,-0.393720886912672,
31.9800599535789));
#55779=CARTESIAN_POINT('Ctrl Pts',(33.3992217475045,-0.502520304242071,
31.9938984489368));
#55780=CARTESIAN_POINT('Ctrl Pts',(33.6509407502508,-0.489795666360267,
32.0077369442947));
#55781=CARTESIAN_POINT('Ctrl Pts',(33.866157880612,-0.358624195726342,32.0215754396526));
#55782=CARTESIAN_POINT('Ctrl Pts',(33.9928273850048,-0.140726955258076,
32.0354139350105));
#55783=CARTESIAN_POINT('Ctrl Pts',(34.0003168872349,0.11120215536802,32.0492524303684));
#55784=CARTESIAN_POINT('Ctrl Pts',(33.8868152098793,0.336239350386304,32.0630909257263));
#55785=CARTESIAN_POINT('Ctrl Pts',(33.6797703599508,0.479964087041306,32.0769294210842));
#55786=CARTESIAN_POINT('Ctrl Pts',(33.4292518066392,0.507619542942049,32.090767916442));
#55787=CARTESIAN_POINT('Ctrl Pts',(33.1958422248624,0.412517823905107,32.1046064117999));
#55788=CARTESIAN_POINT('Ctrl Pts',(33.0359868427148,0.217657292745295,32.1184449071578));
#55789=CARTESIAN_POINT('Ctrl Pts',(32.9883433426058,-0.0298391046319884,
32.1322834025157));
#55790=CARTESIAN_POINT('Ctrl Pts',(33.064433309084,-0.27011953832155,32.1461218978736));
#55791=CARTESIAN_POINT('Ctrl Pts',(33.2458559743834,-0.44507720842952,32.1599603932315));
#55792=CARTESIAN_POINT('Ctrl Pts',(33.4887380594845,-0.512402259865394,
32.1737988885894));
#55793=CARTESIAN_POINT('Ctrl Pts',(33.7343436094716,-0.455813536349459,
32.1876373839473));
#55794=CARTESIAN_POINT('Ctrl Pts',(33.9232780563821,-0.288995837694741,
32.2014758793052));
#55795=CARTESIAN_POINT('Ctrl Pts',(34.0098515538411,-0.0522905370538949,
32.2153143746631));
#55796=CARTESIAN_POINT('Ctrl Pts',(33.9731281112777,0.197060136857534,32.229152870021));
#55797=CARTESIAN_POINT('Ctrl Pts',(33.8219885255849,0.398755936145399,32.2429913653789));
#55798=CARTESIAN_POINT('Ctrl Pts',(33.5929827460405,0.504020948134402,32.2568298607368));
#55799=CARTESIAN_POINT('Ctrl Pts',(33.3414910331391,0.487399030204428,32.2706683560946));
#55800=CARTESIAN_POINT('Ctrl Pts',(33.1283314002966,0.352909845731284,32.2845068514525));
#55801=CARTESIAN_POINT('Ctrl Pts',(33.0050520486862,0.13307679252891,32.2983453468104));
#55802=CARTESIAN_POINT('Ctrl Pts',(33.0014655123815,-0.118938101021272,
32.3121838421683));
#55803=CARTESIAN_POINT('Ctrl Pts',(33.1184391202127,-0.342190301200207,
32.3260223375262));
#55804=CARTESIAN_POINT('Ctrl Pts',(33.3276852504194,-0.482690930406304,
32.3398608328841));
#55805=CARTESIAN_POINT('Ctrl Pts',(33.5786021006306,-0.506462848584172,
32.353699328242));
#55806=CARTESIAN_POINT('Ctrl Pts',(33.8105106759546,-0.407757314266396,
32.3675378235999));
#55807=CARTESIAN_POINT('Ctrl Pts',(33.9673287354196,-0.210444197521941,
32.3813763189578));
#55808=CARTESIAN_POINT('Ctrl Pts',(34.0111331095724,0.0377604491284709,
32.3952148143157));
#55809=CARTESIAN_POINT('Ctrl Pts',(33.9313306262398,0.27683352052657,32.4090533096735));
#55810=CARTESIAN_POINT('Ctrl Pts',(33.7472198477718,0.448960192096371,32.4228918050315));
#55811=CARTESIAN_POINT('Ctrl Pts',(33.5033241171675,0.512515226568531,32.4367303003893));
#55812=CARTESIAN_POINT('Ctrl Pts',(33.2586245183158,0.452129167452444,32.4505687957472));
#55813=CARTESIAN_POINT('Ctrl Pts',(33.0722965338366,0.282405120795205,32.4644072911051));
#55814=CARTESIAN_POINT('Ctrl Pts',(32.9893996916529,0.0443872992571157,
32.478245786463));
#55815=CARTESIAN_POINT('Ctrl Pts',(33.0299808601162,-0.204364662704838,
32.4920842818209));
#55816=CARTESIAN_POINT('Ctrl Pts',(33.1842263319695,-0.403695303165732,
32.5059227771788));
#55817=CARTESIAN_POINT('Ctrl Pts',(33.4148350642942,-0.505400673669678,
32.5197612725367));
#55818=CARTESIAN_POINT('Ctrl Pts',(33.6660391559753,-0.484885456476644,
32.5335997678946));
#55819=CARTESIAN_POINT('Ctrl Pts',(33.877090148776,-0.347110828001091,32.5474382632525));
#55820=CARTESIAN_POINT('Ctrl Pts',(33.9969497720373,-0.125394702007854,
32.5612767586104));
#55821=CARTESIAN_POINT('Ctrl Pts',(33.9966324814981,0.126645511332176,32.5751152539683));
#55822=CARTESIAN_POINT('Ctrl Pts',(33.8762150072425,0.348059155238069,32.5889537493262));
#55823=CARTESIAN_POINT('Ctrl Pts',(33.6648177981328,0.485301968508477,32.6027922446841));
#55824=CARTESIAN_POINT('Ctrl Pts',(33.4135628500049,0.505184645768512,32.616630740042));
#55825=CARTESIAN_POINT('Ctrl Pts',(33.1832109196639,0.402898977163472,32.6304692353998));
#55826=CARTESIAN_POINT('Ctrl Pts',(33.0294678060338,0.203180613398203,32.6443077307577));
#55827=CARTESIAN_POINT('Ctrl Pts',(32.9895130671981,-0.0456727342954641,
32.6581462261156));
#55828=CARTESIAN_POINT('Ctrl Pts',(33.073008921504,-0.283481085972825,32.6719847214735));
#55829=CARTESIAN_POINT('Ctrl Pts',(33.2597636420402,-0.452735463083817,
32.6858232168314));
#55830=CARTESIAN_POINT('Ctrl Pts',(33.5046145036892,-0.512505232729617,
32.6996617121893));
#55831=CARTESIAN_POINT('Ctrl Pts',(33.7483494440856,-0.448336325588192,
32.7135002075472));
#55832=CARTESIAN_POINT('Ctrl Pts',(33.932026263091,-0.27574665042241,32.7273387029051));
#55833=CARTESIAN_POINT('Ctrl Pts',(34.0112265617306,-0.0364734122423689,
32.741177198263));
#55834=CARTESIAN_POINT('Ctrl Pts',(33.966797403434,0.211620158224149,32.7550156936209));
#55835=CARTESIAN_POINT('Ctrl Pts',(33.8094830513586,0.408537817271942,32.7688541889788));
#55836=CARTESIAN_POINT('Ctrl Pts',(33.5773266929505,0.506659145557318,32.7826926843366));
#55837=CARTESIAN_POINT('Ctrl Pts',(33.3264704903407,0.482255551027616,32.7965311796945));
#55838=CARTESIAN_POINT('Ctrl Pts',(33.1175787720664,0.341228532870962,32.8103696750524));
#55839=CARTESIAN_POINT('Ctrl Pts',(33.0011676333814,0.117682527306456,32.8242081704103));
#55840=CARTESIAN_POINT('Ctrl Pts',(33.0053886746414,-0.134322537373713,
32.8380466657682));
#55841=CARTESIAN_POINT('Ctrl Pts',(33.1292211252569,-0.353844504357231,
32.8518851611261));
#55842=CARTESIAN_POINT('Ctrl Pts',(33.3427186957223,-0.487796574961559,
32.865723656484));
#55843=CARTESIAN_POINT('Ctrl Pts',(33.5942514617147,-0.503785241133738,
32.8795621518419));
#55844=CARTESIAN_POINT('Ctrl Pts',(33.8229914819863,-0.397943978197684,
32.8934006471998));
#55845=CARTESIAN_POINT('Ctrl Pts',(33.9736227643672,-0.195868283018701,
32.9072391425577));
#55846=CARTESIAN_POINT('Ctrl Pts',(34.0097182821095,0.0535740618481902,
32.9210776379156));
#55847=CARTESIAN_POINT('Ctrl Pts',(33.9225490888117,0.290060639804727,32.9349161332734));
#55848=CARTESIAN_POINT('Ctrl Pts',(33.7331952316305,0.456402115643996,32.9487546286313));
#55849=CARTESIAN_POINT('Ctrl Pts',(33.4874479825469,0.512372280746522,32.9625931239892));
#55850=CARTESIAN_POINT('Ctrl Pts',(33.2447361764886,0.44443592071962,32.9764316193471));
#55851=CARTESIAN_POINT('Ctrl Pts',(33.0637545899428,0.269022024049182,32.990270114705));
#55852=CARTESIAN_POINT('Ctrl Pts',(32.9882698362566,0.0285507746768112,
33.0041086100629));
#55853=CARTESIAN_POINT('Ctrl Pts',(33.0365363251258,-0.218824882706864,
33.0179471054208));
#55854=CARTESIAN_POINT('Ctrl Pts',(33.1968818152122,-0.413282316667997,
33.0317856007787));
#55855=CARTESIAN_POINT('Ctrl Pts',(33.4305301017064,-0.507796061869929,
33.0456240961366));
#55856=CARTESIAN_POINT('Ctrl Pts',(33.6809782308582,-0.47950994481343,33.0594625914945));
#55857=CARTESIAN_POINT('Ctrl Pts',(33.8876605581656,-0.33526437159691,33.0733010868524));
#55858=CARTESIAN_POINT('Ctrl Pts',(34.0005952833934,-0.109942118697895,
33.0871395822102));
#55859=CARTESIAN_POINT('Ctrl Pts',(33.9924715041075,0.141967337305424,33.1009780775682));
#55860=CARTESIAN_POINT('Ctrl Pts',(33.8652537865034,0.359544960560564,33.114816572926));
#55861=CARTESIAN_POINT('Ctrl Pts',(33.6497070761401,0.490174151269844,33.1286550682839));
#55862=CARTESIAN_POINT('Ctrl Pts',(33.3979568389882,0.502264970419248,33.1424935636418));
#55863=CARTESIAN_POINT('Ctrl Pts',(33.1708836071492,0.392893506151966,33.1563320589997));
#55864=CARTESIAN_POINT('Ctrl Pts',(33.0234002948543,0.188508960727619,33.1701705543576));
#55865=CARTESIAN_POINT('Ctrl Pts',(32.9911726580935,-0.0614625361327144,
33.1840090497155));
#55866=CARTESIAN_POINT('Ctrl Pts',(33.0819942771093,-0.29657060348279,33.1978475450734));
#55867=CARTESIAN_POINT('Ctrl Pts',(33.2739018419382,-0.459959270088812,
33.2116860404313));
#55868=CARTESIAN_POINT('Ctrl Pts',(33.5204865197886,-0.512116402516352,
33.2255245357892));
#55869=CARTESIAN_POINT('Ctrl Pts',(33.7621169610925,-0.440428888616189,
33.2393630311471));
#55870=CARTESIAN_POINT('Ctrl Pts',(33.9403598948212,-0.262232855019252,
33.253201526505));
#55871=CARTESIAN_POINT('Ctrl Pts',(34.0121109935648,-0.0206212873288921,
33.2670400218628));
#55872=CARTESIAN_POINT('Ctrl Pts',(33.9600187540159,0.225977107629683,33.2808785172207));
#55873=CARTESIAN_POINT('Ctrl Pts',(33.7966805953577,0.417927663064147,33.2947170125786));
#55874=CARTESIAN_POINT('Ctrl Pts',(33.5615964366915,0.50881114986548,33.3085555079365));
#55875=CARTESIAN_POINT('Ctrl Pts',(33.3116164675281,0.476649296505977,33.3223940032944));
#55876=CARTESIAN_POINT('Ctrl Pts',(33.1071931174629,0.329219775186188,33.3362324986523));
#55877=CARTESIAN_POINT('Ctrl Pts',(32.9977619007569,0.102175333028977,33.3500709940102));
#55878=CARTESIAN_POINT('Ctrl Pts',(33.0097864685801,-0.149578076467646,
33.3639094893681));
#55879=CARTESIAN_POINT('Ctrl Pts',(33.1403589327563,-0.365159157144441,
33.377747984726));
#55880=CARTESIAN_POINT('Ctrl Pts',(33.3579030677296,-0.492434124234837,
33.3915864800839));
#55881=CARTESIAN_POINT('Ctrl Pts',(33.609810382768,-0.500624202559088,33.4054249754418));
#55882=CARTESIAN_POINT('Ctrl Pts',(33.8351623372906,-0.3877487584928,33.4192634707997));
#55883=CARTESIAN_POINT('Ctrl Pts',(33.9794623238291,-0.181104430520942,
33.4331019661576));
#55884=CARTESIAN_POINT('Ctrl Pts',(34.0078142992225,0.069336338543082,33.4469404615154));
#55885=CARTESIAN_POINT('Ctrl Pts',(33.9133621843763,0.303009339273432,33.4607789568733));
#55886=CARTESIAN_POINT('Ctrl Pts',(33.7189467319906,0.463406465385431,33.4746174522312));
#55887=CARTESIAN_POINT('Ctrl Pts',(33.471584499042,0.511737380133092,33.4884559475891));
#55888=CARTESIAN_POINT('Ctrl Pts',(33.2310924087908,0.436318320607847,33.502294442947));
#55889=CARTESIAN_POINT('Ctrl Pts',(33.055634580726,0.255380012886624,33.5161329383049));
#55890=CARTESIAN_POINT('Ctrl Pts',(32.9876301765048,0.0126987185837221,
33.5299714336628));
#55891=CARTESIAN_POINT('Ctrl Pts',(33.0435551192458,-0.233074971860806,
33.5438099290207));
#55892=CARTESIAN_POINT('Ctrl Pts',(33.1544049364939,-0.359292178734911,
33.5530355925926));
#55893=CARTESIAN_POINT('Ctrl Pts',(33.2215482584371,-0.405409001189644,
33.5576484243786));
#55894=CARTESIAN_POINT('',(33.1650171622239,-0.487714879843178,33.5));
#55895=CARTESIAN_POINT('Ctrl Pts',(33.2772637232775,0.438519776227781,33.5));
#55896=CARTESIAN_POINT('Ctrl Pts',(33.264554241976,0.433572825558528,33.5));
#55897=CARTESIAN_POINT('Ctrl Pts',(33.2520703547844,0.428100356340088,33.5));
#55898=CARTESIAN_POINT('Ctrl Pts',(33.2398461821424,0.422115256115219,33.5));
#55899=CARTESIAN_POINT('Ctrl Pts',(33.2208949675549,0.412836516194648,33.5));
#55900=CARTESIAN_POINT('Ctrl Pts',(33.2025674999342,0.402326836673748,33.5));
#55901=CARTESIAN_POINT('Ctrl Pts',(33.1849490649597,0.390687168471131,33.5));
#55902=CARTESIAN_POINT('Ctrl Pts',(33.1776603524031,0.385871860192905,33.5));
#55903=CARTESIAN_POINT('Ctrl Pts',(33.1704930576834,0.380862889958598,33.5));
#55904=CARTESIAN_POINT('Ctrl Pts',(33.1634536169048,0.375666332886166,33.5));
#55905=CARTESIAN_POINT('Ctrl Pts',(33.1575024102688,0.371273116733489,33.5));
#55906=CARTESIAN_POINT('Ctrl Pts',(33.1516504113687,0.366751562502987,33.5));
#55907=CARTESIAN_POINT('Ctrl Pts',(33.145902317669,0.362107265379308,33.5));
#55908=CARTESIAN_POINT('Ctrl Pts',(33.1275232441798,0.347257493854776,33.5));
#55909=CARTESIAN_POINT('Ctrl Pts',(33.1102011405989,0.331151934805194,33.5));
#55910=CARTESIAN_POINT('Ctrl Pts',(33.0940545291096,0.313921676817133,33.5));
#55911=CARTESIAN_POINT('Ctrl Pts',(33.0857494752691,0.30505924643224,33.5));
#55912=CARTESIAN_POINT('Ctrl Pts',(33.0777556075603,0.295898771155094,33.5));
#55913=CARTESIAN_POINT('Ctrl Pts',(33.0700907996204,0.286455259990925,33.5));
#55914=CARTESIAN_POINT('Ctrl Pts',(33.0658955864609,0.281286501345002,33.5));
#55915=CARTESIAN_POINT('Ctrl Pts',(33.061800004697,0.276033932307431,33.5));
#55916=CARTESIAN_POINT('Ctrl Pts',(33.0578140698389,0.270710086715202,33.5));
#55917=CARTESIAN_POINT('Ctrl Pts',(33.0549239815682,0.266849917332431,33.5));
#55918=CARTESIAN_POINT('Ctrl Pts',(33.0520904344765,0.26295093532825,33.5));
#55919=CARTESIAN_POINT('Ctrl Pts',(33.049314330518,0.259014291594346,33.5));
#55920=CARTESIAN_POINT('Ctrl Pts',(33.0338107317892,0.237029471969558,33.5));
#55921=CARTESIAN_POINT('Ctrl Pts',(33.0200959511177,0.213873549718448,33.5));
#55922=CARTESIAN_POINT('Ctrl Pts',(33.0082075477657,0.189799179432742,33.5));
#55923=CARTESIAN_POINT('Ctrl Pts',(32.9999426033142,0.173062421163136,33.5));
#55924=CARTESIAN_POINT('Ctrl Pts',(32.9925609962723,0.155880697409843,33.5));
#55925=CARTESIAN_POINT('Ctrl Pts',(32.9860862039813,0.138328967918389,33.5));
#55926=CARTESIAN_POINT('Ctrl Pts',(32.9823662821442,0.128245082771157,33.5));
#55927=CARTESIAN_POINT('Ctrl Pts',(32.9789458547006,0.1180389383614,33.5));
#55928=CARTESIAN_POINT('Ctrl Pts',(32.9758309272349,0.107723956008069,33.5));
#55929=CARTESIAN_POINT('Ctrl Pts',(32.9740057553728,0.101679957951775,33.5));
#55930=CARTESIAN_POINT('Ctrl Pts',(32.9722856812918,0.0955986077487019,
33.5));
#55931=CARTESIAN_POINT('Ctrl Pts',(32.9706753632345,0.0894969354091739,
33.5));
#55932=CARTESIAN_POINT('Ctrl Pts',(32.9640744609225,0.064485390099134,33.5));
#55933=CARTESIAN_POINT('Ctrl Pts',(32.9592969078889,0.039075611355351,33.5));
#55934=CARTESIAN_POINT('Ctrl Pts',(32.9563846394091,0.013469266518338,33.5));
#55935=CARTESIAN_POINT('Ctrl Pts',(32.9537796670569,-0.0094351534564494,
33.5));
#55936=CARTESIAN_POINT('Ctrl Pts',(32.9526672019952,-0.03249765710831,33.5));
#55937=CARTESIAN_POINT('Ctrl Pts',(32.9530094279876,-0.0555821660130952,
33.5));
#55938=CARTESIAN_POINT('Ctrl Pts',(32.9532476027417,-0.0716480036578533,
33.5));
#55939=CARTESIAN_POINT('Ctrl Pts',(32.9541908795881,-0.0877247191209388,
33.5));
#55940=CARTESIAN_POINT('Ctrl Pts',(32.9558335304502,-0.103767324918046,
33.5));
#55941=CARTESIAN_POINT('Ctrl Pts',(32.9564700139004,-0.109983407303375,
33.5));
#55942=CARTESIAN_POINT('Ctrl Pts',(32.9572113552717,-0.116191235045043,
33.5));
#55943=CARTESIAN_POINT('Ctrl Pts',(32.9580553900102,-0.122377954099875,
33.5));
#55944=CARTESIAN_POINT('Ctrl Pts',(32.9619296543732,-0.150776056764607,
33.5));
#55945=CARTESIAN_POINT('Ctrl Pts',(32.9679695131037,-0.178790563170583,
33.5));
#55946=CARTESIAN_POINT('Ctrl Pts',(32.9760939678284,-0.206170296562812,
33.5));
#55947=CARTESIAN_POINT('Ctrl Pts',(32.981322310141,-0.223790016710321,33.5));
#55948=CARTESIAN_POINT('Ctrl Pts',(32.9874150180619,-0.241147215258263,
33.5));
#55949=CARTESIAN_POINT('Ctrl Pts',(32.9943618796823,-0.258175364000595,
33.5));
#55950=CARTESIAN_POINT('Ctrl Pts',(32.9998054693488,-0.271518692196782,
33.5));
#55951=CARTESIAN_POINT('Ctrl Pts',(33.005773722051,-0.2846599933777,33.5));
#55952=CARTESIAN_POINT('Ctrl Pts',(33.0122473233693,-0.297575933006044,
33.5));
#55953=CARTESIAN_POINT('Ctrl Pts',(33.015013334055,-0.303094596462559,33.5));
#55954=CARTESIAN_POINT('Ctrl Pts',(33.0178716432429,-0.308572102159929,
33.5));
#55955=CARTESIAN_POINT('Ctrl Pts',(33.0208209167752,-0.314006552440097,
33.5));
#55956=CARTESIAN_POINT('Ctrl Pts',(33.0239419191389,-0.319757437186323,
33.5));
#55957=CARTESIAN_POINT('Ctrl Pts',(33.0271607080724,-0.325452504564708,
33.5));
#55958=CARTESIAN_POINT('Ctrl Pts',(33.0304730359995,-0.331086696102647,
33.5));
#55959=CARTESIAN_POINT('Ctrl Pts',(33.0452281581033,-0.356184810156879,
33.5));
#55960=CARTESIAN_POINT('Ctrl Pts',(33.0618462021435,-0.380095915481538,
33.5));
#55961=CARTESIAN_POINT('Ctrl Pts',(33.0801349436199,-0.402645602306231,
33.5));
#55962=CARTESIAN_POINT('Ctrl Pts',(33.0985591695158,-0.425362338965038,
33.5));
#55963=CARTESIAN_POINT('Ctrl Pts',(33.118679569832,-0.446698575046518,33.5));
#55964=CARTESIAN_POINT('Ctrl Pts',(33.1403470491557,-0.466455159197211,
33.5));
#55965=CARTESIAN_POINT('Ctrl Pts',(33.1483604592386,-0.473761851788011,
33.5));
#55966=CARTESIAN_POINT('Ctrl Pts',(33.1565858923756,-0.480852189022173,
33.5));
#55967=CARTESIAN_POINT('Ctrl Pts',(33.1650171622239,-0.487714879843202,
33.5));
#55968=CARTESIAN_POINT('Ctrl Pts',(33.1650171622239,-0.487714879843177,
33.5));
#55969=CARTESIAN_POINT('Ctrl Pts',(33.0842424455853,-0.432235449302022,
33.495387168214));
#55970=CARTESIAN_POINT('Ctrl Pts',(33.0175652071161,-0.35631457716536,33.4907743364281));
#55971=CARTESIAN_POINT('Ctrl Pts',(32.9730134563489,-0.269075722860955,
33.4861615046421));
#55972=CARTESIAN_POINT('Ctrl Pts',(32.9306815187938,-0.186183588002268,
33.4817785095016));
#55973=CARTESIAN_POINT('Ctrl Pts',(32.908325170312,-0.0930732213935219,
33.477395514361));
#55974=CARTESIAN_POINT('Ctrl Pts',(32.9082801122102,1.43778562331377E-5,
33.4730125192205));
#55975=CARTESIAN_POINT('Origin',(33.5,-5.18803696760693,35.5291310458943));
#55976=CARTESIAN_POINT('',(33.5,-1.5,34.2166945550901));
#55977=CARTESIAN_POINT('Ctrl Pts',(33.5,-1.5,34.2166945550901));
#55978=CARTESIAN_POINT('Ctrl Pts',(33.3993978221096,-1.5,34.2166945550901));
#55979=CARTESIAN_POINT('Ctrl Pts',(33.2928068450241,-1.48895277818718,34.235623681809));
#55980=CARTESIAN_POINT('Ctrl Pts',(33.0978649440217,-1.44851537165468,34.3118781114152));
#55981=CARTESIAN_POINT('Ctrl Pts',(33.0094286355118,-1.41950887463153,34.3691880921119));
#55982=CARTESIAN_POINT('Ctrl Pts',(32.8708460907051,-1.36369370769132,34.50166878881));
#55983=CARTESIAN_POINT('Ctrl Pts',(32.8107426530931,-1.33304799986427,34.5856779758953));
#55984=CARTESIAN_POINT('Ctrl Pts',(32.7307870936806,-1.28856686896643,34.7735600475602));
#55985=CARTESIAN_POINT('Ctrl Pts',(32.7109953412679,-1.27572397033959,34.87769219842));
#55986=CARTESIAN_POINT('Ctrl Pts',(32.7109953412679,-1.27572397033959,34.9767687364291));
#55987=CARTESIAN_POINT('Ctrl Pts',(32.7109953412679,-1.27572397033959,35.0811944929964));
#55988=CARTESIAN_POINT('Ctrl Pts',(32.7325681300429,-1.28966817169834,35.190515575808));
#55989=CARTESIAN_POINT('Ctrl Pts',(32.8047823956101,-1.32964117071253,35.367012109162));
#55990=CARTESIAN_POINT('Ctrl Pts',(32.8470860406361,-1.35151557956927,35.4382625553338));
#55991=CARTESIAN_POINT('Ctrl Pts',(32.8963072647134,-1.37315515560413,35.4999999999999));
#55992=CARTESIAN_POINT('',(33.5,-9.66736334079664,35.5527627697757));
#55993=CARTESIAN_POINT('',(33.5,-5.28545813827897,34.8359433977753));
#55994=CARTESIAN_POINT('',(32.9141578431745,-9.56582650875709,36.2752348701767));
#55995=CARTESIAN_POINT('Origin',(33.5,-9.5838594802206,36.1469236110206));
#55996=CARTESIAN_POINT('',(34.0858421568255,-9.56582650875709,36.2752348701767));
#55997=CARTESIAN_POINT('Origin',(33.5,-9.5838594802206,36.1469236110206));
#55998=CARTESIAN_POINT('Origin',(33.5,-9.5838594802206,36.1469236110206));
#55999=CARTESIAN_POINT('Ctrl Pts',(34.1036927352866,-1.37315515560413,35.4999999999999));
#56000=CARTESIAN_POINT('Ctrl Pts',(34.1529139593639,-1.35151557956927,35.4382625553338));
#56001=CARTESIAN_POINT('Ctrl Pts',(34.1952176043899,-1.32964117071253,35.367012109162));
#56002=CARTESIAN_POINT('Ctrl Pts',(34.2674318699571,-1.28966817169834,35.190515575808));
#56003=CARTESIAN_POINT('Ctrl Pts',(34.2890046587321,-1.27572397033959,35.0811944929964));
#56004=CARTESIAN_POINT('Ctrl Pts',(34.2890046587321,-1.27572397033959,34.87769219842));
#56005=CARTESIAN_POINT('Ctrl Pts',(34.2692129063194,-1.28856686896643,34.7735600475602));
#56006=CARTESIAN_POINT('Ctrl Pts',(34.1892573469069,-1.33304799986427,34.5856779758953));
#56007=CARTESIAN_POINT('Ctrl Pts',(34.1291539092949,-1.36369370769132,34.50166878881));
#56008=CARTESIAN_POINT('Ctrl Pts',(33.9905713644882,-1.41950887463153,34.3691880921119));
#56009=CARTESIAN_POINT('Ctrl Pts',(33.9021350559783,-1.44851537165468,34.3118781114152));
#56010=CARTESIAN_POINT('Ctrl Pts',(33.7071931549759,-1.48895277818718,34.235623681809));
#56011=CARTESIAN_POINT('Ctrl Pts',(33.6006021778904,-1.5,34.2166945550901));
#56012=CARTESIAN_POINT('Ctrl Pts',(33.5,-1.5,34.2166945550901));
#56013=CARTESIAN_POINT('',(33.5756815123179,-0.681375306782742,35.7));
#56014=CARTESIAN_POINT('Origin',(33.5,-5.60904829084331,35.7));
#56015=CARTESIAN_POINT('',(33.4243184876821,-0.681375306782742,35.7));
#56016=CARTESIAN_POINT('Origin',(33.5,-0.792214454993257,34.9113384807681));
#56017=CARTESIAN_POINT('Origin',(33.5,-5.60904829084331,35.7));
#56018=CARTESIAN_POINT('Origin',(33.5,-10.4968415286607,36.2752348701767));
#56019=CARTESIAN_POINT('',(32.4,-10.4968415286607,36.2752348701767));
#56020=CARTESIAN_POINT('Origin',(33.5,-10.4968415286607,36.2752348701767));
#56021=CARTESIAN_POINT('',(34.6,-10.4968415286607,36.2752348701767));
#56022=CARTESIAN_POINT('Origin',(33.5,-10.4968415286607,36.2752348701767));
#56023=CARTESIAN_POINT('Origin',(33.5,-0.792214454993256,34.9113384807681));
#56024=CARTESIAN_POINT('',(33.5,-0.681375306782741,35.7));
#56025=CARTESIAN_POINT('Origin',(33.5,0.,35.7));
#56026=CARTESIAN_POINT('Origin',(34.05,0.,31.8));
#56027=CARTESIAN_POINT('',(32.95,-6.73555739531042E-17,31.8));
#56028=CARTESIAN_POINT('Origin',(33.5,0.,31.8));
#56029=CARTESIAN_POINT('Origin',(33.5,0.,31.825));
#56030=CARTESIAN_POINT('',(32.925,-7.04171909509732E-17,31.825));
#56031=CARTESIAN_POINT('Origin',(33.5,0.,32.675));
#56032=CARTESIAN_POINT('Origin',(33.5,0.,33.5));
#56033=CARTESIAN_POINT('Origin',(35.,0.,33.5));
#56034=CARTESIAN_POINT('',(32.,-1.83697019872103E-16,33.5));
#56035=CARTESIAN_POINT('Origin',(33.5,0.,33.5));
#56036=CARTESIAN_POINT('Origin',(33.5,0.,34.5));
#56037=CARTESIAN_POINT('',(32.,-1.83697019872103E-16,34.5));
#56038=CARTESIAN_POINT('',(0.,0.,0.));
#56039=CARTESIAN_POINT('Origin',(33.5,0.,26.5));
#56040=CARTESIAN_POINT('',(33.5,-1.,29.8541019662497));
#56041=CARTESIAN_POINT('',(32.5,-1.16743491188625E-16,30.));
#56042=CARTESIAN_POINT('Ctrl Pts',(33.5,-1.,29.8541019662497));
#56043=CARTESIAN_POINT('Ctrl Pts',(33.6263404272294,-1.,29.8541019662497));
#56044=CARTESIAN_POINT('Ctrl Pts',(33.7605855308726,-0.974606077798943,
29.861986486613));
#56045=CARTESIAN_POINT('Ctrl Pts',(34.006735263926,-0.872342432005776,29.8899599884511));
#56046=CARTESIAN_POINT('Ctrl Pts',(34.1187060914405,-0.795507470932603,
29.9095916302829));
#56047=CARTESIAN_POINT('Ctrl Pts',(34.2954859845766,-0.618727577796462,
29.9460585378213));
#56048=CARTESIAN_POINT('Ctrl Pts',(34.3723376201997,-0.506747952410379,
29.9653343432958));
#56049=CARTESIAN_POINT('Ctrl Pts',(34.4746135319146,-0.260566482292827,
29.9924834581629));
#56050=CARTESIAN_POINT('Ctrl Pts',(34.5,-0.126309719376294,30.));
#56051=CARTESIAN_POINT('Ctrl Pts',(34.5,0.126309719376294,30.));
#56052=CARTESIAN_POINT('Ctrl Pts',(34.4746135319146,0.260566482292828,29.9924834581629));
#56053=CARTESIAN_POINT('Ctrl Pts',(34.3723376201997,0.50674795241038,29.9653343432958));
#56054=CARTESIAN_POINT('Ctrl Pts',(34.2954859845766,0.618727577796462,29.9460585378213));
#56055=CARTESIAN_POINT('Ctrl Pts',(34.1187060914405,0.795507470932603,29.9095916302829));
#56056=CARTESIAN_POINT('Ctrl Pts',(34.006735263926,0.872342432005776,29.8899599884511));
#56057=CARTESIAN_POINT('Ctrl Pts',(33.7605855308726,0.974606077798943,29.861986486613));
#56058=CARTESIAN_POINT('Ctrl Pts',(33.6263404272294,1.,29.8541019662497));
#56059=CARTESIAN_POINT('Ctrl Pts',(33.3736595727706,1.,29.8541019662497));
#56060=CARTESIAN_POINT('Ctrl Pts',(33.2394144691274,0.974606077798943,29.861986486613));
#56061=CARTESIAN_POINT('Ctrl Pts',(32.993264736074,0.872342432005776,29.8899599884511));
#56062=CARTESIAN_POINT('Ctrl Pts',(32.8812939085595,0.795507470932603,29.9095916302829));
#56063=CARTESIAN_POINT('Ctrl Pts',(32.7045140154234,0.618727577796462,29.9460585378213));
#56064=CARTESIAN_POINT('Ctrl Pts',(32.6276623798003,0.506747952410379,29.9653343432958));
#56065=CARTESIAN_POINT('Ctrl Pts',(32.5253864680854,0.260566482292827,29.9924834581629));
#56066=CARTESIAN_POINT('Ctrl Pts',(32.5,0.126309719376294,30.));
#56067=CARTESIAN_POINT('Ctrl Pts',(32.5,3.05311331771918E-16,30.));
#56068=CARTESIAN_POINT('Ctrl Pts',(32.5,-5.55111512312578E-17,30.));
#56069=CARTESIAN_POINT('Ctrl Pts',(32.5,-0.126309719376293,30.));
#56070=CARTESIAN_POINT('Ctrl Pts',(32.5253864680854,-0.260566482292827,
29.9924834581629));
#56071=CARTESIAN_POINT('Ctrl Pts',(32.6276623798003,-0.506747952410379,
29.9653343432958));
#56072=CARTESIAN_POINT('Ctrl Pts',(32.7045140154234,-0.618727577796462,
29.9460585378213));
#56073=CARTESIAN_POINT('Ctrl Pts',(32.8812939085595,-0.795507470932602,
29.9095916302829));
#56074=CARTESIAN_POINT('Ctrl Pts',(32.993264736074,-0.872342432005776,29.8899599884511));
#56075=CARTESIAN_POINT('Ctrl Pts',(33.2394144691274,-0.974606077798943,
29.861986486613));
#56076=CARTESIAN_POINT('Ctrl Pts',(33.3736595727706,-1.,29.8541019662497));
#56077=CARTESIAN_POINT('Ctrl Pts',(33.5,-1.,29.8541019662497));
#56078=CARTESIAN_POINT('Origin',(33.5,0.,30.675));
#56079=CARTESIAN_POINT('',(32.5,-1.22464679914735E-16,31.75));
#56080=CARTESIAN_POINT('Origin',(33.5,0.,31.75));
#56081=CARTESIAN_POINT('',(32.5,-1.22464679914735E-16,30.675));
#56082=CARTESIAN_POINT('Origin',(33.5,0.,31.775));
#56083=CARTESIAN_POINT('',(32.55,-1.16341445918999E-16,31.8));
#56084=CARTESIAN_POINT('Origin',(33.5,0.,31.8));
#56085=CARTESIAN_POINT('',(32.525,-1.19403062916867E-16,31.775));
#56086=CARTESIAN_POINT('Origin',(33.5,0.,31.8));
#56087=CARTESIAN_POINT('',(0.,0.,0.));
#56088=CARTESIAN_POINT('Origin',(0.,0.,0.93));
#56089=CARTESIAN_POINT('',(-0.393785571917083,0.000248495837930046,0.0937163522034969));
#56090=CARTESIAN_POINT('',(-0.393691807349815,0.000401671216108742,0.0753836477965013));
#56091=CARTESIAN_POINT('',(-0.3933,-4.81653586104654E-17,0.93));
#56092=CARTESIAN_POINT('',(0.175074770038262,0.352555242519502,0.0533));
#56093=CARTESIAN_POINT('Ctrl Pts',(-0.393785571917083,0.000248495837930046,
0.0937163522034969));
#56094=CARTESIAN_POINT('Ctrl Pts',(-0.393873138151706,0.0131776353947525,
0.0930600049995511));
#56095=CARTESIAN_POINT('Ctrl Pts',(-0.393291866198186,0.0260982907353025,
0.0924036577956053));
#56096=CARTESIAN_POINT('Ctrl Pts',(-0.392015953470318,0.038949338819979,
0.0917473105916596));
#56097=CARTESIAN_POINT('Ctrl Pts',(-0.379144732760665,0.168588829543332,
0.0851261761365885));
#56098=CARTESIAN_POINT('Ctrl Pts',(-0.295583540395456,0.29114475257756,
0.0785050416815174));
#56099=CARTESIAN_POINT('Ctrl Pts',(-0.179607489182299,0.350585393928814,
0.0718839072264463));
#56100=CARTESIAN_POINT('Ctrl Pts',(-0.071102006178845,0.40619718129687,
0.0656892714842975));
#56101=CARTESIAN_POINT('Ctrl Pts',(0.0657768433630953,0.406562915311091,
0.0594946357421488));
#56102=CARTESIAN_POINT('Ctrl Pts',(0.175280092543415,0.352824285593914,
0.0533));
#56103=CARTESIAN_POINT('',(-0.174869447533114,0.352286199445087,0.0533));
#56104=CARTESIAN_POINT('Origin',(0.,0.,0.0533));
#56105=CARTESIAN_POINT('Ctrl Pts',(-0.174869447533113,0.352286199445087,
0.0533000000000003));
#56106=CARTESIAN_POINT('Ctrl Pts',(-0.292115409128919,0.294087108586454,
0.0599211344550713));
#56107=CARTESIAN_POINT('Ctrl Pts',(-0.377001626803167,0.173250680215973,
0.0665422689101422));
#56108=CARTESIAN_POINT('Ctrl Pts',(-0.391451042526116,0.0439776134704028,
0.0731634033652133));
#56109=CARTESIAN_POINT('Ctrl Pts',(-0.393066135076189,0.0295280349525525,
0.0739034848423093));
#56110=CARTESIAN_POINT('Ctrl Pts',(-0.393801204906527,0.0149730508336159,
0.0746435663194053));
#56111=CARTESIAN_POINT('Ctrl Pts',(-0.393691807349815,0.000401671216108742,
0.0753836477965013));
#56112=CARTESIAN_POINT('Origin',(0.,0.,0.93));
#56113=CARTESIAN_POINT('',(-0.392774766082733,0.000218508532499828,0.218716352203497));
#56114=CARTESIAN_POINT('',(-0.392747480256298,0.000198404254828114,0.200383647796502));
#56115=CARTESIAN_POINT('',(-0.3933,-4.81653586104654E-17,0.93));
#56116=CARTESIAN_POINT('Ctrl Pts',(-0.392774766082733,0.000218508532499828,
0.218716352203497));
#56117=CARTESIAN_POINT('Ctrl Pts',(-0.393033682673394,0.0517027350259926,
0.216120145063311));
#56118=CARTESIAN_POINT('Ctrl Pts',(-0.383636180758456,0.103096084244051,
0.213523937923125));
#56119=CARTESIAN_POINT('Ctrl Pts',(-0.364141337824362,0.150320959570902,
0.210927730782939));
#56120=CARTESIAN_POINT('Ctrl Pts',(-0.314423434252966,0.270759057256997,
0.204306596327868));
#56121=CARTESIAN_POINT('Ctrl Pts',(-0.19903157760138,0.36408505105081,0.197685461872797));
#56122=CARTESIAN_POINT('Ctrl Pts',(-0.0708595116212159,0.3875222920239,
0.191064327417726));
#56123=CARTESIAN_POINT('Ctrl Pts',(0.0573125543589477,0.41095953299699,
0.184443192962655));
#56124=CARTESIAN_POINT('Ctrl Pts',(0.198264829667689,0.364508021149357,
0.177822058507584));
#56125=CARTESIAN_POINT('Ctrl Pts',(0.287385293506548,0.269454991498079,
0.171200924052513));
#56126=CARTESIAN_POINT('Ctrl Pts',(0.376505757345406,0.174401961846802,
0.164579789597442));
#56127=CARTESIAN_POINT('Ctrl Pts',(0.413794409714382,0.030747414391879,
0.157958655142371));
#56128=CARTESIAN_POINT('Ctrl Pts',(0.38216066130072,-0.0956482825730319,
0.151337520687299));
#56129=CARTESIAN_POINT('Ctrl Pts',(0.350526912887059,-0.222043979537944,
0.144716386232228));
#56130=CARTESIAN_POINT('Ctrl Pts',(0.249970763690759,-0.331180826012843,
0.138095251777157));
#56131=CARTESIAN_POINT('Ctrl Pts',(0.126581974628838,-0.373052348623724,
0.131474117322086));
#56132=CARTESIAN_POINT('Ctrl Pts',(0.0031931855669175,-0.414923871234605,
0.124852982867015));
#56133=CARTESIAN_POINT('Ctrl Pts',(-0.143028243360624,-0.389530069981469,
0.118231848411944));
#56134=CARTESIAN_POINT('Ctrl Pts',(-0.245048333297346,-0.308471640148661,
0.111610713956873));
#56135=CARTESIAN_POINT('Ctrl Pts',(-0.336955261927553,-0.235448460791133,
0.105645926705748));
#56136=CARTESIAN_POINT('Ctrl Pts',(-0.392989782803075,-0.117249630661176,
0.0996811394546222));
#56137=CARTESIAN_POINT('Ctrl Pts',(-0.393785571917083,0.000248495837930046,
0.0937163522034969));
#56138=CARTESIAN_POINT('Ctrl Pts',(-0.393691807349815,0.000401671216108742,
0.0753836477965013));
#56139=CARTESIAN_POINT('Ctrl Pts',(-0.392822480327593,-0.115389708712764,
0.0812647007744764));
#56140=CARTESIAN_POINT('Ctrl Pts',(-0.338627768779739,-0.23221641135412,
0.0871457537524516));
#56141=CARTESIAN_POINT('Ctrl Pts',(-0.248949174886101,-0.305413577230776,
0.0930268067304266));
#56142=CARTESIAN_POINT('Ctrl Pts',(-0.147985277751488,-0.387821996065721,
0.0996479411854977));
#56143=CARTESIAN_POINT('Ctrl Pts',(-0.00204486971061162,-0.414929128614953,
0.106269075640569));
#56144=CARTESIAN_POINT('Ctrl Pts',(0.121875108290386,-0.374587115506913,
0.11289021009564));
#56145=CARTESIAN_POINT('Ctrl Pts',(0.245795086291383,-0.334245102398874,
0.119511344550711));
#56146=CARTESIAN_POINT('Ctrl Pts',(0.347694634252502,-0.226453943633564,
0.126132479005782));
#56147=CARTESIAN_POINT('Ctrl Pts',(0.380915425583095,-0.100483894323947,
0.132753613460853));
#56148=CARTESIAN_POINT('Ctrl Pts',(0.414136216913688,0.0254861549856705,
0.139374747915924));
#56149=CARTESIAN_POINT('Ctrl Pts',(0.378678251613755,0.169635094839595,
0.145995882370995));
#56150=CARTESIAN_POINT('Ctrl Pts',(0.290768388774417,0.26581421567225,0.152617016826066));
#56151=CARTESIAN_POINT('Ctrl Pts',(0.20285852593508,0.361993336504906,0.159238151281137));
#56152=CARTESIAN_POINT('Ctrl Pts',(0.0624967655563389,0.410202638316291,
0.165859285736208));
#56153=CARTESIAN_POINT('Ctrl Pts',(-0.0659627539324038,0.388381262159473,
0.17248042019128));
#56154=CARTESIAN_POINT('Ctrl Pts',(-0.194422273421146,0.366559886002655,
0.179101554646351));
#56155=CARTESIAN_POINT('Ctrl Pts',(-0.310979552019891,0.274707831877633,
0.185722689101422));
#56156=CARTESIAN_POINT('Ctrl Pts',(-0.362213305892249,0.15490936366835,
0.192343823556493));
#56157=CARTESIAN_POINT('Ctrl Pts',(-0.382950455952394,0.106420259816605,
0.195023764969829));
#56158=CARTESIAN_POINT('Ctrl Pts',(-0.392985841361541,0.0533527755479766,
0.197703706383165));
#56159=CARTESIAN_POINT('Ctrl Pts',(-0.392747480256298,0.000198404254828114,
0.200383647796502));
#56160=CARTESIAN_POINT('Origin',(0.,0.,0.93));
#56161=CARTESIAN_POINT('',(-0.392993347059397,-0.000324654934744873,0.343716352203497));
#56162=CARTESIAN_POINT('',(-0.393037056464261,-0.000335938643299616,0.325383647796502));
#56163=CARTESIAN_POINT('',(-0.3933,-4.81653586104654E-17,0.93));
#56164=CARTESIAN_POINT('Ctrl Pts',(-0.392993347059397,-0.000324654934744872,
0.343716352203497));
#56165=CARTESIAN_POINT('Ctrl Pts',(-0.392295244312066,0.089502206410554,
0.339180285127071));
#56166=CARTESIAN_POINT('Ctrl Pts',(-0.361732461003469,0.179758489715605,
0.334644218050645));
#56167=CARTESIAN_POINT('Ctrl Pts',(-0.305324449239513,0.248942199255532,
0.330108150974219));
#56168=CARTESIAN_POINT('Ctrl Pts',(-0.222987697172201,0.349927179249557,
0.323487016519147));
#56169=CARTESIAN_POINT('Ctrl Pts',(-0.0855845998030076,0.406014524643294,
0.316865882064077));
#56170=CARTESIAN_POINT('Ctrl Pts',(0.0439008348702589,0.391494492203043,
0.310244747609005));
#56171=CARTESIAN_POINT('Ctrl Pts',(0.173386269543525,0.376974459762792,
0.303623613153934));
#56172=CARTESIAN_POINT('Ctrl Pts',(0.294954041520864,0.291847049488554,
0.297002478698863));
#56173=CARTESIAN_POINT('Ctrl Pts',(0.352878842457608,0.175133586498971,
0.290381344243792));
#56174=CARTESIAN_POINT('Ctrl Pts',(0.410803643394352,0.0584201235093882,
0.283760209788721));
#56175=CARTESIAN_POINT('Ctrl Pts',(0.4050854732905,-0.0898793921955392,
0.27713907533365));
#56176=CARTESIAN_POINT('Ctrl Pts',(0.338345518826343,-0.201785929869207,
0.270517940878579));
#56177=CARTESIAN_POINT('Ctrl Pts',(0.271605564362186,-0.313692467542874,
0.263896806423508));
#56178=CARTESIAN_POINT('Ctrl Pts',(0.143843825537725,-0.389206027185282,
0.257275671968437));
#56179=CARTESIAN_POINT('Ctrl Pts',(0.0136247512769219,-0.393712466080529,
0.250654537513365));
#56180=CARTESIAN_POINT('Ctrl Pts',(-0.116594322983881,-0.398218904975776,
0.244033403058294));
#56181=CARTESIAN_POINT('Ctrl Pts',(-0.249270732681025,-0.331718223123861,
0.237412268603223));
#56182=CARTESIAN_POINT('Ctrl Pts',(-0.323586962283995,-0.224692781408716,
0.230791134148152));
#56183=CARTESIAN_POINT('Ctrl Pts',(-0.368763121218386,-0.159632990421233,
0.226766206833267));
#56184=CARTESIAN_POINT('Ctrl Pts',(-0.392373364961114,-0.0795980308691116,
0.222741279518382));
#56185=CARTESIAN_POINT('Ctrl Pts',(-0.392774766082733,0.000218508532499828,
0.218716352203497));
#56186=CARTESIAN_POINT('Ctrl Pts',(-0.392747480256298,0.000198404254828114,
0.200383647796502));
#56187=CARTESIAN_POINT('Ctrl Pts',(-0.392396940082276,-0.077971826346426,
0.204324840838236));
#56188=CARTESIAN_POINT('Ctrl Pts',(-0.369826931677392,-0.156329971208392,
0.208266033879971));
#56189=CARTESIAN_POINT('Ctrl Pts',(-0.326398803783175,-0.220590446720741,
0.212207226921706));
#56190=CARTESIAN_POINT('Ctrl Pts',(-0.253440318655772,-0.328546906607003,
0.218828361376777));
#56191=CARTESIAN_POINT('Ctrl Pts',(-0.121613119254995,-0.396714944085984,
0.225449495831848));
#56192=CARTESIAN_POINT('Ctrl Pts',(0.00865273155690482,-0.393852455738489,
0.232070630286919));
#56193=CARTESIAN_POINT('Ctrl Pts',(0.138918582368805,-0.390989967390994,
0.23869176474199));
#56194=CARTESIAN_POINT('Ctrl Pts',(0.267623084591827,-0.317096953217022,
0.245312899197062));
#56195=CARTESIAN_POINT('Ctrl Pts',(0.335770584171616,-0.206042341202286,
0.251934033652133));
#56196=CARTESIAN_POINT('Ctrl Pts',(0.403918083751406,-0.0949877291875496,
0.258555168107204));
#56197=CARTESIAN_POINT('Ctrl Pts',(0.411508580687962,0.0532284806679498,
0.265176302562275));
#56198=CARTESIAN_POINT('Ctrl Pts',(0.355062141117544,0.170664205462423,
0.271797437017346));
#56199=CARTESIAN_POINT('Ctrl Pts',(0.298615701547127,0.288099930256896,
0.278418571472417));
#56200=CARTESIAN_POINT('Ctrl Pts',(0.178132325469737,0.374755169990342,
0.285039705927488));
#56201=CARTESIAN_POINT('Ctrl Pts',(0.0488405039998853,0.390908905805843,
0.291660840382559));
#56202=CARTESIAN_POINT('Ctrl Pts',(-0.0804513174699659,0.407062641621344,
0.29828197483763));
#56203=CARTESIAN_POINT('Ctrl Pts',(-0.218551584332279,0.352714873518899,
0.304903109292701));
#56204=CARTESIAN_POINT('Ctrl Pts',(-0.302156848319226,0.252777605399255,
0.311524243747772));
#56205=CARTESIAN_POINT('Ctrl Pts',(-0.360491218965147,0.183047813735153,
0.316144045097349));
#56206=CARTESIAN_POINT('Ctrl Pts',(-0.392295515188098,0.0911234580827075,
0.320763846446925));
#56207=CARTESIAN_POINT('Ctrl Pts',(-0.393037056464261,-0.000335938643299616,
0.325383647796502));
#56208=CARTESIAN_POINT('Origin',(0.,0.,0.93));
#56209=CARTESIAN_POINT('',(-0.393939358387839,-5.33598371626476E-5,0.468716352203497));
#56210=CARTESIAN_POINT('',(-0.39394666710269,-2.26739104671677E-5,0.450383647796501));
#56211=CARTESIAN_POINT('',(-0.3933,-4.81653586104654E-17,0.93));
#56212=CARTESIAN_POINT('Ctrl Pts',(-0.393939358387839,-5.33598371626476E-5,
0.468716352203497));
#56213=CARTESIAN_POINT('Ctrl Pts',(-0.393697045666046,0.127393873184695,
0.462240425190831));
#56214=CARTESIAN_POINT('Ctrl Pts',(-0.326158936027309,0.255061565108686,
0.455764498178165));
#56215=CARTESIAN_POINT('Ctrl Pts',(-0.220566552565224,0.326413281704456,
0.449288571165498));
#56216=CARTESIAN_POINT('Ctrl Pts',(-0.112606508085655,0.399364892841627,
0.442667436710427));
#56217=CARTESIAN_POINT('Ctrl Pts',(0.0351334982603933,0.413446707607708,
0.436046302255356));
#56218=CARTESIAN_POINT('Ctrl Pts',(0.15493112546501,0.362203783209636,0.429425167800285));
#56219=CARTESIAN_POINT('Ctrl Pts',(0.274728752669627,0.310960858811565,
0.422804033345214));
#56220=CARTESIAN_POINT('Ctrl Pts',(0.366584000732812,0.194393195249342,
0.416182898890143));
#56221=CARTESIAN_POINT('Ctrl Pts',(0.388391466562617,0.0659340835312544,
0.409561764435072));
#56222=CARTESIAN_POINT('Ctrl Pts',(0.410198932392422,-0.0625250281868314,
0.402940629980001));
#56223=CARTESIAN_POINT('Ctrl Pts',(0.361958615988848,-0.202875588060781,
0.39631949552493));
#56224=CARTESIAN_POINT('Ctrl Pts',(0.265783331451548,-0.290782488832414,
0.389698361069858));
#56225=CARTESIAN_POINT('Ctrl Pts',(0.169608046914247,-0.378689389604048,
0.383077226614787));
#56226=CARTESIAN_POINT('Ctrl Pts',(0.0254977942432194,-0.414152631273365,
0.376456092159716));
#56227=CARTESIAN_POINT('Ctrl Pts',(-0.100488924827274,-0.380916274938763,
0.369834957704645));
#56228=CARTESIAN_POINT('Ctrl Pts',(-0.226475643897767,-0.347679918604161,
0.363213823249574));
#56229=CARTESIAN_POINT('Ctrl Pts',(-0.334338829367725,-0.24574396426564,
0.356592688794503));
#56230=CARTESIAN_POINT('Ctrl Pts',(-0.374635218719989,-0.121834679799224,
0.349971554339432));
#56231=CARTESIAN_POINT('Ctrl Pts',(-0.387324990765207,-0.0828142961013362,
0.347886486960787));
#56232=CARTESIAN_POINT('Ctrl Pts',(-0.393314239859455,-0.0416148420421024,
0.345801419582142));
#56233=CARTESIAN_POINT('Ctrl Pts',(-0.392993347059397,-0.000324654934744872,
0.343716352203497));
#56234=CARTESIAN_POINT('Ctrl Pts',(-0.393037056464261,-0.000335938643299616,
0.325383647796502));
#56235=CARTESIAN_POINT('Ctrl Pts',(-0.393358297788893,-0.0399568453935667,
0.327384980901996));
#56236=CARTESIAN_POINT('Ctrl Pts',(-0.387850028107362,-0.0794904938441846,
0.329386314007491));
#56237=CARTESIAN_POINT('Ctrl Pts',(-0.376143742454461,-0.117094674587401,
0.331387647112986));
#56238=CARTESIAN_POINT('Ctrl Pts',(-0.337415111491167,-0.241502918317571,
0.338008781568057));
#56239=CARTESIAN_POINT('Ctrl Pts',(-0.230847588452996,-0.344792637641065,
0.344629916023128));
#56240=CARTESIAN_POINT('Ctrl Pts',(-0.105290555440245,-0.379617105798059,
0.351251050478199));
#56241=CARTESIAN_POINT('Ctrl Pts',(0.0202664775725054,-0.414441573955053,
0.35787218493327));
#56242=CARTESIAN_POINT('Ctrl Pts',(0.164813020559835,-0.380800790945546,
0.364493319388341));
#56243=CARTESIAN_POINT('Ctrl Pts',(0.262090600311147,-0.294115253540458,
0.371114453843412));
#56244=CARTESIAN_POINT('Ctrl Pts',(0.359368180062459,-0.20742971613537,
0.377735588298483));
#56245=CARTESIAN_POINT('Ctrl Pts',(0.409376796577753,-0.0676994243346997,
0.384356722753555));
#56246=CARTESIAN_POINT('Ctrl Pts',(0.389193057131155,0.0610248135294344,
0.390977857208626));
#56247=CARTESIAN_POINT('Ctrl Pts',(0.369009317684557,0.189749051393568,
0.397598991663697));
#56248=CARTESIAN_POINT('Ctrl Pts',(0.278633222276068,0.307467235321165,
0.404220126118768));
#56249=CARTESIAN_POINT('Ctrl Pts',(0.159492152398559,0.36021870182656,0.410841260573839));
#56250=CARTESIAN_POINT('Ctrl Pts',(0.0403510825210511,0.412970168331956,
0.41746239502891));
#56251=CARTESIAN_POINT('Ctrl Pts',(-0.107554961825477,0.400754917415149,
0.424083529483981));
#56252=CARTESIAN_POINT('Ctrl Pts',(-0.21642753240124,0.329172273420514,
0.430704663939052));
#56253=CARTESIAN_POINT('Ctrl Pts',(-0.324289287986974,0.258254230336771,
0.437264325224869));
#56254=CARTESIAN_POINT('Ctrl Pts',(-0.393839008812417,0.1290660563243,0.443823986510685));
#56255=CARTESIAN_POINT('Ctrl Pts',(-0.39394666710269,-2.26739104671677E-5,
0.450383647796501));
#56256=CARTESIAN_POINT('Origin',(0.,0.,0.93));
#56257=CARTESIAN_POINT('',(-0.393151626951805,0.000355166996054868,0.593716352203497));
#56258=CARTESIAN_POINT('',(-0.393104204086639,0.000348908879909379,0.575383647796501));
#56259=CARTESIAN_POINT('',(-0.3933,-4.81653586104654E-17,0.93));
#56260=CARTESIAN_POINT('Ctrl Pts',(-0.393151626951805,0.000355166996054868,
0.593716352203497));
#56261=CARTESIAN_POINT('Ctrl Pts',(-0.39346294402003,0.0358581068632945,
0.591921699709662));
#56262=CARTESIAN_POINT('Ctrl Pts',(-0.389051359657766,0.0712850359655204,
0.590127047215827));
#56263=CARTESIAN_POINT('Ctrl Pts',(-0.3796098892593,0.105316506102462,0.588332394721991));
#56264=CARTESIAN_POINT('Ctrl Pts',(-0.344776825378376,0.230871141473065,
0.58171126026692));
#56265=CARTESIAN_POINT('Ctrl Pts',(-0.241479768298012,0.337431570529307,
0.575090125811849));
#56266=CARTESIAN_POINT('Ctrl Pts',(-0.11706891599188,0.376151702631086,
0.568468991356778));
#56267=CARTESIAN_POINT('Ctrl Pts',(0.00734193631425342,0.414871834732865,
0.561847856901707));
#56268=CARTESIAN_POINT('Ctrl Pts',(0.152866583846155,0.38575166988018,0.555226722446636));
#56269=CARTESIAN_POINT('Ctrl Pts',(0.252798180691623,0.302139560990116,
0.548605587991565));
#56270=CARTESIAN_POINT('Ctrl Pts',(0.35272977753709,0.218527452100053,0.541984453536493));
#56271=CARTESIAN_POINT('Ctrl Pts',(0.407068323696124,0.0804233991726108,
0.535363319081422));
#56272=CARTESIAN_POINT('Ctrl Pts',(0.390905646644255,-0.0488672682230429,
0.528742184626351));
#56273=CARTESIAN_POINT('Ctrl Pts',(0.374742969592385,-0.178157935618697,
0.52212105017128));
#56274=CARTESIAN_POINT('Ctrl Pts',(0.28807906932961,-0.298635217482562,
0.515499915716209));
#56275=CARTESIAN_POINT('Ctrl Pts',(0.170639693637779,-0.355073695805415,
0.508878781261138));
#56276=CARTESIAN_POINT('Ctrl Pts',(0.0532003179459488,-0.411512174128268,
0.502257646806067));
#56277=CARTESIAN_POINT('Ctrl Pts',(-0.095014533174937,-0.403911848910109,
0.495636512350996));
#56278=CARTESIAN_POINT('Ctrl Pts',(-0.206064855064571,-0.335756623093911,
0.489015377895925));
#56279=CARTESIAN_POINT('Ctrl Pts',(-0.317115176954206,-0.267601397277712,
0.482394243440854));
#56280=CARTESIAN_POINT('Ctrl Pts',(-0.39100096961259,-0.138891270863474,
0.475773108985783));
#56281=CARTESIAN_POINT('Ctrl Pts',(-0.393853824635236,-0.00862550390222436,
0.469151974530712));
#56282=CARTESIAN_POINT('Ctrl Pts',(-0.393916390315514,-0.00576865829944947,
0.469006767088307));
#56283=CARTESIAN_POINT('Ctrl Pts',(-0.393944791681099,-0.00291106448894218,
0.468861559645902));
#56284=CARTESIAN_POINT('Ctrl Pts',(-0.393939358387839,-5.33598371626476E-5,
0.468716352203497));
#56285=CARTESIAN_POINT('Ctrl Pts',(-0.39394666710269,-2.26739104671677E-5,
0.450383647796501));
#56286=CARTESIAN_POINT('Ctrl Pts',(-0.393947676010927,-0.00123241523960264,
0.450445120965756));
#56287=CARTESIAN_POINT('Ctrl Pts',(-0.393942586307364,-0.00244214783528503,
0.45050659413501));
#56288=CARTESIAN_POINT('Ctrl Pts',(-0.39393137237124,-0.00365182365794601,
0.450568067304265));
#56289=CARTESIAN_POINT('Ctrl Pts',(-0.392723544960477,-0.133943239669311,
0.457189201759336));
#56290=CARTESIAN_POINT('Ctrl Pts',(-0.320468793333952,-0.263576034619581,
0.463810336214408));
#56291=CARTESIAN_POINT('Ctrl Pts',(-0.210287875943413,-0.333128009521044,
0.470431470669479));
#56292=CARTESIAN_POINT('Ctrl Pts',(-0.100106958552874,-0.402679984422508,
0.47705260512455));
#56293=CARTESIAN_POINT('Ctrl Pts',(0.0480001246016787,-0.412151139275165,
0.483673739579621));
#56294=CARTESIAN_POINT('Ctrl Pts',(0.166142768855205,-0.357200003114843,
0.490294874034692));
#56295=CARTESIAN_POINT('Ctrl Pts',(0.28428541310873,-0.302248866954521,
0.496916008489763));
#56296=CARTESIAN_POINT('Ctrl Pts',(0.372463618461229,-0.18287543978122,
0.503537142944834));
#56297=CARTESIAN_POINT('Ctrl Pts',(0.390257496673607,-0.0537991456500621,
0.510158277399905));
#56298=CARTESIAN_POINT('Ctrl Pts',(0.408051374885984,0.0752771484810965,
0.516779411854976));
#56299=CARTESIAN_POINT('Ctrl Pts',(0.355460925958238,0.214056309570112,
0.523400546310047));
#56300=CARTESIAN_POINT('Ctrl Pts',(0.256593014598855,0.298923546394139,
0.530021680765118));
#56301=CARTESIAN_POINT('Ctrl Pts',(0.157725103239472,0.383790783218166,
0.536642815220189));
#56302=CARTESIAN_POINT('Ctrl Pts',(0.0125797294484521,0.414746095777205,
0.54326394967526));
#56303=CARTESIAN_POINT('Ctrl Pts',(-0.112310115692326,0.37759992014838,
0.549885084130332));
#56304=CARTESIAN_POINT('Ctrl Pts',(-0.237199960833103,0.340453744519554,
0.556506218585403));
#56305=CARTESIAN_POINT('Ctrl Pts',(-0.341834277323639,0.235206080702865,
0.563127353040474));
#56306=CARTESIAN_POINT('Ctrl Pts',(-0.378249882633598,0.110101262730849,
0.569748487495545));
#56307=CARTESIAN_POINT('Ctrl Pts',(-0.388580829934269,0.0746095752927858,
0.57162687426253));
#56308=CARTESIAN_POINT('Ctrl Pts',(-0.393421317183489,0.0375197205815717,
0.573505261029516));
#56309=CARTESIAN_POINT('Ctrl Pts',(-0.393104204086639,0.000348908879909379,
0.575383647796501));
#56310=CARTESIAN_POINT('Origin',(0.,0.,0.93));
#56311=CARTESIAN_POINT('',(-0.392696669456933,-0.000135344718680625,0.718716352203497));
#56312=CARTESIAN_POINT('',(-0.392715395849333,-0.000160388007437934,0.700383647796502));
#56313=CARTESIAN_POINT('',(-0.3933,-4.81653586104654E-17,0.93));
#56314=CARTESIAN_POINT('Ctrl Pts',(-0.392696669456933,-0.000135344718680625,
0.718716352203497));
#56315=CARTESIAN_POINT('Ctrl Pts',(-0.392468153843407,0.0739588116703239,
0.714981839773422));
#56316=CARTESIAN_POINT('Ctrl Pts',(-0.37234718500379,0.148168078169027,
0.711247327343347));
#56317=CARTESIAN_POINT('Ctrl Pts',(-0.333113602562395,0.210310632800857,
0.707512814913271));
#56318=CARTESIAN_POINT('Ctrl Pts',(-0.263554100656184,0.32048678492325,
0.7008916804582));
#56319=CARTESIAN_POINT('Ctrl Pts',(-0.133916376170864,0.392732666678619,
0.694270546003128));
#56320=CARTESIAN_POINT('Ctrl Pts',(-0.00362488990349993,0.393931586261435,
0.687649411548057));
#56321=CARTESIAN_POINT('Ctrl Pts',(0.126666596363864,0.395130505844251,
0.681028277092986));
#56322=CARTESIAN_POINT('Ctrl Pts',(0.257611844413273,0.325282463254515,
0.674407142637916));
#56323=CARTESIAN_POINT('Ctrl Pts',(0.32918703949367,0.216405008053231,0.667786008182845));
#56324=CARTESIAN_POINT('Ctrl Pts',(0.400762234574067,0.107527552851948,
0.661164873727774));
#56325=CARTESIAN_POINT('Ctrl Pts',(0.412967376685453,-0.0403793149608816,
0.654543739272702));
#56326=CARTESIAN_POINT('Ctrl Pts',(0.360207767279832,-0.159516766743925,
0.647922604817631));
#56327=CARTESIAN_POINT('Ctrl Pts',(0.307448157874211,-0.278654218526967,
0.641301470362559));
#56328=CARTESIAN_POINT('Ctrl Pts',(0.189723796951584,-0.369022254280223,
0.634680335907489));
#56329=CARTESIAN_POINT('Ctrl Pts',(0.0609981947349131,-0.38919719259095,
0.628059201452418));
#56330=CARTESIAN_POINT('Ctrl Pts',(-0.0677274074817583,-0.409372130901677,
0.621438066997347));
#56331=CARTESIAN_POINT('Ctrl Pts',(-0.207454250992473,-0.359353971769874,
0.614816932542275));
#56332=CARTESIAN_POINT('Ctrl Pts',(-0.294133137407089,-0.26207047136149,
0.608195798087204));
#56333=CARTESIAN_POINT('Ctrl Pts',(-0.35731779020926,-0.191155575578438,
0.603369316125968));
#56334=CARTESIAN_POINT('Ctrl Pts',(-0.392314380621845,-0.0951253226411819,
0.598542834164733));
#56335=CARTESIAN_POINT('Ctrl Pts',(-0.393151626951805,0.000355166996054868,
0.593716352203497));
#56336=CARTESIAN_POINT('Ctrl Pts',(-0.393104204086639,0.000348908879909379,
0.575383647796501));
#56337=CARTESIAN_POINT('Ctrl Pts',(-0.392303523719111,-0.0935038504989454,
0.580126395484587));
#56338=CARTESIAN_POINT('Ctrl Pts',(-0.35862239822199,-0.187872722353307,
0.584869143172672));
#56339=CARTESIAN_POINT('Ctrl Pts',(-0.297418747627281,-0.258335731793845,
0.589611890860758));
#56340=CARTESIAN_POINT('Ctrl Pts',(-0.211975113181625,-0.356705936219178,
0.596233025315829));
#56341=CARTESIAN_POINT('Ctrl Pts',(-0.0728909501609335,-0.408484372942498,
0.602854159770901));
#56342=CARTESIAN_POINT('Ctrl Pts',(0.0560791404910008,-0.389936394519486,
0.609475294225972));
#56343=CARTESIAN_POINT('Ctrl Pts',(0.185049231142934,-0.371388416096473,
0.616096428681043));
#56344=CARTESIAN_POINT('Ctrl Pts',(0.303905249426109,-0.282514022527131,
0.622717563136114));
#56345=CARTESIAN_POINT('Ctrl Pts',(0.358164946230055,-0.164052226618296,
0.629338697591185));
#56346=CARTESIAN_POINT('Ctrl Pts',(0.412424643034,-0.0455904307094625,0.635959832046256));
#56347=CARTESIAN_POINT('Ctrl Pts',(0.402088018358715,0.102458767538864,
0.642580966501327));
#56348=CARTESIAN_POINT('Ctrl Pts',(0.331893263579618,0.212231296835213,
0.649202100956398));
#56349=CARTESIAN_POINT('Ctrl Pts',(0.261698508800521,0.322003826131562,
0.655823235411469));
#56350=CARTESIAN_POINT('Ctrl Pts',(0.131645623917614,0.393499686475935,
0.66244436986654));
#56351=CARTESIAN_POINT('Ctrl Pts',(0.00134937453860157,0.393945987357729,
0.669065504321611));
#56352=CARTESIAN_POINT('Ctrl Pts',(-0.12894687484041,0.394392288239522,
0.675686638776682));
#56353=CARTESIAN_POINT('Ctrl Pts',(-0.259486488715526,0.323789029658737,
0.682307773231754));
#56354=CARTESIAN_POINT('Ctrl Pts',(-0.330431590434274,0.214499943611983,
0.688928907686825));
#56355=CARTESIAN_POINT('Ctrl Pts',(-0.37134389973501,0.1514755940344,0.692747154390051));
#56356=CARTESIAN_POINT('Ctrl Pts',(-0.392437770891352,0.0755860887410146,
0.696565401093276));
#56357=CARTESIAN_POINT('Ctrl Pts',(-0.392715395849333,-0.000160388007437934,
0.700383647796502));
#56358=CARTESIAN_POINT('Origin',(0.,0.,0.93));
#56359=CARTESIAN_POINT('',(-0.393648583493532,-0.000293579281448297,0.843716352203497));
#56360=CARTESIAN_POINT('',(-0.393692585105431,-0.000275383461774757,0.825383647796502));
#56361=CARTESIAN_POINT('',(-0.3933,-4.81653586104654E-17,0.93));
#56362=CARTESIAN_POINT('Ctrl Pts',(-0.393648583493532,-0.000293579281448297,
0.843716352203497));
#56363=CARTESIAN_POINT('Ctrl Pts',(-0.392716383215227,0.111596578592595,
0.838041979837182));
#56364=CARTESIAN_POINT('Ctrl Pts',(-0.342624531659322,0.22421618264734,
0.832367607470866));
#56365=CARTESIAN_POINT('Ctrl Pts',(-0.258315374189583,0.297436383010721,
0.826693235104551));
#56366=CARTESIAN_POINT('Ctrl Pts',(-0.159939336918106,0.382873284246015,
0.820072100649479));
#56367=CARTESIAN_POINT('Ctrl Pts',(-0.0149752034932887,0.414666476295674,
0.813450966194408));
#56368=CARTESIAN_POINT('Ctrl Pts',(0.110127113469719,0.378242320953161,
0.806829831739337));
#56369=CARTESIAN_POINT('Ctrl Pts',(0.235229430432725,0.341818165610649,
0.800208697284266));
#56370=CARTESIAN_POINT('Ctrl Pts',(0.340469930933922,0.237176662875967,
0.793587562829195));
#56371=CARTESIAN_POINT('Ctrl Pts',(0.377607564606836,0.112284289341377,
0.786966428374124));
#56372=CARTESIAN_POINT('Ctrl Pts',(0.414745198279751,-0.0126080841932143,
0.780345293919053));
#56373=CARTESIAN_POINT('Ctrl Pts',(0.383779965124383,-0.157751328527715,
0.773724159463982));
#56374=CARTESIAN_POINT('Ctrl Pts',(0.29890597639204,-0.256613428639898,
0.767103025008911));
#56375=CARTESIAN_POINT('Ctrl Pts',(0.214031987659696,-0.355475528752083,
0.760481890553839));
#56376=CARTESIAN_POINT('Ctrl Pts',(0.0752492433503761,-0.408056484641949,
0.753860756098768));
#56377=CARTESIAN_POINT('Ctrl Pts',(-0.0538258224982624,-0.390253783214973,
0.747239621643697));
#56378=CARTESIAN_POINT('Ctrl Pts',(-0.182900888346899,-0.372451081787997,
0.740618487188626));
#56379=CARTESIAN_POINT('Ctrl Pts',(-0.302268275734855,-0.284264723044181,
0.733997352733555));
#56380=CARTESIAN_POINT('Ctrl Pts',(-0.357211329765281,-0.166118332427566,
0.727376218278484));
#56381=CARTESIAN_POINT('Ctrl Pts',(-0.381164903123588,-0.114609942794055,
0.724489596253488));
#56382=CARTESIAN_POINT('Ctrl Pts',(-0.392873302475408,-0.0574070308519249,
0.721602974228493));
#56383=CARTESIAN_POINT('Ctrl Pts',(-0.392696669456933,-0.000135344718680625,
0.718716352203497));
#56384=CARTESIAN_POINT('Ctrl Pts',(-0.392715395849333,-0.000160388007437934,
0.700383647796502));
#56385=CARTESIAN_POINT('Ctrl Pts',(-0.392919193994087,-0.0557641476451545,
0.703186535548347));
#56386=CARTESIAN_POINT('Ctrl Pts',(-0.381905756157218,-0.11129083359123,
0.705989423300192));
#56387=CARTESIAN_POINT('Ctrl Pts',(-0.359280377758478,-0.161594776908665,
0.708792311052037));
#56388=CARTESIAN_POINT('Ctrl Pts',(-0.305833473801554,-0.28042549786984,
0.715413445507108));
#56389=CARTESIAN_POINT('Ctrl Pts',(-0.187589076325322,-0.370112026279464,
0.72203457996218));
#56390=CARTESIAN_POINT('Ctrl Pts',(-0.0587490744031055,-0.389543075953546,
0.728655714417251));
#56391=CARTESIAN_POINT('Ctrl Pts',(0.0700909275191088,-0.408974125627628,
0.735276848872322));
#56392=CARTESIAN_POINT('Ctrl Pts',(0.209526533887308,-0.35814969656617,
0.741897983327393));
#56393=CARTESIAN_POINT('Ctrl Pts',(0.295642046109568,-0.260367129912076,
0.748519117782464));
#56394=CARTESIAN_POINT('Ctrl Pts',(0.381757558331829,-0.162584563257981,
0.755140252237535));
#56395=CARTESIAN_POINT('Ctrl Pts',(0.414552976408151,-0.0178438590112496,
0.761761386692606));
#56396=CARTESIAN_POINT('Ctrl Pts',(0.378995253102251,0.107507487611169,
0.768382521147677));
#56397=CARTESIAN_POINT('Ctrl Pts',(0.343437529796352,0.232858834233588,
0.775003655602749));
#56398=CARTESIAN_POINT('Ctrl Pts',(0.239526665108231,0.338820823231692,
0.78162479005782));
#56399=CARTESIAN_POINT('Ctrl Pts',(0.114894219446364,0.376821682104857,
0.788245924512891));
#56400=CARTESIAN_POINT('Ctrl Pts',(-0.00973822621550149,0.414822540978021,
0.794867058967962));
#56401=CARTESIAN_POINT('Ctrl Pts',(-0.155092252851112,0.384862269726245,
0.801488193423032));
#56402=CARTESIAN_POINT('Ctrl Pts',(-0.254539225224928,0.30067431647616,
0.808109327878103));
#56403=CARTESIAN_POINT('Ctrl Pts',(-0.341023841386423,0.227459791705242,
0.813867434517569));
#56404=CARTESIAN_POINT('Ctrl Pts',(-0.392788913023703,0.113232824514289,
0.819625541157036));
#56405=CARTESIAN_POINT('Ctrl Pts',(-0.393692585105431,-0.000275383461774757,
0.825383647796502));
#56406=CARTESIAN_POINT('Origin',(0.,0.,0.93));
#56407=CARTESIAN_POINT('',(-0.393623414358295,0.000302776322228852,0.968716352203497));
#56408=CARTESIAN_POINT('',(-0.393576675000574,0.000317769076113512,0.950383647796502));
#56409=CARTESIAN_POINT('',(-0.3933,-4.81653586104654E-17,0.93));
#56410=CARTESIAN_POINT('Ctrl Pts',(-0.393623414358295,0.000302776322228852,
0.968716352203497));
#56411=CARTESIAN_POINT('Ctrl Pts',(-0.393790054855682,0.0198884434456063,
0.967723254356012));
#56412=CARTESIAN_POINT('Ctrl Pts',(-0.392454790325599,0.0394513098675264,
0.966730156508528));
#56413=CARTESIAN_POINT('Ctrl Pts',(-0.389539024169359,0.0587757018706559,
0.965737058661043));
#56414=CARTESIAN_POINT('Ctrl Pts',(-0.370099167554116,0.187614363679551,
0.959115924205972));
#56415=CARTESIAN_POINT('Ctrl Pts',(-0.280404562957203,0.305852618684086,
0.952494789750901));
#56416=CARTESIAN_POINT('Ctrl Pts',(-0.161570198594696,0.359291393450046,
0.94587365529583));
#56417=CARTESIAN_POINT('Ctrl Pts',(-0.0427358342321878,0.412730168216006,
0.939252520840759));
#56418=CARTESIAN_POINT('Ctrl Pts',(0.105238289895915,0.401369462743389,
0.932631386385688));
#56419=CARTESIAN_POINT('Ctrl Pts',(0.214522515616161,0.330416895413838,
0.926010251930617));
#56420=CARTESIAN_POINT('Ctrl Pts',(0.323806741336407,0.259464328084287,
0.919389117475546));
#56421=CARTESIAN_POINT('Ctrl Pts',(0.394401068648798,0.128919898897802,
0.912767983020475));
#56422=CARTESIAN_POINT('Ctrl Pts',(0.393945859550417,-0.00137630820971424,
0.906146848565404));
#56423=CARTESIAN_POINT('Ctrl Pts',(0.393490650452036,-0.131672515317231,
0.899525714110333));
#56424=CARTESIAN_POINT('Ctrl Pts',(0.321985904942885,-0.261720500345779,
0.892904579655261));
#56425=CARTESIAN_POINT('Ctrl Pts',(0.212208586388978,-0.331907743724061,
0.88628344520019));
#56426=CARTESIAN_POINT('Ctrl Pts',(0.102431267835071,-0.402094987102343,
0.879662310745119));
#56427=CARTESIAN_POINT('Ctrl Pts',(-0.0456186237635904,-0.412421488830358,
0.873041176290049));
#56428=CARTESIAN_POINT('Ctrl Pts',(-0.164076699285435,-0.358153697779043,
0.866420041834977));
#56429=CARTESIAN_POINT('Ctrl Pts',(-0.282534774807279,-0.303885906727728,
0.859798907379906));
#56430=CARTESIAN_POINT('Ctrl Pts',(-0.371401034252306,-0.185023822897081,
0.853177772924835));
#56431=CARTESIAN_POINT('Ctrl Pts',(-0.389940193415752,-0.056052475771292,
0.846556638469764));
#56432=CARTESIAN_POINT('Ctrl Pts',(-0.392591124788987,-0.0376107445509109,
0.845609876381008));
#56433=CARTESIAN_POINT('Ctrl Pts',(-0.393804119969754,-0.0189623152651601,
0.844663114292253));
#56434=CARTESIAN_POINT('Ctrl Pts',(-0.393648583493532,-0.000293579281448297,
0.843716352203497));
#56435=CARTESIAN_POINT('Ctrl Pts',(-0.393692585105431,-0.000275383461774757,
0.825383647796502));
#56436=CARTESIAN_POINT('Ctrl Pts',(-0.39382802791529,-0.0172880487207719,
0.826246675612107));
#56437=CARTESIAN_POINT('Ctrl Pts',(-0.392820912119232,-0.034284567657927,
0.827109703427712));
#56438=CARTESIAN_POINT('Ctrl Pts',(-0.390616889073419,-0.0511244338562125,
0.827972731243317));
#56439=CARTESIAN_POINT('Ctrl Pts',(-0.373707662436067,-0.180319595690092,
0.834593865698388));
#56440=CARTESIAN_POINT('Ctrl Pts',(-0.286349291049343,-0.300294284109454,
0.841215000153459));
#56441=CARTESIAN_POINT('Ctrl Pts',(-0.168585860354973,-0.356053464320865,
0.84783613460853));
#56442=CARTESIAN_POINT('Ctrl Pts',(-0.0508224296606021,-0.411812644532276,
0.854457269063601));
#56443=CARTESIAN_POINT('Ctrl Pts',(0.0973460603414153,-0.403356316535735,
0.861078403518672));
#56444=CARTESIAN_POINT('Ctrl Pts',(0.208000856368157,-0.334560765058647,
0.867699537973743));
#56445=CARTESIAN_POINT('Ctrl Pts',(0.318655652394899,-0.265765213581559,
0.874320672428815));
#56446=CARTESIAN_POINT('Ctrl Pts',(0.391796754446365,-0.136630438623923,
0.880941806883886));
#56447=CARTESIAN_POINT('Ctrl Pts',(0.393897111899264,-0.00635035463052729,
0.887562941338957));
#56448=CARTESIAN_POINT('Ctrl Pts',(0.395997469352162,0.123929729362869,
0.894184075794028));
#56449=CARTESIAN_POINT('Ctrl Pts',(0.327057082206493,0.255355122392025,
0.900805210249099));
#56450=CARTESIAN_POINT('Ctrl Pts',(0.21867744107414,0.327681916699382,0.90742634470417));
#56451=CARTESIAN_POINT('Ctrl Pts',(0.110297799941786,0.40000871100674,0.914047479159241));
#56452=CARTESIAN_POINT('Ctrl Pts',(-0.0375210951772516,0.413236906592297,
0.920668613614312));
#56453=CARTESIAN_POINT('Ctrl Pts',(-0.157020741324571,0.36130284881301,
0.927289748069384));
#56454=CARTESIAN_POINT('Ctrl Pts',(-0.276520387471888,0.309368791033724,
0.933910882524455));
#56455=CARTESIAN_POINT('Ctrl Pts',(-0.367700784647487,0.192272479889591,
0.940532016979525));
#56456=CARTESIAN_POINT('Ctrl Pts',(-0.388765874189203,0.0636895347166177,
0.947153151434597));
#56457=CARTESIAN_POINT('Ctrl Pts',(-0.392191807493608,0.0427773713301666,
0.948229983555232));
#56458=CARTESIAN_POINT('Ctrl Pts',(-0.39376316737147,0.0215613826172752,
0.949306815675866));
#56459=CARTESIAN_POINT('Ctrl Pts',(-0.393576675000574,0.000317769076113512,
0.950383647796502));
#56460=CARTESIAN_POINT('Origin',(0.,0.,0.93));
#56461=CARTESIAN_POINT('',(-0.392687717376401,0.000121152120971441,1.0937163522035));
#56462=CARTESIAN_POINT('',(-0.392674134765212,9.49958190125592E-5,1.0753836477965));
#56463=CARTESIAN_POINT('',(-0.3933,-4.81653586104654E-17,0.93));
#56464=CARTESIAN_POINT('Ctrl Pts',(-0.392687717376401,0.000121152120971441,
1.0937163522035));
#56465=CARTESIAN_POINT('Ctrl Pts',(-0.392848158650017,0.0583154695936899,
1.09078339441977));
#56466=CARTESIAN_POINT('Ctrl Pts',(-0.380745062692883,0.116446324066143,
1.08785043663605));
#56467=CARTESIAN_POINT('Ctrl Pts',(-0.356041906099905,0.168610188250716,
1.08491747885232));
#56468=CARTESIAN_POINT('Ctrl Pts',(-0.300274679522556,0.286369796104153,
1.07829634439725));
#56469=CARTESIAN_POINT('Ctrl Pts',(-0.180294029303511,0.373719957027504,
1.07167520994218));
#56470=CARTESIAN_POINT('Ctrl Pts',(-0.051097723057459,0.390620349162146,
1.06505407548711));
#56471=CARTESIAN_POINT('Ctrl Pts',(0.0780985831885896,0.407520741296788,
1.05843294103204));
#56472=CARTESIAN_POINT('Ctrl Pts',(0.216510545461646,0.353971364642725,
1.05181180657697));
#56473=CARTESIAN_POINT('Ctrl Pts',(0.300691691999046,0.254518645375842,
1.0451906721219));
#56474=CARTESIAN_POINT('Ctrl Pts',(0.384872838536448,0.155065926108957,
1.03856953766683));
#56475=CARTESIAN_POINT('Ctrl Pts',(0.414823169338192,0.00970986422925148,
1.03194840321175));
#56476=CARTESIAN_POINT('Ctrl Pts',(0.376813792867102,-0.114919972094987,
1.02532726875668));
#56477=CARTESIAN_POINT('Ctrl Pts',(0.338804416396012,-0.239549808419227,
1.01870613430161));
#56478=CARTESIAN_POINT('Ctrl Pts',(0.232835332652085,-0.343453419187998,
1.01208499984654));
#56479=CARTESIAN_POINT('Ctrl Pts',(0.107481566286803,-0.379002569107047,
1.00546386539147));
#56480=CARTESIAN_POINT('Ctrl Pts',(-0.0178722000784767,-0.414551719026095,
0.998842730936399));
#56481=CARTESIAN_POINT('Ctrl Pts',(-0.162610649065111,-0.381746408095422,
0.992221596481328));
#56482=CARTESIAN_POINT('Ctrl Pts',(-0.260387319241642,-0.295624218323459,
0.985600462026257));
#56483=CARTESIAN_POINT('Ctrl Pts',(-0.343498556878564,-0.222419416329008,
0.97997242541867));
#56484=CARTESIAN_POINT('Ctrl Pts',(-0.392679037304232,-0.110692179344585,
0.974344388811084));
#56485=CARTESIAN_POINT('Ctrl Pts',(-0.393623414358295,0.000302776322228852,
0.968716352203497));
#56486=CARTESIAN_POINT('Ctrl Pts',(-0.393576675000574,0.000317769076113512,
0.950383647796502));
#56487=CARTESIAN_POINT('Ctrl Pts',(-0.392616478821894,-0.109059555291462,
0.955927950130938));
#56488=CARTESIAN_POINT('Ctrl Pts',(-0.345056898727053,-0.219169193753748,
0.961472252465374));
#56489=CARTESIAN_POINT('Ctrl Pts',(-0.264099282894184,-0.292312898349171,
0.96701655479981));
#56490=CARTESIAN_POINT('Ctrl Pts',(-0.167417820149611,-0.379662807040174,
0.973637689254881));
#56491=CARTESIAN_POINT('Ctrl Pts',(-0.0231051127526314,-0.414293045220361,
0.980258823709952));
#56492=CARTESIAN_POINT('Ctrl Pts',(0.102687532975472,-0.380329504953174,
0.986879958165023));
#56493=CARTESIAN_POINT('Ctrl Pts',(0.228480178703574,-0.346365964685987,
0.993501092620094));
#56494=CARTESIAN_POINT('Ctrl Pts',(0.335752762762798,-0.243808645971423,
1.00012222707516));
#56495=CARTESIAN_POINT('Ctrl Pts',(0.375332750759084,-0.119668659113963,
1.00674336153024));
#56496=CARTESIAN_POINT('Ctrl Pts',(0.414912738755369,0.00447132774349662,
1.01336449598531));
#56497=CARTESIAN_POINT('Ctrl Pts',(0.386800130688718,0.150193982743854,
1.01998563044038));
#56498=CARTESIAN_POINT('Ctrl Pts',(0.303881426862889,0.250701695595161,
1.02660676489545));
#56499=CARTESIAN_POINT('Ctrl Pts',(0.22096272303706,0.351209408446469,1.03322789935052));
#56500=CARTESIAN_POINT('Ctrl Pts',(0.0832379234520517,0.406502179148727,
1.03984903380559));
#56501=CARTESIAN_POINT('Ctrl Pts',(-0.0461614877025709,0.391234429491579,
1.04647016826066));
#56502=CARTESIAN_POINT('Ctrl Pts',(-0.175560898857193,0.375966679834431,
1.05309130271573));
#56503=CARTESIAN_POINT('Ctrl Pts',(-0.296634921581431,0.290138409817877,
1.0597124371708));
#56504=CARTESIAN_POINT('Ctrl Pts',(-0.353884598720045,0.173092323790705,
1.06633357162588));
#56505=CARTESIAN_POINT('Ctrl Pts',(-0.379968443936397,0.119764302678541,
1.06935026368275));
#56506=CARTESIAN_POINT('Ctrl Pts',(-0.392803276473094,0.059955913669758,
1.07236695573963));
#56507=CARTESIAN_POINT('Ctrl Pts',(-0.392674134765212,9.49958190125592E-5,
1.0753836477965));
#56508=CARTESIAN_POINT('Origin',(0.,0.,0.93));
#56509=CARTESIAN_POINT('',(-0.393178387374057,-0.000357709694404185,1.2187163522035));
#56510=CARTESIAN_POINT('',(-0.393227518215404,-0.000360608651032692,1.2003836477965));
#56511=CARTESIAN_POINT('',(-0.3933,-4.81653586104654E-17,0.93));
#56512=CARTESIAN_POINT('Ctrl Pts',(-0.393178387374057,-0.000357709694404185,
1.2187163522035));
#56513=CARTESIAN_POINT('Ctrl Pts',(-0.392322385109892,0.0960227493030975,
1.21384353448353));
#56514=CARTESIAN_POINT('Ctrl Pts',(-0.356584758291295,0.192971013585422,
1.20897071676357));
#56515=CARTESIAN_POINT('Ctrl Pts',(-0.292294815698811,0.264119244274569,
1.2040978990436));
#56516=CARTESIAN_POINT('Ctrl Pts',(-0.204938304850977,0.360794726245326,
1.19747676458853));
#56517=CARTESIAN_POINT('Ctrl Pts',(-0.0648653847631109,0.409835363460394,
1.19085563013346));
#56518=CARTESIAN_POINT('Ctrl Pts',(0.0637161086015447,0.388761484700158,
1.18423449567839));
#56519=CARTESIAN_POINT('Ctrl Pts',(0.192297601966202,0.367687605939922,
1.17761336122332));
#56520=CARTESIAN_POINT('Ctrl Pts',(0.309387668607649,0.27649921120438,1.17099222676825));
#56521=CARTESIAN_POINT('Ctrl Pts',(0.361313551598668,0.156996025148134,
1.16437109231318));
#56522=CARTESIAN_POINT('Ctrl Pts',(0.413239434589687,0.037492839091888,
1.1577499578581));
#56523=CARTESIAN_POINT('Ctrl Pts',(0.400001133930281,-0.11032513828506,
1.15112882340303));
#56524=CARTESIAN_POINT('Ctrl Pts',(0.327666936314771,-0.218699824707789,
1.14450768894796));
#56525=CARTESIAN_POINT('Ctrl Pts',(0.255332738699263,-0.327074511130518,
1.13788655449289));
#56526=CARTESIAN_POINT('Ctrl Pts',(0.123902644127651,-0.396005906599026,
1.13126542003782));
#56527=CARTESIAN_POINT('Ctrl Pts',(-0.00637728450892158,-0.393896642183651,
1.12464428558275));
#56528=CARTESIAN_POINT('Ctrl Pts',(-0.136657213145495,-0.391787377768276,
1.11802315112768));
#56529=CARTESIAN_POINT('Ctrl Pts',(-0.26578697584703,-0.318637453469018,
1.11140201667261));
#56530=CARTESIAN_POINT('Ctrl Pts',(-0.33457495572997,-0.207977963927629,
1.10478088221754));
#56531=CARTESIAN_POINT('Ctrl Pts',(-0.372891988014216,-0.146337205752564,
1.10109270554619));
#56532=CARTESIAN_POINT('Ctrl Pts',(-0.392485963445352,-0.0730578500790584,
1.09740452887484));
#56533=CARTESIAN_POINT('Ctrl Pts',(-0.392687717376401,0.000121152120971441,
1.0937163522035));
#56534=CARTESIAN_POINT('Ctrl Pts',(-0.392674134765212,9.49958190125592E-5,
1.0753836477965));
#56535=CARTESIAN_POINT('Ctrl Pts',(-0.392519832026156,-0.0714287879243111,
1.0789880901947));
#56536=CARTESIAN_POINT('Ctrl Pts',(-0.373857832359423,-0.143027563168594,
1.08259253259289));
#56537=CARTESIAN_POINT('Ctrl Pts',(-0.337174346736183,-0.203736893246021,
1.08619697499109));
#56538=CARTESIAN_POINT('Ctrl Pts',(-0.269789086060714,-0.315256122217786,
1.09281810944616));
#56539=CARTESIAN_POINT('Ctrl Pts',(-0.141593233156782,-0.390030678123524,
1.09943924390123));
#56540=CARTESIAN_POINT('Ctrl Pts',(-0.0113503112617354,-0.393784753641865,
1.1060603783563));
#56541=CARTESIAN_POINT('Ctrl Pts',(0.11889261063331,-0.397538829160207,
1.11268151281137));
#56542=CARTESIAN_POINT('Ctrl Pts',(0.25118260151947,-0.330272424291154,
1.11930264726645));
#56543=CARTESIAN_POINT('Ctrl Pts',(0.32487943179952,-0.222819695180042,
1.12592378172152));
#56544=CARTESIAN_POINT('Ctrl Pts',(0.398576262079569,-0.115366966068929,
1.13254491617659));
#56545=CARTESIAN_POINT('Ctrl Pts',(0.413679931753507,0.0322720872842442,
1.13916605063166));
#56546=CARTESIAN_POINT('Ctrl Pts',(0.363267090153202,0.152421399344478,
1.14578718508673));
#56547=CARTESIAN_POINT('Ctrl Pts',(0.312854248552898,0.272570711404711,
1.1524083195418));
#56548=CARTESIAN_POINT('Ctrl Pts',(0.196924895678351,0.365230282172005,
1.15902945399687));
#56549=CARTESIAN_POINT('Ctrl Pts',(0.0686197304462398,0.387926016606333,
1.16565058845194));
#56550=CARTESIAN_POINT('Ctrl Pts',(-0.0596854347858714,0.410621751040662,
1.17227172290701));
#56551=CARTESIAN_POINT('Ctrl Pts',(-0.200366412375547,0.363353649142024,
1.17889285736209));
#56552=CARTESIAN_POINT('Ctrl Pts',(-0.28893663970491,0.26778887206617,1.18551399181716));
#56553=CARTESIAN_POINT('Ctrl Pts',(-0.355239920476351,0.196249502264644,
1.19047054381027));
#56554=CARTESIAN_POINT('Ctrl Pts',(-0.392340579448797,0.0976449005809497,
1.19542709580339));
#56555=CARTESIAN_POINT('Ctrl Pts',(-0.393227518215404,-0.000360608651032693,
1.2003836477965));
#56556=CARTESIAN_POINT('Origin',(0.,0.,0.93));
#56557=CARTESIAN_POINT('',(-0.393932958190319,7.01566447607431E-5,1.3437163522035));
#56558=CARTESIAN_POINT('',(-0.393917393671661,0.000100014571609002,1.3253836477965));
#56559=CARTESIAN_POINT('',(-0.3933,-4.81653586104654E-17,0.93));
#56560=CARTESIAN_POINT('Ctrl Pts',(-0.393932958190319,7.01566447607431E-5,
1.3437163522035));
#56561=CARTESIAN_POINT('Ctrl Pts',(-0.393942224805097,0.00383992058097464,
1.34352480900236));
#56562=CARTESIAN_POINT('Ctrl Pts',(-0.393892801581458,0.00760943545943395,
1.34333326580123));
#56563=CARTESIAN_POINT('Ctrl Pts',(-0.393783942110804,0.0113772331014927,
1.3431417226001));
#56564=CARTESIAN_POINT('Ctrl Pts',(-0.390020962335796,0.141619886663971,
1.33652058814502));
#56565=CARTESIAN_POINT('Ctrl Pts',(-0.31523764848855,0.269810615534473,
1.32989945368995));
#56566=CARTESIAN_POINT('Ctrl Pts',(-0.20371382249242,0.337188245598414,
1.32327831923488));
#56567=CARTESIAN_POINT('Ctrl Pts',(-0.0921899964962896,0.404565875662355,
1.31665718477981));
#56568=CARTESIAN_POINT('Ctrl Pts',(0.0560743416487236,0.411130406919734,
1.31003605032474));
#56569=CARTESIAN_POINT('Ctrl Pts',(0.173116502991226,0.353872732616968,
1.30341491586967));
#56570=CARTESIAN_POINT('Ctrl Pts',(0.290158664333728,0.296615058314203,
1.2967937814146));
#56571=CARTESIAN_POINT('Ctrl Pts',(0.375978648873719,0.175535178451293,
1.29017264695953));
#56572=CARTESIAN_POINT('Ctrl Pts',(0.391237550214167,0.0461347351175119,
1.28355151250445));
#56573=CARTESIAN_POINT('Ctrl Pts',(0.406496451554614,-0.0832657082162682,
1.27693037804938));
#56574=CARTESIAN_POINT('Ctrl Pts',(0.351194269695518,-0.220986715020921,
1.27030924359431));
#56575=CARTESIAN_POINT('Ctrl Pts',(0.250680896823328,-0.303898539720326,
1.26368810913924));
#56576=CARTESIAN_POINT('Ctrl Pts',(0.150167523951137,-0.386810364419732,
1.25706697468417));
#56577=CARTESIAN_POINT('Ctrl Pts',(0.00444296006585079,-0.414913007013892,
1.2504458402291));
#56578=CARTESIAN_POINT('Ctrl Pts',(-0.119694309533929,-0.375324535234475,
1.24382470577403));
#56579=CARTESIAN_POINT('Ctrl Pts',(-0.243831579133704,-0.335736063455059,
1.23720357131896));
#56580=CARTESIAN_POINT('Ctrl Pts',(-0.346381554447974,-0.228456477302072,
1.23058243686389));
#56581=CARTESIAN_POINT('Ctrl Pts',(-0.38033649130121,-0.102661520862356,
1.22396130240882));
#56582=CARTESIAN_POINT('Ctrl Pts',(-0.389302324081501,-0.0694452451579606,
1.22221298567371));
#56583=CARTESIAN_POINT('Ctrl Pts',(-0.393485512156828,-0.0349380242241585,
1.2204646689386));
#56584=CARTESIAN_POINT('Ctrl Pts',(-0.393178387374057,-0.000357709694404185,
1.2187163522035));
#56585=CARTESIAN_POINT('Ctrl Pts',(-0.393227518215404,-0.000360608651032693,
1.2003836477965));
#56586=CARTESIAN_POINT('Ctrl Pts',(-0.393525383085535,-0.0332742655781063,
1.20204823025846));
#56587=CARTESIAN_POINT('Ctrl Pts',(-0.389738883964958,-0.0661203538703375,
1.20371281272041));
#56588=CARTESIAN_POINT('Ctrl Pts',(-0.381602460640826,-0.0978510286064153,
1.20537739518237));
#56589=CARTESIAN_POINT('Ctrl Pts',(-0.349238577178329,-0.22406469995007,
1.21199852963744));
#56590=CARTESIAN_POINT('Ctrl Pts',(-0.248051333184284,-0.332630590384309,
1.21861966409251));
#56591=CARTESIAN_POINT('Ctrl Pts',(-0.124423812269278,-0.373783328557174,
1.22524079854758));
#56592=CARTESIAN_POINT('Ctrl Pts',(-0.000796291354272574,-0.414936066730039,
1.23186193300265));
#56593=CARTESIAN_POINT('Ctrl Pts',(0.145271506481696,-0.388675652641532,
1.23848306745772));
#56594=CARTESIAN_POINT('Ctrl Pts',(0.246823761390213,-0.307039561911936,
1.2451042019128));
#56595=CARTESIAN_POINT('Ctrl Pts',(0.348376016298731,-0.225403471182339,
1.25172533636787));
#56596=CARTESIAN_POINT('Ctrl Pts',(0.405412728279798,-0.0883917038116555,
1.25834647082294));
#56597=CARTESIAN_POINT('Ctrl Pts',(0.391788916244076,0.0411911018873178,
1.26496760527801));
#56598=CARTESIAN_POINT('Ctrl Pts',(0.378165104208354,0.17077390758629,1.27158873973308));
#56599=CARTESIAN_POINT('Ctrl Pts',(0.293880768155842,0.292927751613551,
1.27820987418815));
#56600=CARTESIAN_POINT('Ctrl Pts',(0.177570890638771,0.351658698977885,
1.28483100864322));
#56601=CARTESIAN_POINT('Ctrl Pts',(0.0612610131216984,0.41038964634222,
1.29145214309829));
#56602=CARTESIAN_POINT('Ctrl Pts',(-0.0870744058599348,0.405697697043627,
1.29807327755336));
#56603=CARTESIAN_POINT('Ctrl Pts',(-0.199440094675204,0.339733587385156,
1.30469441200844));
#56604=CARTESIAN_POINT('Ctrl Pts',(-0.311805783490471,0.273769477726686,
1.31131554646351));
#56605=CARTESIAN_POINT('Ctrl Pts',(-0.388201742139376,0.14653320770834,
1.31793668091858));
#56606=CARTESIAN_POINT('Ctrl Pts',(-0.393608930693719,0.0163484386228601,
1.32455781537365));
#56607=CARTESIAN_POINT('Ctrl Pts',(-0.393833737668765,0.010935931949371,
1.32483309284793));
#56608=CARTESIAN_POINT('Ctrl Pts',(-0.393935838534097,0.00551832871131889,
1.32510837032222));
#56609=CARTESIAN_POINT('Ctrl Pts',(-0.393917393671661,0.000100014571609002,
1.3253836477965));
#56610=CARTESIAN_POINT('Origin',(0.,0.,0.93));
#56611=CARTESIAN_POINT('',(-0.392969983056837,0.000317581071747716,1.4687163522035));
#56612=CARTESIAN_POINT('',(-0.39292938619043,0.000303368867518512,1.4503836477965));
#56613=CARTESIAN_POINT('',(-0.3933,-4.81653586104654E-17,0.93));
#56614=CARTESIAN_POINT('Ctrl Pts',(-0.392969983056837,0.000317581071747716,
1.4687163522035));
#56615=CARTESIAN_POINT('Ctrl Pts',(-0.393289547738009,0.0425316776590403,
1.46658494906612));
#56616=CARTESIAN_POINT('Ctrl Pts',(-0.387024947442207,0.0846534505080271,
1.46445354592875));
#56617=CARTESIAN_POINT('Ctrl Pts',(-0.373774788945001,0.124449361011914,
1.46232214279137));
#56618=CARTESIAN_POINT('Ctrl Pts',(-0.332613602953188,0.24807406137376,
1.4557010083363));
#56619=CARTESIAN_POINT('Ctrl Pts',(-0.224040802499859,0.349253864537994,
1.44907987388123));
#56620=CARTESIAN_POINT('Ctrl Pts',(-0.0978249294402324,0.381609113761947,
1.44245873942616));
#56621=CARTESIAN_POINT('Ctrl Pts',(0.0283909436193927,0.4139643629859,1.43583760497109));
#56622=CARTESIAN_POINT('Ctrl Pts',(0.172249889285313,0.377495058269573,
1.42921647051602));
#56623=CARTESIAN_POINT('Ctrl Pts',(0.267808602042126,0.288918306379673,
1.42259533606095));
#56624=CARTESIAN_POINT('Ctrl Pts',(0.363367314798942,0.20034155448977,1.41597420160588));
#56625=CARTESIAN_POINT('Ctrl Pts',(0.410625794646646,0.0596573554262853,
1.40935306715081));
#56626=CARTESIAN_POINT('Ctrl Pts',(0.387921290244053,-0.0686462471308959,
1.40273193269574));
#56627=CARTESIAN_POINT('Ctrl Pts',(0.36521678584146,-0.196949849688075,
1.39611079824066));
#56628=CARTESIAN_POINT('Ctrl Pts',(0.272549297188576,-0.312872855738954,
1.38948966378559));
#56629=CARTESIAN_POINT('Ctrl Pts',(0.152396549224293,-0.36327747796107,
1.38286852933052));
#56630=CARTESIAN_POINT('Ctrl Pts',(0.0322438012600084,-0.413682100183186,
1.37624739487545));
#56631=CARTESIAN_POINT('Ctrl Pts',(-0.115394206015674,-0.398568338576538,
1.36962626042038));
#56632=CARTESIAN_POINT('Ctrl Pts',(-0.222841886802131,-0.324864168645985,
1.36300512596531));
#56633=CARTESIAN_POINT('Ctrl Pts',(-0.327181207099616,-0.253292191127661,
1.35657553471137));
#56634=CARTESIAN_POINT('Ctrl Pts',(-0.393621902799281,-0.126470702493874,
1.35014594345743));
#56635=CARTESIAN_POINT('Ctrl Pts',(-0.393932958190319,7.01566447607431E-5,
1.3437163522035));
#56636=CARTESIAN_POINT('Ctrl Pts',(-0.393917393671661,0.000100014571609002,
1.3253836477965));
#56637=CARTESIAN_POINT('Ctrl Pts',(-0.393492191938935,-0.124806124940763,
1.33172950477729));
#56638=CARTESIAN_POINT('Ctrl Pts',(-0.329006385569408,-0.25009005295616,
1.33807536175808));
#56639=CARTESIAN_POINT('Ctrl Pts',(-0.22692603833899,-0.322024587425646,
1.34442121873886));
#56640=CARTESIAN_POINT('Ctrl Pts',(-0.12041753897014,-0.397079576236056,
1.35104235319393));
#56641=CARTESIAN_POINT('Ctrl Pts',(0.0270178782273391,-0.414056285704261,
1.357663487649));
#56642=CARTESIAN_POINT('Ctrl Pts',(0.147797492224514,-0.365172785160562,
1.36428462210407));
#56643=CARTESIAN_POINT('Ctrl Pts',(0.268577106221691,-0.316289284616863,
1.37090575655915));
#56644=CARTESIAN_POINT('Ctrl Pts',(0.36270091701856,-0.20154557406126,1.37752689101422));
#56645=CARTESIAN_POINT('Ctrl Pts',(0.387023638563781,-0.073538867107662,
1.38414802546929));
#56646=CARTESIAN_POINT('Ctrl Pts',(0.411346360109002,0.0544678398459324,
1.39076915992436));
#56647=CARTESIAN_POINT('Ctrl Pts',(0.365867992402574,0.195737543197524,
1.39739029437943));
#56648=CARTESIAN_POINT('Ctrl Pts',(0.27143530278721,0.285513814497535,1.4040114288345));
#56649=CARTESIAN_POINT('Ctrl Pts',(0.177002613171845,0.375290085797548,
1.41063256328957));
#56650=CARTESIAN_POINT('Ctrl Pts',(0.0336156016475434,0.413572925045984,
1.41725369774464));
#56651=CARTESIAN_POINT('Ctrl Pts',(-0.0929987539746983,0.382813914657498,
1.42387483219972));
#56652=CARTESIAN_POINT('Ctrl Pts',(-0.21961310959694,0.352054904269012,
1.43049596665479));
#56653=CARTESIAN_POINT('Ctrl Pts',(-0.32945480931712,0.252254044243605,
1.43711710110986));
#56654=CARTESIAN_POINT('Ctrl Pts',(-0.372173665230652,0.129158913215852,
1.44373823556493));
#56655=CARTESIAN_POINT('Ctrl Pts',(-0.386465496413208,0.0879767515117977,
1.44595337297545));
#56656=CARTESIAN_POINT('Ctrl Pts',(-0.393244440240979,0.0441873219369639,
1.44816851038598));
#56657=CARTESIAN_POINT('Ctrl Pts',(-0.39292938619043,0.000303368867518512,
1.4503836477965));
#56658=CARTESIAN_POINT('Origin',(0.,0.,0.93));
#56659=CARTESIAN_POINT('',(-0.392790597751209,-0.000230484700094208,1.5937163522035));
#56660=CARTESIAN_POINT('',(-0.392821510739754,-0.000250701325252446,1.5753836477965));
#56661=CARTESIAN_POINT('',(-0.3933,-4.81653586104654E-17,0.93));
#56662=CARTESIAN_POINT('Ctrl Pts',(-0.392790597751209,-0.000230484700094208,
1.5937163522035));
#56663=CARTESIAN_POINT('Ctrl Pts',(-0.392361248393127,0.0804967654600471,
1.58964508912988));
#56664=CARTESIAN_POINT('Ctrl Pts',(-0.368164027480674,0.161460390358751,
1.58557382605627));
#56665=CARTESIAN_POINT('Ctrl Pts',(-0.322009087387059,0.226948266830839,
1.58150256298265));
#56666=CARTESIAN_POINT('Ctrl Pts',(-0.246946862568883,0.333451832790243,
1.57488142852758));
#56667=CARTESIAN_POINT('Ctrl Pts',(-0.113809037324264,0.399023853241257,
1.56826029407251));
#56668=CARTESIAN_POINT('Ctrl Pts',(0.0163753707382398,0.393607656210794,
1.56163915961744));
#56669=CARTESIAN_POINT('Ctrl Pts',(0.146559778800742,0.388191459180332,
1.55501802516237));
#56670=CARTESIAN_POINT('Ctrl Pts',(0.273790769681132,0.311787044668395,
1.5483968907073));
#56671=CARTESIAN_POINT('Ctrl Pts',(0.339747180380717,0.199416912588678,
1.54177575625223));
#56672=CARTESIAN_POINT('Ctrl Pts',(0.405703591080302,0.0870467805089601,
1.53515462179716));
#56673=CARTESIAN_POINT('Ctrl Pts',(0.410385421599083,-0.0612890691385343,
1.52853348734209));
#56674=CARTESIAN_POINT('Ctrl Pts',(0.351646533070016,-0.177594950249301,
1.52191235288702));
#56675=CARTESIAN_POINT('Ctrl Pts',(0.292907644540948,-0.293900831360069,
1.51529121843194));
#56676=CARTESIAN_POINT('Ctrl Pts',(0.170748036964027,-0.378176743934104,
1.50867008397687));
#56677=CARTESIAN_POINT('Ctrl Pts',(0.0411643086114815,-0.391791679881239,
1.5020489495218));
#56678=CARTESIAN_POINT('Ctrl Pts',(-0.0884194197410625,-0.405406615828374,
1.49542781506673));
#56679=CARTESIAN_POINT('Ctrl Pts',(-0.225427268869233,-0.348360575148612,
1.48880668061166));
#56680=CARTESIAN_POINT('Ctrl Pts',(-0.30705640766817,-0.246802756029003,
1.48218554615659));
#56681=CARTESIAN_POINT('Ctrl Pts',(-0.362408387512275,-0.177937318519413,
1.47769581483889));
#56682=CARTESIAN_POINT('Ctrl Pts',(-0.392296830459881,-0.0886050390430537,
1.47320608352119));
#56683=CARTESIAN_POINT('Ctrl Pts',(-0.392969983056837,0.000317581071747716,
1.4687163522035));
#56684=CARTESIAN_POINT('Ctrl Pts',(-0.39292938619043,0.000303368867518512,
1.4503836477965));
#56685=CARTESIAN_POINT('Ctrl Pts',(-0.392302731063306,-0.0869835717115683,
1.45478964484105));
#56686=CARTESIAN_POINT('Ctrl Pts',(-0.363610231497499,-0.174644473735395,
1.4591956418856));
#56687=CARTESIAN_POINT('Ctrl Pts',(-0.310148212606042,-0.242906048890095,
1.46360163893014));
#56688=CARTESIAN_POINT('Ctrl Pts',(-0.229807891961015,-0.345486477938193,
1.47022277338521));
#56689=CARTESIAN_POINT('Ctrl Pts',(-0.0935312385640766,-0.404257934004288,
1.47684390784028));
#56690=CARTESIAN_POINT('Ctrl Pts',(0.0362140774032489,-0.392280257494778,
1.48346504229536));
#56691=CARTESIAN_POINT('Ctrl Pts',(0.165959393370574,-0.380302580985268,
1.49008617675043));
#56692=CARTESIAN_POINT('Ctrl Pts',(0.289173371908287,-0.297575771900155,
1.4967073112055));
#56693=CARTESIAN_POINT('Ctrl Pts',(0.349376123956583,-0.182020843846168,
1.50332844566057));
#56694=CARTESIAN_POINT('Ctrl Pts',(0.409578876004877,-0.0664659157921843,
1.50994958011564));
#56695=CARTESIAN_POINT('Ctrl Pts',(0.406770401563758,0.0819171312306699,
1.51657071457071));
#56696=CARTESIAN_POINT('Ctrl Pts',(0.342238074307365,0.195111162240944,
1.52319184902578));
#56697=CARTESIAN_POINT('Ctrl Pts',(0.277705747050971,0.30830519325122,1.52981298348085));
#56698=CARTESIAN_POINT('Ctrl Pts',(0.151449566979302,0.386310208248916,
1.53643411793592));
#56699=CARTESIAN_POINT('Ctrl Pts',(0.0213439316380748,0.393369653966392,
1.54305525239099));
#56700=CARTESIAN_POINT('Ctrl Pts',(-0.108761703703154,0.400429099683869,
1.54967638684607));
#56701=CARTESIAN_POINT('Ctrl Pts',(-0.24271679431394,0.336542976121126,
1.55629752130114));
#56702=CARTESIAN_POINT('Ctrl Pts',(-0.319117844548307,0.230995842160026,
1.56291865575621));
#56703=CARTESIAN_POINT('Ctrl Pts',(-0.367062220722499,0.164761261886383,
1.56707365310297));
#56704=CARTESIAN_POINT('Ctrl Pts',(-0.392341764890002,0.0821205388687718,
1.57122865044974));
#56705=CARTESIAN_POINT('Ctrl Pts',(-0.392821510739754,-0.000250701325252446,
1.5753836477965));
#56706=CARTESIAN_POINT('Origin',(0.,0.,0.93));
#56707=CARTESIAN_POINT('',(-0.393805363403874,-0.000235004724456311,1.7187163522035));
#56708=CARTESIAN_POINT('',(-0.393842938295855,-0.000187384875455676,1.7003836477965));
#56709=CARTESIAN_POINT('',(-0.3933,-4.81653586104654E-17,0.93));
#56710=CARTESIAN_POINT('Ctrl Pts',(-0.393805363403874,-0.000235004724456311,
1.7187163522035));
#56711=CARTESIAN_POINT('Ctrl Pts',(-0.393042182615986,0.118159669343525,
1.71270522919364));
#56712=CARTESIAN_POINT('Ctrl Pts',(-0.336019807553631,0.237234833307885,
1.70669410618379));
#56713=CARTESIAN_POINT('Ctrl Pts',(-0.242886995036645,0.310176314488843,
1.70068298317393));
#56714=CARTESIAN_POINT('Ctrl Pts',(-0.140303023149369,0.390519929726693,
1.69406184871886));
#56715=CARTESIAN_POINT('Ctrl Pts',(0.00609226823398873,0.414891431126435,
1.68744071426379));
#56716=CARTESIAN_POINT('Ctrl Pts',(0.129185480108729,0.372158787137547,
1.68081957980872));
#56717=CARTESIAN_POINT('Ctrl Pts',(0.252278691983468,0.329426143148659,
1.67419844535365));
#56718=CARTESIAN_POINT('Ctrl Pts',(0.35206982434959,0.219589353771141,1.66757731089858));
#56719=CARTESIAN_POINT('Ctrl Pts',(0.382819647158814,0.0929757105602073,
1.66095617644351));
#56720=CARTESIAN_POINT('Ctrl Pts',(0.413569469968039,-0.0336379326507284,
1.65433504198844));
#56721=CARTESIAN_POINT('Ctrl Pts',(0.375277983220365,-0.177028429695081,
1.64771390753337));
#56722=CARTESIAN_POINT('Ctrl Pts',(0.285495539318975,-0.271456435539926,
1.64109277307829));
#56723=CARTESIAN_POINT('Ctrl Pts',(0.195713095417587,-0.365884441384768,
1.63447163862322));
#56724=CARTESIAN_POINT('Ctrl Pts',(0.0544396943624859,-0.411349956030106,
1.62785050416815));
#56725=CARTESIAN_POINT('Ctrl Pts',(-0.0735654818810781,-0.387017721917561,
1.62122936971308));
#56726=CARTESIAN_POINT('Ctrl Pts',(-0.201570658124644,-0.362685487805017,
1.61460823525801));
#56727=CARTESIAN_POINT('Ctrl Pts',(-0.316307609556672,-0.268555504934587,
1.60798710080294));
#56728=CARTESIAN_POINT('Ctrl Pts',(-0.36518277307682,-0.147772957765475,
1.60136596634787));
#56729=CARTESIAN_POINT('Ctrl Pts',(-0.384005133741704,-0.101258276256465,
1.59881609496641));
#56730=CARTESIAN_POINT('Ctrl Pts',(-0.393059503400641,-0.0507907411033471,
1.59626622358496));
#56731=CARTESIAN_POINT('Ctrl Pts',(-0.392790597751209,-0.000230484700094208,
1.5937163522035));
#56732=CARTESIAN_POINT('Ctrl Pts',(-0.392821510739754,-0.000250701325252446,
1.5753836477965));
#56733=CARTESIAN_POINT('Ctrl Pts',(-0.393106256780218,-0.0491409304027429,
1.57784978490481));
#56734=CARTESIAN_POINT('Ctrl Pts',(-0.38465443035242,-0.0979362249897565,
1.58031592201311));
#56735=CARTESIAN_POINT('Ctrl Pts',(-0.367019625039806,-0.143149829246245,
1.58278205912142));
#56736=CARTESIAN_POINT('Ctrl Pts',(-0.319673345438989,-0.264540222331967,
1.58940319357649));
#56737=CARTESIAN_POINT('Ctrl Pts',(-0.206133776379406,-0.360112864143958,
1.59602432803156));
#56738=CARTESIAN_POINT('Ctrl Pts',(-0.0784461550906783,-0.386058762652492,
1.60264546248663));
#56739=CARTESIAN_POINT('Ctrl Pts',(0.0492414661980497,-0.412004661161027,
1.60926659694171));
#56740=CARTESIAN_POINT('Ctrl Pts',(0.191077139715923,-0.368323816366105,
1.61588773139678));
#56741=CARTESIAN_POINT('Ctrl Pts',(0.282044980480955,-0.275038222919274,
1.62250886585185));
#56742=CARTESIAN_POINT('Ctrl Pts',(0.373012821245988,-0.181752629472443,
1.62913000030692));
#56743=CARTESIAN_POINT('Ctrl Pts',(0.41311282925818,-0.038862287373702,
1.63575113476199));
#56744=CARTESIAN_POINT('Ctrl Pts',(0.3839636600404,0.0881319427418194,1.64237226921706));
#56745=CARTESIAN_POINT('Ctrl Pts',(0.354814490822621,0.215126172857341,
1.64899340367213));
#56746=CARTESIAN_POINT('Ctrl Pts',(0.256416144374869,0.326224290989643,
1.6556145381272));
#56747=CARTESIAN_POINT('Ctrl Pts',(0.133873221284828,0.370503154207164,
1.66223567258227));
#56748=CARTESIAN_POINT('Ctrl Pts',(0.0113302981947858,0.414782017424686,
1.66885680703735));
#56749=CARTESIAN_POINT('Ctrl Pts',(-0.135357201537546,0.392241625727427,
1.67547794149242));
#56750=CARTESIAN_POINT('Ctrl Pts',(-0.238949232579617,0.313208538429519,
1.68209907594749));
#56751=CARTESIAN_POINT('Ctrl Pts',(-0.334307308924747,0.240457351909347,
1.68819393323049));
#56752=CARTESIAN_POINT('Ctrl Pts',(-0.393148487536621,0.119837142250066,
1.6942887905135));
#56753=CARTESIAN_POINT('Ctrl Pts',(-0.393842938295855,-0.000187384875455676,
1.7003836477965));
#56754=CARTESIAN_POINT('Origin',(0.,0.,-0.177777344927309));
#56755=CARTESIAN_POINT('',(-0.322689101172091,-0.000192565846880319,1.75972265507269));
#56756=CARTESIAN_POINT('',(-0.322321068793906,0.000363350312672553,1.78437734492731));
#56757=CARTESIAN_POINT('',(-0.322275,-2.94787261092574E-14,-0.177777344927309));
#56758=CARTESIAN_POINT('',(0.141600127780395,-0.29010115152588,1.8));
#56759=CARTESIAN_POINT('Ctrl Pts',(-0.322689101172091,-0.000192565846880313,
1.75972265507269));
#56760=CARTESIAN_POINT('Ctrl Pts',(-0.322752562984035,-0.0100375995009947,
1.76033266651791));
#56761=CARTESIAN_POINT('Ctrl Pts',(-0.317877158043228,-0.126673691476083,
1.76756381241819));
#56762=CARTESIAN_POINT('Ctrl Pts',(-0.180463403516937,-0.331269943931176,
1.78098959406063));
#56763=CARTESIAN_POINT('Ctrl Pts',(0.051569323594053,-0.333511267780158,
1.79380536425785));
#56764=CARTESIAN_POINT('Ctrl Pts',(0.141603157807413,-0.290105179958813,
1.8));
#56765=CARTESIAN_POINT('',(-0.227909696623847,-0.227855976023948,1.8));
#56766=CARTESIAN_POINT('Origin',(0.,0.,1.8));
#56767=CARTESIAN_POINT('Ctrl Pts',(-0.322321068793906,0.000363350312672563,
1.78437734492731));
#56768=CARTESIAN_POINT('Ctrl Pts',(-0.321520973335343,-0.0836845372725092,
1.78958489661821));
#56769=CARTESIAN_POINT('Ctrl Pts',(-0.287553299275345,-0.168198311462947,
1.7947924483091));
#56770=CARTESIAN_POINT('Ctrl Pts',(-0.227909696623847,-0.227855976023948,
1.8));
#56771=CARTESIAN_POINT('Origin',(0.,0.,-0.177777344927309));
#56772=CARTESIAN_POINT('',(-0.321857589347244,-0.000188862081689614,1.63472265507269));
#56773=CARTESIAN_POINT('',(-0.322719890514358,-0.000153545539665345,1.65937734492731));
#56774=CARTESIAN_POINT('',(-0.322275,-2.94787261092574E-14,-0.177777344927309));
#56775=CARTESIAN_POINT('Ctrl Pts',(-0.321857589347244,-0.000188862081689604,
1.63472265507269));
#56776=CARTESIAN_POINT('Ctrl Pts',(-0.322077934041294,-0.0416185763770278,
1.63727252645415));
#56777=CARTESIAN_POINT('Ctrl Pts',(-0.295393402245107,-0.190353673042667,
1.64644353229068));
#56778=CARTESIAN_POINT('Ctrl Pts',(-0.0711526387601384,-0.374320380910067,
1.66223567258227));
#56779=CARTESIAN_POINT('Ctrl Pts',(0.276131002163078,-0.262555325743576,
1.68209907594749));
#56780=CARTESIAN_POINT('Ctrl Pts',(0.370260589436959,0.089932640960989,
1.7019624793127));
#56781=CARTESIAN_POINT('Ctrl Pts',(0.124950237161653,0.359937608898739,
1.72182588267791));
#56782=CARTESIAN_POINT('Ctrl Pts',(-0.223872369623273,0.301866542751815,
1.74107927459791));
#56783=CARTESIAN_POINT('Ctrl Pts',(-0.322063741171035,0.0968215292084443,
1.75371153206284));
#56784=CARTESIAN_POINT('Ctrl Pts',(-0.322689101172091,-0.000192565846880313,
1.75972265507269));
#56785=CARTESIAN_POINT('Ctrl Pts',(-0.322719890514358,-0.000153545539665285,
1.65937734492731));
#56786=CARTESIAN_POINT('Ctrl Pts',(-0.322769025984903,-0.00864581304597595,
1.65990362209938));
#56787=CARTESIAN_POINT('Ctrl Pts',(-0.318611706634757,-0.12393053953812,
1.66705103372651));
#56788=CARTESIAN_POINT('Ctrl Pts',(-0.18032609112216,-0.335634029399439,
1.68081957980872));
#56789=CARTESIAN_POINT('Ctrl Pts',(0.184494543087876,-0.333417375353118,
1.70068298317393));
#56790=CARTESIAN_POINT('Ctrl Pts',(0.380171112467216,-0.0254013260161302,
1.72054638653915));
#56791=CARTESIAN_POINT('Ctrl Pts',(0.227322355071844,0.305652478161549,
1.74040978990436));
#56792=CARTESIAN_POINT('Ctrl Pts',(-0.133942736176479,0.356974128119761,
1.76027319326957));
#56793=CARTESIAN_POINT('Ctrl Pts',(-0.309881561511554,0.152660167939229,
1.77492904494389));
#56794=CARTESIAN_POINT('Ctrl Pts',(-0.322538253608777,0.023178034123378,
1.78296376216314));
#56795=CARTESIAN_POINT('Ctrl Pts',(-0.322321068793906,0.000363350312672563,
1.78437734492731));
#56796=CARTESIAN_POINT('Origin',(0.,0.,-0.177777344927309));
#56797=CARTESIAN_POINT('',(-0.322004579938068,0.000260229951415816,1.50972265507269));
#56798=CARTESIAN_POINT('',(-0.321882919841481,-0.000205427840351907,1.53437734492731));
#56799=CARTESIAN_POINT('',(-0.322275,-2.94787261092574E-14,-0.177777344927309));
#56800=CARTESIAN_POINT('Ctrl Pts',(-0.322004579938068,0.000260229951415825,
1.50972265507269));
#56801=CARTESIAN_POINT('Ctrl Pts',(-0.3214529901766,-0.0726040909168692,
1.51421238639039));
#56802=CARTESIAN_POINT('Ctrl Pts',(-0.26084449369421,-0.253754214926255,
1.52532325216316));
#56803=CARTESIAN_POINT('Ctrl Pts',(0.039813974270868,-0.378939562359927,
1.54305525239099));
#56804=CARTESIAN_POINT('Ctrl Pts',(0.340111362004286,-0.171769312742865,
1.56291865575621));
#56805=CARTESIAN_POINT('Ctrl Pts',(0.328602308377735,0.192875507586258,
1.58278205912142));
#56806=CARTESIAN_POINT('Ctrl Pts',(0.0158382535647818,0.380695741658215,
1.60264546248663));
#56807=CARTESIAN_POINT('Ctrl Pts',(-0.269432596141516,0.240196330941153,
1.61995899447039));
#56808=CARTESIAN_POINT('Ctrl Pts',(-0.321505775046774,0.065960068875241,
1.63065139199908));
#56809=CARTESIAN_POINT('Ctrl Pts',(-0.321857589347244,-0.000188862081689604,
1.63472265507269));
#56810=CARTESIAN_POINT('Ctrl Pts',(-0.321882919841481,-0.000205427840351873,
1.53437734492731));
#56811=CARTESIAN_POINT('Ctrl Pts',(-0.322116244352512,-0.0402667005989179,
1.53684348203562));
#56812=CARTESIAN_POINT('Ctrl Pts',(-0.296596899030457,-0.187598639238989,
1.54593075359899));
#56813=CARTESIAN_POINT('Ctrl Pts',(-0.0758728659140442,-0.373394473511197,
1.56163915961744));
#56814=CARTESIAN_POINT('Ctrl Pts',(0.272792974535782,-0.26601656156395,
1.58150256298265));
#56815=CARTESIAN_POINT('Ctrl Pts',(0.37136833748108,0.0852419052542959,
1.60136596634787));
#56816=CARTESIAN_POINT('Ctrl Pts',(0.129481784457052,0.358347519450231,
1.62122936971308));
#56817=CARTESIAN_POINT('Ctrl Pts',(-0.221557160855253,0.304405940632871,
1.64056649590623));
#56818=CARTESIAN_POINT('Ctrl Pts',(-0.322150848769053,0.0981960717483616,
1.65328248764431));
#56819=CARTESIAN_POINT('Ctrl Pts',(-0.322719890514358,-0.000153545539665285,
1.65937734492731));
#56820=CARTESIAN_POINT('Origin',(0.,0.,-0.177777344927309));
#56821=CARTESIAN_POINT('',(-0.322793653955721,5.74872430323103E-5,1.38472265507269));
#56822=CARTESIAN_POINT('',(-0.321971314351693,0.000248584291295761,1.40937734492731));
#56823=CARTESIAN_POINT('',(-0.322275,-2.94787261092574E-14,-0.177777344927309));
#56824=CARTESIAN_POINT('Ctrl Pts',(-0.322793653955721,5.74872430323201E-5,
1.38472265507269));
#56825=CARTESIAN_POINT('Ctrl Pts',(-0.322538771229688,-0.103631695006911,
1.39115224632663));
#56826=CARTESIAN_POINT('Ctrl Pts',(-0.212032190958281,-0.314565804986716,
1.40420297203564));
#56827=CARTESIAN_POINT('Ctrl Pts',(0.147397431593805,-0.351360758602383,
1.42387483219971));
#56828=CARTESIAN_POINT('Ctrl Pts',(0.375196172292565,-0.0663944216454938,
1.44373823556493));
#56829=CARTESIAN_POINT('Ctrl Pts',(0.259023581957562,0.279440820560319,
1.46360163893014));
#56830=CARTESIAN_POINT('Ctrl Pts',(-0.0946159429431672,0.369091050746847,
1.48346504229536));
#56831=CARTESIAN_POINT('Ctrl Pts',(-0.301186735501589,0.176586187251814,
1.49883871434287));
#56832=CARTESIAN_POINT('Ctrl Pts',(-0.322266435284178,0.034850995213737,
1.50759125193532));
#56833=CARTESIAN_POINT('Ctrl Pts',(-0.322004579938068,0.000260229951415825,
1.50972265507269));
#56834=CARTESIAN_POINT('Ctrl Pts',(-0.321971314351693,0.000248584291295775,
1.40937734492731));
#56835=CARTESIAN_POINT('Ctrl Pts',(-0.321457825205757,-0.0712754400542971,
1.41378334197186));
#56836=CARTESIAN_POINT('Ctrl Pts',(-0.262615556824558,-0.251049471647208,
1.42481047347147));
#56837=CARTESIAN_POINT('Ctrl Pts',(0.0350261341603416,-0.379412145143482,
1.44245873942616));
#56838=CARTESIAN_POINT('Ctrl Pts',(0.3379154166412,-0.176049960567548,1.46232214279137));
#56839=CARTESIAN_POINT('Ctrl Pts',(0.331011518086569,0.18871088214253,1.48218554615659));
#56840=CARTESIAN_POINT('Ctrl Pts',(0.0206437802330401,0.380465773129421,
1.5020489495218));
#56841=CARTESIAN_POINT('Ctrl Pts',(-0.267766340380685,0.242916654852083,
1.51944621577871));
#56842=CARTESIAN_POINT('Ctrl Pts',(-0.321489810017616,0.0672906093667012,
1.53022234758055));
#56843=CARTESIAN_POINT('Ctrl Pts',(-0.321882919841481,-0.000205427840351873,
1.53437734492731));
#56844=CARTESIAN_POINT('Origin',(0.,0.,-0.177777344927309));
#56845=CARTESIAN_POINT('',(-0.322175349074432,-0.000293111852957028,1.25972265507269));
#56846=CARTESIAN_POINT('',(-0.322780900192053,8.19532063371861E-5,1.28437734492731));
#56847=CARTESIAN_POINT('',(-0.322275,-2.94787261092574E-14,-0.177777344927309));
#56848=CARTESIAN_POINT('Ctrl Pts',(-0.322175349074432,-0.00029311185295702,
1.25972265507269));
#56849=CARTESIAN_POINT('Ctrl Pts',(-0.322427011010276,-0.0286286594376897,
1.2614709718078));
#56850=CARTESIAN_POINT('Ctrl Pts',(-0.306017829170326,-0.163988402508686,
1.26984042299797));
#56851=CARTESIAN_POINT('Ctrl Pts',(-0.115767935090022,-0.363012632792868,
1.28483100864322));
#56852=CARTESIAN_POINT('Ctrl Pts',(0.242457723385417,-0.293929649253331,
1.30469441200844));
#56853=CARTESIAN_POINT('Ctrl Pts',(0.378403647555055,0.0446213611812189,
1.32455781537365));
#56854=CARTESIAN_POINT('Ctrl Pts',(0.167437701577738,0.342264521233232,
1.34442121873886));
#56855=CARTESIAN_POINT('Ctrl Pts',(-0.197031326459517,0.326127341134279,
1.36428462210407));
#56856=CARTESIAN_POINT('Ctrl Pts',(-0.321360841411568,0.113006387783977,
1.37771843421535));
#56857=CARTESIAN_POINT('Ctrl Pts',(-0.322801247137205,0.00314647954545929,
1.38453111187156));
#56858=CARTESIAN_POINT('Ctrl Pts',(-0.322793653955721,5.74872430323201E-5,
1.38472265507269));
#56859=CARTESIAN_POINT('Ctrl Pts',(-0.322780900192053,8.195320633718E-5,
1.28437734492731));
#56860=CARTESIAN_POINT('Ctrl Pts',(-0.322432484508304,-0.102267719082872,
1.2907232019081));
#56861=CARTESIAN_POINT('Ctrl Pts',(-0.214459339993708,-0.312039456873427,
1.30369019334395));
#56862=CARTESIAN_POINT('Ctrl Pts',(0.142949239214434,-0.353193894022897,
1.32327831923488));
#56863=CARTESIAN_POINT('Ctrl Pts',(0.374327966327785,-0.0711265460495382,
1.3431417226001));
#56864=CARTESIAN_POINT('Ctrl Pts',(0.262531315278285,0.276148005038436,
1.36300512596531));
#56865=CARTESIAN_POINT('Ctrl Pts',(-0.0899480831884954,0.370256334701204,
1.38286852933052));
#56866=CARTESIAN_POINT('Ctrl Pts',(-0.300071343759289,0.179340842955076,
1.39832593565119));
#56867=CARTESIAN_POINT('Ctrl Pts',(-0.322229473629959,0.0362076510989722,
1.40716220751679));
#56868=CARTESIAN_POINT('Ctrl Pts',(-0.321971314351693,0.000248584291295775,
1.40937734492731));
#56869=CARTESIAN_POINT('Origin',(0.,0.,-0.177777344927309));
#56870=CARTESIAN_POINT('',(-0.321773287865446,9.92735819440501E-5,1.13472265507269));
#56871=CARTESIAN_POINT('',(-0.322215607507932,-0.000295487294752678,1.15937734492731));
#56872=CARTESIAN_POINT('',(-0.322275,-2.94787261092574E-14,-0.177777344927309));
#56873=CARTESIAN_POINT('Ctrl Pts',(-0.321773287865446,9.92735819440732E-5,
1.13472265507269));
#56874=CARTESIAN_POINT('Ctrl Pts',(-0.321607968139714,-0.0598645274198684,
1.13841083174404));
#56875=CARTESIAN_POINT('Ctrl Pts',(-0.276728969333462,-0.227707144521845,
1.14872014287045));
#56876=CARTESIAN_POINT('Ctrl Pts',(-0.00616808820702852,-0.380975512392104,
1.16565058845194));
#56877=CARTESIAN_POINT('Ctrl Pts',(0.316918362807963,-0.211525737604811,
1.18551399181716));
#56878=CARTESIAN_POINT('Ctrl Pts',(0.349461256362576,0.151846029436811,
1.20537739518237));
#56879=CARTESIAN_POINT('Ctrl Pts',(0.0616260067296811,0.376008805282698,
1.22524079854758));
#56880=CARTESIAN_POINT('Ctrl Pts',(-0.252399453807821,0.266066007796539,
1.24335588517769));
#56881=CARTESIAN_POINT('Ctrl Pts',(-0.3214739299804,0.0786822566276443,
1.25484983735273));
#56882=CARTESIAN_POINT('Ctrl Pts',(-0.322175349074432,-0.00029311185295702,
1.25972265507269));
#56883=CARTESIAN_POINT('Ctrl Pts',(-0.322215607507932,-0.000295487294752667,
1.15937734492731));
#56884=CARTESIAN_POINT('Ctrl Pts',(-0.322459681754105,-0.0272653545364726,
1.16104192738927));
#56885=CARTESIAN_POINT('Ctrl Pts',(-0.307015485637393,-0.161236448440899,
1.16932764430629));
#56886=CARTESIAN_POINT('Ctrl Pts',(-0.120342294288793,-0.361521982852271,
1.18423449567839));
#56887=CARTESIAN_POINT('Ctrl Pts',(0.238727114922392,-0.296967635404715,
1.2040978990436));
#56888=CARTESIAN_POINT('Ctrl Pts',(0.378936926926189,0.0398398957118962,
1.22396130240882));
#56889=CARTESIAN_POINT('Ctrl Pts',(0.171745970394351,0.34012311526861,1.24382470577403));
#56890=CARTESIAN_POINT('Ctrl Pts',(-0.192897791255575,0.328589187273149,
1.26368810913924));
#56891=CARTESIAN_POINT('Ctrl Pts',(-0.320700046313691,0.115736537458778,
1.27720565552367));
#56892=CARTESIAN_POINT('Ctrl Pts',(-0.322796014145884,0.00452178841960592,
1.28410206745303));
#56893=CARTESIAN_POINT('Ctrl Pts',(-0.322780900192053,8.195320633718E-5,
1.28437734492731));
#56894=CARTESIAN_POINT('Origin',(0.,0.,-0.177777344927309));
#56895=CARTESIAN_POINT('',(-0.322540009820288,0.000248098752203224,1.00972265507269));
#56896=CARTESIAN_POINT('',(-0.321762158101853,7.78407769116696E-5,1.03437734492731));
#56897=CARTESIAN_POINT('',(-0.322275,-2.94787261092574E-14,-0.177777344927309));
#56898=CARTESIAN_POINT('Ctrl Pts',(-0.322540009820288,0.000248098752203227,
1.00972265507269));
#56899=CARTESIAN_POINT('Ctrl Pts',(-0.321766175304399,-0.0907025733493005,
1.01535069168028));
#56900=CARTESIAN_POINT('Ctrl Pts',(-0.234056960396757,-0.289958622799939,
1.02759986274293));
#56901=CARTESIAN_POINT('Ctrl Pts',(0.103955810747213,-0.366570014821552,
1.04647016826066));
#56902=CARTESIAN_POINT('Ctrl Pts',(0.364453037776757,-0.111150211919144,
1.06633357162588));
#56903=CARTESIAN_POINT('Ctrl Pts',(0.290827996898553,0.246169580928165,
1.08619697499109));
#56904=CARTESIAN_POINT('Ctrl Pts',(-0.0494215465152554,0.377806692760261,
1.1060603783563));
#56905=CARTESIAN_POINT('Ctrl Pts',(-0.289598786989554,0.202949158922468,
1.12223560505017));
#56906=CARTESIAN_POINT('Ctrl Pts',(-0.32190475547657,0.04778443418078,1.13178969728897));
#56907=CARTESIAN_POINT('Ctrl Pts',(-0.321773287865446,9.92735819440732E-5,
1.13472265507269));
#56908=CARTESIAN_POINT('Ctrl Pts',(-0.321762158101853,7.78407769116314E-5,
1.03437734492731));
#56909=CARTESIAN_POINT('Ctrl Pts',(-0.321635720483669,-0.058529653262946,
1.03798178732551));
#56910=CARTESIAN_POINT('Ctrl Pts',(-0.278253620036456,-0.224969762308773,
1.04820736417877));
#56911=CARTESIAN_POINT('Ctrl Pts',(-0.0109779830180157,-0.380867294169285,
1.06505407548711));
#56912=CARTESIAN_POINT('Ctrl Pts',(0.314222297781658,-0.215510462520356,
1.08491747885232));
#56913=CARTESIAN_POINT('Ctrl Pts',(0.351350712306201,0.147421466689362,
1.10478088221754));
#56914=CARTESIAN_POINT('Ctrl Pts',(0.066368773346284,0.375200743340994,
1.12464428558275));
#56915=CARTESIAN_POINT('Ctrl Pts',(-0.250477710614327,0.268741916094579,
1.14284310648601));
#56916=CARTESIAN_POINT('Ctrl Pts',(-0.321488838652084,0.0800114679245235,
1.15442079293419));
#56917=CARTESIAN_POINT('Ctrl Pts',(-0.322215607507932,-0.000295487294752667,
1.15937734492731));
#56918=CARTESIAN_POINT('Origin',(0.,0.,-0.177777344927309));
#56919=CARTESIAN_POINT('',(-0.322560633728396,-0.000240562580560466,0.884722655072691));
#56920=CARTESIAN_POINT('',(-0.322501710998753,0.000260384004555324,0.90937734492731));
#56921=CARTESIAN_POINT('',(-0.322275,-2.94787261092574E-14,-0.177777344927309));
#56922=CARTESIAN_POINT('Ctrl Pts',(-0.322560633728396,-0.000240562580560428,
0.884722655072691));
#56923=CARTESIAN_POINT('Ctrl Pts',(-0.322688082286428,-0.0155379612308262,
0.885669417161446));
#56924=CARTESIAN_POINT('Ctrl Pts',(-0.31474304255412,-0.137683963102499,
0.893237313705273));
#56925=CARTESIAN_POINT('Ctrl Pts',(-0.158694433735999,-0.346405056336641,
0.90742634470417));
#56926=CARTESIAN_POINT('Ctrl Pts',(0.205247433654992,-0.321020057523545,
0.927289748069383));
#56927=CARTESIAN_POINT('Ctrl Pts',(0.381023115264154,-0.00133116068848917,
0.947153151434597));
#56928=CARTESIAN_POINT('Ctrl Pts',(0.207485458249651,0.319578114033663,
0.96701655479981));
#56929=CARTESIAN_POINT('Ctrl Pts',(-0.156270154667085,0.347505431777269,
0.986879958165023));
#56930=CARTESIAN_POINT('Ctrl Pts',(-0.314287675546238,0.139201754952349,
1.00111532492265));
#56931=CARTESIAN_POINT('Ctrl Pts',(-0.322676557153865,0.016296842388581,
1.00872955722521));
#56932=CARTESIAN_POINT('Ctrl Pts',(-0.322540009820288,0.000248098752203227,
1.00972265507269));
#56933=CARTESIAN_POINT('Ctrl Pts',(-0.322501710998753,0.000260384004555341,
0.90937734492731));
#56934=CARTESIAN_POINT('Ctrl Pts',(-0.321714914091844,-0.0893647805277536,
0.914921647261746));
#56935=CARTESIAN_POINT('Ctrl Pts',(-0.236204012765627,-0.287339077416759,
0.927087084051252));
#56936=CARTESIAN_POINT('Ctrl Pts',(0.0993190377930615,-0.367853422725428,
0.945873655295831));
#56937=CARTESIAN_POINT('Ctrl Pts',(0.363020578812783,-0.115743126091287,
0.965737058661042));
#56938=CARTESIAN_POINT('Ctrl Pts',(0.293913097770214,0.242477839890713,
0.985600462026258));
#56939=CARTESIAN_POINT('Ctrl Pts',(-0.0446472362210804,0.378400629197116,
1.00546386539147));
#56940=CARTESIAN_POINT('Ctrl Pts',(-0.288267845035054,0.20570020243003,
1.02172282635849));
#56941=CARTESIAN_POINT('Ctrl Pts',(-0.3218679784525,0.0491286348281514,
1.03136065287044));
#56942=CARTESIAN_POINT('Ctrl Pts',(-0.321762158101853,7.78407769116314E-5,
1.03437734492731));
#56943=CARTESIAN_POINT('Origin',(0.,0.,-0.177777344927309));
#56944=CARTESIAN_POINT('',(-0.321780623313585,-0.000110903176248464,0.759722655072691));
#56945=CARTESIAN_POINT('',(-0.322596689206338,-0.000225652695543505,0.78437734492731));
#56946=CARTESIAN_POINT('',(-0.322275,-2.94787261092574E-14,-0.177777344927309));
#56947=CARTESIAN_POINT('Ctrl Pts',(-0.321780623313585,-0.000110903176248449,
0.759722655072691));
#56948=CARTESIAN_POINT('Ctrl Pts',(-0.321925358645465,-0.0470400479730705,
0.762609277097686));
#56949=CARTESIAN_POINT('Ctrl Pts',(-0.290325268145637,-0.201426411122161,
0.772117033577752));
#56950=CARTESIAN_POINT('Ctrl Pts',(-0.0520601551526582,-0.377452151404502,
0.788245924512891));
#56951=CARTESIAN_POINT('Ctrl Pts',(0.289100858747305,-0.248195648281641,
0.808109327878104));
#56952=CARTESIAN_POINT('Ctrl Pts',(0.365220771143536,0.108600988391901,
0.827972731243317));
#56953=CARTESIAN_POINT('Ctrl Pts',(0.106514575117418,0.365834705354672,
0.84783613460853));
#56954=CARTESIAN_POINT('Ctrl Pts',(-0.23285652437024,0.291404635742235,
0.866752775884988));
#56955=CARTESIAN_POINT('Ctrl Pts',(-0.321796777016753,0.091443649544684,
0.879048282706375));
#56956=CARTESIAN_POINT('Ctrl Pts',(-0.322560633728396,-0.000240562580560428,
0.884722655072691));
#56957=CARTESIAN_POINT('Ctrl Pts',(-0.322596689206338,-0.00022565269554343,
0.78437734492731));
#56958=CARTESIAN_POINT('Ctrl Pts',(-0.322707672759724,-0.0141660460246545,
0.785240372742915));
#56959=CARTESIAN_POINT('Ctrl Pts',(-0.315551175979117,-0.134942160877861,
0.792724535013591));
#56960=CARTESIAN_POINT('Ctrl Pts',(-0.16305567921248,-0.344373717573672,
0.806829831739337));
#56961=CARTESIAN_POINT('Ctrl Pts',(0.201177731278749,-0.323586050868213,
0.826693235104551));
#56962=CARTESIAN_POINT('Ctrl Pts',(0.38097596669931,-0.00614204171891747,
0.846556638469764));
#56963=CARTESIAN_POINT('Ctrl Pts',(0.211504088229659,0.31693285178582,0.866420041834977));
#56964=CARTESIAN_POINT('Ctrl Pts',(-0.151869934840427,0.34945090466404,
0.88628344520019));
#56965=CARTESIAN_POINT('Ctrl Pts',(-0.313449894905197,0.141945587024724,
0.900602546230968));
#56966=CARTESIAN_POINT('Ctrl Pts',(-0.322654525208851,0.0176676699287391,
0.908300512806675));
#56967=CARTESIAN_POINT('Ctrl Pts',(-0.322501710998753,0.000260384004555341,
0.90937734492731));
#56968=CARTESIAN_POINT('Origin',(0.,0.,-0.177777344927309));
#56969=CARTESIAN_POINT('',(-0.322153421245596,0.000291028333709336,0.634722655072691));
#56970=CARTESIAN_POINT('',(-0.321795967956633,-0.000131423964174926,0.65937734492731));
#56971=CARTESIAN_POINT('',(-0.322275,-2.94787261092574E-14,-0.177777344927309));
#56972=CARTESIAN_POINT('Ctrl Pts',(-0.322153421245596,0.00029102833370933,
0.634722655072691));
#56973=CARTESIAN_POINT('Ctrl Pts',(-0.321467371001535,-0.0779468938575932,
0.639549137033926));
#56974=CARTESIAN_POINT('Ctrl Pts',(-0.253451104891186,-0.264582767850479,
0.650996753450233));
#56975=CARTESIAN_POINT('Ctrl Pts',(0.0589972495454716,-0.376430220494633,
0.66906550432161));
#56976=CARTESIAN_POINT('Ctrl Pts',(0.348391745474835,-0.154284082261366,
0.688928907686824));
#56977=CARTESIAN_POINT('Ctrl Pts',(0.318388601508794,0.209306198626352,
0.708792311052038));
#56978=CARTESIAN_POINT('Ctrl Pts',(-0.00350598136781482,0.381009310187041,
0.72865571441725));
#56979=CARTESIAN_POINT('Ctrl Pts',(-0.275874568389445,0.229220864270045,
0.745632495757469));
#56980=CARTESIAN_POINT('Ctrl Pts',(-0.32159337472638,0.0606027867557822,
0.755988142642615));
#56981=CARTESIAN_POINT('Ctrl Pts',(-0.321780623313585,-0.000110903176248449,
0.759722655072691));
#56982=CARTESIAN_POINT('Ctrl Pts',(-0.321795967956633,-0.000131423964174919,
0.65937734492731));
#56983=CARTESIAN_POINT('Ctrl Pts',(-0.321962962736951,-0.04569384867112,
0.662180232679155));
#56984=CARTESIAN_POINT('Ctrl Pts',(-0.291620126682177,-0.198673976518742,
0.671604254886071));
#56985=CARTESIAN_POINT('Ctrl Pts',(-0.0568219078975044,-0.376764757722924,
0.687649411548057));
#56986=CARTESIAN_POINT('Ctrl Pts',(0.285943996315395,-0.251826215573555,
0.707512814913272));
#56987=CARTESIAN_POINT('Ctrl Pts',(0.366562938806212,0.103980881765236,
0.727376218278483));
#56988=CARTESIAN_POINT('Ctrl Pts',(0.111125304043702,0.3644606682211,0.747239621643698));
#56989=CARTESIAN_POINT('Ctrl Pts',(-0.230664824743872,0.294011123707778,
0.766239997193306));
#56990=CARTESIAN_POINT('Ctrl Pts',(-0.321856208860203,0.0927844101711982,
0.778619238287844));
#56991=CARTESIAN_POINT('Ctrl Pts',(-0.322596689206338,-0.00022565269554343,
0.78437734492731));
#56992=CARTESIAN_POINT('Origin',(0.,0.,-0.177777344927309));
#56993=CARTESIAN_POINT('',(-0.322798898358608,-4.37237262256661E-5,0.50972265507269));
#56994=CARTESIAN_POINT('',(-0.322114562349406,0.000285900354075996,0.53437734492731));
#56995=CARTESIAN_POINT('',(-0.322275,-2.94787261092574E-14,-0.177777344927309));
#56996=CARTESIAN_POINT('Ctrl Pts',(-0.322798898358608,-4.37237262256363E-5,
0.50972265507269));
#56997=CARTESIAN_POINT('Ctrl Pts',(-0.322803350467903,-0.00238536310240654,
0.509867862515095));
#56998=CARTESIAN_POINT('Ctrl Pts',(-0.321718906904807,-0.111496286111473,
0.516634204412571));
#56999=CARTESIAN_POINT('Ctrl Pts',(-0.199305237284349,-0.324742680645371,
0.530021680765118));
#57000=CARTESIAN_POINT('Ctrl Pts',(0.16504213987037,-0.34342608880465,0.549885084130331));
#57001=CARTESIAN_POINT('Ctrl Pts',(0.378082631534635,-0.0472642580443332,
0.569748487495545));
#57002=CARTESIAN_POINT('Ctrl Pts',(0.244505553247802,0.29222837091975,0.589611890860758));
#57003=CARTESIAN_POINT('Ctrl Pts',(-0.113228663253673,0.363812666327059,
0.609475294225971));
#57004=CARTESIAN_POINT('Ctrl Pts',(-0.305456882130036,0.165511552441047,
0.624512215629949));
#57005=CARTESIAN_POINT('Ctrl Pts',(-0.322408518393226,0.0293825868023487,
0.632928002578855));
#57006=CARTESIAN_POINT('Ctrl Pts',(-0.322153421245596,0.00029102833370933,
0.634722655072691));
#57007=CARTESIAN_POINT('Ctrl Pts',(-0.322114562349406,0.000285900354075976,
0.53437734492731));
#57008=CARTESIAN_POINT('Ctrl Pts',(-0.321458474717958,-0.0766182390530337,
0.539120092615395));
#57009=CARTESIAN_POINT('Ctrl Pts',(-0.255330386675666,-0.261898064899981,
0.550483974758551));
#57010=CARTESIAN_POINT('Ctrl Pts',(0.0542395567617082,-0.377145174129293,
0.568468991356778));
#57011=CARTESIAN_POINT('Ctrl Pts',(0.346415935802215,-0.158670763850418,
0.588332394721992));
#57012=CARTESIAN_POINT('Ctrl Pts',(0.321006052375606,0.205269399120439,
0.608195798087205));
#57013=CARTESIAN_POINT('Ctrl Pts',(0.00130511053243591,0.381023238880027,
0.628059201452419));
#57014=CARTESIAN_POINT('Ctrl Pts',(-0.274311088907133,0.231954299418459,
0.645119717065786));
#57015=CARTESIAN_POINT('Ctrl Pts',(-0.321568478550757,0.0619361981922225,
0.655559098224084));
#57016=CARTESIAN_POINT('Ctrl Pts',(-0.321795967956633,-0.000131423964174919,
0.65937734492731));
#57017=CARTESIAN_POINT('Origin',(0.,0.,-0.177777344927309));
#57018=CARTESIAN_POINT('',(-0.322023724697603,-0.000266026364348698,0.38472265507269));
#57019=CARTESIAN_POINT('',(-0.322804887212102,-1.85792893697689E-5,0.40937734492731));
#57020=CARTESIAN_POINT('',(-0.322275,-2.94787261092574E-14,-0.177777344927309));
#57021=CARTESIAN_POINT('Ctrl Pts',(-0.322023724697603,-0.000266026364348675,
0.38472265507269));
#57022=CARTESIAN_POINT('Ctrl Pts',(-0.322286668321143,-0.0340997285001819,
0.386807722451335));
#57023=CARTESIAN_POINT('Ctrl Pts',(-0.301794699618203,-0.175061960972823,
0.395513924285051));
#57024=CARTESIAN_POINT('Ctrl Pts',(-0.0971925503173641,-0.368420939365887,
0.410841260573839));
#57025=CARTESIAN_POINT('Ctrl Pts',(0.257064747009525,-0.281243851578092,
0.430704663939052));
#57026=CARTESIAN_POINT('Ctrl Pts',(0.375650925262469,0.063771226098318,
0.450568067304265));
#57027=CARTESIAN_POINT('Ctrl Pts',(0.149848865235289,0.350322284637716,
0.470431470669478));
#57028=CARTESIAN_POINT('Ctrl Pts',(-0.210676274915335,0.315958889321312,
0.490149666592287));
#57029=CARTESIAN_POINT('Ctrl Pts',(-0.322600344246189,0.104388152760221,
0.503246728060024));
#57030=CARTESIAN_POINT('Ctrl Pts',(-0.322798898358608,-4.37237262256363E-5,
0.50972265507269));
#57031=CARTESIAN_POINT('Ctrl Pts',(-0.322804887212102,-1.85792893697065E-5,
0.40937734492731));
#57032=CARTESIAN_POINT('Ctrl Pts',(-0.322805713924285,-0.00100985665230741,
0.409438818096564));
#57033=CARTESIAN_POINT('Ctrl Pts',(-0.322352341065637,-0.108768573520454,
0.416121425720889));
#57034=CARTESIAN_POINT('Ctrl Pts',(-0.203389728683596,-0.32220029379513,
0.429425167800285));
#57035=CARTESIAN_POINT('Ctrl Pts',(0.160692729162575,-0.345482646427773,
0.449288571165499));
#57036=CARTESIAN_POINT('Ctrl Pts',(0.377455743121206,-0.0520343531991218,
0.469151974530712));
#57037=CARTESIAN_POINT('Ctrl Pts',(0.248175903852022,0.28911785229258,0.489015377895925));
#57038=CARTESIAN_POINT('Ctrl Pts',(-0.108625967532427,0.365213377502066,
0.508878781261139));
#57039=CARTESIAN_POINT('Ctrl Pts',(-0.304427023238494,0.168264571631386,
0.523999436938266));
#57040=CARTESIAN_POINT('Ctrl Pts',(-0.322374408836283,0.0307441341225915,
0.532498958160324));
#57041=CARTESIAN_POINT('Ctrl Pts',(-0.322114562349406,0.000285900354075976,
0.53437734492731));
#57042=CARTESIAN_POINT('Origin',(0.,0.,-0.177777344927309));
#57043=CARTESIAN_POINT('',(-0.321844616677633,0.000179048658294113,0.25972265507269));
#57044=CARTESIAN_POINT('',(-0.322059540737401,-0.000275272378033348,0.28437734492731));
#57045=CARTESIAN_POINT('',(-0.322275,-2.94787261092574E-14,-0.177777344927309));
#57046=CARTESIAN_POINT('Ctrl Pts',(-0.321844616677632,0.000179048658294108,
0.25972265507269));
#57047=CARTESIAN_POINT('Ctrl Pts',(-0.321515703515998,-0.0652236343715904,
0.263747582387576));
#57048=CARTESIAN_POINT('Ctrl Pts',(-0.270343504415437,-0.238689225402078,
0.274393644157532));
#57049=CARTESIAN_POINT('Ctrl Pts',(0.0131778654856828,-0.380797113767846,
0.291660840382558));
#57050=CARTESIAN_POINT('Ctrl Pts',(0.327246625055882,-0.195166812976406,
0.311524243747772));
#57051=CARTESIAN_POINT('Ctrl Pts',(0.341303248017118,0.169388689874893,
0.331387647112985));
#57052=CARTESIAN_POINT('Ctrl Pts',(0.0424607330362066,0.378652123483815,
0.351251050478199));
#57053=CARTESIAN_POINT('Ctrl Pts',(-0.259853013734845,0.255248969864476,
0.369029386464767));
#57054=CARTESIAN_POINT('Ctrl Pts',(-0.321451690467002,0.0733392412177939,
0.380186587996264));
#57055=CARTESIAN_POINT('Ctrl Pts',(-0.322023724697603,-0.000266026364348675,
0.38472265507269));
#57056=CARTESIAN_POINT('Ctrl Pts',(-0.322059540737401,-0.000275272378033303,
0.28437734492731));
#57057=CARTESIAN_POINT('Ctrl Pts',(-0.322322769946388,-0.032741145052682,
0.286378678032804));
#57058=CARTESIAN_POINT('Ctrl Pts',(-0.302876780071171,-0.172307827867515,
0.295001145593369));
#57059=CARTESIAN_POINT('Ctrl Pts',(-0.101836659246275,-0.367164356955896,
0.310244747609006));
#57060=CARTESIAN_POINT('Ctrl Pts',(0.25349314350919,-0.284467306274055,
0.330108150974219));
#57061=CARTESIAN_POINT('Ctrl Pts',(0.37642622426789,0.0590230048629484,
0.349971554339432));
#57062=CARTESIAN_POINT('Ctrl Pts',(0.154260273483973,0.348402316268487,
0.369834957704646));
#57063=CARTESIAN_POINT('Ctrl Pts',(-0.208202751865538,0.318467252949934,
0.389636887900605));
#57064=CARTESIAN_POINT('Ctrl Pts',(-0.322716670645885,0.105758360798129,
0.402817683641493));
#57065=CARTESIAN_POINT('Ctrl Pts',(-0.322804887212102,-1.85792893697065E-5,
0.40937734492731));
#57066=CARTESIAN_POINT('Origin',(0.,0.,-0.177777344927309));
#57067=CARTESIAN_POINT('',(-0.322672883777213,0.000203620636067219,0.13472265507269));
#57068=CARTESIAN_POINT('',(-0.321822258325956,0.000162574958589262,0.15937734492731));
#57069=CARTESIAN_POINT('',(-0.322275,-2.94787261092574E-14,-0.177777344927309));
#57070=CARTESIAN_POINT('Ctrl Pts',(-0.322672883777213,0.000203620636067221,
0.13472265507269));
#57071=CARTESIAN_POINT('Ctrl Pts',(-0.322020804100839,-0.096075831989152,
0.140687442323816));
#57072=CARTESIAN_POINT('Ctrl Pts',(-0.225137620539939,-0.300440548189766,
0.153273364030012));
#57073=CARTESIAN_POINT('Ctrl Pts',(0.122432227018064,-0.360801876178455,
0.172480420191279));
#57074=CARTESIAN_POINT('Ctrl Pts',(0.369623172725438,-0.0925175344721341,
0.192343823556493));
#57075=CARTESIAN_POINT('Ctrl Pts',(0.277958791015197,0.260619530981986,
0.212207226921706));
#57076=CARTESIAN_POINT('Ctrl Pts',(-0.0685354463999416,0.374808401925503,
0.232070630286919));
#57077=CARTESIAN_POINT('Ctrl Pts',(-0.294717851037753,0.191877835557772,
0.247909106337247));
#57078=CARTESIAN_POINT('Ctrl Pts',(-0.322056776210446,0.0423658757449738,
0.257126447932504));
#57079=CARTESIAN_POINT('Ctrl Pts',(-0.321844616677632,0.000179048658294108,
0.25972265507269));
#57080=CARTESIAN_POINT('Ctrl Pts',(-0.321822258325956,0.00016257495858928,
0.15937734492731));
#57081=CARTESIAN_POINT('Ctrl Pts',(-0.321535021268785,-0.0638911017945661,
0.163318537969044));
#57082=CARTESIAN_POINT('Ctrl Pts',(-0.271971025268605,-0.235966482044706,
0.17388086546585));
#57083=CARTESIAN_POINT('Ctrl Pts',(0.0083695466030628,-0.380931001484488,
0.191064327417726));
#57084=CARTESIAN_POINT('Ctrl Pts',(0.324755842971668,-0.199284387122036,
0.210927730782939));
#57085=CARTESIAN_POINT('Ctrl Pts',(0.343415090875769,0.165066330125723,
0.230791134148153));
#57086=CARTESIAN_POINT('Ctrl Pts',(0.0472382790882686,0.378085532147811,
0.250654537513366));
#57087=CARTESIAN_POINT('Ctrl Pts',(-0.258040470809522,0.25794659916087,
0.268516607773085));
#57088=CARTESIAN_POINT('Ctrl Pts',(-0.321451912426257,0.074667715366378,
0.279757543577733));
#57089=CARTESIAN_POINT('Ctrl Pts',(-0.322059540737401,-0.000275272378033303,
0.28437734492731));
#57090=CARTESIAN_POINT('Ctrl Pts',(-0.143290239521317,0.28866777250487,
0.0122936971308069));
#57091=CARTESIAN_POINT('Ctrl Pts',(-0.239363065031841,0.240978700533178,
0.018914831585878));
#57092=CARTESIAN_POINT('Ctrl Pts',(-0.378476748230256,0.0429489016361644,
0.0321571004960201));
#57093=CARTESIAN_POINT('Ctrl Pts',(-0.240846428651748,-0.295574326569485,
0.0520205038612334));
#57094=CARTESIAN_POINT('Ctrl Pts',(0.117909826126082,-0.362210109500856,
0.0718839072264466));
#57095=CARTESIAN_POINT('Ctrl Pts',(0.368403165707845,-0.0972337884399037,
0.09174731059166));
#57096=CARTESIAN_POINT('Ctrl Pts',(0.281239048491698,0.257118611189565,
0.111610713956873));
#57097=CARTESIAN_POINT('Ctrl Pts',(-0.0638035626910551,0.375628548193864,
0.131474117322087));
#57098=CARTESIAN_POINT('Ctrl Pts',(-0.350329092518743,0.1498343396268,0.1513375206873));
#57099=CARTESIAN_POINT('Ctrl Pts',(-0.315693082587524,-0.213357742304184,
0.171200924052513));
#57100=CARTESIAN_POINT('Ctrl Pts',(0.0083695466030628,-0.380931001484488,
0.191064327417726));
#57101=CARTESIAN_POINT('Ctrl Pts',(0.324755842971668,-0.199284387122036,
0.210927730782939));
#57102=CARTESIAN_POINT('Ctrl Pts',(0.343415090875769,0.165066330125723,
0.230791134148153));
#57103=CARTESIAN_POINT('Ctrl Pts',(0.0472382790882686,0.378085532147811,
0.250654537513366));
#57104=CARTESIAN_POINT('Ctrl Pts',(-0.292245042826693,0.244485784129382,
0.27051794087858));
#57105=CARTESIAN_POINT('Ctrl Pts',(-0.363804992481417,-0.113253645323718,
0.290381344243792));
#57106=CARTESIAN_POINT('Ctrl Pts',(-0.101836659246275,-0.367164356955896,
0.310244747609006));
#57107=CARTESIAN_POINT('Ctrl Pts',(0.25349314350919,-0.284467306274055,
0.330108150974219));
#57108=CARTESIAN_POINT('Ctrl Pts',(0.37642622426789,0.0590230048629484,
0.349971554339432));
#57109=CARTESIAN_POINT('Ctrl Pts',(0.154260273483973,0.348402316268487,
0.369834957704646));
#57110=CARTESIAN_POINT('Ctrl Pts',(-0.209327983127598,0.318374322452967,
0.389698361069859));
#57111=CARTESIAN_POINT('Ctrl Pts',(-0.381009103820433,-0.00353203298202855,
0.409561764435072));
#57112=CARTESIAN_POINT('Ctrl Pts',(-0.203389728683596,-0.32220029379513,
0.429425167800285));
#57113=CARTESIAN_POINT('Ctrl Pts',(0.160692729162575,-0.345482646427773,
0.449288571165499));
#57114=CARTESIAN_POINT('Ctrl Pts',(0.377455743121206,-0.0520343531991218,
0.469151974530712));
#57115=CARTESIAN_POINT('Ctrl Pts',(0.248175903852022,0.28911785229258,0.489015377895925));
#57116=CARTESIAN_POINT('Ctrl Pts',(-0.108625967532427,0.365213377502066,
0.508878781261139));
#57117=CARTESIAN_POINT('Ctrl Pts',(-0.365842018996859,0.106489572341696,
0.528742184626351));
#57118=CARTESIAN_POINT('Ctrl Pts',(-0.287662416064326,-0.249861454106355,
0.548605587991565));
#57119=CARTESIAN_POINT('Ctrl Pts',(0.0542395567617082,-0.377145174129293,
0.568468991356778));
#57120=CARTESIAN_POINT('Ctrl Pts',(0.346415935802215,-0.158670763850418,
0.588332394721992));
#57121=CARTESIAN_POINT('Ctrl Pts',(0.321006052375606,0.205269399120439,
0.608195798087205));
#57122=CARTESIAN_POINT('Ctrl Pts',(0.00130511053243591,0.381023238880027,
0.628059201452419));
#57123=CARTESIAN_POINT('Ctrl Pts',(-0.31959232700839,0.20746362668229,0.64792260481763));
#57124=CARTESIAN_POINT('Ctrl Pts',(-0.34749477743719,-0.156293926729706,
0.667786008182846));
#57125=CARTESIAN_POINT('Ctrl Pts',(-0.0568219078975044,-0.376764757722924,
0.687649411548057));
#57126=CARTESIAN_POINT('Ctrl Pts',(0.285943996315395,-0.251826215573555,
0.707512814913272));
#57127=CARTESIAN_POINT('Ctrl Pts',(0.366562938806212,0.103980881765236,
0.727376218278483));
#57128=CARTESIAN_POINT('Ctrl Pts',(0.111125304043702,0.3644606682211,0.747239621643698));
#57129=CARTESIAN_POINT('Ctrl Pts',(-0.246189485689262,0.290811191351024,
0.767103025008911));
#57130=CARTESIAN_POINT('Ctrl Pts',(-0.377803346174014,-0.0494473811102893,
0.786966428374124));
#57131=CARTESIAN_POINT('Ctrl Pts',(-0.16305567921248,-0.344373717573672,
0.806829831739337));
#57132=CARTESIAN_POINT('Ctrl Pts',(0.201177731278749,-0.323586050868213,
0.826693235104551));
#57133=CARTESIAN_POINT('Ctrl Pts',(0.38097596669931,-0.00614204171891747,
0.846556638469764));
#57134=CARTESIAN_POINT('Ctrl Pts',(0.211504088229659,0.31693285178582,0.866420041834977));
#57135=CARTESIAN_POINT('Ctrl Pts',(-0.151869934840427,0.34945090466404,
0.88628344520019));
#57136=CARTESIAN_POINT('Ctrl Pts',(-0.376013050780663,0.061600304557439,
0.906146848565404));
#57137=CARTESIAN_POINT('Ctrl Pts',(-0.255435941431669,-0.28272405575732,
0.926010251930617));
#57138=CARTESIAN_POINT('Ctrl Pts',(0.0993190377930615,-0.367853422725428,
0.945873655295831));
#57139=CARTESIAN_POINT('Ctrl Pts',(0.363020578812783,-0.115743126091287,
0.965737058661042));
#57140=CARTESIAN_POINT('Ctrl Pts',(0.293913097770214,0.242477839890713,
0.985600462026258));
#57141=CARTESIAN_POINT('Ctrl Pts',(-0.0446472362210804,0.378400629197116,
1.00546386539147));
#57142=CARTESIAN_POINT('Ctrl Pts',(-0.342275998032317,0.167414315546578,
1.02532726875668));
#57143=CARTESIAN_POINT('Ctrl Pts',(-0.326113898308744,-0.197053640435337,
1.0451906721219));
#57144=CARTESIAN_POINT('Ctrl Pts',(-0.0109779830180157,-0.380867294169285,
1.06505407548711));
#57145=CARTESIAN_POINT('Ctrl Pts',(0.314222297781658,-0.215510462520356,
1.08491747885232));
#57146=CARTESIAN_POINT('Ctrl Pts',(0.351350712306201,0.147421466689362,
1.10478088221754));
#57147=CARTESIAN_POINT('Ctrl Pts',(0.066368773346284,0.375200743340994,
1.12464428558275));
#57148=CARTESIAN_POINT('Ctrl Pts',(-0.279458549710258,0.259004499714875,
1.14450768894796));
#57149=CARTESIAN_POINT('Ctrl Pts',(-0.369084621200932,-0.0946411869735989,
1.16437109231318));
#57150=CARTESIAN_POINT('Ctrl Pts',(-0.120342294288793,-0.361521982852271,
1.18423449567839));
#57151=CARTESIAN_POINT('Ctrl Pts',(0.238727114922392,-0.296967635404715,
1.2040978990436));
#57152=CARTESIAN_POINT('Ctrl Pts',(0.378936926926189,0.0398398957118962,
1.22396130240882));
#57153=CARTESIAN_POINT('Ctrl Pts',(0.171745970394351,0.34012311526861,1.24382470577403));
#57154=CARTESIAN_POINT('Ctrl Pts',(-0.192897791255575,0.328589187273149,
1.26368810913924));
#57155=CARTESIAN_POINT('Ctrl Pts',(-0.380697238803822,0.0158121550827373,
1.28355151250445));
#57156=CARTESIAN_POINT('Ctrl Pts',(-0.219482103861983,-0.311461101926292,
1.30341491586967));
#57157=CARTESIAN_POINT('Ctrl Pts',(0.142949239214434,-0.353193894022897,
1.32327831923488));
#57158=CARTESIAN_POINT('Ctrl Pts',(0.374327966327785,-0.0711265460495382,
1.3431417226001));
#57159=CARTESIAN_POINT('Ctrl Pts',(0.262531315278285,0.276148005038436,
1.36300512596531));
#57160=CARTESIAN_POINT('Ctrl Pts',(-0.0899480831884954,0.370256334701204,
1.38286852933052));
#57161=CARTESIAN_POINT('Ctrl Pts',(-0.359965121917103,0.124922069524326,
1.40273193269573));
#57162=CARTESIAN_POINT('Ctrl Pts',(-0.299974311861765,-0.234937919333417,
1.42259533606095));
#57163=CARTESIAN_POINT('Ctrl Pts',(0.0350261341603416,-0.379412145143482,
1.44245873942616));
#57164=CARTESIAN_POINT('Ctrl Pts',(0.3379154166412,-0.176049960567548,1.46232214279137));
#57165=CARTESIAN_POINT('Ctrl Pts',(0.331011518086569,0.18871088214253,1.48218554615659));
#57166=CARTESIAN_POINT('Ctrl Pts',(0.0206437802330401,0.380465773129421,
1.5020489495218));
#57167=CARTESIAN_POINT('Ctrl Pts',(-0.308649711960631,0.223418477391944,
1.52191235288702));
#57168=CARTESIAN_POINT('Ctrl Pts',(-0.354980147521045,-0.138454174960786,
1.54177575625223));
#57169=CARTESIAN_POINT('Ctrl Pts',(-0.0758728659140442,-0.373394473511197,
1.56163915961744));
#57170=CARTESIAN_POINT('Ctrl Pts',(0.272792974535782,-0.26601656156395,
1.58150256298265));
#57171=CARTESIAN_POINT('Ctrl Pts',(0.37136833748108,0.0852419052542959,
1.60136596634787));
#57172=CARTESIAN_POINT('Ctrl Pts',(0.129481784457052,0.358347519450231,
1.62122936971308));
#57173=CARTESIAN_POINT('Ctrl Pts',(-0.231110999495935,0.302937872354617,
1.6410927730783));
#57174=CARTESIAN_POINT('Ctrl Pts',(-0.379825947107903,-0.0302167552855949,
1.66095617644351));
#57175=CARTESIAN_POINT('Ctrl Pts',(-0.18032609112216,-0.335634029399439,
1.68081957980872));
#57176=CARTESIAN_POINT('Ctrl Pts',(0.184494543087876,-0.333417375353118,
1.70068298317393));
#57177=CARTESIAN_POINT('Ctrl Pts',(0.380171112467216,-0.0254013260161302,
1.72054638653915));
#57178=CARTESIAN_POINT('Ctrl Pts',(0.227322355071844,0.305652478161549,
1.74040978990436));
#57179=CARTESIAN_POINT('Ctrl Pts',(-0.133942736176479,0.356974128119761,
1.76027319326957));
#57180=CARTESIAN_POINT('Ctrl Pts',(-0.372396558778726,0.0800628510138407,
1.78013659663479));
#57181=CARTESIAN_POINT('Ctrl Pts',(-0.303743473412038,-0.152004320240206,
1.79337886554493));
#57182=CARTESIAN_POINT('Ctrl Pts',(-0.227909696623847,-0.227855976023948,
1.8));
#57183=CARTESIAN_POINT('Ctrl Pts',(-0.153816642191914,0.309873914818277,
0.0259624647538713));
#57184=CARTESIAN_POINT('Ctrl Pts',(-0.256947179730866,0.258681503217605,
0.0325835992089423));
#57185=CARTESIAN_POINT('Ctrl Pts',(-0.40628044697931,0.0461040183726067,
0.0458258681190845));
#57186=CARTESIAN_POINT('Ctrl Pts',(-0.258539514365286,-0.317287838885153,
0.0656892714842978));
#57187=CARTESIAN_POINT('Ctrl Pts',(0.126571730194143,-0.388818826721966,
0.0855526748495111));
#57188=CARTESIAN_POINT('Ctrl Pts',(0.395466837876437,-0.104376787249354,
0.105416078214724));
#57189=CARTESIAN_POINT('Ctrl Pts',(0.301899461099073,0.276007085690883,
0.125279481579938));
#57190=CARTESIAN_POINT('Ctrl Pts',(-0.0684907067348376,0.403223012171802,
0.145142884945151));
#57191=CARTESIAN_POINT('Ctrl Pts',(-0.376065005218707,0.160841485668737,
0.165006288310364));
#57192=CARTESIAN_POINT('Ctrl Pts',(-0.338884561077199,-0.229031451245463,
0.184869691675577));
#57193=CARTESIAN_POINT('Ctrl Pts',(0.00898439111730312,-0.408914994844647,
0.20473309504079));
#57194=CARTESIAN_POINT('Ctrl Pts',(0.348613090919395,-0.213924237762373,
0.224596498406004));
#57195=CARTESIAN_POINT('Ctrl Pts',(0.368643086458686,0.177192450258299,
0.244459901771217));
#57196=CARTESIAN_POINT('Ctrl Pts',(0.0507085025229608,0.405860491339804,
0.264323305136431));
#57197=CARTESIAN_POINT('Ctrl Pts',(-0.313713978949325,0.262446224558406,
0.284186708501643));
#57198=CARTESIAN_POINT('Ctrl Pts',(-0.390530873164058,-0.121573496547171,
0.304050111866857));
#57199=CARTESIAN_POINT('Ctrl Pts',(-0.109317794635791,-0.394137023625451,
0.32391351523207));
#57200=CARTESIAN_POINT('Ctrl Pts',(0.272115283521848,-0.305364873494716,
0.343776918597283));
#57201=CARTESIAN_POINT('Ctrl Pts',(0.404079287209609,0.0633589590639552,
0.363640321962497));
#57202=CARTESIAN_POINT('Ctrl Pts',(0.165592557945175,0.373996683928579,
0.38350372532771));
#57203=CARTESIAN_POINT('Ctrl Pts',(-0.224705657475733,0.341762770468092,
0.403367128692924));
#57204=CARTESIAN_POINT('Ctrl Pts',(-0.408998834742623,-0.00379150356103331,
0.423230532058136));
#57205=CARTESIAN_POINT('Ctrl Pts',(-0.218331166358207,-0.345869805720036,
0.443093935423351));
#57206=CARTESIAN_POINT('Ctrl Pts',(0.17249755536046,-0.370862528994456,
0.462957338788562));
#57207=CARTESIAN_POINT('Ctrl Pts',(0.40518443668538,-0.0558569063353875,
0.482820742153777));
#57208=CARTESIAN_POINT('Ctrl Pts',(0.266407428244846,0.310357058414762,
0.502684145518989));
#57209=CARTESIAN_POINT('Ctrl Pts',(-0.116605859802474,0.392042721113458,
0.522547548884203));
#57210=CARTESIAN_POINT('Ctrl Pts',(-0.392717543935965,0.114312520523188,
0.542410952249416));
#57211=CARTESIAN_POINT('Ctrl Pts',(-0.308794702776989,-0.268216802569522,
0.562274355614629));
#57212=CARTESIAN_POINT('Ctrl Pts',(0.05822410879439,-0.404851052641468,
0.582137758979843));
#57213=CARTESIAN_POINT('Ctrl Pts',(0.371864379771239,-0.170327052219542,
0.602001162345056));
#57214=CARTESIAN_POINT('Ctrl Pts',(0.344587832811547,0.220348921342689,
0.621864565710269));
#57215=CARTESIAN_POINT('Ctrl Pts',(0.00140098669985904,0.409014008193454,
0.641727969075482));
#57216=CARTESIAN_POINT('Ctrl Pts',(-0.343070252202474,0.222704341480843,
0.661591372440696));
#57217=CARTESIAN_POINT('Ctrl Pts',(-0.373022475384054,-0.167775607639877,
0.681454775805909));
#57218=CARTESIAN_POINT('Ctrl Pts',(-0.060996164881367,-0.404442690044978,
0.701318179171122));
#57219=CARTESIAN_POINT('Ctrl Pts',(0.306950044295433,-0.270325899550608,
0.721181582536336));
#57220=CARTESIAN_POINT('Ctrl Pts',(0.393491424032298,0.111619536255318,
0.741044985901548));
#57221=CARTESIAN_POINT('Ctrl Pts',(0.119288802835838,0.391234716223999,
0.760908389266763));
#57222=CARTESIAN_POINT('Ctrl Pts',(-0.26427508362175,0.312174793725505,
0.780771792631975));
#57223=CARTESIAN_POINT('Ctrl Pts',(-0.405557575390273,-0.053079889830436,
0.800635195997189));
#57224=CARTESIAN_POINT('Ctrl Pts',(-0.17503409269586,-0.369672135892053,
0.820498599362402));
#57225=CARTESIAN_POINT('Ctrl Pts',(0.215956670966977,-0.347357363425207,
0.840362002727614));
#57226=CARTESIAN_POINT('Ctrl Pts',(0.408963263298817,-0.00659324903470751,
0.860225406092828));
#57227=CARTESIAN_POINT('Ctrl Pts',(0.227041623840047,0.340215406330941,
0.880088809458042));
#57228=CARTESIAN_POINT('Ctrl Pts',(-0.163026619992382,0.375122303835311,
0.899952212823254));
#57229=CARTESIAN_POINT('Ctrl Pts',(-0.403635761128137,0.0661255926201126,
0.919815616188469));
#57230=CARTESIAN_POINT('Ctrl Pts',(-0.274200803469975,-0.303493560124875,
0.93967901955368));
#57231=CARTESIAN_POINT('Ctrl Pts',(0.106615223410158,-0.394876709617135,
0.959542422918895));
#57232=CARTESIAN_POINT('Ctrl Pts',(0.389688834815862,-0.124245859813145,
0.979405826284108));
#57233=CARTESIAN_POINT('Ctrl Pts',(0.315504572720832,0.260290772508546,
0.999269229649321));
#57234=CARTESIAN_POINT('Ctrl Pts',(-0.0479271161917057,0.406198736081739,
1.01913263301453));
#57235=CARTESIAN_POINT('Ctrl Pts',(-0.367420313456767,0.179712923631493,
1.03899603637975));
#57236=CARTESIAN_POINT('Ctrl Pts',(-0.350070911860711,-0.211529615727575,
1.05885943974496));
#57237=CARTESIAN_POINT('Ctrl Pts',(-0.0117844487629612,-0.408846607455944,
1.07872284311017));
#57238=CARTESIAN_POINT('Ctrl Pts',(0.337305729322982,-0.231342314820938,
1.09858624647539));
#57239=CARTESIAN_POINT('Ctrl Pts',(0.377161675346616,0.15825135800538,1.1184496498406));
#57240=CARTESIAN_POINT('Ctrl Pts',(0.0712443631654572,0.402763779873762,
1.13831305320581));
#57241=CARTESIAN_POINT('Ctrl Pts',(-0.29998816312858,0.278031515557712,
1.15817645657103));
#57242=CARTESIAN_POINT('Ctrl Pts',(-0.396198354524746,-0.101593727821009,
1.17803985993624));
#57243=CARTESIAN_POINT('Ctrl Pts',(-0.129182892589275,-0.38808014884103,
1.19790326330145));
#57244=CARTESIAN_POINT('Ctrl Pts',(0.256264511387483,-0.318783503120817,
1.21776666666667));
#57245=CARTESIAN_POINT('Ctrl Pts',(0.406774431371081,0.0427666183276071,
1.23763007003188));
#57246=CARTESIAN_POINT('Ctrl Pts',(0.18436279096401,0.365109275392678,1.25749347339709));
#57247=CARTESIAN_POINT('Ctrl Pts',(-0.207068469117572,0.352728040763777,
1.27735687676231));
#57248=CARTESIAN_POINT('Ctrl Pts',(-0.408664059465309,0.0169737492851567,
1.29722028012752));
#57249=CARTESIAN_POINT('Ctrl Pts',(-0.235605721297195,-0.334341690206812,
1.31708368349273));
#57250=CARTESIAN_POINT('Ctrl Pts',(0.153450591284563,-0.379140261072753,
1.33694708685795));
#57251=CARTESIAN_POINT('Ctrl Pts',(0.401826886823667,-0.0763516518682445,
1.35681049022316));
#57252=CARTESIAN_POINT('Ctrl Pts',(0.281817418417573,0.296434418875328,
1.37667389358837));
#57253=CARTESIAN_POINT('Ctrl Pts',(-0.0965558587512498,0.39745614456561,
1.39653729695359));
#57254=CARTESIAN_POINT('Ctrl Pts',(-0.386408917623835,0.134099107755616,
1.4164007003188));
#57255=CARTESIAN_POINT('Ctrl Pts',(-0.322011056360493,-0.252196953512977,
1.43626410368402));
#57256=CARTESIAN_POINT('Ctrl Pts',(0.0375992277178473,-0.407284560119116,
1.45612750704922));
#57257=CARTESIAN_POINT('Ctrl Pts',(0.362739394576132,-0.188982961316714,
1.47599091041444));
#57258=CARTESIAN_POINT('Ctrl Pts',(0.355328321098593,0.202573980846195,
1.49585431377965));
#57259=CARTESIAN_POINT('Ctrl Pts',(0.0221603157912376,0.408415589835151,
1.51571771714486));
#57260=CARTESIAN_POINT('Ctrl Pts',(-0.331323769615328,0.239831269114091,
1.53558112051008));
#57261=CARTESIAN_POINT('Ctrl Pts',(-0.381057736513555,-0.148625310147182,
1.55544452387529));
#57262=CARTESIAN_POINT('Ctrl Pts',(-0.081446646382637,-0.400824817659447,
1.57530792724051));
#57263=CARTESIAN_POINT('Ctrl Pts',(0.292832920768453,-0.285558698233028,
1.59517133060572));
#57264=CARTESIAN_POINT('Ctrl Pts',(0.398649837410844,0.0915039550778764,
1.61503473397093));
#57265=CARTESIAN_POINT('Ctrl Pts',(0.138993788947073,0.384672482674136,
1.63489813733614));
#57266=CARTESIAN_POINT('Ctrl Pts',(-0.248088900087248,0.325192326246467,
1.65476154070136));
#57267=CARTESIAN_POINT('Ctrl Pts',(-0.407728760847038,-0.0324365417455611,
1.67462494406657));
#57268=CARTESIAN_POINT('Ctrl Pts',(-0.193573225424597,-0.360290411824483,
1.69448834743178));
#57269=CARTESIAN_POINT('Ctrl Pts',(0.198047900647739,-0.357910917705102,
1.714351750797));
#57270=CARTESIAN_POINT('Ctrl Pts',(0.408099282780338,-0.0272673609038275,
1.73421515416221));
#57271=CARTESIAN_POINT('Ctrl Pts',(0.244021933867365,0.328106352711155,
1.75407855752742));
#57272=CARTESIAN_POINT('Ctrl Pts',(-0.143782451571646,0.383198199125069,
1.77394196089264));
#57273=CARTESIAN_POINT('Ctrl Pts',(-0.399753594009775,0.0859444366092283,
1.79380536425785));
#57274=CARTESIAN_POINT('Ctrl Pts',(-0.326057108453634,-0.163170877626556,
1.80704763316799));
#57275=CARTESIAN_POINT('Ctrl Pts',(-0.244652422766334,-0.244594755738063,
1.81366876762306));
#57276=CARTESIAN_POINT('Ctrl Pts',(-0.164343044862511,0.331080057131683,
0.0396312323769356));
#57277=CARTESIAN_POINT('Ctrl Pts',(-0.274531294429891,0.276384305902031,
0.0462523668320067));
#57278=CARTESIAN_POINT('Ctrl Pts',(-0.434084145728363,0.0492591351090493,
0.0594946357421488));
#57279=CARTESIAN_POINT('Ctrl Pts',(-0.276232600078826,-0.339001351200821,
0.0793580391073622));
#57280=CARTESIAN_POINT('Ctrl Pts',(0.135233634262204,-0.415427543943075,
0.0992214424725753));
#57281=CARTESIAN_POINT('Ctrl Pts',(0.422530510045029,-0.111519786058804,
0.119084845837789));
#57282=CARTESIAN_POINT('Ctrl Pts',(0.322559873706447,0.294895560192201,
0.138948249203002));
#57283=CARTESIAN_POINT('Ctrl Pts',(-0.0731778507786196,0.430817476149739,
0.158811652568215));
#57284=CARTESIAN_POINT('Ctrl Pts',(-0.401800917918672,0.171848631710674,
0.178675055933429));
#57285=CARTESIAN_POINT('Ctrl Pts',(-0.362076039566874,-0.244705160186743,
0.198538459298642));
#57286=CARTESIAN_POINT('Ctrl Pts',(0.0095992356315428,-0.436898988204806,
0.218401862663855));
#57287=CARTESIAN_POINT('Ctrl Pts',(0.372470338867123,-0.228564088402712,
0.238265266029068));
#57288=CARTESIAN_POINT('Ctrl Pts',(0.393871082041601,0.189318570390874,
0.258128669394281));
#57289=CARTESIAN_POINT('Ctrl Pts',(0.0541787259576539,0.433635450531796,
0.277992072759495));
#57290=CARTESIAN_POINT('Ctrl Pts',(-0.335182915071958,0.28040666498743,
0.297855476124708));
#57291=CARTESIAN_POINT('Ctrl Pts',(-0.417256753846697,-0.129893347770624,
0.317718879489921));
#57292=CARTESIAN_POINT('Ctrl Pts',(-0.116798930025308,-0.421109690295005,
0.337582282855134));
#57293=CARTESIAN_POINT('Ctrl Pts',(0.290737423534506,-0.326262440715378,
0.357445686220348));
#57294=CARTESIAN_POINT('Ctrl Pts',(0.431732350151328,0.067694913264962,
0.377309089585562));
#57295=CARTESIAN_POINT('Ctrl Pts',(0.176924842406377,0.399591051588671,
0.397172492950774));
#57296=CARTESIAN_POINT('Ctrl Pts',(-0.240083331823868,0.365151218483217,
0.417035896315988));
#57297=CARTESIAN_POINT('Ctrl Pts',(-0.436988565664813,-0.00405097414003781,
0.4368992996812));
#57298=CARTESIAN_POINT('Ctrl Pts',(-0.233272604032816,-0.369539317644943,
0.456762703046414));
#57299=CARTESIAN_POINT('Ctrl Pts',(0.184302381558345,-0.396242411561139,
0.476626106411628));
#57300=CARTESIAN_POINT('Ctrl Pts',(0.432913130249555,-0.0596794594716531,
0.496489509776841));
#57301=CARTESIAN_POINT('Ctrl Pts',(0.284638952637669,0.331596264536944,
0.516352913142054));
#57302=CARTESIAN_POINT('Ctrl Pts',(-0.124585752072521,0.418872064724852,
0.536216316507267));
#57303=CARTESIAN_POINT('Ctrl Pts',(-0.419593068875071,0.12213546870468,
0.556079719872481));
#57304=CARTESIAN_POINT('Ctrl Pts',(-0.329926989489652,-0.28657215103269,
0.575943123237694));
#57305=CARTESIAN_POINT('Ctrl Pts',(0.0622086608270722,-0.432556931153643,
0.595806526602907));
#57306=CARTESIAN_POINT('Ctrl Pts',(0.397312823740262,-0.181983340588665,
0.615669929968121));
#57307=CARTESIAN_POINT('Ctrl Pts',(0.368169613247489,0.235428443564939,
0.635533333333333));
#57308=CARTESIAN_POINT('Ctrl Pts',(0.00149686286728203,0.437004777506881,
0.655396736698547));
#57309=CARTESIAN_POINT('Ctrl Pts',(-0.366548177396557,0.237945056279397,
0.675260140063759));
#57310=CARTESIAN_POINT('Ctrl Pts',(-0.398550173330919,-0.179257288550047,
0.695123543428974));
#57311=CARTESIAN_POINT('Ctrl Pts',(-0.0651704218652294,-0.432120622367032,
0.714986946794186));
#57312=CARTESIAN_POINT('Ctrl Pts',(0.327956092275469,-0.28882558352766,
0.7348503501594));
#57313=CARTESIAN_POINT('Ctrl Pts',(0.420419909258386,0.1192581907454,0.754713753524613));
#57314=CARTESIAN_POINT('Ctrl Pts',(0.127452301627973,0.418008764226898,
0.774577156889826));
#57315=CARTESIAN_POINT('Ctrl Pts',(-0.282360681554238,0.333538396099987,
0.79444056025504));
#57316=CARTESIAN_POINT('Ctrl Pts',(-0.433311804606533,-0.0567123985505825,
0.814303963620252));
#57317=CARTESIAN_POINT('Ctrl Pts',(-0.18701250617924,-0.394970554210435,
0.834167366985467));
#57318=CARTESIAN_POINT('Ctrl Pts',(0.230735610655205,-0.371128675982201,
0.854030770350678));
#57319=CARTESIAN_POINT('Ctrl Pts',(0.436950559898324,-0.00704445635049757,
0.873894173715893));
#57320=CARTESIAN_POINT('Ctrl Pts',(0.242579159450435,0.363497960876062,
0.893757577081105));
#57321=CARTESIAN_POINT('Ctrl Pts',(-0.174183305144337,0.400793703006583,
0.913620980446319));
#57322=CARTESIAN_POINT('Ctrl Pts',(-0.43125847147561,0.0706508806827865,
0.933484383811532));
#57323=CARTESIAN_POINT('Ctrl Pts',(-0.292965665508282,-0.324263064492431,
0.953347787176745));
#57324=CARTESIAN_POINT('Ctrl Pts',(0.113911409027256,-0.421899996508841,
0.97321119054196));
#57325=CARTESIAN_POINT('Ctrl Pts',(0.416357090818941,-0.132748593535004,
0.993074593907171));
#57326=CARTESIAN_POINT('Ctrl Pts',(0.33709604767145,0.278103705126378,1.01293799727239));
#57327=CARTESIAN_POINT('Ctrl Pts',(-0.0512069961623312,0.433996842966362,
1.0328014006376));
#57328=CARTESIAN_POINT('Ctrl Pts',(-0.392564628881217,0.192011531716408,
1.05266480400281));
#57329=CARTESIAN_POINT('Ctrl Pts',(-0.374027925412677,-0.226005591019812,
1.07252820736802));
#57330=CARTESIAN_POINT('Ctrl Pts',(-0.0125909145079066,-0.436825920742602,
1.09239161073324));
#57331=CARTESIAN_POINT('Ctrl Pts',(0.360389160864306,-0.24717416712152,
1.11225501409845));
#57332=CARTESIAN_POINT('Ctrl Pts',(0.402972638387031,0.169081249321399,
1.13211841746366));
#57333=CARTESIAN_POINT('Ctrl Pts',(0.0761199529846302,0.430326816406531,
1.15198182082888));
#57334=CARTESIAN_POINT('Ctrl Pts',(-0.320517776546902,0.297058531400549,
1.17184522419409));
#57335=CARTESIAN_POINT('Ctrl Pts',(-0.423312087848561,-0.10854626866842,
1.1917086275593));
#57336=CARTESIAN_POINT('Ctrl Pts',(-0.138023490889758,-0.414638314829788,
1.21157203092452));
#57337=CARTESIAN_POINT('Ctrl Pts',(0.273801907852573,-0.340599370836921,
1.23143543428973));
#57338=CARTESIAN_POINT('Ctrl Pts',(0.434611935815974,0.0456933409433185,
1.25129883765494));
#57339=CARTESIAN_POINT('Ctrl Pts',(0.196979611533669,0.390095435516746,
1.27116224102016));
#57340=CARTESIAN_POINT('Ctrl Pts',(-0.221239146979568,0.376866894254405,
1.29102564438537));
#57341=CARTESIAN_POINT('Ctrl Pts',(-0.436630880126795,0.018135343487576,
1.31088904775058));
#57342=CARTESIAN_POINT('Ctrl Pts',(-0.251729338732408,-0.357222278487332,
1.3307524511158));
#57343=CARTESIAN_POINT('Ctrl Pts',(0.163951943354692,-0.405086628122609,
1.35061585448101));
#57344=CARTESIAN_POINT('Ctrl Pts',(0.429325807319548,-0.0815767576869509,
1.37047925784622));
#57345=CARTESIAN_POINT('Ctrl Pts',(0.301103521556861,0.31672083271222,1.39034266121144));
#57346=CARTESIAN_POINT('Ctrl Pts',(-0.103163634314005,0.424655954430015,
1.41020606457665));
#57347=CARTESIAN_POINT('Ctrl Pts',(-0.412852713330567,0.143276145986907,
1.43006946794186));
#57348=CARTESIAN_POINT('Ctrl Pts',(-0.344047800859222,-0.269455987692538,
1.44993287130708));
#57349=CARTESIAN_POINT('Ctrl Pts',(0.0401723212753536,-0.435156975094748,
1.46979627467229));
#57350=CARTESIAN_POINT('Ctrl Pts',(0.387563372511063,-0.20191596206588,
1.4896596780375));
#57351=CARTESIAN_POINT('Ctrl Pts',(0.379645124110617,0.21643707954986,1.50952308140272));
#57352=CARTESIAN_POINT('Ctrl Pts',(0.0236768513494346,0.436365406540881,
1.52938648476793));
#57353=CARTESIAN_POINT('Ctrl Pts',(-0.353997827270024,0.256244060836238,
1.54924988813314));
#57354=CARTESIAN_POINT('Ctrl Pts',(-0.407135325506065,-0.158796445333579,
1.56911329149836));
#57355=CARTESIAN_POINT('Ctrl Pts',(-0.0870204268512302,-0.428255161807698,
1.58897669486357));
#57356=CARTESIAN_POINT('Ctrl Pts',(0.312872867001124,-0.305100834902106,
1.60884009822878));
#57357=CARTESIAN_POINT('Ctrl Pts',(0.425931337340609,0.0977660049014583,
1.628703501594));
#57358=CARTESIAN_POINT('Ctrl Pts',(0.148505793437094,0.410997445898041,
1.64856690495921));
#57359=CARTESIAN_POINT('Ctrl Pts',(-0.265066800678562,0.347446780138317,
1.66843030832442));
#57360=CARTESIAN_POINT('Ctrl Pts',(-0.435631574586173,-0.0346563282055276,
1.68829371168964));
#57361=CARTESIAN_POINT('Ctrl Pts',(-0.206820359727034,-0.384946794249528,
1.70815711505485));
#57362=CARTESIAN_POINT('Ctrl Pts',(0.211601258207602,-0.382404460057085,
1.72802051842006));
#57363=CARTESIAN_POINT('Ctrl Pts',(0.43602745309346,-0.0291333957915248,
1.74788392178528));
#57364=CARTESIAN_POINT('Ctrl Pts',(0.260721512662886,0.35056022726076,1.76774732515049));
#57365=CARTESIAN_POINT('Ctrl Pts',(-0.153622166966813,0.409422270130377,
1.7876107285157));
#57366=CARTESIAN_POINT('Ctrl Pts',(-0.427110629240823,0.0918260222046154,
1.80747413188091));
#57367=CARTESIAN_POINT('Ctrl Pts',(-0.34837074349523,-0.174337435012907,
1.82071640079106));
#57368=CARTESIAN_POINT('Ctrl Pts',(-0.261395148908821,-0.261333535452179,
1.82733753524613));
#57369=CARTESIAN_POINT('Ctrl Pts',(-0.174869447533108,0.35228619944509,
0.0533));
#57370=CARTESIAN_POINT('Ctrl Pts',(-0.292115409128916,0.294087108586458,
0.0599211344550711));
#57371=CARTESIAN_POINT('Ctrl Pts',(-0.461887844477417,0.0524142518454919,
0.0731634033652132));
#57372=CARTESIAN_POINT('Ctrl Pts',(-0.293925685792365,-0.36071486351649,
0.0930268067304267));
#57373=CARTESIAN_POINT('Ctrl Pts',(0.143895538330264,-0.442036261164184,
0.11289021009564));
#57374=CARTESIAN_POINT('Ctrl Pts',(0.449594182213621,-0.118662784868254,
0.132753613460853));
#57375=CARTESIAN_POINT('Ctrl Pts',(0.343220286313821,0.31378403469352,0.152617016826066));
#57376=CARTESIAN_POINT('Ctrl Pts',(-0.0778649948224021,0.458411940127677,
0.17248042019128));
#57377=CARTESIAN_POINT('Ctrl Pts',(-0.427536830618635,0.182855777752611,
0.192343823556493));
#57378=CARTESIAN_POINT('Ctrl Pts',(-0.385267518056549,-0.260378869128022,
0.212207226921706));
#57379=CARTESIAN_POINT('Ctrl Pts',(0.0102140801457829,-0.464882981564965,
0.232070630286919));
#57380=CARTESIAN_POINT('Ctrl Pts',(0.39632758681485,-0.243203939043049,
0.251934033652133));
#57381=CARTESIAN_POINT('Ctrl Pts',(0.419099077624518,0.201444690523449,
0.271797437017346));
#57382=CARTESIAN_POINT('Ctrl Pts',(0.0576489493923463,0.461410409723788,
0.291660840382559));
#57383=CARTESIAN_POINT('Ctrl Pts',(-0.35665185119459,0.298367105416454,
0.311524243747772));
#57384=CARTESIAN_POINT('Ctrl Pts',(-0.443982634529337,-0.138213198994076,
0.331387647112986));
#57385=CARTESIAN_POINT('Ctrl Pts',(-0.124280065414824,-0.44808235696456,
0.351251050478199));
#57386=CARTESIAN_POINT('Ctrl Pts',(0.309359563547165,-0.34716000793604,
0.371114453843412));
#57387=CARTESIAN_POINT('Ctrl Pts',(0.459385413093047,0.0720308674659688,
0.390977857208626));
#57388=CARTESIAN_POINT('Ctrl Pts',(0.188257126867579,0.425185419248763,
0.410841260573838));
#57389=CARTESIAN_POINT('Ctrl Pts',(-0.255461006172004,0.388539666498342,
0.430704663939053));
#57390=CARTESIAN_POINT('Ctrl Pts',(-0.464978296587002,-0.00431044471904228,
0.450568067304264));
#57391=CARTESIAN_POINT('Ctrl Pts',(-0.248214041707426,-0.39320882956985,
0.470431470669479));
#57392=CARTESIAN_POINT('Ctrl Pts',(0.19610720775623,-0.421622294127823,
0.490294874034691));
#57393=CARTESIAN_POINT('Ctrl Pts',(0.460641823813729,-0.0635020126079185,
0.510158277399905));
#57394=CARTESIAN_POINT('Ctrl Pts',(0.302870477030493,0.352835470659127,
0.530021680765118));
#57395=CARTESIAN_POINT('Ctrl Pts',(-0.132565644342568,0.445701408336244,
0.549885084130331));
#57396=CARTESIAN_POINT('Ctrl Pts',(-0.446468593814177,0.129958416886173,
0.569748487495545));
#57397=CARTESIAN_POINT('Ctrl Pts',(-0.351059276202315,-0.304927499495857,
0.589611890860758));
#57398=CARTESIAN_POINT('Ctrl Pts',(0.0661932128597544,-0.460262809665817,
0.609475294225972));
#57399=CARTESIAN_POINT('Ctrl Pts',(0.422761267709286,-0.193639628957789,
0.629338697591184));
#57400=CARTESIAN_POINT('Ctrl Pts',(0.39175139368343,0.250507965787189,0.649202100956398));
#57401=CARTESIAN_POINT('Ctrl Pts',(0.00159273903470509,0.464995546820308,
0.66906550432161));
#57402=CARTESIAN_POINT('Ctrl Pts',(-0.390026102590641,0.253185771077951,
0.688928907686825));
#57403=CARTESIAN_POINT('Ctrl Pts',(-0.424077871277783,-0.190738969460217,
0.708792311052037));
#57404=CARTESIAN_POINT('Ctrl Pts',(-0.0693446788490918,-0.459798554689087,
0.728655714417252));
#57405=CARTESIAN_POINT('Ctrl Pts',(0.348962140255506,-0.307325267504712,
0.748519117782463));
#57406=CARTESIAN_POINT('Ctrl Pts',(0.447348394484473,0.126896845235482,
0.768382521147677));
#57407=CARTESIAN_POINT('Ctrl Pts',(0.135615800420108,0.444782812229798,
0.788245924512891));
#57408=CARTESIAN_POINT('Ctrl Pts',(-0.300446279486727,0.354901998474468,
0.808109327878103));
#57409=CARTESIAN_POINT('Ctrl Pts',(-0.461066033822792,-0.0603449072707291,
0.827972731243318));
#57410=CARTESIAN_POINT('Ctrl Pts',(-0.198990919662619,-0.420268972528816,
0.84783613460853));
#57411=CARTESIAN_POINT('Ctrl Pts',(0.245514550343433,-0.394899988539195,
0.867699537973743));
#57412=CARTESIAN_POINT('Ctrl Pts',(0.464937856497831,-0.00749566366628734,
0.887562941338958));
#57413=CARTESIAN_POINT('Ctrl Pts',(0.258116695060824,0.386780515421183,
0.907426344704169));
#57414=CARTESIAN_POINT('Ctrl Pts',(-0.185339990296292,0.426465102177854,
0.927289748069384));
#57415=CARTESIAN_POINT('Ctrl Pts',(-0.458881181823084,0.0751761687454602,
0.947153151434596));
#57416=CARTESIAN_POINT('Ctrl Pts',(-0.311730527546589,-0.345032568859987,
0.96701655479981));
#57417=CARTESIAN_POINT('Ctrl Pts',(0.121207594644353,-0.448923283400548,
0.986879958165023));
#57418=CARTESIAN_POINT('Ctrl Pts',(0.44302534682202,-0.141251327256863,
1.00674336153024));
#57419=CARTESIAN_POINT('Ctrl Pts',(0.358687522622067,0.295916637744211,
1.02660676489545));
#57420=CARTESIAN_POINT('Ctrl Pts',(-0.0544868761329562,0.461794949850985,
1.04647016826066));
#57421=CARTESIAN_POINT('Ctrl Pts',(-0.417708944305668,0.204310139801323,
1.06633357162588));
#57422=CARTESIAN_POINT('Ctrl Pts',(-0.397984938964643,-0.24048156631205,
1.08619697499109));
#57423=CARTESIAN_POINT('Ctrl Pts',(-0.0133973802528527,-0.46480523402926,
1.1060603783563));
#57424=CARTESIAN_POINT('Ctrl Pts',(0.383472592405631,-0.263006019422102,
1.12592378172152));
#57425=CARTESIAN_POINT('Ctrl Pts',(0.428783601427445,0.179911140637417,
1.14578718508673));
#57426=CARTESIAN_POINT('Ctrl Pts',(0.080995542803804,0.457889852939299,
1.16565058845194));
#57427=CARTESIAN_POINT('Ctrl Pts',(-0.341047389965224,0.316085547243385,
1.18551399181716));
#57428=CARTESIAN_POINT('Ctrl Pts',(-0.450425821172375,-0.11549880951583,
1.20537739518237));
#57429=CARTESIAN_POINT('Ctrl Pts',(-0.14686408919024,-0.441196480818547,
1.22524079854758));
#57430=CARTESIAN_POINT('Ctrl Pts',(0.291339304317663,-0.362415238553024,
1.24510420191279));
#57431=CARTESIAN_POINT('Ctrl Pts',(0.462449440260866,0.0486200635590298,
1.26496760527801));
#57432=CARTESIAN_POINT('Ctrl Pts',(0.209596432103329,0.415081595640813,
1.28483100864322));
#57433=CARTESIAN_POINT('Ctrl Pts',(-0.235409824841565,0.401005747745034,
1.30469441200844));
#57434=CARTESIAN_POINT('Ctrl Pts',(-0.464597700788281,0.019296937689995,
1.32455781537365));
#57435=CARTESIAN_POINT('Ctrl Pts',(-0.26785295616762,-0.380102866767851,
1.34442121873886));
#57436=CARTESIAN_POINT('Ctrl Pts',(0.174453295424821,-0.431032995172465,
1.36428462210407));
#57437=CARTESIAN_POINT('Ctrl Pts',(0.45682472781543,-0.0868018635056573,
1.38414802546929));
#57438=CARTESIAN_POINT('Ctrl Pts',(0.320389624696148,0.337007246549112,
1.4040114288345));
#57439=CARTESIAN_POINT('Ctrl Pts',(-0.10977140987676,0.45185576429442,1.42387483219972));
#57440=CARTESIAN_POINT('Ctrl Pts',(-0.4392965090373,0.152453184218197,1.44373823556493));
#57441=CARTESIAN_POINT('Ctrl Pts',(-0.366084545357951,-0.286715021872099,
1.46360163893014));
#57442=CARTESIAN_POINT('Ctrl Pts',(0.0427454148328597,-0.463029390070381,
1.48346504229536));
#57443=CARTESIAN_POINT('Ctrl Pts',(0.412387350445995,-0.214848962815045,
1.50332844566057));
#57444=CARTESIAN_POINT('Ctrl Pts',(0.403961927122641,0.230300178253525,
1.52319184902578));
#57445=CARTESIAN_POINT('Ctrl Pts',(0.025193386907632,0.464315223246611,
1.54305525239099));
#57446=CARTESIAN_POINT('Ctrl Pts',(-0.376671884924722,0.272656852558385,
1.56291865575621));
#57447=CARTESIAN_POINT('Ctrl Pts',(-0.433212914498574,-0.168967580519975,
1.58278205912142));
#57448=CARTESIAN_POINT('Ctrl Pts',(-0.0925942073198233,-0.455685505955948,
1.60264546248664));
#57449=CARTESIAN_POINT('Ctrl Pts',(0.332912813233796,-0.324642971571184,
1.62250886585185));
#57450=CARTESIAN_POINT('Ctrl Pts',(0.453212837270372,0.104028054725039,
1.64237226921706));
#57451=CARTESIAN_POINT('Ctrl Pts',(0.158017797927116,0.437322409121946,
1.66223567258227));
#57452=CARTESIAN_POINT('Ctrl Pts',(-0.282044701269876,0.369701234030167,
1.68209907594749));
#57453=CARTESIAN_POINT('Ctrl Pts',(-0.463534388325307,-0.0368761146654934,
1.7019624793127));
#57454=CARTESIAN_POINT('Ctrl Pts',(-0.220067494029471,-0.409603176674573,
1.72182588267792));
#57455=CARTESIAN_POINT('Ctrl Pts',(0.225154615767464,-0.406898002409068,
1.74168928604313));
#57456=CARTESIAN_POINT('Ctrl Pts',(0.463955623406581,-0.0309994306792224,
1.76155268940834));
#57457=CARTESIAN_POINT('Ctrl Pts',(0.277421091458407,0.373014101810366,
1.78141609277355));
#57458=CARTESIAN_POINT('Ctrl Pts',(-0.16346188236198,0.435646341135685,
1.80127949613877));
#57459=CARTESIAN_POINT('Ctrl Pts',(-0.454467664471872,0.0977076078000029,
1.82114289950398));
#57460=CARTESIAN_POINT('Ctrl Pts',(-0.370684378536826,-0.185503992399258,
1.83438516841412));
#57461=CARTESIAN_POINT('Ctrl Pts',(-0.278137875051309,-0.278072315166294,
1.84100630286919));
#57462=CARTESIAN_POINT('',(-0.114300952321843,0.376324570415379,1.8));
#57463=CARTESIAN_POINT('Ctrl Pts',(-0.114617201976748,0.376923011799598,
1.8));
#57464=CARTESIAN_POINT('Ctrl Pts',(-0.122438613579645,0.373814783061767,
1.8));
#57465=CARTESIAN_POINT('Ctrl Pts',(-0.130137853077703,0.370443137950288,
1.8));
#57466=CARTESIAN_POINT('Ctrl Pts',(-0.137702035174531,0.366805935526825,
1.8));
#57467=CARTESIAN_POINT('Ctrl Pts',(-0.157131838454901,0.357463203335275,
1.8));
#57468=CARTESIAN_POINT('Ctrl Pts',(-0.175673019394112,0.346371270199071,
1.8));
#57469=CARTESIAN_POINT('Ctrl Pts',(-0.193189853500601,0.333742567265917,
1.8));
#57470=CARTESIAN_POINT('Ctrl Pts',(-0.203658595767835,0.326195162559511,
1.8));
#57471=CARTESIAN_POINT('Ctrl Pts',(-0.213760867036217,0.318097980230398,
1.8));
#57472=CARTESIAN_POINT('Ctrl Pts',(-0.223460905504529,0.309490823080894,
1.8));
#57473=CARTESIAN_POINT('Ctrl Pts',(-0.228445288511021,0.30506801919508,
1.8));
#57474=CARTESIAN_POINT('Ctrl Pts',(-0.233323372737349,0.30051050816285,
1.8));
#57475=CARTESIAN_POINT('Ctrl Pts',(-0.238089676004254,0.295823442462311,
1.8));
#57476=CARTESIAN_POINT('Ctrl Pts',(-0.242014920947028,0.291963452883965,
1.8));
#57477=CARTESIAN_POINT('Ctrl Pts',(-0.245858070184263,0.288021683976271,
1.8));
#57478=CARTESIAN_POINT('Ctrl Pts',(-0.249613876501175,0.284004910638523,
1.8));
#57479=CARTESIAN_POINT('Ctrl Pts',(-0.264084819509805,0.268528474117447,
1.8));
#57480=CARTESIAN_POINT('Ctrl Pts',(-0.277277817225154,0.251925602751329,
1.8));
#57481=CARTESIAN_POINT('Ctrl Pts',(-0.289049676537754,0.23438536611199,
1.8));
#57482=CARTESIAN_POINT('Ctrl Pts',(-0.29705015058476,0.222464546784734,
1.8));
#57483=CARTESIAN_POINT('Ctrl Pts',(-0.304393399646152,0.210110059716389,
1.8));
#57484=CARTESIAN_POINT('Ctrl Pts',(-0.311021403614141,0.197377127459023,
1.8));
#57485=CARTESIAN_POINT('Ctrl Pts',(-0.314228507045358,0.191216022105243,
1.8));
#57486=CARTESIAN_POINT('Ctrl Pts',(-0.317267976480838,0.184966286029691,
1.8));
#57487=CARTESIAN_POINT('Ctrl Pts',(-0.320132207960069,0.178634142888421,
1.8));
#57488=CARTESIAN_POINT('Ctrl Pts',(-0.322113958988996,0.174252956773918,
1.8));
#57489=CARTESIAN_POINT('Ctrl Pts',(-0.324010248252346,0.169835507334254,
1.8));
#57490=CARTESIAN_POINT('Ctrl Pts',(-0.325816003087781,0.1653916009695,1.8));
#57491=CARTESIAN_POINT('Ctrl Pts',(-0.333354523194409,0.146839537962231,
1.8));
#57492=CARTESIAN_POINT('Ctrl Pts',(-0.339336883851923,0.127787956818189,
1.8));
#57493=CARTESIAN_POINT('Ctrl Pts',(-0.343615830426459,0.108394982215767,
1.8));
#57494=CARTESIAN_POINT('Ctrl Pts',(-0.346015117263807,0.0975209720148686,
1.8));
#57495=CARTESIAN_POINT('Ctrl Pts',(-0.347877980992209,0.0865394609170954,
1.8));
#57496=CARTESIAN_POINT('Ctrl Pts',(-0.349171180768184,0.075478399293499,
1.8));
#57497=CARTESIAN_POINT('Ctrl Pts',(-0.350451949842727,0.0645236605730705,
1.8));
#57498=CARTESIAN_POINT('Ctrl Pts',(-0.351173826587271,0.0534908072357066,
1.8));
#57499=CARTESIAN_POINT('Ctrl Pts',(-0.351345950689055,0.0424165497826654,
1.8));
#57500=CARTESIAN_POINT('Ctrl Pts',(-0.351425035191472,0.0373283481233097,
1.8));
#57501=CARTESIAN_POINT('Ctrl Pts',(-0.351387829017759,0.0322398913435546,
1.8));
#57502=CARTESIAN_POINT('Ctrl Pts',(-0.351236346246636,0.0271582460828918,
1.8));
#57503=CARTESIAN_POINT('Ctrl Pts',(-0.350642909162813,0.00725078913467943,
1.8));
#57504=CARTESIAN_POINT('Ctrl Pts',(-0.348299967417274,-0.012571236927833,
1.8));
#57505=CARTESIAN_POINT('Ctrl Pts',(-0.344298540808079,-0.0320964970107567,
1.8));
#57506=CARTESIAN_POINT('Ctrl Pts',(-0.34158866400112,-0.0453195433430291,
1.8));
#57507=CARTESIAN_POINT('Ctrl Pts',(-0.338116987271259,-0.0584063854402795,
1.8));
#57508=CARTESIAN_POINT('Ctrl Pts',(-0.333899902424356,-0.07128511617414,
1.8));
#57509=CARTESIAN_POINT('Ctrl Pts',(-0.331891313091662,-0.0774192306417845,
1.8));
#57510=CARTESIAN_POINT('Ctrl Pts',(-0.329713494344077,-0.0835060326977867,
1.8));
#57511=CARTESIAN_POINT('Ctrl Pts',(-0.327367582606868,-0.0895371018240274,
1.8));
#57512=CARTESIAN_POINT('Ctrl Pts',(-0.325415778789272,-0.0945549648399598,
1.8));
#57513=CARTESIAN_POINT('Ctrl Pts',(-0.323351086569145,-0.0995252754617292,
1.8));
#57514=CARTESIAN_POINT('Ctrl Pts',(-0.321175405691638,-0.104442985850223,
1.8));
#57515=CARTESIAN_POINT('Ctrl Pts',(-0.315899089074665,-0.116369090137169,
1.8));
#57516=CARTESIAN_POINT('Ctrl Pts',(-0.309969963495991,-0.127987830133287,
1.8));
#57517=CARTESIAN_POINT('Ctrl Pts',(-0.303405158120671,-0.139233631733587,
1.8));
#57518=CARTESIAN_POINT('Ctrl Pts',(-0.299533235856367,-0.145866405609847,
1.8));
#57519=CARTESIAN_POINT('Ctrl Pts',(-0.295440032784457,-0.152369323019986,
1.8));
#57520=CARTESIAN_POINT('Ctrl Pts',(-0.291127918360532,-0.158727583407761,
1.8));
#57521=CARTESIAN_POINT('Ctrl Pts',(-0.287043388654486,-0.164750267613112,
1.8));
#57522=CARTESIAN_POINT('Ctrl Pts',(-0.282760740964221,-0.170644775881678,
1.8));
#57523=CARTESIAN_POINT('Ctrl Pts',(-0.278296041684024,-0.176380379709159,
1.8));
#57524=CARTESIAN_POINT('Ctrl Pts',(-0.266967254489208,-0.190933976965644,
1.8));
#57525=CARTESIAN_POINT('Ctrl Pts',(-0.254451318609441,-0.204494493516429,
1.8));
#57526=CARTESIAN_POINT('Ctrl Pts',(-0.240784361479587,-0.216852648005559,
1.8));
#57527=CARTESIAN_POINT('Ctrl Pts',(-0.236600651283484,-0.220635709330032,
1.8));
#57528=CARTESIAN_POINT('Ctrl Pts',(-0.232308897488585,-0.224305786482091,
1.8));
#57529=CARTESIAN_POINT('Ctrl Pts',(-0.227909696623847,-0.227855976023948,
1.8));
#57530=CARTESIAN_POINT('Ctrl Pts',(-0.393842938295855,-0.000187384875455676,
1.7003836477965));
#57531=CARTESIAN_POINT('Ctrl Pts',(-0.393902902551742,-0.0105512319322723,
1.70090992496857));
#57532=CARTESIAN_POINT('Ctrl Pts',(-0.393529328713883,-0.0209106376201641,
1.70143620214063));
#57533=CARTESIAN_POINT('Ctrl Pts',(-0.392708291433429,-0.0312344002177303,
1.7019624793127));
#57534=CARTESIAN_POINT('Ctrl Pts',(-0.382378756893362,-0.161118468668519,
1.70858361376777));
#57535=CARTESIAN_POINT('Ctrl Pts',(-0.301223125461419,-0.285360822671543,
1.71520474822284));
#57536=CARTESIAN_POINT('Ctrl Pts',(-0.186441624779293,-0.347031137295473,
1.72182588267791));
#57537=CARTESIAN_POINT('Ctrl Pts',(-0.0716601240971649,-0.408701451919404,
1.72844701713299));
#57538=CARTESIAN_POINT('Ctrl Pts',(0.0767472458351461,-0.407799727164238,
1.73506815158806));
#57539=CARTESIAN_POINT('Ctrl Pts',(0.190751098741156,-0.344699102831681,
1.74168928604313));
#57540=CARTESIAN_POINT('Ctrl Pts',(0.304754951647168,-0.281598478499124,
1.7483104204982));
#57541=CARTESIAN_POINT('Ctrl Pts',(0.384355287526875,-0.156298954589174,
1.75493155495327));
#57542=CARTESIAN_POINT('Ctrl Pts',(0.393066366808699,-0.0263136038859339,
1.76155268940834));
#57543=CARTESIAN_POINT('Ctrl Pts',(0.401777446090523,0.103671746817305,
1.76817382386341));
#57544=CARTESIAN_POINT('Ctrl Pts',(0.339599268774464,0.238342924313838,
1.77479495831848));
#57545=CARTESIAN_POINT('Ctrl Pts',(0.235029684479703,0.316117219616322,
1.78141609277355));
#57546=CARTESIAN_POINT('Ctrl Pts',(0.137195923693007,0.388881703221125,
1.7876107285157));
#57547=CARTESIAN_POINT('Ctrl Pts',(0.00225612663044948,0.411843221433994,
1.79380536425785));
#57548=CARTESIAN_POINT('Ctrl Pts',(-0.114617201976764,0.376923011799593,
1.8));
#57549=CARTESIAN_POINT('',(-0.187158653173899,-0.262360084935061,0.0533));
#57550=CARTESIAN_POINT('Ctrl Pts',(-0.187560716198532,-0.262742134024652,
0.0533));
#57551=CARTESIAN_POINT('Ctrl Pts',(-0.193636511193937,-0.259359136538732,
0.0533));
#57552=CARTESIAN_POINT('Ctrl Pts',(-0.19958510398352,-0.255771278629542,
0.0533));
#57553=CARTESIAN_POINT('Ctrl Pts',(-0.205394875738649,-0.251980685507045,
0.0533));
#57554=CARTESIAN_POINT('Ctrl Pts',(-0.217956745144151,-0.243784677508594,
0.0533));
#57555=CARTESIAN_POINT('Ctrl Pts',(-0.229870284953525,-0.234642384833593,
0.0533));
#57556=CARTESIAN_POINT('Ctrl Pts',(-0.241105135118966,-0.224672721347691,
0.0533));
#57557=CARTESIAN_POINT('Ctrl Pts',(-0.245472230993061,-0.220797415879949,
0.0533));
#57558=CARTESIAN_POINT('Ctrl Pts',(-0.249736686373294,-0.216796863541336,
0.0533000000000001));
#57559=CARTESIAN_POINT('Ctrl Pts',(-0.253896307158604,-0.212677223544441,
0.0533000000000001));
#57560=CARTESIAN_POINT('Ctrl Pts',(-0.258330366693657,-0.208285782604984,
0.0533000000000001));
#57561=CARTESIAN_POINT('Ctrl Pts',(-0.262639027648536,-0.203765130777088,
0.0533000000000001));
#57562=CARTESIAN_POINT('Ctrl Pts',(-0.266817483432449,-0.199126826877465,
0.0533000000000001));
#57563=CARTESIAN_POINT('Ctrl Pts',(-0.275301291296798,-0.18970935756922,
0.0533000000000001));
#57564=CARTESIAN_POINT('Ctrl Pts',(-0.283252555387633,-0.17980358772735,
0.0533));
#57565=CARTESIAN_POINT('Ctrl Pts',(-0.290652088370279,-0.169475045182507,
0.0533));
#57566=CARTESIAN_POINT('Ctrl Pts',(-0.295150312948837,-0.163196256501539,
0.0533));
#57567=CARTESIAN_POINT('Ctrl Pts',(-0.29944455411437,-0.156761050609704,
0.0533));
#57568=CARTESIAN_POINT('Ctrl Pts',(-0.303529464395936,-0.150182734495315,
0.0533));
#57569=CARTESIAN_POINT('Ctrl Pts',(-0.307092531148336,-0.144444792210579,
0.0533));
#57570=CARTESIAN_POINT('Ctrl Pts',(-0.310497232713595,-0.138595640257259,
0.0533));
#57571=CARTESIAN_POINT('Ctrl Pts',(-0.313728903073767,-0.132664844733238,
0.0533));
#57572=CARTESIAN_POINT('Ctrl Pts',(-0.323341236409495,-0.115024189230276,
0.0533));
#57573=CARTESIAN_POINT('Ctrl Pts',(-0.331449415040724,-0.0966280872271142,
0.0533));
#57574=CARTESIAN_POINT('Ctrl Pts',(-0.337977761615037,-0.0777141154187473,
0.0533));
#57575=CARTESIAN_POINT('Ctrl Pts',(-0.34214350835192,-0.0656450845477116,
0.0533));
#57576=CARTESIAN_POINT('Ctrl Pts',(-0.345665382203141,-0.0533642266892958,
0.0533000000000001));
#57577=CARTESIAN_POINT('Ctrl Pts',(-0.348515086834976,-0.0409264571618923,
0.0533000000000001));
#57578=CARTESIAN_POINT('Ctrl Pts',(-0.350083642823025,-0.0340803659381738,
0.0533000000000001));
#57579=CARTESIAN_POINT('Ctrl Pts',(-0.351448420077869,-0.0271866616054783,
0.0533));
#57580=CARTESIAN_POINT('Ctrl Pts',(-0.352603627980865,-0.0202541240282325,
0.0533));
#57581=CARTESIAN_POINT('Ctrl Pts',(-0.353341821950461,-0.0158241357808845,
0.0533));
#57582=CARTESIAN_POINT('Ctrl Pts',(-0.353994073919582,-0.011379600904418,
0.0533));
#57583=CARTESIAN_POINT('Ctrl Pts',(-0.354557987170772,-0.00693268604601465,
0.0533));
#57584=CARTESIAN_POINT('Ctrl Pts',(-0.356544004100534,0.00872867352545007,
0.0533));
#57585=CARTESIAN_POINT('Ctrl Pts',(-0.357441243642084,0.0244515531282482,
0.0533));
#57586=CARTESIAN_POINT('Ctrl Pts',(-0.357208358621734,0.0401306151146961,
0.0533));
#57587=CARTESIAN_POINT('Ctrl Pts',(-0.356976992543487,0.0557074138153622,
0.0533));
#57588=CARTESIAN_POINT('Ctrl Pts',(-0.355630556643009,0.0712413952181323,
0.0533));
#57589=CARTESIAN_POINT('Ctrl Pts',(-0.353239351858838,0.0866540484795216,
0.0533));
#57590=CARTESIAN_POINT('Ctrl Pts',(-0.352085419540309,0.0940917881621845,
0.0533));
#57591=CARTESIAN_POINT('Ctrl Pts',(-0.350687882387897,0.101501314598154,
0.0533));
#57592=CARTESIAN_POINT('Ctrl Pts',(-0.349053024053041,0.10887384878209,
0.0533));
#57593=CARTESIAN_POINT('Ctrl Pts',(-0.347355284894117,0.116529949447026,
0.0533));
#57594=CARTESIAN_POINT('Ctrl Pts',(-0.345399312227588,0.124152796342384,
0.0533));
#57595=CARTESIAN_POINT('Ctrl Pts',(-0.343202678426538,0.131696252532374,
0.0533));
#57596=CARTESIAN_POINT('Ctrl Pts',(-0.33743136038184,0.151515525461643,
0.0533));
#57597=CARTESIAN_POINT('Ctrl Pts',(-0.329997551557849,0.170823614573644,
0.0533));
#57598=CARTESIAN_POINT('Ctrl Pts',(-0.321061225945632,0.189447349149852,
0.0533));
#57599=CARTESIAN_POINT('Ctrl Pts',(-0.313086943720081,0.206066138801092,
0.0533));
#57600=CARTESIAN_POINT('Ctrl Pts',(-0.303915204286004,0.222140756471803,
0.0533));
#57601=CARTESIAN_POINT('Ctrl Pts',(-0.2936268562705,0.237543508329172,0.0533));
#57602=CARTESIAN_POINT('Ctrl Pts',(-0.290722215070209,0.241892065315711,
0.0533));
#57603=CARTESIAN_POINT('Ctrl Pts',(-0.287728400765138,0.246187004087764,
0.0533));
#57604=CARTESIAN_POINT('Ctrl Pts',(-0.284646842060306,0.250425257901783,
0.0533));
#57605=CARTESIAN_POINT('Ctrl Pts',(-0.281599100702271,0.254617000676173,
0.0533));
#57606=CARTESIAN_POINT('Ctrl Pts',(-0.278470738930216,0.258746075409449,
0.0533));
#57607=CARTESIAN_POINT('Ctrl Pts',(-0.275265448025107,0.262808141138579,
0.0533));
#57608=CARTESIAN_POINT('Ctrl Pts',(-0.261269669386206,0.280544993875083,
0.0533));
#57609=CARTESIAN_POINT('Ctrl Pts',(-0.245803353568857,0.297017252463422,
0.0533));
#57610=CARTESIAN_POINT('Ctrl Pts',(-0.229026180874183,0.312007620837193,
0.0533000000000001));
#57611=CARTESIAN_POINT('Ctrl Pts',(-0.213164506043965,0.326179993802361,
0.0533000000000001));
#57612=CARTESIAN_POINT('Ctrl Pts',(-0.196130043934341,0.339029002927305,
0.0533));
#57613=CARTESIAN_POINT('Ctrl Pts',(-0.178016632246539,0.350342635307754,
0.0533));
#57614=CARTESIAN_POINT('Ctrl Pts',(-0.176971169526133,0.350995631059742,
0.0533));
#57615=CARTESIAN_POINT('Ctrl Pts',(-0.175922103056024,0.351643500814262,
0.0533));
#57616=CARTESIAN_POINT('Ctrl Pts',(-0.174869447533108,0.35228619944509,
0.0533));
#57617=CARTESIAN_POINT('Ctrl Pts',(-0.18756071619853,-0.262742134024653,
0.0533000000000001));
#57618=CARTESIAN_POINT('Ctrl Pts',(-0.105929749524472,-0.320418481561441,
0.059494635742149));
#57619=CARTESIAN_POINT('Ctrl Pts',(0.123288314644033,-0.356520648444787,
0.0723104059393689));
#57620=CARTESIAN_POINT('Ctrl Pts',(0.368403165707845,-0.0972337884399037,
0.09174731059166));
#57621=CARTESIAN_POINT('Ctrl Pts',(0.281239048491698,0.257118611189565,
0.111610713956873));
#57622=CARTESIAN_POINT('Ctrl Pts',(-0.0638035626910551,0.375628548193864,
0.131474117322087));
#57623=CARTESIAN_POINT('Ctrl Pts',(-0.293478189192993,0.194635250493208,
0.147396327645565));
#57624=CARTESIAN_POINT('Ctrl Pts',(-0.322017574433746,0.0437179398416368,
0.156697403513973));
#57625=CARTESIAN_POINT('Ctrl Pts',(-0.321822258325956,0.00016257495858928,
0.15937734492731));
#57626=CARTESIAN_POINT('Origin',(-5.160062080289E-17,2.1385152528819E-17,
0.0533));
#57627=CARTESIAN_POINT('',(-0.3933,-4.81653586104654E-17,0.0533000000000001));
#57628=CARTESIAN_POINT('Origin',(0.,0.,0.0533));
#57629=CARTESIAN_POINT('Origin',(0.,0.,0.0533));
#57630=CARTESIAN_POINT('',(0.187158653173902,-0.262360084935058,0.0533));
#57631=CARTESIAN_POINT('Ctrl Pts',(0.175280092543415,0.352824285593914,
0.0533));
#57632=CARTESIAN_POINT('Ctrl Pts',(0.182476661777002,0.348469857043458,
0.0533));
#57633=CARTESIAN_POINT('Ctrl Pts',(0.189513753595691,0.343873471838117,
0.0532999999999999));
#57634=CARTESIAN_POINT('Ctrl Pts',(0.196377574736944,0.339034381908458,
0.0532999999999999));
#57635=CARTESIAN_POINT('Ctrl Pts',(0.209106724890824,0.330060152968759,
0.0532999999999999));
#57636=CARTESIAN_POINT('Ctrl Pts',(0.221240628245203,0.320251656613418,
0.0533));
#57637=CARTESIAN_POINT('Ctrl Pts',(0.232739197742172,0.309694329310758,
0.0533));
#57638=CARTESIAN_POINT('Ctrl Pts',(0.23985544575162,0.303160598360795,0.0533));
#57639=CARTESIAN_POINT('Ctrl Pts',(0.246728142345483,0.296339860335349,
0.0533));
#57640=CARTESIAN_POINT('Ctrl Pts',(0.25334550097625,0.289251071117036,0.0533));
#57641=CARTESIAN_POINT('Ctrl Pts',(0.257726631531975,0.284557822227207,
0.0533));
#57642=CARTESIAN_POINT('Ctrl Pts',(0.261988647138667,0.279754733652569,
0.0533000000000001));
#57643=CARTESIAN_POINT('Ctrl Pts',(0.266128947248262,0.274848072424167,
0.0533));
#57644=CARTESIAN_POINT('Ctrl Pts',(0.280033143836886,0.258370237362071,
0.0533));
#57645=CARTESIAN_POINT('Ctrl Pts',(0.292568657834103,0.24072534694436,0.0533));
#57646=CARTESIAN_POINT('Ctrl Pts',(0.303609786261102,0.222132165374485,
0.0533));
#57647=CARTESIAN_POINT('Ctrl Pts',(0.306585509497727,0.21712106865497,0.0533));
#57648=CARTESIAN_POINT('Ctrl Pts',(0.309453480170002,0.212038981971964,
0.0533));
#57649=CARTESIAN_POINT('Ctrl Pts',(0.312207122974928,0.206896593722832,
0.0533));
#57650=CARTESIAN_POINT('Ctrl Pts',(0.322145270739341,0.188337246014253,
0.0533));
#57651=CARTESIAN_POINT('Ctrl Pts',(0.33056064005666,0.169066507843323,0.0533000000000001));
#57652=CARTESIAN_POINT('Ctrl Pts',(0.337346359383174,0.149290670646457,
0.0533000000000001));
#57653=CARTESIAN_POINT('Ctrl Pts',(0.343948622498527,0.130049485708268,
0.0533000000000001));
#57654=CARTESIAN_POINT('Ctrl Pts',(0.349008411343874,0.11032878114862,0.0533));
#57655=CARTESIAN_POINT('Ctrl Pts',(0.352378978874987,0.0903158693762518,
0.0533));
#57656=CARTESIAN_POINT('Ctrl Pts',(0.353314918731474,0.0847586800901094,
0.0533));
#57657=CARTESIAN_POINT('Ctrl Pts',(0.354120303577725,0.0791790087202579,
0.0533));
#57658=CARTESIAN_POINT('Ctrl Pts',(0.354791265827591,0.0735810373368519,
0.0533));
#57659=CARTESIAN_POINT('Ctrl Pts',(0.355398841269737,0.0685119146864081,
0.0533));
#57660=CARTESIAN_POINT('Ctrl Pts',(0.355894985776107,0.0634376947345237,
0.0533));
#57661=CARTESIAN_POINT('Ctrl Pts',(0.356277894215268,0.05836243273793,0.0533));
#57662=CARTESIAN_POINT('Ctrl Pts',(0.357324187933274,0.0444943269424352,
0.0533));
#57663=CARTESIAN_POINT('Ctrl Pts',(0.357526229414497,0.0306157185946321,
0.0533));
#57664=CARTESIAN_POINT('Ctrl Pts',(0.356841349994185,0.0167882255892583,
0.0533));
#57665=CARTESIAN_POINT('Ctrl Pts',(0.355823943567287,-0.00375287965396633,
0.0533));
#57666=CARTESIAN_POINT('Ctrl Pts',(0.352851156603884,-0.0241829177690499,
0.0533));
#57667=CARTESIAN_POINT('Ctrl Pts',(0.348040392606845,-0.0442816943231375,
0.0533));
#57668=CARTESIAN_POINT('Ctrl Pts',(0.346677645286907,-0.0499750839593708,
0.0533));
#57669=CARTESIAN_POINT('Ctrl Pts',(0.345167119967579,-0.0556417158423305,
0.0533000000000001));
#57670=CARTESIAN_POINT('Ctrl Pts',(0.343510841709222,-0.0612760897393585,
0.0533000000000001));
#57671=CARTESIAN_POINT('Ctrl Pts',(0.342016897594177,-0.0663582307883981,
0.0533000000000001));
#57672=CARTESIAN_POINT('Ctrl Pts',(0.340406836566637,-0.0714055112317436,
0.0533));
#57673=CARTESIAN_POINT('Ctrl Pts',(0.338684647603792,-0.0764102645429386,
0.0533));
#57674=CARTESIAN_POINT('Ctrl Pts',(0.332034323863772,-0.0957363840782725,
0.0533));
#57675=CARTESIAN_POINT('Ctrl Pts',(0.323709882928168,-0.114451208546047,
0.0533));
#57676=CARTESIAN_POINT('Ctrl Pts',(0.313836238571883,-0.13233991066745,
0.0533));
#57677=CARTESIAN_POINT('Ctrl Pts',(0.305752963403788,-0.14698488839093,
0.0533));
#57678=CARTESIAN_POINT('Ctrl Pts',(0.296630038821398,-0.161076128885772,
0.0533));
#57679=CARTESIAN_POINT('Ctrl Pts',(0.286516038219096,-0.174473672389921,
0.0533));
#57680=CARTESIAN_POINT('Ctrl Pts',(0.283304266742829,-0.178728155830319,
0.0533000000000001));
#57681=CARTESIAN_POINT('Ctrl Pts',(0.279991464896629,-0.182913345906162,
0.0533000000000001));
#57682=CARTESIAN_POINT('Ctrl Pts',(0.27659067946394,-0.187011031331933,
0.0533000000000001));
#57683=CARTESIAN_POINT('Ctrl Pts',(0.264023874271964,-0.20215306704777,
0.0533000000000001));
#57684=CARTESIAN_POINT('Ctrl Pts',(0.250225650942623,-0.216149152210811,
0.0533000000000001));
#57685=CARTESIAN_POINT('Ctrl Pts',(0.235292709668539,-0.228787207872994,
0.0533000000000001));
#57686=CARTESIAN_POINT('Ctrl Pts',(0.221444282279375,-0.240507417104762,
0.0533000000000001));
#57687=CARTESIAN_POINT('Ctrl Pts',(0.206618876313766,-0.251060092225123,
0.0533));
#57688=CARTESIAN_POINT('Ctrl Pts',(0.190874522418597,-0.260231075837034,
0.0533));
#57689=CARTESIAN_POINT('Ctrl Pts',(0.189641532568663,-0.260949284395015,
0.0533));
#57690=CARTESIAN_POINT('Ctrl Pts',(0.188402901061074,-0.261658992964495,
0.0533));
#57691=CARTESIAN_POINT('Ctrl Pts',(0.187158653173906,-0.262360084935055,
0.0533));
#57692=CARTESIAN_POINT('Origin',(0.,0.,0.0533));
#57693=CARTESIAN_POINT('Origin',(0.,0.,-0.177777344927309));
#57694=CARTESIAN_POINT('Ctrl Pts',(0.187158653173902,-0.262360084935059,
0.0532999999999997));
#57695=CARTESIAN_POINT('Ctrl Pts',(0.274475898331453,-0.200070968026944,
0.0599211344550708));
#57696=CARTESIAN_POINT('Ctrl Pts',(0.380505034319934,0.0174746478065457,
0.0731634033652129));
#57697=CARTESIAN_POINT('Ctrl Pts',(0.191046375307344,0.329958431462181,
0.0930268067304262));
#57698=CARTESIAN_POINT('Ctrl Pts',(-0.173733796622045,0.338991571911486,
0.11289021009564));
#57699=CARTESIAN_POINT('Ctrl Pts',(-0.31746347429697,0.128188891668771,
0.126788826209727));
#57700=CARTESIAN_POINT('Ctrl Pts',(-0.322744636658635,0.0107979212988577,
0.134066307868744));
#57701=CARTESIAN_POINT('Ctrl Pts',(-0.322672883777213,0.000203620636067221,
0.13472265507269));
#57702=CARTESIAN_POINT('Ctrl Pts',(0.22840585926086,-0.320180657528383,
0.0122936971308065));
#57703=CARTESIAN_POINT('Ctrl Pts',(0.334966630404962,-0.244163871615853,
0.0189148315858776));
#57704=CARTESIAN_POINT('Ctrl Pts',(0.464363137066263,0.0213258210606221,
0.0321571004960198));
#57705=CARTESIAN_POINT('Ctrl Pts',(0.23315038215307,0.402676754616631,0.052020503861233));
#57706=CARTESIAN_POINT('Ctrl Pts',(-0.212022348030248,0.413700675611787,
0.0718839072264463));
#57707=CARTESIAN_POINT('Ctrl Pts',(-0.462705925125873,0.0460329065091048,
0.0917473105916596));
#57708=CARTESIAN_POINT('Ctrl Pts',(-0.289249672288166,-0.364136268728332,
0.111610713956873));
#57709=CARTESIAN_POINT('Ctrl Pts',(0.14941461449446,-0.440317672487742,
0.131474117322086));
#57710=CARTESIAN_POINT('Ctrl Pts',(0.451083062083358,-0.112907133063045,
0.151337520687299));
#57711=CARTESIAN_POINT('Ctrl Pts',(0.33921710497643,0.318056509301725,0.171200924052513));
#57712=CARTESIAN_POINT('Ctrl Pts',(-0.0836397209497935,0.457411044844623,
0.191064327417726));
#57713=CARTESIAN_POINT('Ctrl Pts',(-0.429815290904552,0.177433063463184,
0.210927730782939));
#57714=CARTESIAN_POINT('Ctrl Pts',(-0.38194714237817,-0.265217541271947,
0.230791134148153));
#57715=CARTESIAN_POINT('Ctrl Pts',(0.0160820867132626,-0.46471958682769,
0.250654537513365));
#57716=CARTESIAN_POINT('Ctrl Pts',(0.399367303186648,-0.238178907900465,
0.270517940878579));
#57717=CARTESIAN_POINT('Ctrl Pts',(0.416521813498203,0.206719639214314,
0.290381344243792));
#57718=CARTESIAN_POINT('Ctrl Pts',(0.0518184975661857,0.462101870037031,
0.310244747609006));
#57719=CARTESIAN_POINT('Ctrl Pts',(-0.360390794541395,0.293839833855819,
0.330108150974218));
#57720=CARTESIAN_POINT('Ctrl Pts',(-0.442202014837683,-0.143808009927119,
0.349971554339432));
#57721=CARTESIAN_POINT('Ctrl Pts',(-0.118612458427808,-0.449615872942682,
0.369834957704645));
#57722=CARTESIAN_POINT('Ctrl Pts',(0.313718299585274,-0.343226147934731,
0.389698361069858));
#57723=CARTESIAN_POINT('Ctrl Pts',(0.458439248795996,0.0778255316871185,
0.409561764435072));
#57724=CARTESIAN_POINT('Ctrl Pts',(0.182873504606443,0.427528522373788,
0.429425167800285));
#57725=CARTESIAN_POINT('Ctrl Pts',(-0.260346514431703,0.385283078075547,
0.449288571165498));
#57726=CARTESIAN_POINT('Ctrl Pts',(-0.464886762270973,-0.0101811444492372,
0.469151974530712));
#57727=CARTESIAN_POINT('Ctrl Pts',(-0.243229384295824,-0.39631152369195,
0.489015377895925));
#57728=CARTESIAN_POINT('Ctrl Pts',(0.201415169066835,-0.419112499346427,
0.508878781261138));
#57729=CARTESIAN_POINT('Ctrl Pts',(0.461406869855159,-0.0576806537548328,
0.528742184626351));
#57730=CARTESIAN_POINT('Ctrl Pts',(0.298391231378055,0.356631505027496,
0.548605587991565));
#57731=CARTESIAN_POINT('Ctrl Pts',(-0.138182711217647,0.443991999585549,
0.568468991356778));
#57732=CARTESIAN_POINT('Ctrl Pts',(-0.448073882458741,0.124310712416823,
0.588332394721992));
#57733=CARTESIAN_POINT('Ctrl Pts',(-0.347181094503187,-0.309335812638073,
0.608195798087204));
#57734=CARTESIAN_POINT('Ctrl Pts',(0.0719994360289554,-0.459390290033479,
0.628059201452418));
#57735=CARTESIAN_POINT('Ctrl Pts',(0.425172518796839,-0.188286182773711,
0.64792260481763));
#57736=CARTESIAN_POINT('Ctrl Pts',(0.38855709246268,0.255434420664781,0.667786008182846));
#57737=CARTESIAN_POINT('Ctrl Pts',(-0.0042786516855454,0.464978548433987,
0.687649411548056));
#57738=CARTESIAN_POINT('Ctrl Pts',(-0.393191825141502,0.248240903167881,
0.707512814913272));
#57739=CARTESIAN_POINT('Ctrl Pts',(-0.42163566312281,-0.196078364300367,
0.727376218278484));
#57740=CARTESIAN_POINT('Ctrl Pts',(-0.0635335009589411,-0.460637440531813,
0.747239621643697));
#57741=CARTESIAN_POINT('Ctrl Pts',(0.352814731969012,-0.302894572862218,
0.76710302500891));
#57742=CARTESIAN_POINT('Ctrl Pts',(0.445710431435121,0.132535160141284,
0.786966428374124));
#57743=CARTESIAN_POINT('Ctrl Pts',(0.129988929931527,0.446459668345332,
0.806829831739337));
#57744=CARTESIAN_POINT('Ctrl Pts',(-0.304903470342924,0.351080092196355,
0.826693235104551));
#57745=CARTESIAN_POINT('Ctrl Pts',(-0.460267293697333,-0.0661617390664321,
0.846556638469763));
#57746=CARTESIAN_POINT('Ctrl Pts',(-0.193668515362254,-0.422747990558374,
0.866420041834978));
#57747=CARTESIAN_POINT('Ctrl Pts',(0.250481159433732,-0.391768485374328,
0.886283445200189));
#57748=CARTESIAN_POINT('Ctrl Pts',(0.464995395961188,-0.00162453028868252,
0.906146848565404));
#57749=CARTESIAN_POINT('Ctrl Pts',(0.253212414024016,0.390008757270772,
0.926010251930616));
#57750=CARTESIAN_POINT('Ctrl Pts',(-0.190709958360289,0.424090873688623,
0.94587365529583));
#57751=CARTESIAN_POINT('Ctrl Pts',(-0.45979377215103,0.0693761086750143,
0.965737058661043));
#57752=CARTESIAN_POINT('Ctrl Pts',(-0.307349098051745,-0.348941097164749,
0.985600462026257));
#57753=CARTESIAN_POINT('Ctrl Pts',(0.126866248908158,-0.447357029956768,
1.00546386539147));
#57754=CARTESIAN_POINT('Ctrl Pts',(0.444773500139936,-0.135646197650459,
1.02532726875668));
#57755=CARTESIAN_POINT('Ctrl Pts',(0.354922507734706,0.30042198798866,1.0451906721219));
#57756=CARTESIAN_POINT('Ctrl Pts',(-0.0603133790844696,0.461070117950852,
1.06505407548711));
#57757=CARTESIAN_POINT('Ctrl Pts',(-0.420255329741598,0.199019635180803,
1.08491747885232));
#57758=CARTESIAN_POINT('Ctrl Pts',(-0.394916738548566,-0.245487529169761,
1.10478088221754));
#57759=CARTESIAN_POINT('Ctrl Pts',(-0.00752745044395922,-0.464937302067533,
1.12464428558275));
#57760=CARTESIAN_POINT('Ctrl Pts',(0.386762833270873,-0.25814311566201,
1.14450768894796));
#57761=CARTESIAN_POINT('Ctrl Pts',(0.426477735249094,0.18531081646884,1.16437109231318));
#57762=CARTESIAN_POINT('Ctrl Pts',(0.0752075353247572,0.458876000675463,
1.18423449567839));
#57763=CARTESIAN_POINT('Ctrl Pts',(-0.345011224938844,0.311754089030257,
1.2040978990436));
#57764=CARTESIAN_POINT('Ctrl Pts',(-0.448931529762247,-0.121176891149078,
1.22396130240882));
#57765=CARTESIAN_POINT('Ctrl Pts',(-0.141281603819434,-0.44301564960805,
1.24382470577403));
#57766=CARTESIAN_POINT('Ctrl Pts',(0.295892087836421,-0.358707721825574,
1.26368810913924));
#57767=CARTESIAN_POINT('Ctrl Pts',(0.46179863341371,0.0544552985883825,
1.28355151250445));
#57768=CARTESIAN_POINT('Ctrl Pts',(0.204338679793737,0.417694938177113,
1.30341491586967));
#57769=CARTESIAN_POINT('Ctrl Pts',(-0.240454334641303,0.398001344404975,
1.32327831923488));
#57770=CARTESIAN_POINT('Ctrl Pts',(-0.464804276183042,0.0134291577934678,
1.3431417226001));
#57771=CARTESIAN_POINT('Ctrl Pts',(-0.26303221329135,-0.383454576969892,
1.36300512596531));
#57772=CARTESIAN_POINT('Ctrl Pts',(0.179881808535696,-0.428795861789832,
1.38286852933052));
#57773=CARTESIAN_POINT('Ctrl Pts',(0.457884274494346,-0.0810268436371889,
1.40273193269574));
#57774=CARTESIAN_POINT('Ctrl Pts',(0.316108834951241,0.341025753553244,
1.42259533606095));
#57775=CARTESIAN_POINT('Ctrl Pts',(-0.115468002046529,0.450433667702228,
1.44245873942616));
#57776=CARTESIAN_POINT('Ctrl Pts',(-0.441186403406519,0.146894258209524,
1.46232214279137));
#57777=CARTESIAN_POINT('Ctrl Pts',(-0.362435117997404,-0.291314534468849,
1.48218554615659));
#57778=CARTESIAN_POINT('Ctrl Pts',(0.0485884293871068,-0.462452656508136,
1.5020489495218));
#57779=CARTESIAN_POINT('Ctrl Pts',(0.415067252117864,-0.209624918786039,
1.52191235288702));
#57780=CARTESIAN_POINT('Ctrl Pts',(0.401021760561521,0.235382630156459,
1.54177575625222));
#57781=CARTESIAN_POINT('Ctrl Pts',(0.0193287879203514,0.464595873692269,
1.56163915961744));
#57782=CARTESIAN_POINT('Ctrl Pts',(-0.380084687813499,0.267879812339231,
1.58150256298265));
#57783=CARTESIAN_POINT('Ctrl Pts',(-0.431044560988702,-0.174425522064151,
1.60136596634787));
#57784=CARTESIAN_POINT('Ctrl Pts',(-0.0868337066926223,-0.456815470675444,
1.62122936971308));
#57785=CARTESIAN_POINT('Ctrl Pts',(0.336986496472692,-0.320418926739431,
1.64109277307829));
#57786=CARTESIAN_POINT('Ctrl Pts',(0.451860956715713,0.109752564393622,
1.66095617644351));
#57787=CARTESIAN_POINT('Ctrl Pts',(0.152487559617347,0.439262932526176,
1.68081957980872));
#57788=CARTESIAN_POINT('Ctrl Pts',(-0.286698314532727,0.366148428326951,
1.70068298317393));
#57789=CARTESIAN_POINT('Ctrl Pts',(-0.463016271706304,-0.0427987589009261,
1.72054638653915));
#57790=CARTESIAN_POINT('Ctrl Pts',(-0.214907786272786,-0.41220913195275,
1.74040978990436));
#57791=CARTESIAN_POINT('Ctrl Pts',(0.230331103324425,-0.404295995834807,
1.76027319326957));
#57792=CARTESIAN_POINT('Ctrl Pts',(0.464202793554047,-0.0245699036739876,
1.78013659663479));
#57793=CARTESIAN_POINT('Ctrl Pts',(0.336664478059399,0.241817428859645,
1.79337886554493));
#57794=CARTESIAN_POINT('Ctrl Pts',(0.230637453473697,0.318576921724045,
1.8));
#57795=CARTESIAN_POINT('Ctrl Pts',(0.214656790565208,-0.300907133330608,
0.0259624647538709));
#57796=CARTESIAN_POINT('Ctrl Pts',(0.314803053047126,-0.229466237086217,
0.032583599208942));
#57797=CARTESIAN_POINT('Ctrl Pts',(0.43641043615082,0.0200420966425965,
0.0458258681190842));
#57798=CARTESIAN_POINT('Ctrl Pts',(0.219115713204495,0.378437313565148,
0.0656892714842974));
#57799=CARTESIAN_POINT('Ctrl Pts',(-0.199259497560847,0.38879764104502,
0.0855526748495107));
#57800=CARTESIAN_POINT('Ctrl Pts',(-0.434852981374653,0.0432619198281897,
0.105416078214724));
#57801=CARTESIAN_POINT('Ctrl Pts',(-0.271838062851545,-0.342216802259624,
0.125279481579937));
#57802=CARTESIAN_POINT('Ctrl Pts',(0.140420485335661,-0.413812407051313,
0.145142884945151));
#57803=CARTESIAN_POINT('Ctrl Pts',(0.423929765630718,-0.106110600199408,
0.165006288310364));
#57804=CARTESIAN_POINT('Ctrl Pts',(0.318797666989352,0.298910849861812,
0.184869691675577));
#57805=CARTESIAN_POINT('Ctrl Pts',(-0.0786049627665092,0.429876830538249,
0.20473309504079));
#57806=CARTESIAN_POINT('Ctrl Pts',(-0.403942224512066,0.166752341933838,
0.224596498406004));
#57807=CARTESIAN_POINT('Ctrl Pts',(-0.358955536490034,-0.24925256469017,
0.244459901771217));
#57808=CARTESIAN_POINT('Ctrl Pts',(0.0151140129707359,-0.436745429141075,
0.26432330513643));
#57809=CARTESIAN_POINT('Ctrl Pts',(0.37532707714306,-0.223841542925779,
0.284186708501643));
#57810=CARTESIAN_POINT('Ctrl Pts',(0.391448958337841,0.194275989434508,
0.304050111866857));
#57811=CARTESIAN_POINT('Ctrl Pts',(0.0486992427228591,0.434285287852625,
0.323913515232069));
#57812=CARTESIAN_POINT('Ctrl Pts',(-0.33869678981023,0.276151916066506,
0.343776918597283));
#57813=CARTESIAN_POINT('Ctrl Pts',(-0.415583319945026,-0.135151374699497,
0.363640321962496));
#57814=CARTESIAN_POINT('Ctrl Pts',(-0.111472489057659,-0.422550895083751,
0.38350372532771));
#57815=CARTESIAN_POINT('Ctrl Pts',(0.294833782060024,-0.322565382482518,
0.403367128692922));
#57816=CARTESIAN_POINT('Ctrl Pts',(0.430843140951487,0.0731407631575176,
0.423230532058136));
#57817=CARTESIAN_POINT('Ctrl Pts',(0.171865291482725,0.401793109795098,
0.443093935423349));
#57818=CARTESIAN_POINT('Ctrl Pts',(-0.244674753106583,0.362090662938401,
0.462957338788563));
#57819=CARTESIAN_POINT('Ctrl Pts',(-0.436902541328269,-0.00956828252491728,
0.482820742153776));
#57820=CARTESIAN_POINT('Ctrl Pts',(-0.228588001958665,-0.372455242676424,
0.502684145518989));
#57821=CARTESIAN_POINT('Ctrl Pts',(0.189290826001347,-0.393883695832501,
0.522547548884203));
#57822=CARTESIAN_POINT('Ctrl Pts',(0.433632123748318,-0.0542085218513332,
0.542410952249415));
#57823=CARTESIAN_POINT('Ctrl Pts',(0.280429338667971,0.335163793658248,
0.56227435561463));
#57824=CARTESIAN_POINT('Ctrl Pts',(-0.129864695229655,0.417265555166052,
0.582137758979841));
#57825=CARTESIAN_POINT('Ctrl Pts',(-0.421101725918668,0.116827732207138,
0.602001162345057));
#57826=CARTESIAN_POINT('Ctrl Pts',(-0.326282257960183,-0.290715102329896,
0.621864565710268));
#57827=CARTESIAN_POINT('Ctrl Pts',(0.0676653738677941,-0.43173693352053,
0.641727969075482));
#57828=CARTESIAN_POINT('Ctrl Pts',(0.399578927689504,-0.176952149269596,
0.661591372440696));
#57829=CARTESIAN_POINT('Ctrl Pts',(0.365167595478051,0.240058346651971,
0.681454775805909));
#57830=CARTESIAN_POINT('Ctrl Pts',(-0.00402109491296832,0.436988802351671,
0.701318179171121));
#57831=CARTESIAN_POINT('Ctrl Pts',(-0.369523336811412,0.233297848546726,
0.721181582536336));
#57832=CARTESIAN_POINT('Ctrl Pts',(-0.396254975799055,-0.184275274356786,
0.741044985901549));
#57833=CARTESIAN_POINT('Ctrl Pts',(-0.0597090523568472,-0.432909010822709,
0.760908389266761));
#57834=CARTESIAN_POINT('Ctrl Pts',(0.331576774228443,-0.284661598002026,
0.780771792631975));
#57835=CARTESIAN_POINT('Ctrl Pts',(0.418880544671259,0.12455710289149,0.800635195997188));
#57836=CARTESIAN_POINT('Ctrl Pts',(0.12216414499349,0.419584680681779,0.820498599362401));
#57837=CARTESIAN_POINT('Ctrl Pts',(-0.286549568333344,0.329946552448709,
0.840362002727615));
#57838=CARTESIAN_POINT('Ctrl Pts',(-0.432561145265387,-0.0621790816232671,
0.860225406092828));
#57839=CARTESIAN_POINT('Ctrl Pts',(-0.182010488153502,-0.397300345817796,
0.880088809458042));
#57840=CARTESIAN_POINT('Ctrl Pts',(0.235403250840818,-0.368185676090734,
0.899952212823254));
#57841=CARTESIAN_POINT('Ctrl Pts',(0.437004635728844,-0.00152674042195095,
0.919815616188469));
#57842=CARTESIAN_POINT('Ctrl Pts',(0.23797009543256,0.366531876191735,0.93967901955368));
#57843=CARTESIAN_POINT('Ctrl Pts',(-0.179230023795887,0.398562393051505,
0.959542422918895));
#57844=CARTESIAN_POINT('Ctrl Pts',(-0.432116127717582,0.0651999597482869,
0.979405826284106));
#57845=CARTESIAN_POINT('Ctrl Pts',(-0.288847979576343,-0.327936315889959,
0.999269229649322));
#57846=CARTESIAN_POINT('Ctrl Pts',(0.119229436187843,-0.420428024911697,
1.01913263301453));
#57847=CARTESIAN_POINT('Ctrl Pts',(0.418000012685543,-0.127480869073353,
1.03899603637975));
#57848=CARTESIAN_POINT('Ctrl Pts',(0.333557670789321,0.282337852301828,
1.05885943974496));
#57849=CARTESIAN_POINT('Ctrl Pts',(-0.0566827682280645,0.433315642887322,
1.07872284311017));
#57850=CARTESIAN_POINT('Ctrl Pts',(-0.394957732661426,0.187039493144428,
1.09858624647539));
#57851=CARTESIAN_POINT('Ctrl Pts',(-0.371144417711704,-0.23071021604214,
1.1184496498406));
#57852=CARTESIAN_POINT('Ctrl Pts',(-0.00707432969831571,-0.43695003884239,
1.13831305320581));
#57853=CARTESIAN_POINT('Ctrl Pts',(0.36348134311657,-0.242603989642943,
1.15817645657103));
#57854=CARTESIAN_POINT('Ctrl Pts',(0.400805575620254,0.174155887458163,
1.17803985993624));
#57855=CARTESIAN_POINT('Ctrl Pts',(0.0706803591263985,0.431253602211208,
1.19790326330145));
#57856=CARTESIAN_POINT('Ctrl Pts',(-0.324243005385255,0.292987808690079,
1.21776666666667));
#57857=CARTESIAN_POINT('Ctrl Pts',(-0.421907746474372,-0.113882553752806,
1.23763007003188));
#57858=CARTESIAN_POINT('Ctrl Pts',(-0.132777047576297,-0.416347977336323,
1.2574934733971));
#57859=CARTESIAN_POINT('Ctrl Pts',(0.27808063301942,-0.337115030968159,
1.27735687676231));
#57860=CARTESIAN_POINT('Ctrl Pts',(0.434000304794158,0.0511773194526611,
1.29722028012752));
#57861=CARTESIAN_POINT('Ctrl Pts',(0.192038353721738,0.392551465862486,
1.31708368349273));
#57862=CARTESIAN_POINT('Ctrl Pts',(-0.225979998580708,0.374043343314743,
1.33694708685795));
#57863=CARTESIAN_POINT('Ctrl Pts',(-0.436825020554684,0.0126207791747009,
1.35681049022316));
#57864=CARTESIAN_POINT('Ctrl Pts',(-0.247198784230396,-0.360372229881762,
1.37667389358837));
#57865=CARTESIAN_POINT('Ctrl Pts',(0.169053682888399,-0.402984160727349,
1.39653729695359));
#57866=CARTESIAN_POINT('Ctrl Pts',(0.430321573760419,-0.0761493696399576,
1.4164007003188));
#57867=CARTESIAN_POINT('Ctrl Pts',(0.297080417286682,0.320497442555603,
1.43626410368401));
#57868=CARTESIAN_POINT('Ctrl Pts',(-0.108517315678742,0.423319462050434,
1.45612750704923));
#57869=CARTESIAN_POINT('Ctrl Pts',(-0.41462884403543,0.138051843861415,
1.47599091041444));
#57870=CARTESIAN_POINT('Ctrl Pts',(-0.340618053622654,-0.273778629044111,
1.49585431377965));
#57871=CARTESIAN_POINT('Ctrl Pts',(0.0456636110150272,-0.434614958458733,
1.51571771714486));
#57872=CARTESIAN_POINT('Ctrl Pts',(0.390081955413338,-0.197006383438314,
1.53558112051008));
#57873=CARTESIAN_POINT('Ctrl Pts',(0.376881943166925,0.221213589299725,
1.55544452387529));
#57874=CARTESIAN_POINT('Ctrl Pts',(0.0181652764684949,0.436629163014252,
1.57530792724051));
#57875=CARTESIAN_POINT('Ctrl Pts',(-0.357205193829303,0.251754578275839,
1.59517133060572));
#57876=CARTESIAN_POINT('Ctrl Pts',(-0.405097497725524,-0.163925841833111,
1.61503473397093));
#57877=CARTESIAN_POINT('Ctrl Pts',(-0.0816066840484612,-0.429317107420319,
1.63489813733615));
#57878=CARTESIAN_POINT('Ctrl Pts',(0.316701331702821,-0.301131059740813,
1.65476154070136));
#57879=CARTESIAN_POINT('Ctrl Pts',(0.424660834289461,0.103145923249411,
1.67462494406657));
#57880=CARTESIAN_POINT('Ctrl Pts',(0.143308452132116,0.412821157983697,
1.69448834743178));
#57881=CARTESIAN_POINT('Ctrl Pts',(-0.26944028606448,0.344107838343119,
1.714351750797));
#57882=CARTESIAN_POINT('Ctrl Pts',(-0.43514464640082,-0.0402224542556716,
1.73421515416221));
#57883=CARTESIAN_POINT('Ctrl Pts',(-0.20197124459974,-0.387395882018906,
1.75407855752743));
#57884=CARTESIAN_POINT('Ctrl Pts',(0.216466143062017,-0.379959083296314,
1.77394196089264));
#57885=CARTESIAN_POINT('Ctrl Pts',(0.436259744641278,-0.0230908991749218,
1.79380536425785));
#57886=CARTESIAN_POINT('Ctrl Pts',(0.316398697438863,0.227261040280313,
1.80704763316799));
#57887=CARTESIAN_POINT('Ctrl Pts',(0.21675405222531,0.299399935652811,1.81366876762306));
#57888=CARTESIAN_POINT('Ctrl Pts',(0.200907721869555,-0.281633609132834,
0.0396312323769353));
#57889=CARTESIAN_POINT('Ctrl Pts',(0.294639475689289,-0.21476860255658,
0.0462523668320064));
#57890=CARTESIAN_POINT('Ctrl Pts',(0.408457735235377,0.0187583722245711,
0.0594946357421486));
#57891=CARTESIAN_POINT('Ctrl Pts',(0.20508104425592,0.354197872513664,0.0793580391073618));
#57892=CARTESIAN_POINT('Ctrl Pts',(-0.186496647091446,0.363894606478253,
0.0992214424725751));
#57893=CARTESIAN_POINT('Ctrl Pts',(-0.407000037623433,0.0404909331472749,
0.119084845837788));
#57894=CARTESIAN_POINT('Ctrl Pts',(-0.254426453414924,-0.320297335790916,
0.138948249203002));
#57895=CARTESIAN_POINT('Ctrl Pts',(0.131426356176862,-0.387307141614884,
0.158811652568215));
#57896=CARTESIAN_POINT('Ctrl Pts',(0.396776469178078,-0.0993140673357709,
0.178675055933428));
#57897=CARTESIAN_POINT('Ctrl Pts',(0.298378229002275,0.279765190421899,
0.198538459298642));
#57898=CARTESIAN_POINT('Ctrl Pts',(-0.0735702045832253,0.402342616231877,
0.218401862663855));
#57899=CARTESIAN_POINT('Ctrl Pts',(-0.378069158119579,0.156071620404493,
0.238265266029068));
#57900=CARTESIAN_POINT('Ctrl Pts',(-0.335963930601898,-0.233287588108394,
0.258128669394281));
#57901=CARTESIAN_POINT('Ctrl Pts',(0.0141459392282093,-0.408771271454461,
0.277992072759494));
#57902=CARTESIAN_POINT('Ctrl Pts',(0.351286851099471,-0.209504177951092,
0.297855476124708));
#57903=CARTESIAN_POINT('Ctrl Pts',(0.36637610317748,0.1818323396547,0.317718879489921));
#57904=CARTESIAN_POINT('Ctrl Pts',(0.0455799878795328,0.406468705668221,
0.337582282855134));
#57905=CARTESIAN_POINT('Ctrl Pts',(-0.317002785079066,0.258463998277192,
0.357445686220348));
#57906=CARTESIAN_POINT('Ctrl Pts',(-0.388964625052368,-0.126494739471875,
0.377309089585561));
#57907=CARTESIAN_POINT('Ctrl Pts',(-0.104332519687512,-0.395485917224819,
0.397172492950774));
#57908=CARTESIAN_POINT('Ctrl Pts',(0.275949264534774,-0.301904617030305,
0.417035896315987));
#57909=CARTESIAN_POINT('Ctrl Pts',(0.403247033106978,0.0684559946279179,
0.436899299681201));
#57910=CARTESIAN_POINT('Ctrl Pts',(0.160857078359007,0.376057697216407,
0.456762703046413));
#57911=CARTESIAN_POINT('Ctrl Pts',(-0.229002991781463,0.338898247801257,
0.476626106411628));
#57912=CARTESIAN_POINT('Ctrl Pts',(-0.408918320385565,-0.00895542060059796,
0.49648950977684));
#57913=CARTESIAN_POINT('Ctrl Pts',(-0.213946619621507,-0.348598961660897,
0.516352913142054));
#57914=CARTESIAN_POINT('Ctrl Pts',(0.177166482935859,-0.368654892318575,
0.536216316507268));
#57915=CARTESIAN_POINT('Ctrl Pts',(0.405857377641476,-0.0507363899478331,
0.556079719872479));
#57916=CARTESIAN_POINT('Ctrl Pts',(0.262467445957887,0.313696082288999,
0.575943123237694));
#57917=CARTESIAN_POINT('Ctrl Pts',(-0.121546679241664,0.390539110746556,
0.595806526602906));
#57918=CARTESIAN_POINT('Ctrl Pts',(-0.394129569378595,0.109344751997453,
0.61566992996812));
#57919=CARTESIAN_POINT('Ctrl Pts',(-0.305383421417179,-0.27209439202172,
0.635533333333333));
#57920=CARTESIAN_POINT('Ctrl Pts',(0.063331311706633,-0.404083577007581,
0.655396736698547));
#57921=CARTESIAN_POINT('Ctrl Pts',(0.373985336582169,-0.165618115765482,
0.67526014006376));
#57922=CARTESIAN_POINT('Ctrl Pts',(0.341778098493423,0.224682272639162,
0.695123543428973));
#57923=CARTESIAN_POINT('Ctrl Pts',(-0.00376353814039183,0.408999056269356,
0.714986946794187));
#57924=CARTESIAN_POINT('Ctrl Pts',(-0.345854848481321,0.218354793925571,
0.7348503501594));
#57925=CARTESIAN_POINT('Ctrl Pts',(-0.3708742884753,-0.172472184413205,
0.754713753524613));
#57926=CARTESIAN_POINT('Ctrl Pts',(-0.0558846037547525,-0.405180581113605,
0.774577156889825));
#57927=CARTESIAN_POINT('Ctrl Pts',(0.310338816487874,-0.266428623141834,
0.79444056025504));
#57928=CARTESIAN_POINT('Ctrl Pts',(0.392050657907398,0.116579045641696,
0.814303963620252));
#57929=CARTESIAN_POINT('Ctrl Pts',(0.114339360055454,0.392709693018225,
0.834167366985466));
#57930=CARTESIAN_POINT('Ctrl Pts',(-0.268195666323763,0.308813012701063,
0.85403077035068));
#57931=CARTESIAN_POINT('Ctrl Pts',(-0.404854996833441,-0.0581964241801013,
0.873894173715892));
#57932=CARTESIAN_POINT('Ctrl Pts',(-0.17035246094475,-0.371852701077219,
0.893757577081107));
#57933=CARTESIAN_POINT('Ctrl Pts',(0.220325342247905,-0.344602866807139,
0.913620980446318));
#57934=CARTESIAN_POINT('Ctrl Pts',(0.4090138754965,-0.00142895055522028,
0.933484383811533));
#57935=CARTESIAN_POINT('Ctrl Pts',(0.222727776841105,0.343054995112699,
0.953347787176745));
#57936=CARTESIAN_POINT('Ctrl Pts',(-0.167750089231486,0.373033912414387,
0.973211190541959));
#57937=CARTESIAN_POINT('Ctrl Pts',(-0.404438483284133,0.0610238108215602,
0.993074593907172));
#57938=CARTESIAN_POINT('Ctrl Pts',(-0.270346861100941,-0.306931534615169,
1.01293799727239));
#57939=CARTESIAN_POINT('Ctrl Pts',(0.111592623467528,-0.393499019866625,
1.0328014006376));
#57940=CARTESIAN_POINT('Ctrl Pts',(0.39122652523115,-0.119315540496249,
1.05266480400281));
#57941=CARTESIAN_POINT('Ctrl Pts',(0.312192833843937,0.264253716614997,
1.07252820736802));
#57942=CARTESIAN_POINT('Ctrl Pts',(-0.0530521573716599,0.405561167823791,
1.09239161073324));
#57943=CARTESIAN_POINT('Ctrl Pts',(-0.369660135581253,0.175059351108053,
1.11225501409845));
#57944=CARTESIAN_POINT('Ctrl Pts',(-0.347372096874843,-0.215932902914519,
1.13211841746366));
#57945=CARTESIAN_POINT('Ctrl Pts',(-0.00662120895267193,-0.408962775617247,
1.15198182082888));
#57946=CARTESIAN_POINT('Ctrl Pts',(0.340199852962266,-0.227064863623877,
1.17184522419409));
#57947=CARTESIAN_POINT('Ctrl Pts',(0.375133415991415,0.163000958447487,
1.1917086275593));
#57948=CARTESIAN_POINT('Ctrl Pts',(0.0661531829280398,0.403631203746953,
1.21157203092452));
#57949=CARTESIAN_POINT('Ctrl Pts',(-0.303474785831665,0.274221528349901,
1.23143543428973));
#57950=CARTESIAN_POINT('Ctrl Pts',(-0.394883963186496,-0.106588216356535,
1.25129883765494));
#57951=CARTESIAN_POINT('Ctrl Pts',(-0.124272491333159,-0.389680305064596,
1.27116224102016));
#57952=CARTESIAN_POINT('Ctrl Pts',(0.260269178202419,-0.315522340110745,
1.29102564438537));
#57953=CARTESIAN_POINT('Ctrl Pts',(0.406201976174607,0.0478993403169399,
1.31088904775058));
#57954=CARTESIAN_POINT('Ctrl Pts',(0.179738027649738,0.367407993547859,
1.3307524511158));
#57955=CARTESIAN_POINT('Ctrl Pts',(-0.211505662520113,0.350085342224511,
1.35061585448101));
#57956=CARTESIAN_POINT('Ctrl Pts',(-0.408845764926325,0.0118124005559338,
1.37047925784622));
#57957=CARTESIAN_POINT('Ctrl Pts',(-0.231365355169441,-0.337289882793632,
1.39034266121144));
#57958=CARTESIAN_POINT('Ctrl Pts',(0.158225557241102,-0.377172459664866,
1.41020606457665));
#57959=CARTESIAN_POINT('Ctrl Pts',(0.402758873026492,-0.0712718956427259,
1.43006946794187));
#57960=CARTESIAN_POINT('Ctrl Pts',(0.278051999622122,0.299969131557961,
1.44993287130708));
#57961=CARTESIAN_POINT('Ctrl Pts',(-0.101566629310955,0.39620525639864,
1.46979627467229));
#57962=CARTESIAN_POINT('Ctrl Pts',(-0.388071284664342,0.129209429513306,
1.4896596780375));
#57963=CARTESIAN_POINT('Ctrl Pts',(-0.318800989247905,-0.256242723619373,
1.50952308140272));
#57964=CARTESIAN_POINT('Ctrl Pts',(0.0427387926429474,-0.40677726040933,
1.52938648476793));
#57965=CARTESIAN_POINT('Ctrl Pts',(0.365096658708812,-0.184387848090589,
1.54924988813315));
#57966=CARTESIAN_POINT('Ctrl Pts',(0.35274212577233,0.207044548442991,1.56911329149835));
#57967=CARTESIAN_POINT('Ctrl Pts',(0.0170017650166384,0.408662452336233,
1.58897669486357));
#57968=CARTESIAN_POINT('Ctrl Pts',(-0.334325699845108,0.235629344212447,
1.60884009822878));
#57969=CARTESIAN_POINT('Ctrl Pts',(-0.379150434462346,-0.153426161602072,
1.628703501594));
#57970=CARTESIAN_POINT('Ctrl Pts',(-0.0763796614043001,-0.401818744165193,
1.64856690495921));
#57971=CARTESIAN_POINT('Ctrl Pts',(0.29641616693295,-0.281843192742194,
1.66843030832442));
#57972=CARTESIAN_POINT('Ctrl Pts',(0.397460711863209,0.0965392821051996,
1.68829371168964));
#57973=CARTESIAN_POINT('Ctrl Pts',(0.134129344646885,0.386379383441219,
1.70815711505485));
#57974=CARTESIAN_POINT('Ctrl Pts',(-0.252182257596233,0.322067248359287,
1.72802051842006));
#57975=CARTESIAN_POINT('Ctrl Pts',(-0.407273021095337,-0.0376461496104168,
1.74788392178527));
#57976=CARTESIAN_POINT('Ctrl Pts',(-0.189034702926694,-0.362582632085062,
1.76774732515049));
#57977=CARTESIAN_POINT('Ctrl Pts',(0.202601182799609,-0.35562217075782,
1.7876107285157));
#57978=CARTESIAN_POINT('Ctrl Pts',(0.408316695728509,-0.0216118946758564,
1.80747413188092));
#57979=CARTESIAN_POINT('Ctrl Pts',(0.296132916818328,0.21270465170098,1.82071640079106));
#57980=CARTESIAN_POINT('Ctrl Pts',(0.202870650976924,0.280222949581577,
1.82733753524613));
#57981=CARTESIAN_POINT('Ctrl Pts',(0.187158653173902,-0.262360084935059,
0.0532999999999997));
#57982=CARTESIAN_POINT('Ctrl Pts',(0.274475898331453,-0.200070968026944,
0.0599211344550708));
#57983=CARTESIAN_POINT('Ctrl Pts',(0.380505034319934,0.0174746478065457,
0.0731634033652129));
#57984=CARTESIAN_POINT('Ctrl Pts',(0.191046375307344,0.329958431462181,
0.0930268067304262));
#57985=CARTESIAN_POINT('Ctrl Pts',(-0.173733796622045,0.338991571911486,
0.11289021009564));
#57986=CARTESIAN_POINT('Ctrl Pts',(-0.379147093872213,0.0377199464663596,
0.132753613460853));
#57987=CARTESIAN_POINT('Ctrl Pts',(-0.237014843978304,-0.298377869322208,
0.152617016826066));
#57988=CARTESIAN_POINT('Ctrl Pts',(0.122432227018064,-0.360801876178455,
0.172480420191279));
#57989=CARTESIAN_POINT('Ctrl Pts',(0.369623172725438,-0.0925175344721341,
0.192343823556493));
#57990=CARTESIAN_POINT('Ctrl Pts',(0.277958791015197,0.260619530981986,
0.212207226921706));
#57991=CARTESIAN_POINT('Ctrl Pts',(-0.0685354463999416,0.374808401925503,
0.232070630286919));
#57992=CARTESIAN_POINT('Ctrl Pts',(-0.352196091727093,0.145390898875147,
0.251934033652132));
#57993=CARTESIAN_POINT('Ctrl Pts',(-0.312972324713763,-0.217322611526617,
0.271797437017346));
#57994=CARTESIAN_POINT('Ctrl Pts',(0.0131778654856828,-0.380797113767846,
0.291660840382558));
#57995=CARTESIAN_POINT('Ctrl Pts',(0.327246625055882,-0.195166812976406,
0.311524243747772));
#57996=CARTESIAN_POINT('Ctrl Pts',(0.341303248017118,0.169388689874893,
0.331387647112985));
#57997=CARTESIAN_POINT('Ctrl Pts',(0.0424607330362066,0.378652123483815,
0.351251050478199));
#57998=CARTESIAN_POINT('Ctrl Pts',(-0.295308780347901,0.240776080487878,
0.371114453843412));
#57999=CARTESIAN_POINT('Ctrl Pts',(-0.362345930159709,-0.117838104244253,
0.390977857208625));
#58000=CARTESIAN_POINT('Ctrl Pts',(-0.0971925503173641,-0.368420939365887,
0.410841260573839));
#58001=CARTESIAN_POINT('Ctrl Pts',(0.257064747009525,-0.281243851578092,
0.430704663939052));
#58002=CARTESIAN_POINT('Ctrl Pts',(0.375650925262469,0.063771226098318,
0.450568067304265));
#58003=CARTESIAN_POINT('Ctrl Pts',(0.149848865235289,0.350322284637716,
0.470431470669478));
#58004=CARTESIAN_POINT('Ctrl Pts',(-0.213331230456342,0.315705832664112,
0.490294874034692));
#58005=CARTESIAN_POINT('Ctrl Pts',(-0.380934099442862,-0.00834255867627857,
0.510158277399905));
#58006=CARTESIAN_POINT('Ctrl Pts',(-0.199305237284349,-0.324742680645371,
0.530021680765118));
#58007=CARTESIAN_POINT('Ctrl Pts',(0.16504213987037,-0.34342608880465,0.549885084130331));
#58008=CARTESIAN_POINT('Ctrl Pts',(0.378082631534635,-0.0472642580443332,
0.569748487495545));
#58009=CARTESIAN_POINT('Ctrl Pts',(0.244505553247802,0.29222837091975,0.589611890860758));
#58010=CARTESIAN_POINT('Ctrl Pts',(-0.113228663253673,0.363812666327059,
0.609475294225971));
#58011=CARTESIAN_POINT('Ctrl Pts',(-0.367157412838523,0.101861771787768,
0.629338697591184));
#58012=CARTESIAN_POINT('Ctrl Pts',(-0.284484584874175,-0.253473681713543,
0.649202100956398));
#58013=CARTESIAN_POINT('Ctrl Pts',(0.0589972495454716,-0.376430220494633,
0.66906550432161));
#58014=CARTESIAN_POINT('Ctrl Pts',(0.348391745474835,-0.154284082261366,
0.688928907686824));
#58015=CARTESIAN_POINT('Ctrl Pts',(0.318388601508794,0.209306198626352,
0.708792311052038));
#58016=CARTESIAN_POINT('Ctrl Pts',(-0.00350598136781482,0.381009310187041,
0.72865571441725));
#58017=CARTESIAN_POINT('Ctrl Pts',(-0.322186360151231,0.203411739304416,
0.748519117782465));
#58018=CARTESIAN_POINT('Ctrl Pts',(-0.345493601151545,-0.160669094469624,
0.768382521147676));
#58019=CARTESIAN_POINT('Ctrl Pts',(-0.0520601551526582,-0.377452151404502,
0.788245924512891));
#58020=CARTESIAN_POINT('Ctrl Pts',(0.289100858747305,-0.248195648281641,
0.808109327878104));
#58021=CARTESIAN_POINT('Ctrl Pts',(0.365220771143536,0.108600988391901,
0.827972731243317));
#58022=CARTESIAN_POINT('Ctrl Pts',(0.106514575117418,0.365834705354672,
0.84783613460853));
#58023=CARTESIAN_POINT('Ctrl Pts',(-0.249841764314182,0.287679472953417,
0.867699537973743));
#58024=CARTESIAN_POINT('Ctrl Pts',(-0.377148848401494,-0.0542137667369359,
0.887562941338957));
#58025=CARTESIAN_POINT('Ctrl Pts',(-0.158694433735999,-0.346405056336641,
0.90742634470417));
#58026=CARTESIAN_POINT('Ctrl Pts',(0.205247433654992,-0.321020057523545,
0.927289748069383));
#58027=CARTESIAN_POINT('Ctrl Pts',(0.381023115264154,-0.00133116068848917,
0.947153151434597));
#58028=CARTESIAN_POINT('Ctrl Pts',(0.207485458249651,0.319578114033663,
0.96701655479981));
#58029=CARTESIAN_POINT('Ctrl Pts',(-0.156270154667085,0.347505431777269,
0.986879958165023));
#58030=CARTESIAN_POINT('Ctrl Pts',(-0.376760838850683,0.0568476618948332,
1.00674336153024));
#58031=CARTESIAN_POINT('Ctrl Pts',(-0.251845742625539,-0.28592675334038,
1.02660676489545));
#58032=CARTESIAN_POINT('Ctrl Pts',(0.103955810747213,-0.366570014821552,
1.04647016826066));
#58033=CARTESIAN_POINT('Ctrl Pts',(0.364453037776757,-0.111150211919144,
1.06633357162588));
#58034=CARTESIAN_POINT('Ctrl Pts',(0.290827996898553,0.246169580928165,
1.08619697499109));
#58035=CARTESIAN_POINT('Ctrl Pts',(-0.0494215465152554,0.377806692760261,
1.1060603783563));
#58036=CARTESIAN_POINT('Ctrl Pts',(-0.34436253850108,0.163079209071679,
1.12592378172152));
#58037=CARTESIAN_POINT('Ctrl Pts',(-0.323599776037981,-0.201155589786898,
1.14578718508673));
#58038=CARTESIAN_POINT('Ctrl Pts',(-0.00616808820702852,-0.380975512392104,
1.16565058845194));
#58039=CARTESIAN_POINT('Ctrl Pts',(0.316918362807963,-0.211525737604811,
1.18551399181716));
#58040=CARTESIAN_POINT('Ctrl Pts',(0.349461256362576,0.151846029436811,
1.20537739518237));
#58041=CARTESIAN_POINT('Ctrl Pts',(0.0616260067296811,0.376008805282698,
1.22524079854758));
#58042=CARTESIAN_POINT('Ctrl Pts',(-0.282706566278076,0.255455248009724,
1.2451042019128));
#58043=CARTESIAN_POINT('Ctrl Pts',(-0.367860179898621,-0.0992938789602632,
1.26496760527801));
#58044=CARTESIAN_POINT('Ctrl Pts',(-0.115767935090022,-0.363012632792868,
1.28483100864322));
#58045=CARTESIAN_POINT('Ctrl Pts',(0.242457723385417,-0.293929649253331,
1.30469441200844));
#58046=CARTESIAN_POINT('Ctrl Pts',(0.378403647555055,0.0446213611812189,
1.32455781537365));
#58047=CARTESIAN_POINT('Ctrl Pts',(0.167437701577738,0.342264521233232,
1.34442121873886));
#58048=CARTESIAN_POINT('Ctrl Pts',(-0.197031326459517,0.326127341134279,
1.36428462210407));
#58049=CARTESIAN_POINT('Ctrl Pts',(-0.380866509297967,0.0110040219371662,
1.38414802546929));
#58050=CARTESIAN_POINT('Ctrl Pts',(-0.215531926108487,-0.314207535705501,
1.4040114288345));
#58051=CARTESIAN_POINT('Ctrl Pts',(0.147397431593805,-0.351360758602383,
1.42387483219971));
#58052=CARTESIAN_POINT('Ctrl Pts',(0.375196172292565,-0.0663944216454938,
1.44373823556493));
#58053=CARTESIAN_POINT('Ctrl Pts',(0.259023581957562,0.279440820560319,
1.46360163893014));
#58054=CARTESIAN_POINT('Ctrl Pts',(-0.0946159429431672,0.369091050746847,
1.48346504229536));
#58055=CARTESIAN_POINT('Ctrl Pts',(-0.361513725293254,0.120367015165197,
1.50332844566056));
#58056=CARTESIAN_POINT('Ctrl Pts',(-0.296983924873155,-0.238706818194636,
1.52319184902578));
#58057=CARTESIAN_POINT('Ctrl Pts',(0.039813974270868,-0.378939562359927,
1.54305525239099));
#58058=CARTESIAN_POINT('Ctrl Pts',(0.340111362004286,-0.171769312742865,
1.56291865575621));
#58059=CARTESIAN_POINT('Ctrl Pts',(0.328602308377735,0.192875507586258,
1.58278205912142));
#58060=CARTESIAN_POINT('Ctrl Pts',(0.0158382535647818,0.380695741658215,
1.60264546248663));
#58061=CARTESIAN_POINT('Ctrl Pts',(-0.311446205860912,0.219504110149056,
1.62250886585185));
#58062=CARTESIAN_POINT('Ctrl Pts',(-0.353203371199169,-0.142926481371032,
1.64237226921706));
#58063=CARTESIAN_POINT('Ctrl Pts',(-0.0711526387601384,-0.374320380910067,
1.66223567258227));
#58064=CARTESIAN_POINT('Ctrl Pts',(0.276131002163078,-0.262555325743576,
1.68209907594749));
#58065=CARTESIAN_POINT('Ctrl Pts',(0.370260589436959,0.089932640960989,
1.7019624793127));
#58066=CARTESIAN_POINT('Ctrl Pts',(0.124950237161653,0.359937608898739,
1.72182588267791));
#58067=CARTESIAN_POINT('Ctrl Pts',(-0.234924229127985,0.300026658375456,
1.74168928604313));
#58068=CARTESIAN_POINT('Ctrl Pts',(-0.379401395789853,-0.0350698449651625,
1.76155268940834));
#58069=CARTESIAN_POINT('Ctrl Pts',(-0.176098161253648,-0.337769382151217,
1.78141609277355));
#58070=CARTESIAN_POINT('Ctrl Pts',(0.188736222537201,-0.331285258219327,
1.80127949613877));
#58071=CARTESIAN_POINT('Ctrl Pts',(0.38037364681574,-0.0201328901767907,
1.82114289950398));
#58072=CARTESIAN_POINT('Ctrl Pts',(0.275867136197792,0.198148263121647,
1.83438516841412));
#58073=CARTESIAN_POINT('Ctrl Pts',(0.188987249728538,0.261045963510343,
1.84100630286919));
#58074=CARTESIAN_POINT('',(0.230637453473697,0.318576921724045,1.8));
#58075=CARTESIAN_POINT('Ctrl Pts',(0.141603157807409,-0.290105179958815,
1.8));
#58076=CARTESIAN_POINT('Ctrl Pts',(0.148157166114403,-0.287770754305551,
1.8));
#58077=CARTESIAN_POINT('Ctrl Pts',(0.154616475711889,-0.285214128338566,
1.8));
#58078=CARTESIAN_POINT('Ctrl Pts',(0.160969423134311,-0.282436150032975,
1.8));
#58079=CARTESIAN_POINT('Ctrl Pts',(0.177873482965308,-0.275044445306887,
1.8));
#58080=CARTESIAN_POINT('Ctrl Pts',(0.194025306149541,-0.266089662887484,
1.8));
#58081=CARTESIAN_POINT('Ctrl Pts',(0.209336262334518,-0.255787677754136,
1.8));
#58082=CARTESIAN_POINT('Ctrl Pts',(0.219828851204133,-0.248727733669706,
1.8));
#58083=CARTESIAN_POINT('Ctrl Pts',(0.229926482288665,-0.241033833322765,
1.8));
#58084=CARTESIAN_POINT('Ctrl Pts',(0.239596477203674,-0.232762290241159,
1.8));
#58085=CARTESIAN_POINT('Ctrl Pts',(0.243434784886035,-0.229479069553439,
1.8));
#58086=CARTESIAN_POINT('Ctrl Pts',(0.247207605954188,-0.226102903767889,
1.8));
#58087=CARTESIAN_POINT('Ctrl Pts',(0.250906256816858,-0.222642971761847,
1.8));
#58088=CARTESIAN_POINT('Ctrl Pts',(0.265338639470732,-0.209142086027652,
1.8));
#58089=CARTESIAN_POINT('Ctrl Pts',(0.278586410411045,-0.194425703806486,
1.8));
#58090=CARTESIAN_POINT('Ctrl Pts',(0.290546071531598,-0.178726454802016,
1.8));
#58091=CARTESIAN_POINT('Ctrl Pts',(0.299413028045636,-0.167086947894376,
1.8));
#58092=CARTESIAN_POINT('Ctrl Pts',(0.307571782002005,-0.154905816290907,
1.8));
#58093=CARTESIAN_POINT('Ctrl Pts',(0.314970614874736,-0.142261835016312,
1.8));
#58094=CARTESIAN_POINT('Ctrl Pts',(0.319430822453677,-0.134639716490457,
1.8));
#58095=CARTESIAN_POINT('Ctrl Pts',(0.323614695300392,-0.126849161122988,
1.8));
#58096=CARTESIAN_POINT('Ctrl Pts',(0.327508820353545,-0.118905724928063,
1.8));
#58097=CARTESIAN_POINT('Ctrl Pts',(0.329797917149386,-0.114236307769246,
1.8));
#58098=CARTESIAN_POINT('Ctrl Pts',(0.331983045551948,-0.109521668097398,
1.8));
#58099=CARTESIAN_POINT('Ctrl Pts',(0.334060558900541,-0.104769521658052,
1.8));
#58100=CARTESIAN_POINT('Ctrl Pts',(0.342241183697153,-0.0860569935170526,
1.8));
#58101=CARTESIAN_POINT('Ctrl Pts',(0.348765534562484,-0.066746552171421,
1.8));
#58102=CARTESIAN_POINT('Ctrl Pts',(0.353504988432865,-0.0470500087636206,
1.8));
#58103=CARTESIAN_POINT('Ctrl Pts',(0.355704075360087,-0.037910894362647,
1.8));
#58104=CARTESIAN_POINT('Ctrl Pts',(0.357518357519014,-0.0286881552166209,
1.8));
#58105=CARTESIAN_POINT('Ctrl Pts',(0.358931711772656,-0.0194009408651651,
1.8));
#58106=CARTESIAN_POINT('Ctrl Pts',(0.360583937406819,-0.00854409193157186,
1.8));
#58107=CARTESIAN_POINT('Ctrl Pts',(0.361688388824116,0.00240089241339821,
1.8));
#58108=CARTESIAN_POINT('Ctrl Pts',(0.362260654583105,0.0134037927651624,
1.8));
#58109=CARTESIAN_POINT('Ctrl Pts',(0.36252518757313,0.0184899438816373,
1.8));
#58110=CARTESIAN_POINT('Ctrl Pts',(0.362675431445883,0.0235795032329619,
1.8));
#58111=CARTESIAN_POINT('Ctrl Pts',(0.362713867593775,0.0286667428322311,
1.8));
#58112=CARTESIAN_POINT('Ctrl Pts',(0.362867054460235,0.0489418831852718,
1.8));
#58113=CARTESIAN_POINT('Ctrl Pts',(0.361248999287613,0.0691916862605563,
1.8));
#58114=CARTESIAN_POINT('Ctrl Pts',(0.357992028648484,0.0892225189703539,
1.8));
#58115=CARTESIAN_POINT('Ctrl Pts',(0.35587100389236,0.102267122920059,1.8));
#58116=CARTESIAN_POINT('Ctrl Pts',(0.353053837305762,0.115219322766376,
1.8));
#58117=CARTESIAN_POINT('Ctrl Pts',(0.349565738552542,0.128027375249902,
1.8));
#58118=CARTESIAN_POINT('Ctrl Pts',(0.34755041814521,0.135427489574188,1.8));
#58119=CARTESIAN_POINT('Ctrl Pts',(0.345310966761358,0.142779491872179,
1.8));
#58120=CARTESIAN_POINT('Ctrl Pts',(0.342850970118154,0.150073252099977,
1.8));
#58121=CARTESIAN_POINT('Ctrl Pts',(0.341081076039099,0.155320894643267,
1.8));
#58122=CARTESIAN_POINT('Ctrl Pts',(0.339197374240118,0.160536742001126,
1.8));
#58123=CARTESIAN_POINT('Ctrl Pts',(0.337205955025213,0.165705865160006,
1.8));
#58124=CARTESIAN_POINT('Ctrl Pts',(0.331562736590182,0.180353956774669,
1.8));
#58125=CARTESIAN_POINT('Ctrl Pts',(0.325047469011081,0.194651789699771,
1.8));
#58126=CARTESIAN_POINT('Ctrl Pts',(0.317704114220749,0.208516108946925,
1.8));
#58127=CARTESIAN_POINT('Ctrl Pts',(0.313549190673617,0.216360641609406,
1.8));
#58128=CARTESIAN_POINT('Ctrl Pts',(0.309128890575192,0.224066387719809,
1.8));
#58129=CARTESIAN_POINT('Ctrl Pts',(0.304449133391761,0.231617862092355,
1.8));
#58130=CARTESIAN_POINT('Ctrl Pts',(0.299771419854562,0.239166038742062,
1.8));
#58131=CARTESIAN_POINT('Ctrl Pts',(0.294831254196119,0.246563958455385,
1.8));
#58132=CARTESIAN_POINT('Ctrl Pts',(0.289651947072993,0.253771225125073,
1.8));
#58133=CARTESIAN_POINT('Ctrl Pts',(0.276941700269071,0.271458173586651,
1.8));
#58134=CARTESIAN_POINT('Ctrl Pts',(0.262780082335297,0.288025513613553,
1.8));
#58135=CARTESIAN_POINT('Ctrl Pts',(0.24725665255325,0.303250481813621,1.8));
#58136=CARTESIAN_POINT('Ctrl Pts',(0.24187988232453,0.308523875445098,1.8));
#58137=CARTESIAN_POINT('Ctrl Pts',(0.236339326786495,0.313636036829337,
1.8));
#58138=CARTESIAN_POINT('Ctrl Pts',(0.230637453473697,0.318576921724045,
1.8));
#58139=CARTESIAN_POINT('Ctrl Pts',(0.230637453473696,0.318576921724045,
1.8));
#58140=CARTESIAN_POINT('Ctrl Pts',(0.336664478059399,0.241817428859645,
1.79337886554493));
#58141=CARTESIAN_POINT('Ctrl Pts',(0.400433635806723,0.108623762592829,
1.78675773108986));
#58142=CARTESIAN_POINT('Ctrl Pts',(0.393339599642115,-0.0212607525673823,
1.78013659663479));
#58143=CARTESIAN_POINT('Ctrl Pts',(0.386245563477507,-0.151145267727593,
1.77351546217972));
#58144=CARTESIAN_POINT('Ctrl Pts',(0.308288333400966,-0.277720631781199,
1.76689432772464));
#58145=CARTESIAN_POINT('Ctrl Pts',(0.195103236763162,-0.34232716982766,
1.76027319326957));
#58146=CARTESIAN_POINT('Ctrl Pts',(0.0819181401253553,-0.406933707874121,
1.7536520588145));
#58147=CARTESIAN_POINT('Ctrl Pts',(-0.0664948230737163,-0.409571419913436,
1.74703092435943));
#58148=CARTESIAN_POINT('Ctrl Pts',(-0.182052718912172,-0.349321880424455,
1.74040978990436));
#58149=CARTESIAN_POINT('Ctrl Pts',(-0.297610614750626,-0.289072340935474,
1.73378865544929));
#58150=CARTESIAN_POINT('Ctrl Pts',(-0.380313443228465,-0.1659355499182,
1.72716752099422));
#58151=CARTESIAN_POINT('Ctrl Pts',(-0.392278531271789,-0.0362092898715836,
1.72054638653915));
#58152=CARTESIAN_POINT('Ctrl Pts',(-0.393380886268349,-0.0242574855530751,
1.71993637509393));
#58153=CARTESIAN_POINT('Ctrl Pts',(-0.393882811330762,-0.0122497490768379,
1.71932636364871));
#58154=CARTESIAN_POINT('Ctrl Pts',(-0.393805363403874,-0.000235004724456311,
1.7187163522035));
#58155=CARTESIAN_POINT('Origin',(0.275,0.,1.8));
#58156=CARTESIAN_POINT('Origin',(0.,0.,1.8));
#58157=CARTESIAN_POINT('',(-0.275,-3.36777869765522E-17,1.8));
#58158=CARTESIAN_POINT('Origin',(0.,0.,1.8));
#58159=CARTESIAN_POINT('Origin',(-0.115470053837925,-0.2,0.));
#58160=CARTESIAN_POINT('',(-0.115470053837925,-0.2,0.));
#58161=CARTESIAN_POINT('',(0.115470053837925,-0.2,0.));
#58162=CARTESIAN_POINT('',(0.112264973081037,-0.2,0.));
#58163=CARTESIAN_POINT('',(-0.115470053837925,-0.2,0.36));
#58164=CARTESIAN_POINT('',(-0.115470053837925,-0.2,0.));
#58165=CARTESIAN_POINT('',(0.115470053837925,-0.2,0.36));
#58166=CARTESIAN_POINT('',(-0.115470053837925,-0.2,0.36));
#58167=CARTESIAN_POINT('',(0.115470053837925,-0.2,0.));
#58168=CARTESIAN_POINT('Origin',(-0.23094010767585,2.82820063659975E-17,
0.));
#58169=CARTESIAN_POINT('',(-0.23094010767585,2.82820063659975E-17,0.));
#58170=CARTESIAN_POINT('',(-0.159572594216369,-0.123612159321677,0.));
#58171=CARTESIAN_POINT('',(-0.23094010767585,2.77555756156289E-17,0.36));
#58172=CARTESIAN_POINT('',(-0.23094010767585,2.82820063659975E-17,0.));
#58173=CARTESIAN_POINT('',(-0.23094010767585,2.82820063659975E-17,0.36));
#58174=CARTESIAN_POINT('Origin',(-0.115470053837925,0.2,0.));
#58175=CARTESIAN_POINT('',(-0.115470053837925,0.2,0.));
#58176=CARTESIAN_POINT('',(-0.101837567297406,0.223612159321677,0.));
#58177=CARTESIAN_POINT('',(-0.115470053837925,0.2,0.36));
#58178=CARTESIAN_POINT('',(-0.115470053837925,0.2,0.));
#58179=CARTESIAN_POINT('',(-0.115470053837925,0.2,0.36));
#58180=CARTESIAN_POINT('Origin',(0.115470053837925,0.2,0.));
#58181=CARTESIAN_POINT('',(0.115470053837925,0.2,0.));
#58182=CARTESIAN_POINT('',(0.227735026918963,0.2,0.));
#58183=CARTESIAN_POINT('',(0.115470053837925,0.2,0.36));
#58184=CARTESIAN_POINT('',(0.115470053837925,0.2,0.));
#58185=CARTESIAN_POINT('',(0.115470053837925,0.2,0.36));
#58186=CARTESIAN_POINT('Origin',(0.23094010767585,0.,0.));
#58187=CARTESIAN_POINT('',(0.23094010767585,0.,0.));
#58188=CARTESIAN_POINT('',(0.244572594216369,-0.0236121593216773,0.));
#58189=CARTESIAN_POINT('',(0.23094010767585,0.,0.36));
#58190=CARTESIAN_POINT('',(0.23094010767585,0.,0.));
#58191=CARTESIAN_POINT('',(0.23094010767585,0.,0.36));
#58192=CARTESIAN_POINT('Origin',(0.115470053837925,-0.2,0.));
#58193=CARTESIAN_POINT('',(0.186837567297406,-0.0763878406783227,0.));
#58194=CARTESIAN_POINT('',(0.115470053837925,-0.2,0.36));
#58195=CARTESIAN_POINT('Origin',(0.,0.,0.36));
#58196=CARTESIAN_POINT('Origin',(0.34,0.,0.));
#58197=CARTESIAN_POINT('',(-0.34,-4.163799117101E-17,1.73472347597681E-17));
#58198=CARTESIAN_POINT('Origin',(0.,0.,0.));
#58199=CARTESIAN_POINT('Origin',(0.,0.,0.03));
#58200=CARTESIAN_POINT('',(-0.37,-4.53119315684521E-17,0.03));
#58201=CARTESIAN_POINT('Origin',(0.,0.,0.93));
#58202=CARTESIAN_POINT('Origin',(0.,0.,1.885));
#58203=CARTESIAN_POINT('',(-0.275,-3.36777869765522E-17,1.97));
#58204=CARTESIAN_POINT('Origin',(0.,0.,1.97));
#58205=CARTESIAN_POINT('',(-0.275,-3.36777869765522E-17,1.885));
#58206=CARTESIAN_POINT('Origin',(0.,0.,1.985));
#58207=CARTESIAN_POINT('',(-0.245,-3.00038465791101E-17,2.));
#58208=CARTESIAN_POINT('Origin',(0.,0.,2.));
#58209=CARTESIAN_POINT('',(-0.26,-3.18408167778312E-17,1.985));
#58210=CARTESIAN_POINT('Origin',(0.,0.,2.));
#58211=CARTESIAN_POINT('',(0.,0.,0.));
#58212=CARTESIAN_POINT('Origin',(19.0265,9.976,3.6));
#58213=CARTESIAN_POINT('',(19.0265,9.976,4.764));
#58214=CARTESIAN_POINT('',(19.0505,10.,4.74));
#58215=CARTESIAN_POINT('',(19.4655416666666,10.4150416666667,4.32495833333334));
#58216=CARTESIAN_POINT('',(19.0505,10.,3.65));
#58217=CARTESIAN_POINT('',(19.0505,10.,3.6));
#58218=CARTESIAN_POINT('',(19.0265,9.976,3.626));
#58219=CARTESIAN_POINT('',(19.2672083333333,10.2167083333333,3.86670833333333));
#58220=CARTESIAN_POINT('',(19.0025,9.952,3.65));
#58221=CARTESIAN_POINT('',(18.2018333333333,9.15133333333324,4.45066666666668));
#58222=CARTESIAN_POINT('',(19.0025,9.952,4.74));
#58223=CARTESIAN_POINT('',(19.0025,9.952,3.6));
#58224=CARTESIAN_POINT('',(18.0035,8.95299999999991,3.741));
#58225=CARTESIAN_POINT('Origin',(20.9975,10.,3.6));
#58226=CARTESIAN_POINT('',(20.9495,10.,4.74));
#58227=CARTESIAN_POINT('',(20.49875,10.,4.74));
#58228=CARTESIAN_POINT('',(20.9495,10.,3.65));
#58229=CARTESIAN_POINT('',(20.9495,10.,3.6));
#58230=CARTESIAN_POINT('',(20.49875,10.,3.65));
#58231=CARTESIAN_POINT('Origin',(20.49875,9.975,4.765));
#58232=CARTESIAN_POINT('',(19.0525,9.95,4.79));
#58233=CARTESIAN_POINT('',(19.0525,9.95,4.79));
#58234=CARTESIAN_POINT('',(20.9475,9.95,4.79));
#58235=CARTESIAN_POINT('',(20.49875,9.95,4.79));
#58236=CARTESIAN_POINT('',(20.9735,9.976,4.764));
#58237=CARTESIAN_POINT('',(20.9475,9.95,4.79));
#58238=CARTESIAN_POINT('',(20.7007083333333,10.2487916666667,4.49120833333333));
#58239=CARTESIAN_POINT('Origin',(19.0275,5.,4.765));
#58240=CARTESIAN_POINT('',(19.0025,-9.952,4.74));
#58241=CARTESIAN_POINT('',(19.0025,5.,4.74));
#58242=CARTESIAN_POINT('',(19.0265,-9.976,4.764));
#58243=CARTESIAN_POINT('',(16.3368333333333,-7.28633333333305,2.0743333333333));
#58244=CARTESIAN_POINT('',(19.0525,-9.95,4.79));
#58245=CARTESIAN_POINT('',(19.0525,-9.95,4.79));
#58246=CARTESIAN_POINT('',(19.0525,5.,4.79));
#58247=CARTESIAN_POINT('Origin',(20.9735,9.976,3.6));
#58248=CARTESIAN_POINT('',(20.9975,9.952,4.74));
#58249=CARTESIAN_POINT('',(23.6631666666667,7.28633333333305,2.0743333333333));
#58250=CARTESIAN_POINT('',(20.9975,9.952,3.65));
#58251=CARTESIAN_POINT('',(20.9975,9.952,3.6));
#58252=CARTESIAN_POINT('',(20.9735,9.976,3.626));
#58253=CARTESIAN_POINT('',(23.4648333333334,7.48466666666639,6.11733333333338));
#58254=CARTESIAN_POINT('',(20.8990416666667,10.0504583333333,3.70045833333333));
#58255=CARTESIAN_POINT('Origin',(20.9725,-5.,3.625));
#58256=CARTESIAN_POINT('',(20.9975,-9.952,3.65));
#58257=CARTESIAN_POINT('',(20.9975,-5.,3.65));
#58258=CARTESIAN_POINT('',(20.9735,-9.976,3.626));
#58259=CARTESIAN_POINT('',(21.7981666666667,-9.15133333333324,4.45066666666668));
#58260=CARTESIAN_POINT('',(20.9475,-9.95,3.6));
#58261=CARTESIAN_POINT('',(20.9475,-9.95,3.6));
#58262=CARTESIAN_POINT('',(20.9475,9.95,3.6));
#58263=CARTESIAN_POINT('',(20.9475,-5.,3.6));
#58264=CARTESIAN_POINT('',(20.9475,9.95,3.6));
#58265=CARTESIAN_POINT('Origin',(20.9975,-10.,3.6));
#58266=CARTESIAN_POINT('',(20.9975,-9.952,4.74));
#58267=CARTESIAN_POINT('',(20.9975,-5.,4.74));
#58268=CARTESIAN_POINT('',(20.9975,-9.952,3.6));
#58269=CARTESIAN_POINT('Origin',(20.9725,-5.,4.765));
#58270=CARTESIAN_POINT('',(20.9475,-9.95,4.79));
#58271=CARTESIAN_POINT('',(20.9475,-5.,4.79));
#58272=CARTESIAN_POINT('',(20.9735,-9.976,4.764));
#58273=CARTESIAN_POINT('',(20.9475,-9.95,4.79));
#58274=CARTESIAN_POINT('',(21.9965,-8.95299999999991,3.741));
#58275=CARTESIAN_POINT('Origin',(19.0265,-9.976,3.6));
#58276=CARTESIAN_POINT('',(19.0025,-9.952,3.65));
#58277=CARTESIAN_POINT('',(19.0025,-9.952,3.6));
#58278=CARTESIAN_POINT('',(19.0265,-9.976,3.626));
#58279=CARTESIAN_POINT('',(16.5351666666666,-7.48466666666639,6.11733333333338));
#58280=CARTESIAN_POINT('',(19.0505,-10.,3.65));
#58281=CARTESIAN_POINT('',(19.1009583333333,-10.0504583333333,3.70045833333333));
#58282=CARTESIAN_POINT('',(19.0505,-10.,4.74));
#58283=CARTESIAN_POINT('',(19.0505,-10.,3.6));
#58284=CARTESIAN_POINT('',(19.2992916666667,-10.2487916666667,4.49120833333333));
#58285=CARTESIAN_POINT('Origin',(19.0025,-10.,3.6));
#58286=CARTESIAN_POINT('',(20.9495,-10.,3.65));
#58287=CARTESIAN_POINT('',(19.50125,-10.,3.65));
#58288=CARTESIAN_POINT('',(20.9495,-10.,4.74));
#58289=CARTESIAN_POINT('',(20.9495,-10.,3.6));
#58290=CARTESIAN_POINT('',(19.50125,-10.,4.74));
#58291=CARTESIAN_POINT('Origin',(19.50125,-9.975,3.625));
#58292=CARTESIAN_POINT('',(19.0525,-9.95,3.6));
#58293=CARTESIAN_POINT('',(19.0525,-9.95,3.6));
#58294=CARTESIAN_POINT('',(19.50125,-9.95,3.6));
#58295=CARTESIAN_POINT('',(20.7327916666667,-10.2167083333333,3.86670833333333));
#58296=CARTESIAN_POINT('Origin',(19.0275,5.,3.625));
#58297=CARTESIAN_POINT('',(19.0525,9.95,3.6));
#58298=CARTESIAN_POINT('',(19.0025,10.,3.65));
#58299=CARTESIAN_POINT('',(19.0525,5.,3.6));
#58300=CARTESIAN_POINT('',(19.0025,5.,3.65));
#58301=CARTESIAN_POINT('Origin',(20.9735,-9.976,3.6));
#58302=CARTESIAN_POINT('',(20.5344583333334,-10.4150416666667,4.32495833333334));
#58303=CARTESIAN_POINT('Origin',(20.49875,9.975,3.625));
#58304=CARTESIAN_POINT('',(20.49875,9.95,3.6));
#58305=CARTESIAN_POINT('Origin',(20.,0.,3.6));
#58306=CARTESIAN_POINT('Origin',(19.50125,-9.975,4.765));
#58307=CARTESIAN_POINT('',(19.50125,-9.95,4.79));
#58308=CARTESIAN_POINT('Origin',(20.,0.,4.79));
#58309=CARTESIAN_POINT('Origin',(19.0025,10.,3.6));
#58310=CARTESIAN_POINT('',(0.,0.,0.));
#58311=CARTESIAN_POINT('Origin',(0.,0.,-1.97));
#58312=CARTESIAN_POINT('',(-0.791095370814336,2.02259992215237E-5,-3.8846668491763));
#58313=CARTESIAN_POINT('',(-0.791088063690405,1.27402156131747E-5,-3.91313315082371));
#58314=CARTESIAN_POINT('',(-0.7911,-9.68818082805471E-17,-1.97));
#58315=CARTESIAN_POINT('',(0.342080900406933,0.713328864346838,-3.9489));
#58316=CARTESIAN_POINT('Ctrl Pts',(-0.791095370814336,2.02259992215237E-5,
-3.8846668491763));
#58317=CARTESIAN_POINT('Ctrl Pts',(-0.791127180071213,0.0317239595158518,
-3.88594249553439));
#58318=CARTESIAN_POINT('Ctrl Pts',(-0.789257131989506,0.0634239528721169,
-3.88721814189247));
#58319=CARTESIAN_POINT('Ctrl Pts',(-0.785455659529297,0.0948905938491621,
-3.88849378825056));
#58320=CARTESIAN_POINT('Ctrl Pts',(-0.769753962153839,0.224861198454451,
-3.89376275002326));
#58321=CARTESIAN_POINT('Ctrl Pts',(-0.72110136963018,0.35085071538898,-3.89903171179596));
#58322=CARTESIAN_POINT('Ctrl Pts',(-0.64537450685374,0.457642147479495,
-3.90430067356865));
#58323=CARTESIAN_POINT('Ctrl Pts',(-0.5696476440773,0.564433579570009,-3.90956963534135));
#58324=CARTESIAN_POINT('Ctrl Pts',(-0.466846511048079,0.65202692681651,
-3.91483859711405));
#58325=CARTESIAN_POINT('Ctrl Pts',(-0.349388046343934,0.709840384691014,
-3.92010755888674));
#58326=CARTESIAN_POINT('Ctrl Pts',(-0.231929581639788,0.767653842565517,
-3.92537652065944));
#58327=CARTESIAN_POINT('Ctrl Pts',(-0.0998137852607172,0.795687411068025,
-3.93064548243214));
#58328=CARTESIAN_POINT('Ctrl Pts',(0.0310013642589058,0.79055831756017,
-3.93591444420484));
#58329=CARTESIAN_POINT('Ctrl Pts',(0.138467660670603,0.786344702506695,
-3.94024296280323));
#58330=CARTESIAN_POINT('Ctrl Pts',(0.245056172644429,0.759750171050252,
-3.94457148140161));
#58331=CARTESIAN_POINT('Ctrl Pts',(0.342093838304098,0.713335417936179,
-3.9489));
#58332=CARTESIAN_POINT('',(-0.342067962509736,0.713322310757513,-3.9489));
#58333=CARTESIAN_POINT('Origin',(0.,0.,-3.9489));
#58334=CARTESIAN_POINT('Ctrl Pts',(-0.342067962509735,0.713322310757513,
-3.9489));
#58335=CARTESIAN_POINT('Ctrl Pts',(-0.46014371667664,0.65670003490751,-3.9436310382273));
#58336=CARTESIAN_POINT('Ctrl Pts',(-0.563833106070677,0.570227774954663,
-3.93836207645461));
#58337=CARTESIAN_POINT('Ctrl Pts',(-0.640649635030828,0.464237010222487,
-3.93309311468191));
#58338=CARTESIAN_POINT('Ctrl Pts',(-0.717466163990983,0.358246245490307,
-3.92782415290921));
#58339=CARTESIAN_POINT('Ctrl Pts',(-0.76740983251725,0.232736975978797,
-3.92255519113652));
#58340=CARTESIAN_POINT('Ctrl Pts',(-0.784443001930775,0.102927663684584,
-3.91728622936382));
#58341=CARTESIAN_POINT('Ctrl Pts',(-0.788918272607942,0.068821749815602,
-3.91590186985045));
#58342=CARTESIAN_POINT('Ctrl Pts',(-0.791121680212704,0.0344189972881027,
-3.91451751033708));
#58343=CARTESIAN_POINT('Ctrl Pts',(-0.791088063690405,1.27402156131747E-5,
-3.91313315082371));
#58344=CARTESIAN_POINT('Origin',(0.,0.,-1.97));
#58345=CARTESIAN_POINT('',(-0.791148086150792,-1.30343001421562E-5,-3.6846668491763));
#58346=CARTESIAN_POINT('',(-0.791154135421776,-1.08354013588121E-5,-3.71313315082371));
#58347=CARTESIAN_POINT('',(-0.7911,-9.68818082805471E-17,-1.97));
#58348=CARTESIAN_POINT('Ctrl Pts',(-0.791148086150792,-1.30343001421562E-5,
-3.6846668491763));
#58349=CARTESIAN_POINT('Ctrl Pts',(-0.791056365338982,0.117140979863682,
-3.68938162092869));
#58350=CARTESIAN_POINT('Ctrl Pts',(-0.764692832251995,0.234334903162113,
-3.69409639268107));
#58351=CARTESIAN_POINT('Ctrl Pts',(-0.714334439804961,0.340104540826193,
-3.69881116443346));
#58352=CARTESIAN_POINT('Ctrl Pts',(-0.658056753699895,0.458306694998732,
-3.70408012620616));
#58353=CARTESIAN_POINT('Ctrl Pts',(-0.571811812939802,0.562241023229086,
-3.70934908797886));
#58354=CARTESIAN_POINT('Ctrl Pts',(-0.466016861463421,0.639353638687129,
-3.71461804975155));
#58355=CARTESIAN_POINT('Ctrl Pts',(-0.360221909987037,0.716466254145174,
-3.71988701152425));
#58356=CARTESIAN_POINT('Ctrl Pts',(-0.234876947794366,0.766757156830906,
-3.72515597329695));
#58357=CARTESIAN_POINT('Ctrl Pts',(-0.105121982318275,0.784151872785568,
-3.73042493506965));
#58358=CARTESIAN_POINT('Ctrl Pts',(0.0246329831578159,0.80154658874023,
-3.73569389684234));
#58359=CARTESIAN_POINT('Ctrl Pts',(0.158797951917326,0.786045117963822,
-3.74096285861504));
#58360=CARTESIAN_POINT('Ctrl Pts',(0.281167576752436,0.739519833388521,
-3.74623182038774));
#58361=CARTESIAN_POINT('Ctrl Pts',(0.403537201587544,0.692994548813219,
-3.75150078216043));
#58362=CARTESIAN_POINT('Ctrl Pts',(0.514111482498253,0.615445450439025,
-3.75676974393313));
#58363=CARTESIAN_POINT('Ctrl Pts',(0.599534514333022,0.516239437821845,
-3.76203870570583));
#58364=CARTESIAN_POINT('Ctrl Pts',(0.684957546167791,0.417033425204665,
-3.76730766747853));
#58365=CARTESIAN_POINT('Ctrl Pts',(0.745229328926622,0.2961704983445,-3.77257662925122));
#58366=CARTESIAN_POINT('Ctrl Pts',(0.773069831196375,0.16824929834069,-3.77784559102392));
#58367=CARTESIAN_POINT('Ctrl Pts',(0.800910333466129,0.0403280983368783,
-3.78311455279662));
#58368=CARTESIAN_POINT('Ctrl Pts',(0.796319555246806,-0.0946513748105791,
-3.78838351456931));
#58369=CARTESIAN_POINT('Ctrl Pts',(0.759852001945513,-0.220385400473636,
-3.79365247634201));
#58370=CARTESIAN_POINT('Ctrl Pts',(0.72338444864422,-0.346119426136694,
-3.79892143811471));
#58371=CARTESIAN_POINT('Ctrl Pts',(0.655040120260958,-0.462608004315351,
-3.80419039988741));
#58372=CARTESIAN_POINT('Ctrl Pts',(0.563074103712653,-0.555780845804767,
-3.8094593616601));
#58373=CARTESIAN_POINT('Ctrl Pts',(0.471108087164348,-0.648953687294184,
-3.8147283234328));
#58374=CARTESIAN_POINT('Ctrl Pts',(0.355520382451001,-0.718810792094359,
-3.8199972852055));
#58375=CARTESIAN_POINT('Ctrl Pts',(0.230272451163248,-0.756914379389003,
-3.82526624697819));
#58376=CARTESIAN_POINT('Ctrl Pts',(0.105024519875495,-0.795017966683648,
-3.83053520875089));
#58377=CARTESIAN_POINT('Ctrl Pts',(-0.0298836379866628,-0.801368036472762,
-3.83580417052359));
#58378=CARTESIAN_POINT('Ctrl Pts',(-0.158156910444709,-0.775197525753902,
-3.84107313229629));
#58379=CARTESIAN_POINT('Ctrl Pts',(-0.286430182902755,-0.749027015035042,
-3.84634209406899));
#58380=CARTESIAN_POINT('Ctrl Pts',(-0.408068569956688,-0.690335923808209,
-3.85161105584168));
#58381=CARTESIAN_POINT('Ctrl Pts',(-0.508379764208429,-0.606213471982601,
-3.85688001761438));
#58382=CARTESIAN_POINT('Ctrl Pts',(-0.60869095846017,-0.522091020156992,
-3.86214897938708));
#58383=CARTESIAN_POINT('Ctrl Pts',(-0.687674959909718,-0.412537207732608,
-3.86741794115977));
#58384=CARTESIAN_POINT('Ctrl Pts',(-0.735791559520864,-0.290784455382393,
-3.87268690293247));
#58385=CARTESIAN_POINT('Ctrl Pts',(-0.772258849893215,-0.198508754076189,
-3.87668021834708));
#58386=CARTESIAN_POINT('Ctrl Pts',(-0.790995794317285,-0.0992259380727511,
-3.88067353376169));
#58387=CARTESIAN_POINT('Ctrl Pts',(-0.791095370814336,2.02259992215237E-5,
-3.8846668491763));
#58388=CARTESIAN_POINT('Ctrl Pts',(-0.791088063690405,1.27402156131747E-5,
-3.91313315082371));
#58389=CARTESIAN_POINT('Ctrl Pts',(-0.790993733556351,-0.0965334406484677,
-3.90924854856438));
#58390=CARTESIAN_POINT('Ctrl Pts',(-0.773285078394182,-0.193107216295182,
-3.90536394630505));
#58391=CARTESIAN_POINT('Ctrl Pts',(-0.738731862930085,-0.283227384398608,
-3.90147934404572));
#58392=CARTESIAN_POINT('Ctrl Pts',(-0.691864884215088,-0.405463765110667,
-3.89621038227303));
#58393=CARTESIAN_POINT('Ctrl Pts',(-0.614008256484312,-0.515827171457867,
-3.89094142050033));
#58394=CARTESIAN_POINT('Ctrl Pts',(-0.514564415044768,-0.600974467117274,
-3.88567245872763));
#58395=CARTESIAN_POINT('Ctrl Pts',(-0.415120573605223,-0.686121762776682,
-3.88040349695494));
#58396=CARTESIAN_POINT('Ctrl Pts',(-0.29408951845691,-0.746052947748297,
-3.87513453518224));
#58397=CARTESIAN_POINT('Ctrl Pts',(-0.166091021675515,-0.773535586441187,
-3.86986557340954));
#58398=CARTESIAN_POINT('Ctrl Pts',(-0.0380925248941205,-0.801018225134078,
-3.86459661163685));
#58399=CARTESIAN_POINT('Ctrl Pts',(0.0968734135203562,-0.796052317548245,
-3.85932764986415));
#58400=CARTESIAN_POINT('Ctrl Pts',(0.222505123087384,-0.75923438303122,
-3.85405868809145));
#58401=CARTESIAN_POINT('Ctrl Pts',(0.348136832654412,-0.722416448514195,
-3.84878972631875));
#58402=CARTESIAN_POINT('Ctrl Pts',(0.46443431337399,-0.653746487065977,
-3.84352076454606));
#58403=CARTESIAN_POINT('Ctrl Pts',(0.557350157120219,-0.561520602927027,
-3.83825180277336));
#58404=CARTESIAN_POINT('Ctrl Pts',(0.650266000866448,-0.469294718788076,
-3.83298284100066));
#58405=CARTESIAN_POINT('Ctrl Pts',(0.719800207639327,-0.353512911958392,
-3.82771387922796));
#58406=CARTESIAN_POINT('Ctrl Pts',(0.757554078908919,-0.228159226736181,
-3.82244491745526));
#58407=CARTESIAN_POINT('Ctrl Pts',(0.79530795017851,-0.10280554151397,-3.81717595568257));
#58408=CARTESIAN_POINT('Ctrl Pts',(0.801281485944814,0.0321200221007681,
-3.81190699390987));
#58409=CARTESIAN_POINT('Ctrl Pts',(0.77475310587338,0.160319807147988,-3.80663803213718));
#58410=CARTESIAN_POINT('Ctrl Pts',(0.748224725801946,0.288519592195209,
-3.80136907036448));
#58411=CARTESIAN_POINT('Ctrl Pts',(0.689194429892775,0.409993598674911,
-3.79610010859178));
#58412=CARTESIAN_POINT('Ctrl Pts',(0.604792323138865,0.510069604101474,
-3.79083114681908));
#58413=CARTESIAN_POINT('Ctrl Pts',(0.520390216384955,0.610145609528036,
-3.78556218504638));
#58414=CARTESIAN_POINT('Ctrl Pts',(0.410616298786307,0.68882361390146,-3.78029322327369));
#58415=CARTESIAN_POINT('Ctrl Pts',(0.288729787557062,0.736600243804584,
-3.77502426150099));
#58416=CARTESIAN_POINT('Ctrl Pts',(0.166843276327817,0.784376873707709,
-3.7697552997283));
#58417=CARTESIAN_POINT('Ctrl Pts',(0.0328441714679761,0.801252129140533,
-3.7644863379556));
#58418=CARTESIAN_POINT('Ctrl Pts',(-0.0970822064716226,0.785187762022969,
-3.7592173761829));
#58419=CARTESIAN_POINT('Ctrl Pts',(-0.227008584411221,0.769123394905404,
-3.7539484144102));
#58420=CARTESIAN_POINT('Ctrl Pts',(-0.352862235430576,0.72011940523745,
-3.7486794526375));
#58421=CARTESIAN_POINT('Ctrl Pts',(-0.459441713072965,0.644094794404274,
-3.74341049086481));
#58422=CARTESIAN_POINT('Ctrl Pts',(-0.566021190715353,0.568070183571098,
-3.73814152909211));
#58423=CARTESIAN_POINT('Ctrl Pts',(-0.653326494980774,0.465024951572699,
-3.73287256731941));
#58424=CARTESIAN_POINT('Ctrl Pts',(-0.710812302136216,0.347405609839384,
-3.72760360554672));
#58425=CARTESIAN_POINT('Ctrl Pts',(-0.763437835435081,0.239730674211535,
-3.72278012063905));
#58426=CARTESIAN_POINT('Ctrl Pts',(-0.79107303432946,0.11984185467478,-3.71795663573138));
#58427=CARTESIAN_POINT('Ctrl Pts',(-0.791154135421776,-1.08354013588121E-5,
-3.71313315082371));
#58428=CARTESIAN_POINT('Origin',(0.,0.,-1.97));
#58429=CARTESIAN_POINT('',(-0.791035972316788,-5.6290844032969E-6,-3.4846668491763));
#58430=CARTESIAN_POINT('',(-0.791038502556067,-7.96146359545246E-6,-3.51313315082371));
#58431=CARTESIAN_POINT('',(-0.7911,-9.68818082805471E-17,-1.97));
#58432=CARTESIAN_POINT('Ctrl Pts',(-0.791035972316788,-5.6290844032969E-6,
-3.4846668491763));
#58433=CARTESIAN_POINT('Ctrl Pts',(-0.791017986661468,0.0717093183474517,
-3.48755178455029));
#58434=CARTESIAN_POINT('Ctrl Pts',(-0.781352061791521,0.143429019127269,
-3.49043671992428));
#58435=CARTESIAN_POINT('Ctrl Pts',(-0.762101399692471,0.2124764625646,-3.49332165529827));
#58436=CARTESIAN_POINT('Ctrl Pts',(-0.726942552248791,0.338582698168257,
-3.49859061707097));
#58437=CARTESIAN_POINT('Ctrl Pts',(-0.659812564339618,0.455775271058536,
-3.50385957884366));
#58438=CARTESIAN_POINT('Ctrl Pts',(-0.568819847341814,0.549898874182554,
-3.50912854061636));
#58439=CARTESIAN_POINT('Ctrl Pts',(-0.477827130344009,0.644022477306572,
-3.51439750238906));
#58440=CARTESIAN_POINT('Ctrl Pts',(-0.362971684257575,0.715077110664329,
-3.51966646416176));
#58441=CARTESIAN_POINT('Ctrl Pts',(-0.238126522243223,0.754480317809225,
-3.52493542593445));
#58442=CARTESIAN_POINT('Ctrl Pts',(-0.113281360228871,0.793883524954121,
-3.53020438770715));
#58443=CARTESIAN_POINT('Ctrl Pts',(0.0215535177133972,0.801635305886155,
-3.53547334947985));
#58444=CARTESIAN_POINT('Ctrl Pts',(0.150091848285218,0.776799348374844,
-3.54074231125254));
#58445=CARTESIAN_POINT('Ctrl Pts',(0.278630178857039,0.751963390863533,
-3.54601127302524));
#58446=CARTESIAN_POINT('Ctrl Pts',(0.400871962058412,0.694539694908876,
-3.55128023479794));
#58447=CARTESIAN_POINT('Ctrl Pts',(0.502052013260071,0.611464280672721,
-3.55654919657064));
#58448=CARTESIAN_POINT('Ctrl Pts',(0.60323206446173,0.528388866436566,-3.56181815834333));
#58449=CARTESIAN_POINT('Ctrl Pts',(0.683350383663675,0.419661733918913,
-3.56708712011603));
#58450=CARTESIAN_POINT('Ctrl Pts',(0.732729741491315,0.298415677355171,
-3.57235608188873));
#58451=CARTESIAN_POINT('Ctrl Pts',(0.782109099318956,0.177169620791428,
-3.57762504366142));
#58452=CARTESIAN_POINT('Ctrl Pts',(0.800749495772293,0.0434046401815959,
-3.58289400543412));
#58453=CARTESIAN_POINT('Ctrl Pts',(0.786399418414295,-0.0867222305693646,
-3.58816296720682));
#58454=CARTESIAN_POINT('Ctrl Pts',(0.772049341056297,-0.216849101320323,
-3.59343192897952));
#58455=CARTESIAN_POINT('Ctrl Pts',(0.724708789886964,-0.34333786221241,
-3.59870089075221));
#58456=CARTESIAN_POINT('Ctrl Pts',(0.650095875033401,-0.450910350093206,
-3.60396985252491));
#58457=CARTESIAN_POINT('Ctrl Pts',(0.575482960179837,-0.558482837974004,
-3.60923881429761));
#58458=CARTESIAN_POINT('Ctrl Pts',(0.473597681642042,-0.647139052843511,
-3.61450777607031));
#58459=CARTESIAN_POINT('Ctrl Pts',(0.356746428521924,-0.706170500867693,
-3.619776737843));
#58460=CARTESIAN_POINT('Ctrl Pts',(0.239895175401807,-0.765201948891874,
-3.6250456996157));
#58461=CARTESIAN_POINT('Ctrl Pts',(0.108077947699368,-0.79460863007073,
-3.6303146613884));
#58462=CARTESIAN_POINT('Ctrl Pts',(-0.0227834833757317,-0.79083860770631,
-3.63558362316109));
#58463=CARTESIAN_POINT('Ctrl Pts',(-0.153644914450832,-0.787068585341889,
-3.64085258493379));
#58464=CARTESIAN_POINT('Ctrl Pts',(-0.283550548898593,-0.750121859434192,
-3.64612154670649));
#58465=CARTESIAN_POINT('Ctrl Pts',(-0.396809510599002,-0.684461103979865,
-3.65139050847919));
#58466=CARTESIAN_POINT('Ctrl Pts',(-0.510068472299412,-0.618800348525538,
-3.65665947025188));
#58467=CARTESIAN_POINT('Ctrl Pts',(-0.606680761252469,-0.52442556352458,
-3.66192843202458));
#58468=CARTESIAN_POINT('Ctrl Pts',(-0.674976895496427,-0.412735970199464,
-3.66719739379728));
#58469=CARTESIAN_POINT('Ctrl Pts',(-0.743273029740385,-0.301046376874347,
-3.67246635556998));
#58470=CARTESIAN_POINT('Ctrl Pts',(-0.783253009275243,-0.172041975225071,
-3.67773531734267));
#58471=CARTESIAN_POINT('Ctrl Pts',(-0.790087783317653,-0.04130478434307,
-3.68300427911537));
#58472=CARTESIAN_POINT('Ctrl Pts',(-0.790806665657055,-0.027553831195994,
-3.68355846913568));
#58473=CARTESIAN_POINT('Ctrl Pts',(-0.791158867321383,-0.0137837084490869,
-3.68411265915599));
#58474=CARTESIAN_POINT('Ctrl Pts',(-0.791148086150792,-1.30343001421562E-5,
-3.6846668491763));
#58475=CARTESIAN_POINT('Ctrl Pts',(-0.791154135421776,-1.08354013588121E-5,
-3.71313315082371));
#58476=CARTESIAN_POINT('Ctrl Pts',(-0.791161625579006,-0.0110799279064996,
-3.71268767395868));
#58477=CARTESIAN_POINT('Ctrl Pts',(-0.790934090413866,-0.0221487122419377,
-3.71224219709365));
#58478=CARTESIAN_POINT('Ctrl Pts',(-0.790469510301835,-0.033207538364532,
-3.71179672022862));
#58479=CARTESIAN_POINT('Ctrl Pts',(-0.784974601266551,-0.164007893366901,
-3.70652775845593));
#58480=CARTESIAN_POINT('Ctrl Pts',(-0.746318473150519,-0.293415151903407,
-3.70125879668323));
#58481=CARTESIAN_POINT('Ctrl Pts',(-0.679170272548202,-0.405798631037627,
-3.69598983491053));
#58482=CARTESIAN_POINT('Ctrl Pts',(-0.612022071945885,-0.518182110171848,
-3.69072087313784));
#58483=CARTESIAN_POINT('Ctrl Pts',(-0.516381798857284,-0.613541809903783,
-3.68545191136514));
#58484=CARTESIAN_POINT('Ctrl Pts',(-0.40380152889302,-0.680359546472222,
-3.68018294959244));
#58485=CARTESIAN_POINT('Ctrl Pts',(-0.291221258928757,-0.747177283040659,
-3.67491398781975));
#58486=CARTESIAN_POINT('Ctrl Pts',(-0.161700992088831,-0.785453056445601,
-3.66964502604705));
#58487=CARTESIAN_POINT('Ctrl Pts',(-0.0308850570683372,-0.79056366032998,
-3.66437606427435));
#58488=CARTESIAN_POINT('Ctrl Pts',(0.099930877952157,-0.795674264214359,
-3.65910710250165));
#58489=CARTESIAN_POINT('Ctrl Pts',(0.232042481153218,-0.767619698578176,
-3.65383814072896));
#58490=CARTESIAN_POINT('Ctrl Pts',(0.349492424604498,-0.709788583056294,
-3.64856917895626));
#58491=CARTESIAN_POINT('Ctrl Pts',(0.466942368055779,-0.651957467534411,
-3.64330021718356));
#58492=CARTESIAN_POINT('Ctrl Pts',(0.569730651757277,-0.564349802126829,
-3.63803125541086));
#58493=CARTESIAN_POINT('Ctrl Pts',(0.645441815605794,-0.457547429533762,
-3.63276229363817));
#58494=CARTESIAN_POINT('Ctrl Pts',(0.72115297945431,-0.350745056940696,
-3.62749333186547));
#58495=CARTESIAN_POINT('Ctrl Pts',(0.769787023449843,-0.224747977162145,
-3.62222437009277));
#58496=CARTESIAN_POINT('Ctrl Pts',(0.785469600685382,-0.0947749649415118,
-3.61695540832007));
#58497=CARTESIAN_POINT('Ctrl Pts',(0.80115217792092,0.0351980472791211,
-3.61168644654738));
#58498=CARTESIAN_POINT('Ctrl Pts',(0.783883288396462,0.169146991941836,
-3.60641748477468));
#58499=CARTESIAN_POINT('Ctrl Pts',(0.735748784728155,0.290892614798992,
-3.60114852300198));
#58500=CARTESIAN_POINT('Ctrl Pts',(0.687614281059848,0.412638237656147,
-3.59587956122929));
#58501=CARTESIAN_POINT('Ctrl Pts',(0.608614163247692,0.522180538707743,
-3.59061059945659));
#58502=CARTESIAN_POINT('Ctrl Pts',(0.508290596778049,0.606288262143795,
-3.58534163768389));
#58503=CARTESIAN_POINT('Ctrl Pts',(0.407967030308406,0.690395985579847,
-3.58007267591119));
#58504=CARTESIAN_POINT('Ctrl Pts',(0.286320015181275,0.749069131400354,
-3.5748037141385));
#58505=CARTESIAN_POINT('Ctrl Pts',(0.158042895940592,0.77522076250535,-3.5695347523658));
#58506=CARTESIAN_POINT('Ctrl Pts',(0.0297657766999073,0.801372393610346,
-3.5642657905931));
#58507=CARTESIAN_POINT('Ctrl Pts',(-0.105141446654331,0.79500250999983,
-3.55899682882041));
#58508=CARTESIAN_POINT('Ctrl Pts',(-0.230383772459609,0.756880509043066,
-3.55372786704771));
#58509=CARTESIAN_POINT('Ctrl Pts',(-0.355626098264886,0.718758508086303,
-3.54845890527501));
#58510=CARTESIAN_POINT('Ctrl Pts',(-0.471203526521203,0.648884389783291,
-3.54318994350231));
#58511=CARTESIAN_POINT('Ctrl Pts',(-0.563155838205542,0.555698020038532,
-3.53792098172961));
#58512=CARTESIAN_POINT('Ctrl Pts',(-0.655108149889881,0.462511650293772,
-3.53265201995692));
#58513=CARTESIAN_POINT('Ctrl Pts',(-0.723435345002244,0.346013029107264,
-3.52738305818422));
#58514=CARTESIAN_POINT('Ctrl Pts',(-0.759884405429078,0.220273643375871,
-3.52211409641153));
#58515=CARTESIAN_POINT('Ctrl Pts',(-0.780593547162765,0.148832713757253,
-3.51912044788225));
#58516=CARTESIAN_POINT('Ctrl Pts',(-0.791012000528327,0.0744087417130748,
-3.51612679935298));
#58517=CARTESIAN_POINT('Ctrl Pts',(-0.791038502556067,-7.96146359545246E-6,
-3.51313315082371));
#58518=CARTESIAN_POINT('Origin',(0.,0.,-1.97));
#58519=CARTESIAN_POINT('',(-0.791112467551816,1.9457402925846E-5,-3.2846668491763));
#58520=CARTESIAN_POINT('',(-0.791104010802578,1.99443795460114E-5,-3.31313315082371));
#58521=CARTESIAN_POINT('',(-0.7911,-9.68818082805471E-17,-1.97));
#58522=CARTESIAN_POINT('Ctrl Pts',(-0.791112467551816,1.9457402925846E-5,
-3.2846668491763));
#58523=CARTESIAN_POINT('Ctrl Pts',(-0.791139111989659,0.0262402740262119,
-3.28572194817189));
#58524=CARTESIAN_POINT('Ctrl Pts',(-0.789860844776933,0.0524585044539771,
-3.28677704716749));
#58525=CARTESIAN_POINT('Ctrl Pts',(-0.787258239359726,0.078544605909112,
-3.28783214616308));
#58526=CARTESIAN_POINT('Ctrl Pts',(-0.774261327686072,0.208813587246341,
-3.29310110793578));
#58527=CARTESIAN_POINT('Ctrl Pts',(-0.728237913550483,0.335787520668241,
-3.29837006970847));
#58528=CARTESIAN_POINT('Ctrl Pts',(-0.654747014411506,0.444129640619056,
-3.30363903148117));
#58529=CARTESIAN_POINT('Ctrl Pts',(-0.581256115272529,0.552471760569871,
-3.30890799325386));
#58530=CARTESIAN_POINT('Ctrl Pts',(-0.480297731130164,0.642182067049603,
-3.31417695502656));
#58531=CARTESIAN_POINT('Ctrl Pts',(-0.364066294548254,0.702424745955819,
-3.31944591679926));
#58532=CARTESIAN_POINT('Ctrl Pts',(-0.247834857966343,0.762667424862035,
-3.32471487857196));
#58533=CARTESIAN_POINT('Ctrl Pts',(-0.116330368944885,0.793442476194735,
-3.32998384034465));
#58534=CARTESIAN_POINT('Ctrl Pts',(0.0145631759878715,0.791032682297223,
-3.33525280211735));
#58535=CARTESIAN_POINT('Ctrl Pts',(0.145456720920629,0.788622888399711,
-3.34052176389005));
#58536=CARTESIAN_POINT('Ctrl Pts',(0.275739321764686,0.753028249271988,
-3.34579072566275));
#58537=CARTESIAN_POINT('Ctrl Pts',(0.389674569862843,0.6885481247955,-3.35105968743544));
#58538=CARTESIAN_POINT('Ctrl Pts',(0.503609817961001,0.624068000319013,
-3.35632864920814));
#58539=CARTESIAN_POINT('Ctrl Pts',(0.601197713313261,0.53070239049376,-3.36159761098084));
#58540=CARTESIAN_POINT('Ctrl Pts',(0.670650933657783,0.41972862154151,-3.36686657275354));
#58541=CARTESIAN_POINT('Ctrl Pts',(0.740104154002306,0.308754852589261,
-3.37213553452623));
#58542=CARTESIAN_POINT('Ctrl Pts',(0.781422699339092,0.180172924510018,
-3.37740449629893));
#58543=CARTESIAN_POINT('Ctrl Pts',(0.789615837902518,0.0495138272677194,
-3.38267345807163));
#58544=CARTESIAN_POINT('Ctrl Pts',(0.797808976465944,-0.0811452699745802,
-3.38794241984432));
#58545=CARTESIAN_POINT('Ctrl Pts',(0.772876708256009,-0.213881536379933,
-3.39321138161702));
#58546=CARTESIAN_POINT('Ctrl Pts',(0.717830520292166,-0.332662193064182,
-3.39848034338972));
#58547=CARTESIAN_POINT('Ctrl Pts',(0.662784332328323,-0.45144284974843,
-3.40374930516242));
#58548=CARTESIAN_POINT('Ctrl Pts',(0.577624224610571,-0.556267896711576,
-3.40901826693511));
#58549=CARTESIAN_POINT('Ctrl Pts',(0.472636407635597,-0.634475859851665,
-3.41428722870781));
#58550=CARTESIAN_POINT('Ctrl Pts',(0.367648590660623,-0.712683822991754,
-3.41955619048051));
#58551=CARTESIAN_POINT('Ctrl Pts',(0.242833064428427,-0.764274702308787,
-3.4248251522532));
#58552=CARTESIAN_POINT('Ctrl Pts',(0.113265887559485,-0.783017004459389,
-3.4300941140259));
#58553=CARTESIAN_POINT('Ctrl Pts',(-0.0163012893094561,-0.801759306609992,
-3.4353630757986));
#58554=CARTESIAN_POINT('Ctrl Pts',(-0.150620116815143,-0.787653031594163,
-3.4406320375713));
#58555=CARTESIAN_POINT('Ctrl Pts',(-0.273466663701279,-0.742402030170502,
-3.44590099934399));
#58556=CARTESIAN_POINT('Ctrl Pts',(-0.396313210587416,-0.697151028746841,
-3.45116996111669));
#58557=CARTESIAN_POINT('Ctrl Pts',(-0.507687476854002,-0.620755300915348,
-3.45643892288939));
#58558=CARTESIAN_POINT('Ctrl Pts',(-0.594136929649284,-0.522442436431149,
-3.46170788466209));
#58559=CARTESIAN_POINT('Ctrl Pts',(-0.680586382444567,-0.42412957194695,
-3.46697684643478));
#58560=CARTESIAN_POINT('Ctrl Pts',(-0.742111021768545,-0.303899570810043,
-3.47224580820748));
#58561=CARTESIAN_POINT('Ctrl Pts',(-0.771279487941441,-0.176274621083071,
-3.47751476998018));
#58562=CARTESIAN_POINT('Ctrl Pts',(-0.784477229046018,-0.118528662313859,
-3.47989879637888));
#58563=CARTESIAN_POINT('Ctrl Pts',(-0.791050835137449,-0.0592687687029965,
-3.48228282277759));
#58564=CARTESIAN_POINT('Ctrl Pts',(-0.791035972316788,-5.6290844032969E-6,
-3.4846668491763));
#58565=CARTESIAN_POINT('Ctrl Pts',(-0.791038502556067,-7.96146359545246E-6,
-3.51313315082371));
#58566=CARTESIAN_POINT('Ctrl Pts',(-0.791058645339732,-0.0565681450035753,
-3.51085783758028));
#58567=CARTESIAN_POINT('Ctrl Pts',(-0.785075656402411,-0.113124129527635,
-3.50858252433686));
#58568=CARTESIAN_POINT('Ctrl Pts',(-0.773045075503138,-0.168362997183885,
-3.50630721109343));
#58569=CARTESIAN_POINT('Ctrl Pts',(-0.745185759409057,-0.296280101735969,
-3.50103824932074));
#58570=CARTESIAN_POINT('Ctrl Pts',(-0.684896201479589,-0.41713416056386,
-3.49576928754804));
#58571=CARTESIAN_POINT('Ctrl Pts',(-0.599458579958063,-0.516327607720986,
-3.49050032577534));
#58572=CARTESIAN_POINT('Ctrl Pts',(-0.514020958436537,-0.615521054878112,
-3.48523136400264));
#58573=CARTESIAN_POINT('Ctrl Pts',(-0.403435273322952,-0.693053890364472,
-3.47996240222995));
#58574=CARTESIAN_POINT('Ctrl Pts',(-0.281058807334294,-0.739561176915201,
-3.47469344045725));
#58575=CARTESIAN_POINT('Ctrl Pts',(-0.158682341345636,-0.78606846346593,
-3.46942447868455));
#58576=CARTESIAN_POINT('Ctrl Pts',(-0.0245150944819038,-0.801550201081026,
-3.46415551691186));
#58577=CARTESIAN_POINT('Ctrl Pts',(0.105237310929872,-0.784136401379585,
-3.45888655513916));
#58578=CARTESIAN_POINT('Ctrl Pts',(0.234989716341648,-0.766722601678145,
-3.45361759336646));
#58579=CARTESIAN_POINT('Ctrl Pts',(0.360327280301469,-0.716413264660167,
-3.44834863159376));
#58580=CARTESIAN_POINT('Ctrl Pts',(0.466110888961514,-0.639285090371915,
-3.44307966982107));
#58581=CARTESIAN_POINT('Ctrl Pts',(0.571894497621558,-0.562156916083665,
-3.43781070804837));
#58582=CARTESIAN_POINT('Ctrl Pts',(0.658124150981828,-0.458209904525141,
-3.43254174627567));
#58583=CARTESIAN_POINT('Ctrl Pts',(0.714384451630426,-0.339999474777539,
-3.42727278450297));
#58584=CARTESIAN_POINT('Ctrl Pts',(0.770644752279024,-0.221789045029936,
-3.42200382273028));
#58585=CARTESIAN_POINT('Ctrl Pts',(0.796935700215949,-0.0893151970932543,
-3.41673486095758));
#58586=CARTESIAN_POINT('Ctrl Pts',(0.790081697947446,0.0414209868157352,
-3.41146589918488));
#58587=CARTESIAN_POINT('Ctrl Pts',(0.783227695678943,0.172157170724725,
-3.40619693741219));
#58588=CARTESIAN_POINT('Ctrl Pts',(0.743228743205012,0.301155690606022,
-3.40092797563949));
#58589=CARTESIAN_POINT('Ctrl Pts',(0.674916182991274,0.412835237736315,
-3.39565901386679));
#58590=CARTESIAN_POINT('Ctrl Pts',(0.606603622777536,0.524514784866607,
-3.39039005209409));
#58591=CARTESIAN_POINT('Ctrl Pts',(0.509977454823992,0.618875359245894,
-3.3851210903214));
#58592=CARTESIAN_POINT('Ctrl Pts',(0.396708837489817,0.684519456142618,
-3.3798521285487));
#58593=CARTESIAN_POINT('Ctrl Pts',(0.283440220155643,0.750163553039342,
-3.374583166776));
#58594=CARTESIAN_POINT('Ctrl Pts',(0.153529153440839,0.787091172453503,
-3.3693142050033));
#58595=CARTESIAN_POINT('Ctrl Pts',(0.0226671696119708,0.790841948180603,
-3.36404524323061));
#58596=CARTESIAN_POINT('Ctrl Pts',(-0.108194814216899,0.794592723907703,
-3.35877628145791));
#58597=CARTESIAN_POINT('Ctrl Pts',(-0.240007715159833,0.765166655947741,
-3.35350731968522));
#58598=CARTESIAN_POINT('Ctrl Pts',(-0.356850284622694,0.70611802267398,
-3.34823835791252));
#58599=CARTESIAN_POINT('Ctrl Pts',(-0.473692854085554,0.64706938940022,
-3.34296939613982));
#58600=CARTESIAN_POINT('Ctrl Pts',(-0.575565092068342,0.558398190812661,
-3.33770043436712));
#58601=CARTESIAN_POINT('Ctrl Pts',(-0.650162184594864,0.450814730574705,
-3.33243147259442));
#58602=CARTESIAN_POINT('Ctrl Pts',(-0.724759277121385,0.343231270336749,
-3.32716251082173));
#58603=CARTESIAN_POINT('Ctrl Pts',(-0.772081224191642,0.216735548448396,
-3.32189354904903));
#58604=CARTESIAN_POINT('Ctrl Pts',(-0.786412162806834,0.0866065688604893,
-3.31662458727633));
#58605=CARTESIAN_POINT('Ctrl Pts',(-0.789577591066389,0.0578635841589875,
-3.31546077512546));
#58606=CARTESIAN_POINT('Ctrl Pts',(-0.791133444132945,0.0289433389935947,
-3.31429696297458));
#58607=CARTESIAN_POINT('Ctrl Pts',(-0.791104010802578,1.99443795460114E-5,
-3.31313315082371));
#58608=CARTESIAN_POINT('Origin',(0.,0.,-1.97));
#58609=CARTESIAN_POINT('',(-0.79113354225774,-1.66712748377318E-5,-3.0846668491763));
#58610=CARTESIAN_POINT('',(-0.791141030195672,-1.50259769734546E-5,-3.11313315082371));
#58611=CARTESIAN_POINT('',(-0.7911,-9.68818082805471E-17,-1.97));
#58612=CARTESIAN_POINT('Ctrl Pts',(-0.79113354225774,-1.66712748377318E-5,
-3.0846668491763));
#58613=CARTESIAN_POINT('Ctrl Pts',(-0.791029149168141,0.111663060150681,
-3.08916107356619));
#58614=CARTESIAN_POINT('Ctrl Pts',(-0.767145880831491,0.223386024459756,
-3.09365529795608));
#58615=CARTESIAN_POINT('Ctrl Pts',(-0.721249064670457,0.325183912992608,
-3.09814952234598));
#58616=CARTESIAN_POINT('Ctrl Pts',(-0.667440320633363,0.444530242122759,
-3.10341848411867));
#58617=CARTESIAN_POINT('Ctrl Pts',(-0.583374244479453,0.550234685063485,
-3.10868744589137));
#58618=CARTESIAN_POINT('Ctrl Pts',(-0.479204902215964,0.62952954835288,
-3.11395640766407));
#58619=CARTESIAN_POINT('Ctrl Pts',(-0.375035559952474,0.708824411642276,
-3.11922536943676));
#58620=CARTESIAN_POINT('Ctrl Pts',(-0.250762951579405,0.761709695280341,
-3.12449433120946));
#58621=CARTESIAN_POINT('Ctrl Pts',(-0.121397558447183,0.781797559065168,
-3.12976329298216));
#58622=CARTESIAN_POINT('Ctrl Pts',(0.00796783468503921,0.801885422849996,
-3.13503225475486));
#58623=CARTESIAN_POINT('Ctrl Pts',(0.142426012576414,0.789175866781586,
-3.14030121652755));
#58624=CARTESIAN_POINT('Ctrl Pts',(0.265736212293957,0.745204036511379,
-3.14557017830025));
#58625=CARTESIAN_POINT('Ctrl Pts',(0.3890464120115,0.701232206241173,-3.15083914007295));
#58626=CARTESIAN_POINT('Ctrl Pts',(0.501208633555211,0.625998101769169,
-3.15610810184565));
#58627=CARTESIAN_POINT('Ctrl Pts',(0.588675169536104,0.528589004169432,
-3.16137706361834));
#58628=CARTESIAN_POINT('Ctrl Pts',(0.676141705516998,0.431179906569694,
-3.16664602539104));
#58629=CARTESIAN_POINT('Ctrl Pts',(0.738912555935075,0.311595815842222,
-3.17191498716374));
#58630=CARTESIAN_POINT('Ctrl Pts',(0.769405835354065,0.184280902646762,
-3.17718394893643));
#58631=CARTESIAN_POINT('Ctrl Pts',(0.799899114773056,0.056965989451302,
-3.18245291070913));
#58632=CARTESIAN_POINT('Ctrl Pts',(0.798114823192961,-0.0780797462121464,
-3.18772187248183));
#58633=CARTESIAN_POINT('Ctrl Pts',(0.764268479349867,-0.204544572231665,
-3.19299083425453));
#58634=CARTESIAN_POINT('Ctrl Pts',(0.730422135506773,-0.331009398251184,
-3.19825979602722));
#58635=CARTESIAN_POINT('Ctrl Pts',(0.664513739400679,-0.448893314626773,
-3.20352875779992));
#58636=CARTESIAN_POINT('Ctrl Pts',(0.574504150335489,-0.543957509190278,
-3.20879771957262));
#58637=CARTESIAN_POINT('Ctrl Pts',(0.484494561270298,-0.639021703753782,
-3.21406668134531));
#58638=CARTESIAN_POINT('Ctrl Pts',(0.370383779246011,-0.711266176505201,
-3.21933564311801));
#58639=CARTESIAN_POINT('Ctrl Pts',(0.245954871890178,-0.751964754194423,
-3.22460460489071));
#58640=CARTESIAN_POINT('Ctrl Pts',(0.121525964534345,-0.792663331883645,
-3.22987356666341));
#58641=CARTESIAN_POINT('Ctrl Pts',(-0.0132210681530342,-0.801816014510671,
-3.2351425284361));
#58642=CARTESIAN_POINT('Ctrl Pts',(-0.142010573414216,-0.778317279517651,
-3.2404114902088));
#58643=CARTESIAN_POINT('Ctrl Pts',(-0.270800078675396,-0.754818544524631,
-3.2456804519815));
#58644=CARTESIAN_POINT('Ctrl Pts',(-0.393632056510379,-0.698668391911567,
-3.2509494137542));
#58645=CARTESIAN_POINT('Ctrl Pts',(-0.495670034613112,-0.616649014710823,
-3.2562183755269));
#58646=CARTESIAN_POINT('Ctrl Pts',(-0.597708012715845,-0.53462963751008,
-3.26148733729959));
#58647=CARTESIAN_POINT('Ctrl Pts',(-0.678951991086329,-0.426741035721658,
-3.26675629907229));
#58648=CARTESIAN_POINT('Ctrl Pts',(-0.729588775665712,-0.306014720201168,
-3.27202526084498));
#58649=CARTESIAN_POINT('Ctrl Pts',(-0.770085645997359,-0.209463606502664,
-3.27623912362209));
#58650=CARTESIAN_POINT('Ctrl Pts',(-0.791006054783621,-0.10470144899133,
-3.28045298639919));
#58651=CARTESIAN_POINT('Ctrl Pts',(-0.791112467551816,1.9457402925846E-5,
-3.2846668491763));
#58652=CARTESIAN_POINT('Ctrl Pts',(-0.791104010802578,1.99443795460114E-5,
-3.31313315082371));
#58653=CARTESIAN_POINT('Ctrl Pts',(-0.79100018973065,-0.102002415820376,
-3.30902800120189));
#58654=CARTESIAN_POINT('Ctrl Pts',(-0.7711721440249,-0.204063961641823,
-3.30492285158006));
#58655=CARTESIAN_POINT('Ctrl Pts',(-0.732685842008116,-0.298523440455128,
-3.30081770195824));
#58656=CARTESIAN_POINT('Ctrl Pts',(-0.68328865243408,-0.419762232895373,
-3.29554874018554));
#58657=CARTESIAN_POINT('Ctrl Pts',(-0.603154343125882,-0.528477580488403,
-3.29027977841284));
#58658=CARTESIAN_POINT('Ctrl Pts',(-0.501962074850703,-0.611538112460611,
-3.28501081664015));
#58659=CARTESIAN_POINT('Ctrl Pts',(-0.400769806575523,-0.694598644432819,
-3.27974185486745));
#58660=CARTESIAN_POINT('Ctrl Pts',(-0.278519579333359,-0.752004360784205,
-3.27447289309475));
#58661=CARTESIAN_POINT('Ctrl Pts',(-0.149977597681499,-0.776821413050642,
-3.26920393132206));
#58662=CARTESIAN_POINT('Ctrl Pts',(-0.0214356160296378,-0.801638465317079,
-3.26393496954936));
#58663=CARTESIAN_POINT('Ctrl Pts',(0.113398120031922,-0.793866853498568,
-3.25866600777666));
#58664=CARTESIAN_POINT('Ctrl Pts',(0.238237485128838,-0.754445285133253,
-3.25339704600397));
#58665=CARTESIAN_POINT('Ctrl Pts',(0.363076850225755,-0.715023716767938,
-3.24812808423127));
#58666=CARTESIAN_POINT('Ctrl Pts',(0.477921844358028,-0.643952191855818,
-3.24285912245857));
#58667=CARTESIAN_POINT('Ctrl Pts',(0.56890071682226,-0.549815207119108,
-3.23759016068587));
#58668=CARTESIAN_POINT('Ctrl Pts',(0.659879589286491,-0.4556782223824,-3.23232119891318));
#58669=CARTESIAN_POINT('Ctrl Pts',(0.726992340082681,-0.338475777821101,
-3.22705223714048));
#58670=CARTESIAN_POINT('Ctrl Pts',(0.762132639848386,-0.212364372854862,
-3.22178327536778));
#58671=CARTESIAN_POINT('Ctrl Pts',(0.797272939614092,-0.0862529678886238,
-3.21651431359509));
#58672=CARTESIAN_POINT('Ctrl Pts',(0.800440788349314,0.0487673974825542,
-3.21124535182239));
#58673=CARTESIAN_POINT('Ctrl Pts',(0.771253551980593,0.176388055541266,
-3.20597639004969));
#58674=CARTESIAN_POINT('Ctrl Pts',(0.742066315611872,0.304008713599979,
-3.20070742827699));
#58675=CARTESIAN_POINT('Ctrl Pts',(0.680523994139208,0.424229664346224,
-3.19543846650429));
#58676=CARTESIAN_POINT('Ctrl Pts',(0.594060083011206,0.52252981288442,-3.1901695047316));
#58677=CARTESIAN_POINT('Ctrl Pts',(0.507596171883205,0.620829961422615,
-3.1849005429589));
#58678=CARTESIAN_POINT('Ctrl Pts',(0.396210671099867,0.697209307752761,
-3.1796315811862));
#58679=CARTESIAN_POINT('Ctrl Pts',(0.273357470493429,0.742442240787621,
-3.17436261941351));
#58680=CARTESIAN_POINT('Ctrl Pts',(0.150504269886989,0.787675173822481,
-3.16909365764081));
#58681=CARTESIAN_POINT('Ctrl Pts',(0.0161833694574468,0.801761693562055,
-3.16382469586811));
#58682=CARTESIAN_POINT('Ctrl Pts',(-0.113381049157215,0.783000335422864,
-3.15855573409542));
#58683=CARTESIAN_POINT('Ctrl Pts',(-0.242945467771877,0.764238977283673,
-3.15328677232272));
#58684=CARTESIAN_POINT('Ctrl Pts',(-0.367753404571661,0.712629741265718,
-3.14801781055002));
#58685=CARTESIAN_POINT('Ctrl Pts',(-0.472729717638774,0.634406337958153,
-3.14274884877732));
#58686=CARTESIAN_POINT('Ctrl Pts',(-0.577706030705887,0.556182934650588,
-3.13747988700463));
#58687=CARTESIAN_POINT('Ctrl Pts',(-0.662850720040329,0.451345364053415,
-3.13221092523193));
#58688=CARTESIAN_POINT('Ctrl Pts',(-0.717879437481436,0.332556612957322,
-3.12694196345923));
#58689=CARTESIAN_POINT('Ctrl Pts',(-0.765952238253124,0.228783379073186,
-3.12233902591406));
#58690=CARTESIAN_POINT('Ctrl Pts',(-0.791041497371546,0.114363052701224,
-3.11773608836888));
#58691=CARTESIAN_POINT('Ctrl Pts',(-0.791141030195672,-1.50259769734546E-5,
-3.11313315082371));
#58692=CARTESIAN_POINT('Origin',(0.,0.,-1.97));
#58693=CARTESIAN_POINT('',(-0.791033587110486,-6.80849259582228E-7,-2.8846668491763));
#58694=CARTESIAN_POINT('',(-0.79103429425828,-3.14382039938683E-6,-2.91313315082371));
#58695=CARTESIAN_POINT('',(-0.7911,-9.68818082805471E-17,-1.97));
#58696=CARTESIAN_POINT('Ctrl Pts',(-0.791033587110486,-6.80849259582228E-7,
-2.8846668491763));
#58697=CARTESIAN_POINT('Ctrl Pts',(-0.791031585449306,0.0662323781931633,
-2.88733123718779));
#58698=CARTESIAN_POINT('Ctrl Pts',(-0.782802743498501,0.132465925751853,
-2.88999562519929));
#58699=CARTESIAN_POINT('Ctrl Pts',(-0.766353006923597,0.196590588117425,
-2.89266001321078));
#58700=CARTESIAN_POINT('Ctrl Pts',(-0.733822822577261,0.323400344516865,
-2.89792897498348));
#58701=CARTESIAN_POINT('Ctrl Pts',(-0.669143137337217,0.441962871204574,
-2.90319793675618));
#58702=CARTESIAN_POINT('Ctrl Pts',(-0.580126398546105,0.537957388895363,
-2.90846689852887));
#58703=CARTESIAN_POINT('Ctrl Pts',(-0.491109659754995,0.633951906586151,
-2.91373586030157));
#58704=CARTESIAN_POINT('Ctrl Pts',(-0.377755867412819,0.707378415280021,
-2.91900482207427));
#58705=CARTESIAN_POINT('Ctrl Pts',(-0.253756654842699,0.749367967476751,
-2.92427378384697));
#58706=CARTESIAN_POINT('Ctrl Pts',(-0.129757442272579,0.79135751967348,
-2.92954274561967));
#58707=CARTESIAN_POINT('Ctrl Pts',(0.00488719052548373,0.801910115373071,
-2.93481170739236));
#58708=CARTESIAN_POINT('Ctrl Pts',(0.133913959340999,0.779751141102602,
-2.94008066916506));
#58709=CARTESIAN_POINT('Ctrl Pts',(0.262940728156516,0.757592166832132,
-2.94534963093776));
#58710=CARTESIAN_POINT('Ctrl Pts',(0.386349632989485,0.702721622591603,
-2.95061859271045));
#58711=CARTESIAN_POINT('Ctrl Pts',(0.489234516411306,0.621767141709007,
-2.95588755448315));
#58712=CARTESIAN_POINT('Ctrl Pts',(0.592119399833126,0.540812660826412,
-2.96115651625585));
#58713=CARTESIAN_POINT('Ctrl Pts',(0.674480261843798,0.43377424330175,-2.96642547802854));
#58714=CARTESIAN_POINT('Ctrl Pts',(0.726369003667566,0.313580709017918,
-2.97169443980124));
#58715=CARTESIAN_POINT('Ctrl Pts',(0.778257745491333,0.193387174734087,
-2.97696340157394));
#58716=CARTESIAN_POINT('Ctrl Pts',(0.799674367128196,0.0600385236910853,
-2.98223236334664));
#58717=CARTESIAN_POINT('Ctrl Pts',(0.788032024993892,-0.0703584972922178,
-2.98750132511934));
#58718=CARTESIAN_POINT('Ctrl Pts',(0.776389682859588,-0.200755518275521,
-2.99277028689203));
#58719=CARTESIAN_POINT('Ctrl Pts',(0.731688376954118,-0.328200909199126,
-2.99803924866473));
#58720=CARTESIAN_POINT('Ctrl Pts',(0.659327431613055,-0.437300958699755,
-3.00330821043743));
#58721=CARTESIAN_POINT('Ctrl Pts',(0.586966486271991,-0.546401008200385,
-3.00857717221012));
#58722=CARTESIAN_POINT('Ctrl Pts',(0.486945901495334,-0.637155716278039,
-3.01384613398282));
#58723=CARTESIAN_POINT('Ctrl Pts',(0.371346836133002,-0.698603118981874,
-3.01911509575552));
#58724=CARTESIAN_POINT('Ctrl Pts',(0.255747770770669,-0.760050521685709,
-3.02438405752821));
#58725=CARTESIAN_POINT('Ctrl Pts',(0.12457022482266,-0.792190619015725,
-3.02965301930091));
#58726=CARTESIAN_POINT('Ctrl Pts',(-0.00634129556582329,-0.791141313879979,
-3.03492198107361));
#58727=CARTESIAN_POINT('Ctrl Pts',(-0.137252815954308,-0.790092008744234,
-3.04019094284631));
#58728=CARTESIAN_POINT('Ctrl Pts',(-0.267898310783268,-0.755853301142726,
-3.04545990461901));
#58729=CARTESIAN_POINT('Ctrl Pts',(-0.382497538619609,-0.692560772428769,
-3.0507288663917));
#58730=CARTESIAN_POINT('Ctrl Pts',(-0.497096766455945,-0.629268243714814,
-3.0559978281644));
#58731=CARTESIAN_POINT('Ctrl Pts',(-0.595649727299664,-0.536921893888413,
-3.0612667899371));
#58732=CARTESIAN_POINT('Ctrl Pts',(-0.666252531788976,-0.426675936094329,
-3.06653575170979));
#58733=CARTESIAN_POINT('Ctrl Pts',(-0.736855336278291,-0.316429978300241,
-3.07180471348249));
#58734=CARTESIAN_POINT('Ctrl Pts',(-0.779507984413199,-0.188284412538469,
-3.07707367525519));
#58735=CARTESIAN_POINT('Ctrl Pts',(-0.789058602520514,-0.0577175219977951,
-3.08234263702788));
#58736=CARTESIAN_POINT('Ctrl Pts',(-0.79046290591003,-0.0385192329567601,
-3.08311737441069));
#58737=CARTESIAN_POINT('Ctrl Pts',(-0.791151538072368,-0.019268594483546,
-3.08389211179349));
#58738=CARTESIAN_POINT('Ctrl Pts',(-0.79113354225774,-1.66712748377318E-5,
-3.0846668491763));
#58739=CARTESIAN_POINT('Ctrl Pts',(-0.791141030195672,-1.50259769734546E-5,
-3.11313315082371));
#58740=CARTESIAN_POINT('Ctrl Pts',(-0.791155432144787,-0.0165650162276427,
-3.11246712659618));
#58741=CARTESIAN_POINT('Ctrl Pts',(-0.79064662969104,-0.0331141219476401,
-3.11180110236866));
#58742=CARTESIAN_POINT('Ctrl Pts',(-0.789608545183721,-0.0496299602372971,
-3.11113507814114));
#58743=CARTESIAN_POINT('Ctrl Pts',(-0.781396189897128,-0.180287850740814,
-3.10586611636844));
#58744=CARTESIAN_POINT('Ctrl Pts',(-0.74005873377617,-0.30886370015284,
-3.10059715459575));
#58745=CARTESIAN_POINT('Ctrl Pts',(-0.670589192758155,-0.419827252731733,
-3.09532819282305));
#58746=CARTESIAN_POINT('Ctrl Pts',(-0.60111965174014,-0.530790805310627,
-3.09005923105035));
#58747=CARTESIAN_POINT('Ctrl Pts',(-0.50351802582507,-0.624142061056388,
-3.08479026927766));
#58748=CARTESIAN_POINT('Ctrl Pts',(-0.389573295744491,-0.688605427529499,
-3.07952130750496));
#58749=CARTESIAN_POINT('Ctrl Pts',(-0.275628565663913,-0.75306879400261,
-3.07425234573226));
#58750=CARTESIAN_POINT('Ctrl Pts',(-0.145340731417827,-0.788644271203071,
-3.06898338395956));
#58751=CARTESIAN_POINT('Ctrl Pts',(-0.0144468337889248,-0.79103481375587,
-3.06371442218686));
#58752=CARTESIAN_POINT('Ctrl Pts',(0.116447063839978,-0.79342535630867,
-3.05844546041417));
#58753=CARTESIAN_POINT('Ctrl Pts',(0.247947024851698,-0.762630964213808,
-3.05317649864147));
#58754=CARTESIAN_POINT('Ctrl Pts',(0.364169599641456,-0.702371191235297,
-3.04790753686877));
#58755=CARTESIAN_POINT('Ctrl Pts',(0.480392174431212,-0.642111418256788,
-3.04263857509608));
#58756=CARTESIAN_POINT('Ctrl Pts',(0.581337362999006,-0.552386264394629,
-3.03736961332338));
#58757=CARTESIAN_POINT('Ctrl Pts',(0.654812326631231,-0.444033337117951,
-3.03210065155068));
#58758=CARTESIAN_POINT('Ctrl Pts',(0.728287290263455,-0.335680409841273,
-3.02683168977798));
#58759=CARTESIAN_POINT('Ctrl Pts',(0.774292028960111,-0.208699709150073,
-3.02156272800529));
#58760=CARTESIAN_POINT('Ctrl Pts',(0.787269781007753,-0.0784288179964015,
-3.01629376623259));
#58761=CARTESIAN_POINT('Ctrl Pts',(0.800247533055396,0.0518420731572732,
-3.01102480445989));
#58762=CARTESIAN_POINT('Ctrl Pts',(0.780198298454025,0.185403154773419,
-3.0057558426872));
#58763=CARTESIAN_POINT('Ctrl Pts',(0.729543758586319,0.306122021239989,
-3.0004868809145));
#58764=CARTESIAN_POINT('Ctrl Pts',(0.678889218718613,0.426840887706558,
-2.9952179191418));
#58765=CARTESIAN_POINT('Ctrl Pts',(0.597629373584572,0.53471753902355,-2.9899489573691));
#58766=CARTESIAN_POINT('Ctrl Pts',(0.495579333737454,0.616721907793659,
-2.98467999559641));
#58767=CARTESIAN_POINT('Ctrl Pts',(0.393529293890335,0.698726276563767,
-2.97941103382371));
#58768=CARTESIAN_POINT('Ctrl Pts',(0.270689059330137,0.754858362786991,
-2.97414207205101));
#58769=CARTESIAN_POINT('Ctrl Pts',(0.141896099665709,0.778338155611023,
-2.96887311027832));
#58770=CARTESIAN_POINT('Ctrl Pts',(0.0131031400012812,0.801817948435054,
-2.96360414850562));
#58771=CARTESIAN_POINT('Ctrl Pts',(-0.121642544767378,0.792645447859891,
-2.95833518673292));
#58772=CARTESIAN_POINT('Ctrl Pts',(-0.24606546469321,0.751928570188435,
-2.95306622496022));
#58773=CARTESIAN_POINT('Ctrl Pts',(-0.370488384619043,0.711211692516977,
-2.94779726318752));
#58774=CARTESIAN_POINT('Ctrl Pts',(-0.484588539702047,0.638950437749227,
-2.94252830141483));
#58775=CARTESIAN_POINT('Ctrl Pts',(-0.57458414590811,0.54387300618008,-2.93725933964213));
#58776=CARTESIAN_POINT('Ctrl Pts',(-0.664579752114172,0.448795574610933,
-2.93199037786943));
#58777=CARTESIAN_POINT('Ctrl Pts',(-0.730470809443291,0.330901966240389,
-2.92672141609674));
#58778=CARTESIAN_POINT('Ctrl Pts',(-0.764298552885645,0.204432163900935,
-2.92145245432404));
#58779=CARTESIAN_POINT('Ctrl Pts',(-0.782102393349158,0.137869988740161,
-2.91867935315726));
#58780=CARTESIAN_POINT('Ctrl Pts',(-0.791024663908618,0.0689321993021295,
-2.91590625199048));
#58781=CARTESIAN_POINT('Ctrl Pts',(-0.79103429425828,-3.14382039938683E-6,
-2.91313315082371));
#58782=CARTESIAN_POINT('Origin',(0.,0.,-1.97));
#58783=CARTESIAN_POINT('',(-0.791129214786214,1.74461675192319E-5,-2.6846668491763));
#58784=CARTESIAN_POINT('',(-0.791121074183877,1.86068176132095E-5,-2.71313315082371));
#58785=CARTESIAN_POINT('',(-0.7911,-9.68818082805471E-17,-1.97));
#58786=CARTESIAN_POINT('Ctrl Pts',(-0.791129214786214,1.74461675192319E-5,
-2.6846668491763));
#58787=CARTESIAN_POINT('Ctrl Pts',(-0.791149167492266,0.0207560581004413,
-2.68550140080939));
#58788=CARTESIAN_POINT('Ctrl Pts',(-0.790349974374689,0.0414931362015937,
-2.68633595244249));
#58789=CARTESIAN_POINT('Ctrl Pts',(-0.788720691736706,0.0621647889368653,
-2.68717050407559));
#58790=CARTESIAN_POINT('Ctrl Pts',(-0.778434176683608,0.192675764796195,
-2.69243946584829));
#58791=CARTESIAN_POINT('Ctrl Pts',(-0.735059807397815,0.320578847270327,
-2.69770842762099));
#58792=CARTESIAN_POINT('Ctrl Pts',(-0.663836631886564,0.430425041932617,
-2.70297738939368));
#58793=CARTESIAN_POINT('Ctrl Pts',(-0.592613456375313,0.540271236594907,
-2.70824635116638));
#58794=CARTESIAN_POINT('Ctrl Pts',(-0.493541474638603,0.632060543445355,
-2.71351531293908));
#58795=CARTESIAN_POINT('Ctrl Pts',(-0.378587266872002,0.694706032735847,
-2.71878427471178));
#58796=CARTESIAN_POINT('Ctrl Pts',(-0.263633059105401,0.757351522026339,
-2.72405323648447));
#58797=CARTESIAN_POINT('Ctrl Pts',(-0.132796625308907,0.790853193756876,
-2.72932219825717));
#58798=CARTESIAN_POINT('Ctrl Pts',(-0.00188126980814461,0.791164490723075,
-2.73459116002987));
#58799=CARTESIAN_POINT('Ctrl Pts',(0.129034085692618,0.791475787689273,
-2.73986012180256));
#58800=CARTESIAN_POINT('Ctrl Pts',(0.260028362897649,0.758596709891134,
-2.74512908357526));
#58801=CARTESIAN_POINT('Ctrl Pts',(0.375279192092976,0.69649861345105,-2.75039804534796));
#58802=CARTESIAN_POINT('Ctrl Pts',(0.4905300212883,0.634400517010968,-2.75566700712066));
#58803=CARTESIAN_POINT('Ctrl Pts',(0.590037402473921,0.543083401928943,
-2.76093596889336));
#58804=CARTESIAN_POINT('Ctrl Pts',(0.661782164980846,0.433577163455892,
-2.76620493066605));
#58805=CARTESIAN_POINT('Ctrl Pts',(0.733526927487771,0.324070924982842,
-2.77147389243875));
#58806=CARTESIAN_POINT('Ctrl Pts',(0.777509071316001,0.196375563118767,
-2.77674285421144));
#58807=CARTESIAN_POINT('Ctrl Pts',(0.788416137361891,0.0659149823981434,
-2.78201181598414));
#58808=CARTESIAN_POINT('Ctrl Pts',(0.799323203407781,-0.0645455983224819,
-2.78728077775684));
#58809=CARTESIAN_POINT('Ctrl Pts',(0.77715519167133,-0.197771397899656,
-2.79254973952954));
#58810=CARTESIAN_POINT('Ctrl Pts',(0.72458970368599,-0.317670508340706,
-2.79781870130223));
#58811=CARTESIAN_POINT('Ctrl Pts',(0.67202421570065,-0.437569618781756,
-2.80308766307493));
#58812=CARTESIAN_POINT('Ctrl Pts',(0.589061251466421,-0.544142040086684,
-2.80835662484763));
#58813=CARTESIAN_POINT('Ctrl Pts',(0.485721635714653,-0.624515238529753,
-2.81362558662032));
#58814=CARTESIAN_POINT('Ctrl Pts',(0.382382019962884,-0.704888436972823,
-2.81889454839302));
#58815=CARTESIAN_POINT('Ctrl Pts',(0.258665752693575,-0.759062412554035,
-2.82416351016572));
#58816=CARTESIAN_POINT('Ctrl Pts',(0.129516116637345,-0.780493668192366,
-2.82943247193842));
#58817=CARTESIAN_POINT('Ctrl Pts',(0.000366480581115436,-0.801924923830697,
-2.83470143371112));
#58818=CARTESIAN_POINT('Ctrl Pts',(-0.134216524262036,-0.790613459526147,
-2.83997039548381));
#58819=CARTESIAN_POINT('Ctrl Pts',(-0.257977057520448,-0.747925550005001,
-2.84523935725651));
#58820=CARTESIAN_POINT('Ctrl Pts',(-0.381737590778861,-0.705237640483855,
-2.85050831902921));
#58821=CARTESIAN_POINT('Ctrl Pts',(-0.494675652452535,-0.631173285746112,
-2.8557772808019));
#58822=CARTESIAN_POINT('Ctrl Pts',(-0.583149823964202,-0.534678476626573,
-2.8610462425746));
#58823=CARTESIAN_POINT('Ctrl Pts',(-0.671623995475868,-0.438183667507034,
-2.8663152043473));
#58824=CARTESIAN_POINT('Ctrl Pts',(-0.735634276825528,-0.319258404005699,
-2.87158416611999));
#58825=CARTESIAN_POINT('Ctrl Pts',(-0.767449075774044,-0.192267279199444,
-2.87685312789269));
#58826=CARTESIAN_POINT('Ctrl Pts',(-0.783175891441716,-0.129492530426392,
-2.87945770165389));
#58827=CARTESIAN_POINT('Ctrl Pts',(-0.791035543835318,-0.0647468390521015,
-2.8820622754151));
#58828=CARTESIAN_POINT('Ctrl Pts',(-0.791033587110486,-6.80849259582228E-7,
-2.8846668491763));
#58829=CARTESIAN_POINT('Ctrl Pts',(-0.79103429425828,-3.14382039938683E-6,
-2.91313315082371));
#58830=CARTESIAN_POINT('Ctrl Pts',(-0.791042961814527,-0.0620466816892262,
-2.91063729021779));
#58831=CARTESIAN_POINT('Ctrl Pts',(-0.783831988405732,-0.124088237932048,
-2.90814142961187));
#58832=CARTESIAN_POINT('Ctrl Pts',(-0.769378721885218,-0.184394061429801,
-2.90564556900595));
#58833=CARTESIAN_POINT('Ctrl Pts',(-0.738866717886847,-0.311704488112714,
-2.90037660723325));
#58834=CARTESIAN_POINT('Ctrl Pts',(-0.676078280334516,-0.431279345170175,
-2.89510764546055));
#58835=CARTESIAN_POINT('Ctrl Pts',(-0.588597418956837,-0.528675577247199,
-2.88983868368786));
#58836=CARTESIAN_POINT('Ctrl Pts',(-0.501116557579159,-0.626071809324222,
-2.88456972191516));
#58837=CARTESIAN_POINT('Ctrl Pts',(-0.388943272376134,-0.701289416420807,
-2.87930076014246));
#58838=CARTESIAN_POINT('Ctrl Pts',(-0.265626607079919,-0.745243110126836,
-2.87403179836976));
#58839=CARTESIAN_POINT('Ctrl Pts',(-0.142309941783703,-0.789196803832866,
-2.86876283659707));
#58840=CARTESIAN_POINT('Ctrl Pts',(-0.00784989639429788,-0.801886584148338,
-2.86349387482437));
#58841=CARTESIAN_POINT('Ctrl Pts',(0.121512540586341,-0.781779694070242,
-2.85822491305167));
#58842=CARTESIAN_POINT('Ctrl Pts',(0.25087497756698,-0.761672803992146,
-2.85295595127898));
#58843=CARTESIAN_POINT('Ctrl Pts',(0.375139806138853,-0.708769243520481,
-2.84768698950628));
#58844=CARTESIAN_POINT('Ctrl Pts',(0.479297484648239,-0.629459060456024,
-2.84241802773358));
#58845=CARTESIAN_POINT('Ctrl Pts',(0.583455163157625,-0.550148877391566,
-2.83714906596088));
#58846=CARTESIAN_POINT('Ctrl Pts',(0.667505691604525,-0.444432071734316,
-2.83188010418819));
#58847=CARTESIAN_POINT('Ctrl Pts',(0.721296881938309,-0.325077830198219,
-2.82661114241549));
#58848=CARTESIAN_POINT('Ctrl Pts',(0.775088072272093,-0.205723588662121,
-2.82134218064279));
#58849=CARTESIAN_POINT('Ctrl Pts',(0.798619924492762,-0.0727319112471769,
-2.8160732188701));
#58850=CARTESIAN_POINT('Ctrl Pts',(0.789050103241593,0.0578335729031265,
-2.8108042570974));
#58851=CARTESIAN_POINT('Ctrl Pts',(0.779480281990424,0.18839905705343,-2.8055352953247));
#58852=CARTESIAN_POINT('Ctrl Pts',(0.736808787267417,0.316538347939092,
-2.800266333552));
#58853=CARTESIAN_POINT('Ctrl Pts',(0.666189769163409,0.426773920293066,
-2.79499737177931));
#58854=CARTESIAN_POINT('Ctrl Pts',(0.595570751059401,0.537009492647041,
-2.78972841000661));
#58855=CARTESIAN_POINT('Ctrl Pts',(0.497004209574392,0.629341346469327,
-2.78445944823391));
#58856=CARTESIAN_POINT('Ctrl Pts',(0.382395674431353,0.69261701954002,-2.77919048646121));
#58857=CARTESIAN_POINT('Ctrl Pts',(0.267787139288316,0.755892692610712,
-2.77392152468852));
#58858=CARTESIAN_POINT('Ctrl Pts',(0.137136610487249,0.790112184929811,
-2.76865256291582));
#58859=CARTESIAN_POINT('Ctrl Pts',(0.00622493749824819,0.791142236095035,
-2.76338360114312));
#58860=CARTESIAN_POINT('Ctrl Pts',(-0.124686735490752,0.792172287260259,
-2.75811463937043));
#58861=CARTESIAN_POINT('Ctrl Pts',(-0.255859552667686,0.760012897271608,
-2.75284567759773));
#58862=CARTESIAN_POINT('Ctrl Pts',(-0.371449579060123,0.698548493518071,
-2.74757671582503));
#58863=CARTESIAN_POINT('Ctrl Pts',(-0.487039605452563,0.637084089764534,
-2.74230775405233));
#58864=CARTESIAN_POINT('Ctrl Pts',(-0.587046841060505,0.546314672246109,
-2.73703879227964));
#58865=CARTESIAN_POINT('Ctrl Pts',(-0.6593917394364,0.437203981618818,-2.73176983050694));
#58866=CARTESIAN_POINT('Ctrl Pts',(-0.731736637812292,0.32809329099153,
-2.72650086873424));
#58867=CARTESIAN_POINT('Ctrl Pts',(-0.776419198956139,0.200641327255376,
-2.72123190696154));
#58868=CARTESIAN_POINT('Ctrl Pts',(-0.78804236265073,0.0702425956821335,
-2.71596294518885));
#58869=CARTESIAN_POINT('Ctrl Pts',(-0.790123175060398,0.0468982372964096,
-2.71501968040047));
#58870=CARTESIAN_POINT('Ctrl Pts',(-0.791144460334759,0.0234594373683183,
-2.71407641561209));
#58871=CARTESIAN_POINT('Ctrl Pts',(-0.791121074183877,1.86068176132095E-5,
-2.71313315082371));
#58872=CARTESIAN_POINT('Origin',(0.,0.,-1.97));
#58873=CARTESIAN_POINT('',(-0.791117092312022,-1.90463126063522E-5,-2.4846668491763));
#58874=CARTESIAN_POINT('',(-0.79112535605936,-1.80419918197743E-5,-2.51313315082371));
#58875=CARTESIAN_POINT('',(-0.7911,-9.68818082805471E-17,-1.97));
#58876=CARTESIAN_POINT('Ctrl Pts',(-0.791117092312022,-1.90463126063523E-5,
-2.4846668491763));
#58877=CARTESIAN_POINT('Ctrl Pts',(-0.791009985970769,0.106186545028923,
-2.4889405262037));
#58878=CARTESIAN_POINT('Ctrl Pts',(-0.76947514909813,0.212434259761034,
-2.49321420323109));
#58879=CARTESIAN_POINT('Ctrl Pts',(-0.727852076501281,0.310122790665191,
-2.49748788025849));
#58880=CARTESIAN_POINT('Ctrl Pts',(-0.676535522403009,0.430561731573734,
-2.50275684203119));
#58881=CARTESIAN_POINT('Ctrl Pts',(-0.594684631292216,0.537990619875222,
-2.50802580380389));
#58882=CARTESIAN_POINT('Ctrl Pts',(-0.492185904229906,0.61943347200049,
-2.51329476557658));
#58883=CARTESIAN_POINT('Ctrl Pts',(-0.389687177167596,0.700876324125758,
-2.51856372734928));
#58884=CARTESIAN_POINT('Ctrl Pts',(-0.26654061415377,0.756333140074806,
-2.52383268912198));
#58885=CARTESIAN_POINT('Ctrl Pts',(-0.13762068520791,0.77910547268011,-2.52910165089467));
#58886=CARTESIAN_POINT('Ctrl Pts',(-0.00870075626205005,0.801877805285414,
-2.53437061266737));
#58887=CARTESIAN_POINT('Ctrl Pts',(0.125992538615843,0.791965654546976,
-2.53963957444007));
#58888=CARTESIAN_POINT('Ctrl Pts',(0.250190037482034,0.750566276688429,
-2.54490853621277));
#58889=CARTESIAN_POINT('Ctrl Pts',(0.374387536348225,0.709166898829882,
-2.55017749798546));
#58890=CARTESIAN_POINT('Ctrl Pts',(0.488089239202712,0.636280293851226,
-2.55544645975816));
#58891=CARTESIAN_POINT('Ctrl Pts',(0.577561489751059,0.540710196051203,
-2.56071542153086));
#58892=CARTESIAN_POINT('Ctrl Pts',(0.667033740299406,0.445140098251179,
-2.56598438330356));
#58893=CARTESIAN_POINT('Ctrl Pts',(0.732276538541612,0.326886507629788,
-2.57125334507625));
#58894=CARTESIAN_POINT('Ctrl Pts',(0.765409420559802,0.200232888096587,
-2.57652230684895));
#58895=CARTESIAN_POINT('Ctrl Pts',(0.798542302577993,0.073579268563386,
-2.58179126862165));
#58896=CARTESIAN_POINT('Ctrl Pts',(0.799565268372166,-0.0614743798816252,
-2.58706023039434));
#58897=CARTESIAN_POINT('Ctrl Pts',(0.768354757254441,-0.18861536936756,
-2.59232919216704));
#58898=CARTESIAN_POINT('Ctrl Pts',(0.737144246136717,-0.315756358853493,
-2.59759815393974));
#58899=CARTESIAN_POINT('Ctrl Pts',(0.673700258107094,-0.434984689380349,
-2.60286711571244));
#58900=CARTESIAN_POINT('Ctrl Pts',(0.585685984689295,-0.531899161397838,
-2.60813607748513));
#58901=CARTESIAN_POINT('Ctrl Pts',(0.497671711271496,-0.628813633415326,
-2.61340503925783));
#58902=CARTESIAN_POINT('Ctrl Pts',(0.385087152465521,-0.703414246923448,
-2.61867400103053));
#58903=CARTESIAN_POINT('Ctrl Pts',(0.261531028395032,-0.74669023814687,
-2.62394296280322));
#58904=CARTESIAN_POINT('Ctrl Pts',(0.137974904324542,-0.789966229370293,
-2.62921192457592));
#58905=CARTESIAN_POINT('Ctrl Pts',(0.0034472149895384,-0.801917598309016,
-2.63448088634862));
#58906=CARTESIAN_POINT('Ctrl Pts',(-0.12580288061738,-0.781100778251796,
-2.63974984812132));
#58907=CARTESIAN_POINT('Ctrl Pts',(-0.255052976224298,-0.760283958194577,
-2.64501880989402));
#58908=CARTESIAN_POINT('Ctrl Pts',(-0.379025478103131,-0.706698949141413,
-2.65028777166671));
#58909=CARTESIAN_POINT('Ctrl Pts',(-0.482746153783988,-0.626818108835377,
-2.65555673343941));
#58910=CARTESIAN_POINT('Ctrl Pts',(-0.586466829464846,-0.54693726852934,
-2.6608256952121));
#58911=CARTESIAN_POINT('Ctrl Pts',(-0.669935678947729,-0.44076059697043,
-2.6660946569848));
#58912=CARTESIAN_POINT('Ctrl Pts',(-0.723070773278968,-0.321112826568711,
-2.6713636187575));
#58913=CARTESIAN_POINT('Ctrl Pts',(-0.767789792174107,-0.220416084185967,
-2.6757980288971));
#58914=CARTESIAN_POINT('Ctrl Pts',(-0.79102319560355,-0.110177666260909,
-2.6802324390367));
#58915=CARTESIAN_POINT('Ctrl Pts',(-0.791129214786214,1.74461675192319E-5,
-2.6846668491763));
#58916=CARTESIAN_POINT('Ctrl Pts',(-0.791121074183877,1.86068176132095E-5,
-2.71313315082371));
#58917=CARTESIAN_POINT('Ctrl Pts',(-0.791013828155412,-0.107478175922634,
-2.70880745383939));
#58918=CARTESIAN_POINT('Ctrl Pts',(-0.768936855257277,-0.215017663213923,
-2.70448175685507));
#58919=CARTESIAN_POINT('Ctrl Pts',(-0.726322873854477,-0.313687536405388,
-2.70015605987076));
#58920=CARTESIAN_POINT('Ctrl Pts',(-0.674416455118296,-0.43387343750933,
-2.69488709809806));
#58921=CARTESIAN_POINT('Ctrl Pts',(-0.592039851400596,-0.540899740306881,
-2.68961813632536));
#58922=CARTESIAN_POINT('Ctrl Pts',(-0.48914306286637,-0.621839088213354,
-2.68434917455266));
#58923=CARTESIAN_POINT('Ctrl Pts',(-0.386246274332143,-0.702778436119827,
-2.67908021277997));
#58924=CARTESIAN_POINT('Ctrl Pts',(-0.26282930098139,-0.757630829135223,
-2.67381125100727));
#58925=CARTESIAN_POINT('Ctrl Pts',(-0.133799274812547,-0.779770826358582,
-2.66854228923457));
#58926=CARTESIAN_POINT('Ctrl Pts',(-0.00476924864370518,-0.801910823581941,
-2.66327332746188));
#58927=CARTESIAN_POINT('Ctrl Pts',(0.129873830343226,-0.791338425013262,
-2.65800436568918));
#58928=CARTESIAN_POINT('Ctrl Pts',(0.253866865617512,-0.749330636049166,
-2.65273540391648));
#58929=CARTESIAN_POINT('Ctrl Pts',(0.377859900891799,-0.707322847085071,
-2.64746644214378));
#58930=CARTESIAN_POINT('Ctrl Pts',(0.491202892453441,-0.633879667725558,
-2.64219748037109));
#58931=CARTESIAN_POINT('Ctrl Pts',(0.58020551157022,-0.537872059065953,
-2.63692851859839));
#58932=CARTESIAN_POINT('Ctrl Pts',(0.669208130686999,-0.441864450406348,
-2.63165955682569));
#58933=CARTESIAN_POINT('Ctrl Pts',(0.733870377358915,-0.323292412446649,
-2.62639059505299));
#58934=CARTESIAN_POINT('Ctrl Pts',(0.766381910590859,-0.196477873307437,
-2.6211216332803));
#58935=CARTESIAN_POINT('Ctrl Pts',(0.798893443822801,-0.0696633341682291,
-2.6158526715076));
#58936=CARTESIAN_POINT('Ctrl Pts',(0.799254263614774,0.0653937061504918,
-2.6105837097349));
#58937=CARTESIAN_POINT('Ctrl Pts',(0.767420787725851,0.192380150084523,
-2.60531474796221));
#58938=CARTESIAN_POINT('Ctrl Pts',(0.735587311836928,0.319366594018558,
-2.60004578618951));
#58939=CARTESIAN_POINT('Ctrl Pts',(0.671559540267108,0.438282441567903,
-2.59477682441681));
#58940=CARTESIAN_POINT('Ctrl Pts',(0.583071177841939,0.534764236977682,
-2.58950786264412));
#58941=CARTESIAN_POINT('Ctrl Pts',(0.494582815416771,0.631246032387461,
-2.58423890087142));
#58942=CARTESIAN_POINT('Ctrl Pts',(0.381633862136254,0.705293775657674,
-2.57896993909872));
#58943=CARTESIAN_POINT('Ctrl Pts',(0.257867052139174,0.747963482398279,
-2.57370097732602));
#58944=CARTESIAN_POINT('Ctrl Pts',(0.134100242142095,0.790633189138884,
-2.56843201555332));
#58945=CARTESIAN_POINT('Ctrl Pts',(-0.000484424571547404,0.801924859349881,
-2.56316305378063));
#58946=CARTESIAN_POINT('Ctrl Pts',(-0.129630906898198,0.780474609168716,
-2.55789409200793));
#58947=CARTESIAN_POINT('Ctrl Pts',(-0.258777389224849,0.759024358987551,
-2.55262513023523));
#58948=CARTESIAN_POINT('Ctrl Pts',(-0.382485687164508,0.704832188414225,
-2.54735616846254));
#58949=CARTESIAN_POINT('Ctrl Pts',(-0.485813480575784,0.624443792243266,
-2.54208720668984));
#58950=CARTESIAN_POINT('Ctrl Pts',(-0.58914127398706,0.544055396072307,
-2.53681824491714));
#58951=CARTESIAN_POINT('Ctrl Pts',(-0.672088562869954,0.437470774303715,
-2.53154928314444));
#58952=CARTESIAN_POINT('Ctrl Pts',(-0.724636415867464,0.317563934317272,
-2.52628032137175));
#58953=CARTESIAN_POINT('Ctrl Pts',(-0.768342406730885,0.21783298521156,
-2.52189793118907));
#58954=CARTESIAN_POINT('Ctrl Pts',(-0.791018482792984,0.10888590738746,
-2.51751554100639));
#58955=CARTESIAN_POINT('Ctrl Pts',(-0.79112535605936,-1.80419918197743E-5,
-2.51313315082371));
#58956=CARTESIAN_POINT('Origin',(0.,0.,-1.97));
#58957=CARTESIAN_POINT('',(-0.791034957252612,4.30828170744357E-6,-2.2846668491763));
#58958=CARTESIAN_POINT('',(-0.791033810580254,1.8628665638589E-6,-2.31313315082371));
#58959=CARTESIAN_POINT('',(-0.7911,-9.68818082805471E-17,-1.97));
#58960=CARTESIAN_POINT('Ctrl Pts',(-0.791034957252612,4.30828170744357E-6,
-2.2846668491763));
#58961=CARTESIAN_POINT('Ctrl Pts',(-0.791046599626097,0.0607545590049239,
-2.2871106898253));
#58962=CARTESIAN_POINT('Ctrl Pts',(-0.784135866741558,0.12150220338301,
-2.2895545304743));
#58963=CARTESIAN_POINT('Ctrl Pts',(-0.770273514124328,0.180619777421388,
-2.2919983711233));
#58964=CARTESIAN_POINT('Ctrl Pts',(-0.740386047423214,0.30807826692241,
-2.297267332896));
#58965=CARTESIAN_POINT('Ctrl Pts',(-0.678184609475154,0.427959522898974,
-2.30253629466869));
#58966=CARTESIAN_POINT('Ctrl Pts',(-0.591182308249092,0.525783481074166,
-2.30780525644139));
#58967=CARTESIAN_POINT('Ctrl Pts',(-0.504180007023029,0.623607439249358,
-2.31307421821409));
#58968=CARTESIAN_POINT('Ctrl Pts',(-0.392376842518966,0.699374099623178,
-2.31834317998679));
#58969=CARTESIAN_POINT('Ctrl Pts',(-0.26927715280204,0.743931855438399,
-2.32361214175948));
#58970=CARTESIAN_POINT('Ctrl Pts',(-0.146177463085118,0.788489611253618,
-2.32888110353218));
#58971=CARTESIAN_POINT('Ctrl Pts',(-0.0117812481553361,0.80183846251024,
-2.33415006530488));
#58972=CARTESIAN_POINT('Ctrl Pts',(0.117678213357513,0.782366045184846,
-2.33941902707757));
#58973=CARTESIAN_POINT('Ctrl Pts',(0.247137674870368,0.76289362785945,-2.34468798885027));
#58974=CARTESIAN_POINT('Ctrl Pts',(0.371660382966294,0.710599941952033,
-2.34995695062297));
#58975=CARTESIAN_POINT('Ctrl Pts',(0.476205647568452,0.631801370512207,
-2.35522591239567));
#58976=CARTESIAN_POINT('Ctrl Pts',(0.580750912170611,0.553002799072381,
-2.36049487416836));
#58977=CARTESIAN_POINT('Ctrl Pts',(0.665318733279004,0.44769934210015,-2.36576383594106));
#58978=CARTESIAN_POINT('Ctrl Pts',(0.719694440756652,0.328610259275577,
-2.37103279771376));
#58979=CARTESIAN_POINT('Ctrl Pts',(0.774070148234299,0.209521176451008,
-2.37630175948645));
#58980=CARTESIAN_POINT('Ctrl Pts',(0.7982537420812,0.0766464677740978,-2.38157072125915));
#58981=CARTESIAN_POINT('Ctrl Pts',(0.789324165202169,-0.0539643658824301,
-2.38683968303185));
#58982=CARTESIAN_POINT('Ctrl Pts',(0.780394588323137,-0.18457519953896,
-2.39210864480455));
#58983=CARTESIAN_POINT('Ctrl Pts',(0.738351840718173,-0.312922158175111,
-2.39737760657724));
#58984=CARTESIAN_POINT('Ctrl Pts',(0.668274128172985,-0.423502633016406,
-2.40264656834994));
#58985=CARTESIAN_POINT('Ctrl Pts',(0.598196415627797,-0.534083107857701,
-2.40791553012264));
#58986=CARTESIAN_POINT('Ctrl Pts',(0.500083738142384,-0.626897098904138,
-2.41318449189533));
#58987=CARTESIAN_POINT('Ctrl Pts',(0.385786804693692,-0.690733908159592,
-2.41845345366803));
#58988=CARTESIAN_POINT('Ctrl Pts',(0.271489871244999,-0.754570717415047,
-2.42372241544073));
#58989=CARTESIAN_POINT('Ctrl Pts',(0.141008681833027,-0.789430344879519,
-2.42899137721343));
#58990=CARTESIAN_POINT('Ctrl Pts',(0.0101036319776801,-0.791102210323073,
-2.43426033898612));
#58991=CARTESIAN_POINT('Ctrl Pts',(-0.120801417877665,-0.792774075766627,
-2.43952930075882));
#58992=CARTESIAN_POINT('Ctrl Pts',(-0.252130328176385,-0.761258179189264,
-2.44479826253152));
#58993=CARTESIAN_POINT('Ctrl Pts',(-0.368020309969101,-0.70036122251838,
-2.45006722430422));
#58994=CARTESIAN_POINT('Ctrl Pts',(-0.483910291761818,-0.639464265847496,
-2.45533618607691));
#58995=CARTESIAN_POINT('Ctrl Pts',(-0.58436134504853,-0.549186249083092,
-2.46060514784961));
#58996=CARTESIAN_POINT('Ctrl Pts',(-0.657240316097855,-0.440431558193533,
-2.46587410962231));
#58997=CARTESIAN_POINT('Ctrl Pts',(-0.730119287147181,-0.331676867303971,
-2.471143071395));
#58998=CARTESIAN_POINT('Ctrl Pts',(-0.775426175959118,-0.204445502289255,
-2.4764120331677));
#58999=CARTESIAN_POINT('Ctrl Pts',(-0.78768851182221,-0.0741053230240971,
-2.4816809949404));
#59000=CARTESIAN_POINT('Ctrl Pts',(-0.790004815555806,-0.0494846106867235,
-2.4826762796857));
#59001=CARTESIAN_POINT('Ctrl Pts',(-0.791142036009661,-0.0247529708113624,
-2.483671564431));
#59002=CARTESIAN_POINT('Ctrl Pts',(-0.791117092312022,-1.90463126063523E-5,
-2.4846668491763));
#59003=CARTESIAN_POINT('Ctrl Pts',(-0.79112535605936,-1.80419918197743E-5,
-2.51313315082371));
#59004=CARTESIAN_POINT('Ctrl Pts',(-0.791146976863933,-0.0220496602493374,
-2.51224657923369));
#59005=CARTESIAN_POINT('Ctrl Pts',(-0.790244917210455,-0.0440795134067749,
-2.51136000764367));
#59006=CARTESIAN_POINT('Ctrl Pts',(-0.78840643244089,-0.0660309387040414,
-2.51047343605365));
#59007=CARTESIAN_POINT('Ctrl Pts',(-0.777480178904677,-0.196489913534617,
-2.50520447428096));
#59008=CARTESIAN_POINT('Ctrl Pts',(-0.733479254720125,-0.324178804991475,
-2.49993551250826));
#59009=CARTESIAN_POINT('Ctrl Pts',(-0.66171838740861,-0.433674490079434,
-2.49466655073556));
#59010=CARTESIAN_POINT('Ctrl Pts',(-0.589957520097096,-0.543170175167392,
-2.48939758896287));
#59011=CARTESIAN_POINT('Ctrl Pts',(-0.49043670965862,-0.634472653886452,
-2.48412862719017));
#59012=CARTESIAN_POINT('Ctrl Pts',(-0.375176748837641,-0.69655379886404,
-2.47885966541747));
#59013=CARTESIAN_POINT('Ctrl Pts',(-0.259916788016662,-0.758634943841629,
-2.47359070364477));
#59014=CARTESIAN_POINT('Ctrl Pts',(-0.128917676813181,-0.791494755077747,
-2.46832174187208));
#59015=CARTESIAN_POINT('Ctrl Pts',(0.00199763117598858,-0.791164203594926,
-2.46305278009938));
#59016=CARTESIAN_POINT('Ctrl Pts',(0.13291293916516,-0.790833652112105,
-2.45778381832668));
#59017=CARTESIAN_POINT('Ctrl Pts',(0.26374444394002,-0.757312737910344,
-2.45251485655398));
#59018=CARTESIAN_POINT('Ctrl Pts',(0.378689436535325,-0.694650342429101,
-2.44724589478129));
#59019=CARTESIAN_POINT('Ctrl Pts',(0.49363442913063,-0.631987946947858,
-2.44197693300859));
#59020=CARTESIAN_POINT('Ctrl Pts',(0.59269290954638,-0.540184070187133,
-2.43670797123589));
#59021=CARTESIAN_POINT('Ctrl Pts',(0.663899928367349,-0.430327401746784,
-2.4314390094632));
#59022=CARTESIAN_POINT('Ctrl Pts',(0.735106947188317,-0.320470733306435,
-2.4261700476905));
#59023=CARTESIAN_POINT('Ctrl Pts',(0.778462504414503,-0.192561273186463,
-2.4209010859178));
#59024=CARTESIAN_POINT('Ctrl Pts',(0.788729824285738,-0.0620487861484625,
-2.4156321241451));
#59025=CARTESIAN_POINT('Ctrl Pts',(0.798997144156974,0.0684637008895377,
-2.41036316237241));
#59026=CARTESIAN_POINT('Ctrl Pts',(0.776176226673258,0.201579214845565,
-2.40509420059971));
#59027=CARTESIAN_POINT('Ctrl Pts',(0.723023535714875,0.321219168765922,
-2.39982523882701));
#59028=CARTESIAN_POINT('Ctrl Pts',(0.669870844756492,0.440859122686279,
-2.39455627705432));
#59029=CARTESIAN_POINT('Ctrl Pts',(0.586386380323441,0.547023516570965,
-2.38928731528162));
#59030=CARTESIAN_POINT('Ctrl Pts',(0.48265395744808,0.626889100989973,-2.38401835350892));
#59031=CARTESIAN_POINT('Ctrl Pts',(0.378921534572719,0.706754685408981,
-2.37874939173623));
#59032=CARTESIAN_POINT('Ctrl Pts',(0.254941153255048,0.760321460362311,
-2.37348042996353));
#59033=CARTESIAN_POINT('Ctrl Pts',(0.125687997696566,0.781119270544093,
-2.36821146819083));
#59034=CARTESIAN_POINT('Ctrl Pts',(-0.00356515786191522,0.801917080725876,
-2.36294250641813));
#59035=CARTESIAN_POINT('Ctrl Pts',(-0.138091087661207,0.78994592613611,
-2.35767354464544));
#59036=CARTESIAN_POINT('Ctrl Pts',(-0.261640845237265,0.746651763330027,
-2.35240458287274));
#59037=CARTESIAN_POINT('Ctrl Pts',(-0.385190602813323,0.703357600523944,
-2.34713562110004));
#59038=CARTESIAN_POINT('Ctrl Pts',(-0.497764188166149,0.628740429501544,
-2.34186665932734));
#59039=CARTESIAN_POINT('Ctrl Pts',(-0.585764206619544,0.531813013966079,
-2.33659769755465));
#59040=CARTESIAN_POINT('Ctrl Pts',(-0.673764225072938,0.434885598430616,
-2.33132873578195));
#59041=CARTESIAN_POINT('Ctrl Pts',(-0.737190676626901,0.315647938382089,
-2.32605977400925));
#59042=CARTESIAN_POINT('Ctrl Pts',(-0.768382487931173,0.188502360253156,
-2.32079081223656));
#59043=CARTESIAN_POINT('Ctrl Pts',(-0.783493392136204,0.126906557673506,
-2.31823825843227));
#59044=CARTESIAN_POINT('Ctrl Pts',(-0.79103905925902,0.0634548238769548,
-2.31568570462799));
#59045=CARTESIAN_POINT('Ctrl Pts',(-0.791033810580254,1.8628665638589E-6,
-2.31313315082371));
#59046=CARTESIAN_POINT('Origin',(0.,0.,-1.97));
#59047=CARTESIAN_POINT('',(-0.791144406175107,1.41356307707188E-5,-2.0846668491763));
#59048=CARTESIAN_POINT('',(-0.791137191533222,1.59212896634344E-5,-2.11313315082371));
#59049=CARTESIAN_POINT('',(-0.7911,-9.68818082805471E-17,-1.97));
#59050=CARTESIAN_POINT('Ctrl Pts',(-0.791144406175107,1.41356307707188E-5,
-2.0846668491763));
#59051=CARTESIAN_POINT('Ctrl Pts',(-0.791157104778467,0.0152712971938506,
-2.0852808534469));
#59052=CARTESIAN_POINT('Ctrl Pts',(-0.790724724866188,0.0305277394974985,
-2.0858948577175));
#59053=CARTESIAN_POINT('Ctrl Pts',(-0.78984238020639,0.0457581138935725,
-2.08650886198811));
#59054=CARTESIAN_POINT('Ctrl Pts',(-0.782270706025277,0.176454697482384,
-2.0917778237608));
#59055=CARTESIAN_POINT('Ctrl Pts',(-0.741564121327834,0.305231668946985,
-2.0970467855335));
#59056=CARTESIAN_POINT('Ctrl Pts',(-0.672639441158341,0.416534479671716,
-2.1023157473062));
#59057=CARTESIAN_POINT('Ctrl Pts',(-0.60371476098885,0.527837290396444,
-2.1075847090789));
#59058=CARTESIAN_POINT('Ctrl Pts',(-0.50657198534731,0.621665940381303,
-2.11285367085159));
#59059=CARTESIAN_POINT('Ctrl Pts',(-0.392944671943546,0.686687174300185,
-2.11812263262429));
#59060=CARTESIAN_POINT('Ctrl Pts',(-0.279317358539779,0.751708408219068,
-2.12339159439699));
#59061=CARTESIAN_POINT('Ctrl Pts',(-0.149205507373787,0.787922226071974,
-2.12866055616968));
#59062=CARTESIAN_POINT('Ctrl Pts',(-0.0183249028083912,0.790954479407162,
-2.13392951794238));
#59063=CARTESIAN_POINT('Ctrl Pts',(0.112555701757004,0.793986732742351,
-2.13919847971508));
#59064=CARTESIAN_POINT('Ctrl Pts',(0.244205059721803,0.763837421559821,
-2.14446744148778));
#59065=CARTESIAN_POINT('Ctrl Pts',(0.360721676312565,0.70414818241294,-2.14973640326047));
#59066=CARTESIAN_POINT('Ctrl Pts',(0.47723829290333,0.644458943266057,-2.15500536503317));
#59067=CARTESIAN_POINT('Ctrl Pts',(0.578622168120057,0.555229776154819,
-2.16027432680587));
#59068=CARTESIAN_POINT('Ctrl Pts',(0.65262747572559,0.447238379933159,-2.16554328857856));
#59069=CARTESIAN_POINT('Ctrl Pts',(0.726632783331119,0.339246983711505,
-2.17081225035126));
#59070=CARTESIAN_POINT('Ctrl Pts',(0.773259523325458,0.212493358379431,
-2.17608121212396));
#59071=CARTESIAN_POINT('Ctrl Pts',(0.78687580449558,0.0822876592000658,
-2.18135017389666));
#59072=CARTESIAN_POINT('Ctrl Pts',(0.800492085665702,-0.0479180399793047,
-2.18661913566935));
#59073=CARTESIAN_POINT('Ctrl Pts',(0.781097908011607,-0.181575813005962,
-2.19188809744205));
#59074=CARTESIAN_POINT('Ctrl Pts',(0.73103583073274,-0.302541575229069,
-2.19715705921475));
#59075=CARTESIAN_POINT('Ctrl Pts',(0.680973753453872,-0.423507337452174,
-2.20242602098744));
#59076=CARTESIAN_POINT('Ctrl Pts',(0.600243776550234,-0.531781088871725,
-2.20769498276014));
#59077=CARTESIAN_POINT('Ctrl Pts',(0.498597009526942,-0.614284797669602,
-2.21296394453284));
#59078=CARTESIAN_POINT('Ctrl Pts',(0.39695024250365,-0.696788506467478,
-2.21823290630554));
#59079=CARTESIAN_POINT('Ctrl Pts',(0.274386685360704,-0.753522172643679,
-2.22350186807823));
#59080=CARTESIAN_POINT('Ctrl Pts',(0.145710388747892,-0.777633122473658,
-2.22877082985093));
#59081=CARTESIAN_POINT('Ctrl Pts',(0.0170340921350798,-0.801744072303636,
-2.23403979162363));
#59082=CARTESIAN_POINT('Ctrl Pts',(-0.117754943947599,-0.793232305787391,
-2.23930875339633));
#59083=CARTESIAN_POINT('Ctrl Pts',(-0.242375993289851,-0.753125931324868,
-2.24457771516902));
#59084=CARTESIAN_POINT('Ctrl Pts',(-0.3669970426321,-0.713019556862346,
-2.24984667694172));
#59085=CARTESIAN_POINT('Ctrl Pts',(-0.481450105233923,-0.641318574453546,
-2.25511563871442));
#59086=CARTESIAN_POINT('Ctrl Pts',(-0.571910770517838,-0.546683510930122,
-2.26038460048711));
#59087=CARTESIAN_POINT('Ctrl Pts',(-0.662371435801757,-0.452048447406696,
-2.26565356225981));
#59088=CARTESIAN_POINT('Ctrl Pts',(-0.728839703767767,-0.334479302768643,
-2.27092252403251));
#59089=CARTESIAN_POINT('Ctrl Pts',(-0.763287090023688,-0.208176868936877,
-2.27619148580521));
#59090=CARTESIAN_POINT('Ctrl Pts',(-0.781757149736784,-0.140455809421626,
-2.2790166069289));
#59091=CARTESIAN_POINT('Ctrl Pts',(-0.791021498471951,-0.0702240090425869,
-2.2818417280526));
#59092=CARTESIAN_POINT('Ctrl Pts',(-0.791034957252612,4.30828170744357E-6,
-2.2846668491763));
#59093=CARTESIAN_POINT('Ctrl Pts',(-0.791033810580254,1.8628665638589E-6,
-2.31313315082371));
#59094=CARTESIAN_POINT('Ctrl Pts',(-0.791028224977005,-0.0675242862860532,
-2.31041674285529));
#59095=CARTESIAN_POINT('Ctrl Pts',(-0.782471188428489,-0.13505182526465,
-2.30770033488688));
#59096=CARTESIAN_POINT('Ctrl Pts',(-0.765379960987778,-0.200345458892024,
-2.30498392691846));
#59097=CARTESIAN_POINT('Ctrl Pts',(-0.732228451685532,-0.326994203698933,
-2.29971496514576));
#59098=CARTESIAN_POINT('Ctrl Pts',(-0.66696826202646,-0.445238197103409,
-2.29444600337307));
#59099=CARTESIAN_POINT('Ctrl Pts',(-0.577481956580721,-0.540795134412294,
-2.28917704160037));
#59100=CARTESIAN_POINT('Ctrl Pts',(-0.487995651134981,-0.636352071721179,
-2.28390807982767));
#59101=CARTESIAN_POINT('Ctrl Pts',(-0.374283229902573,-0.709221952934474,
-2.27863911805498));
#59102=CARTESIAN_POINT('Ctrl Pts',(-0.2500796438157,-0.75060306376228,-2.27337015628228));
#59103=CARTESIAN_POINT('Ctrl Pts',(-0.125876057728828,-0.791984174590086,
-2.26810119450958));
#59104=CARTESIAN_POINT('Ctrl Pts',(0.00881869321251119,-0.801876515032405,
-2.26283223273689));
#59105=CARTESIAN_POINT('Ctrl Pts',(0.137735271191444,-0.779085221686388,
-2.25756327096419));
#59106=CARTESIAN_POINT('Ctrl Pts',(0.266651849170376,-0.756293928340371,
-2.25229430919149));
#59107=CARTESIAN_POINT('Ctrl Pts',(0.389790254186903,-0.700819001206018,
-2.24702534741879));
#59108=CARTESIAN_POINT('Ctrl Pts',(0.492277001599317,-0.619361075041607,
-2.2417563856461));
#59109=CARTESIAN_POINT('Ctrl Pts',(0.59476374901173,-0.537903148877196,
-2.2364874238734));
#59110=CARTESIAN_POINT('Ctrl Pts',(0.676598838820031,-0.430462223682727,
-2.2312184621007));
#59111=CARTESIAN_POINT('Ctrl Pts',(0.727897678550787,-0.310015736924248,
-2.225949500328));
#59112=CARTESIAN_POINT('Ctrl Pts',(0.779196518281544,-0.189569250165767,
-2.22068053855531));
#59113=CARTESIAN_POINT('Ctrl Pts',(0.799959107934757,-0.0561172018432798,
-2.21541157678261));
#59114=CARTESIAN_POINT('Ctrl Pts',(0.7876776023074,0.074221172205609,-2.21014261500991));
#59115=CARTESIAN_POINT('Ctrl Pts',(0.775396096680042,0.204559546254496,
-2.20487365323722));
#59116=CARTESIAN_POINT('Ctrl Pts',(0.730070495772115,0.331784246029781,
-2.19960469146452));
#59117=CARTESIAN_POINT('Ctrl Pts',(0.657175530467858,0.440528216729188,
-2.19433572969182));
#59118=CARTESIAN_POINT('Ctrl Pts',(0.584280565163601,0.549272187428595,
-2.18906676791912));
#59119=CARTESIAN_POINT('Ctrl Pts',(0.483816235463015,0.639535429052127,
-2.18379780614643));
#59120=CARTESIAN_POINT('Ctrl Pts',(0.367917298712036,0.70041534027229,-2.17852884437373));
#59121=CARTESIAN_POINT('Ctrl Pts',(0.25201836196106,0.761295251492451,-2.17325988260103));
#59122=CARTESIAN_POINT('Ctrl Pts',(0.120684818159691,0.792791832309247,
-2.16799092082833));
#59123=CARTESIAN_POINT('Ctrl Pts',(-0.0102199840770827,0.791100713882735,
-2.16272195905564));
#59124=CARTESIAN_POINT('Ctrl Pts',(-0.14112478631386,0.789409595456224,
-2.15745299728294));
#59125=CARTESIAN_POINT('Ctrl Pts',(-0.271600846986045,0.754530777786403,
-2.15218403551024));
#59126=CARTESIAN_POINT('Ctrl Pts',(-0.385888390057411,0.690677159025263,
-2.14691507373755));
#59127=CARTESIAN_POINT('Ctrl Pts',(-0.500175933128777,0.626823540264123,
-2.14164611196485));
#59128=CARTESIAN_POINT('Ctrl Pts',(-0.598274958599326,0.533995120411663,
-2.13637715019215));
#59129=CARTESIAN_POINT('Ctrl Pts',(-0.668336406474275,0.42340434027223,
-2.13110818841946));
#59130=CARTESIAN_POINT('Ctrl Pts',(-0.738397854349223,0.312813560132798,
-2.12583922664676));
#59131=CARTESIAN_POINT('Ctrl Pts',(-0.780421724628571,0.184460419706392,
-2.12057026487406));
#59132=CARTESIAN_POINT('Ctrl Pts',(-0.789332091656947,0.0538482744456927,
-2.11530130310136));
#59133=CARTESIAN_POINT('Ctrl Pts',(-0.790554282631232,0.0359328524926724,
-2.11457858567548));
#59134=CARTESIAN_POINT('Ctrl Pts',(-0.791153467809793,0.0179749290533651,
-2.11385586824959));
#59135=CARTESIAN_POINT('Ctrl Pts',(-0.791137191533222,1.59212896634344E-5,
-2.11313315082371));
#59136=CARTESIAN_POINT('Origin',(0.,0.,-1.97));
#59137=CARTESIAN_POINT('',(-0.791099975804956,-2.00585267497999E-5,-1.8846668491763));
#59138=CARTESIAN_POINT('',(-0.791108422200728,-1.97323857704162E-5,-1.91313315082371));
#59139=CARTESIAN_POINT('',(-0.7911,-9.68818082805471E-17,-1.97));
#59140=CARTESIAN_POINT('Ctrl Pts',(-0.791099975804956,-2.00585267497999E-5,
-1.8846668491763));
#59141=CARTESIAN_POINT('Ctrl Pts',(-0.79099794526589,0.100710966905559,
-1.8887199788412));
#59142=CARTESIAN_POINT('Ctrl Pts',(-0.77168153183872,0.201480004270866,
-1.8927731085061));
#59143=CARTESIAN_POINT('Ctrl Pts',(-0.734140622488718,0.294927680913593,
-1.89682623817101));
#59144=CARTESIAN_POINT('Ctrl Pts',(-0.685338429459896,0.416407198393984,
-1.9020951999437));
#59145=CARTESIAN_POINT('Ctrl Pts',(-0.60573808677214,0.525514117795622,
-1.9073641617164));
#59146=CARTESIAN_POINT('Ctrl Pts',(-0.504954259113385,0.609069771668604,
-1.9126331234891));
#59147=CARTESIAN_POINT('Ctrl Pts',(-0.404170431454624,0.692625425541591,
-1.91790208526179));
#59148=CARTESIAN_POINT('Ctrl Pts',(-0.282203118824861,0.750629813885918,
-1.92317104703449));
#59149=CARTESIAN_POINT('Ctrl Pts',(-0.153784353451944,0.776076776608192,
-1.92844000880719));
#59150=CARTESIAN_POINT('Ctrl Pts',(-0.0253655880790338,0.801523739330464,
-1.93370897057989));
#59151=CARTESIAN_POINT('Ctrl Pts',(0.10950463003703,0.794413276430685,-1.93897793235258));
#59152=CARTESIAN_POINT('Ctrl Pts',(0.234535768974027,0.755604237434488,
-1.94424689412528));
#59153=CARTESIAN_POINT('Ctrl Pts',(0.359566907911032,0.716795198438288,
-1.94951585589798));
#59154=CARTESIAN_POINT('Ctrl Pts',(0.47475896766897,0.646287583345665,-1.95478481767068));
#59155=CARTESIAN_POINT('Ctrl Pts',(0.56619827662422,0.552597776058642,-1.96005377944337));
#59156=CARTESIAN_POINT('Ctrl Pts',(0.657637585579464,0.458907968771624,
-1.96532274121607));
#59157=CARTESIAN_POINT('Ctrl Pts',(0.725324143732022,0.342035969290208,
-1.97059170298877));
#59158=CARTESIAN_POINT('Ctrl Pts',(0.761082313408198,0.216098363655112,
-1.97586066476146));
#59159=CARTESIAN_POINT('Ctrl Pts',(0.796840483084376,0.0901607580200119,
-1.98112962653416));
#59160=CARTESIAN_POINT('Ctrl Pts',(0.800670264284169,-0.0448424537687684,
-1.98639858830686));
#59161=CARTESIAN_POINT('Ctrl Pts',(0.772109070279671,-0.172604675918861,
-1.99166755007956));
#59162=CARTESIAN_POINT('Ctrl Pts',(0.743547876275173,-0.300366898068953,
-1.99693651185225));
#59163=CARTESIAN_POINT('Ctrl Pts',(0.682595707066384,-0.420888130580358,
-2.00220547362495));
#59164=CARTESIAN_POINT('Ctrl Pts',(0.596614775542808,-0.519611008506553,
-2.00747443539765));
#59165=CARTESIAN_POINT('Ctrl Pts',(0.510633844019231,-0.618333886432751,
-2.01274339717035));
#59166=CARTESIAN_POINT('Ctrl Pts',(0.399624150180865,-0.695258409773738,
-2.01801235894304));
#59167=CARTESIAN_POINT('Ctrl Pts',(0.276994191369901,-0.741093117296691,
-2.02328132071574));
#59168=CARTESIAN_POINT('Ctrl Pts',(0.154364232558945,-0.78692782481964,
-2.02855028248844));
#59169=CARTESIAN_POINT('Ctrl Pts',(0.0201140087753928,-0.80167271652456,
-2.03381924426113));
#59170=CARTESIAN_POINT('Ctrl Pts',(-0.109540835143368,-0.783546805234561,
-2.03908820603383));
#59171=CARTESIAN_POINT('Ctrl Pts',(-0.239195679062133,-0.765420893944561,
-2.04435716780653));
#59172=CARTESIAN_POINT('Ctrl Pts',(-0.364255143116106,-0.71442417965964,
-2.04962612957922));
#59173=CARTESIAN_POINT('Ctrl Pts',(-0.469613704234257,-0.636716388474941,
-2.05489509135192));
#59174=CARTESIAN_POINT('Ctrl Pts',(-0.574972265352409,-0.559008597290241,
-2.06016405312462));
#59175=CARTESIAN_POINT('Ctrl Pts',(-0.66062992353474,-0.454589729205763,
-2.06543301489732));
#59176=CARTESIAN_POINT('Ctrl Pts',(-0.716240370793513,-0.336072197307012,
-2.07070197667002));
#59177=CARTESIAN_POINT('Ctrl Pts',(-0.765370404342706,-0.231365786814431,
-2.07535693417211));
#59178=CARTESIAN_POINT('Ctrl Pts',(-0.791048134110227,-0.115655155413321,
-2.0800118916742));
#59179=CARTESIAN_POINT('Ctrl Pts',(-0.791144406175107,1.41356307707188E-5,
-2.0846668491763));
#59180=CARTESIAN_POINT('Ctrl Pts',(-0.791137191533222,1.59212896634344E-5,
-2.11313315082371));
#59181=CARTESIAN_POINT('Ctrl Pts',(-0.791034805832124,-0.112954977979898,
-2.10858690647689));
#59182=CARTESIAN_POINT('Ctrl Pts',(-0.766578473242961,-0.225968784207304,
-2.10404066213008));
#59183=CARTESIAN_POINT('Ctrl Pts',(-0.719646100543896,-0.328716104796029,
-2.09949441778327));
#59184=CARTESIAN_POINT('Ctrl Pts',(-0.665252878625066,-0.447797188682058,
-2.09422545601057));
#59185=CARTESIAN_POINT('Ctrl Pts',(-0.580669571010003,-0.553088206359121,
-2.08895649423788));
#59186=CARTESIAN_POINT('Ctrl Pts',(-0.476112718400113,-0.631871400648869,
-2.08368753246518));
#59187=CARTESIAN_POINT('Ctrl Pts',(-0.371555865790223,-0.710654594938617,
-2.07841857069248));
#59188=CARTESIAN_POINT('Ctrl Pts',(-0.247025468185505,-0.762929965841049,
-2.07314960891978));
#59189=CARTESIAN_POINT('Ctrl Pts',(-0.117563144453371,-0.782383342516024,
-2.06788064714709));
#59190=CARTESIAN_POINT('Ctrl Pts',(0.0118991792787638,-0.801836719190998,
-2.06261168537439));
#59191=CARTESIAN_POINT('Ctrl Pts',(0.146293429138315,-0.788468101638515,
-2.05734272360169));
#59192=CARTESIAN_POINT('Ctrl Pts',(0.269386563849886,-0.743892241388133,
-2.052073761829));
#59193=CARTESIAN_POINT('Ctrl Pts',(0.392479698561456,-0.699316381137751,
-2.0468048000563));
#59194=CARTESIAN_POINT('Ctrl Pts',(0.504271718125046,-0.623533278189469,
-2.0415358382836));
#59195=CARTESIAN_POINT('Ctrl Pts',(0.591259630636372,-0.525696525345232,
-2.0362668765109));
#59196=CARTESIAN_POINT('Ctrl Pts',(0.678247543147696,-0.427859772500998,
-2.03099791473821));
#59197=CARTESIAN_POINT('Ctrl Pts',(0.740431348606757,-0.307969369760809,
-2.02572895296551));
#59198=CARTESIAN_POINT('Ctrl Pts',(0.77030006881521,-0.180506486209202,
-2.02045999119281));
#59199=CARTESIAN_POINT('Ctrl Pts',(0.800168789023663,-0.0530436026575909,
-2.01519102942012));
#59200=CARTESIAN_POINT('Ctrl Pts',(0.797722423981506,0.0819917617054397,
-2.00992206764742));
#59201=CARTESIAN_POINT('Ctrl Pts',(0.7632564621099,0.208289127483382,-2.00465310587472));
#59202=CARTESIAN_POINT('Ctrl Pts',(0.728790500238293,0.334586493261325,
-1.99938414410202));
#59203=CARTESIAN_POINT('Ctrl Pts',(0.662304941537236,0.452145860454179,
-1.99411518232933));
#59204=CARTESIAN_POINT('Ctrl Pts',(0.571830358890167,0.546767618126615,
-1.98884622055663));
#59205=CARTESIAN_POINT('Ctrl Pts',(0.481355776243099,0.641389375799051,
-1.98357725878393));
#59206=CARTESIAN_POINT('Ctrl Pts',(0.366892169650018,0.713073523951068,
-1.97830829701123));
#59207=CARTESIAN_POINT('Ctrl Pts',(0.242265223262576,0.753161569105755,
-1.97303933523854));
#59208=CARTESIAN_POINT('Ctrl Pts',(0.117638276875135,0.793249614260442,
-1.96777037346584));
#59209=CARTESIAN_POINT('Ctrl Pts',(-0.0171520093066676,0.8017415564178,
-1.96250141169314));
#59210=CARTESIAN_POINT('Ctrl Pts',(-0.145824758077158,0.777611681697264,
-1.95723244992045));
#59211=CARTESIAN_POINT('Ctrl Pts',(-0.274497506847648,0.753481806976729,
-1.95196348814775));
#59212=CARTESIAN_POINT('Ctrl Pts',(-0.397052718206826,0.696730115378302,
-1.94669452637505));
#59213=CARTESIAN_POINT('Ctrl Pts',(-0.498687349564794,0.614211457858244,
-1.94142556460235));
#59214=CARTESIAN_POINT('Ctrl Pts',(-0.600321980922761,0.531692800338187,
-1.93615660282966));
#59215=CARTESIAN_POINT('Ctrl Pts',(-0.681036032279518,0.4234071768965,-1.93088764105696));
#59216=CARTESIAN_POINT('Ctrl Pts',(-0.731080317724594,0.302434053333974,
-1.92561867928426));
#59217=CARTESIAN_POINT('Ctrl Pts',(-0.770609253225731,0.206879910515361,
-1.92145683646408));
#59218=CARTESIAN_POINT('Ctrl Pts',(-0.791003045630741,0.103409922135896,
-1.91729499364389));
#59219=CARTESIAN_POINT('Ctrl Pts',(-0.791108422200728,-1.97323857704162E-5,
-1.91313315082371));
#59220=CARTESIAN_POINT('Origin',(0.,0.,-1.97));
#59221=CARTESIAN_POINT('',(-0.791040023293942,9.038082159879E-6,-1.6846668491763));
#59222=CARTESIAN_POINT('',(-0.791037072492376,6.75761974000038E-6,-1.7131331508237));
#59223=CARTESIAN_POINT('',(-0.7911,-9.68818082805471E-17,-1.97));
#59224=CARTESIAN_POINT('Ctrl Pts',(-0.791040023293942,9.038082159879E-6,
-1.6846668491763));
#59225=CARTESIAN_POINT('Ctrl Pts',(-0.791062421323145,0.0552757956668374,
-1.6868901424628));
#59226=CARTESIAN_POINT('Ctrl Pts',(-0.785351984343387,0.110537990535984,
-1.68911343574931));
#59227=CARTESIAN_POINT('Ctrl Pts',(-0.773861227453778,0.164570930607212,
-1.69133672903581));
#59228=CARTESIAN_POINT('Ctrl Pts',(-0.746629391169211,0.292623085232824,
-1.69660569080851));
#59229=CARTESIAN_POINT('Ctrl Pts',(-0.686933074418255,0.413771276237449,
-1.70187465258121));
#59230=CARTESIAN_POINT('Ctrl Pts',(-0.601982799785173,0.513382410411572,
-1.7071436143539));
#59231=CARTESIAN_POINT('Ctrl Pts',(-0.517032525152087,0.612993544585701,
-1.7124125761266));
#59232=CARTESIAN_POINT('Ctrl Pts',(-0.406828292636872,0.691067621929326,
-1.7176815378993));
#59233=CARTESIAN_POINT('Ctrl Pts',(-0.284681310546525,0.738174330346637,
-1.722950499672));
#59234=CARTESIAN_POINT('Ctrl Pts',(-0.162534328456181,0.785281038763947,
-1.72821946144469));
#59235=CARTESIAN_POINT('Ctrl Pts',(-0.0284445967907067,0.801420378254945,
-1.73348842321739));
#59236=CARTESIAN_POINT('Ctrl Pts',(0.101391624929814,0.784642930861729,
-1.73875738499009));
#59237=CARTESIAN_POINT('Ctrl Pts',(0.231227846650335,0.767865483468514,
-1.74402634676279));
#59238=CARTESIAN_POINT('Ctrl Pts',(0.356810558425899,0.718171249191085,
-1.74929530853548));
#59239=CARTESIAN_POINT('Ctrl Pts',(0.462971035806919,0.641562631830331,
-1.75456427030818));
#59240=CARTESIAN_POINT('Ctrl Pts',(0.569131513187935,0.56495401446958,-1.75983323208088));
#59241=CARTESIAN_POINT('Ctrl Pts',(0.655869756174406,0.461431014025508,
-1.76510219385357));
#59242=CARTESIAN_POINT('Ctrl Pts',(0.712708936479214,0.343497834665462,
-1.77037115562627));
#59243=CARTESIAN_POINT('Ctrl Pts',(0.769548116784024,0.225564655305408,
-1.77564011739897));
#59244=CARTESIAN_POINT('Ctrl Pts',(0.796488234407167,0.0932212970293808,
-1.78090907917167));
#59245=CARTESIAN_POINT('Ctrl Pts',(0.790275280774633,-0.0375469193645623,
-1.78617804094436));
#59246=CARTESIAN_POINT('Ctrl Pts',(0.784062327142098,-0.168315135758502,
-1.79144700271706));
#59247=CARTESIAN_POINT('Ctrl Pts',(0.744696302253884,-0.297508210270366,
-1.79671596448976));
#59248=CARTESIAN_POINT('Ctrl Pts',(0.676932099325491,-0.40952133456021,
-1.80198492626246));
#59249=CARTESIAN_POINT('Ctrl Pts',(0.609167896397101,-0.52153445885005,
-1.80725388803515));
#59250=CARTESIAN_POINT('Ctrl Pts',(0.513005515428532,-0.61636763291788,
-1.81252284980785));
#59251=CARTESIAN_POINT('Ctrl Pts',(0.400060095468028,-0.682566268263607,
-1.81779181158055));
#59252=CARTESIAN_POINT('Ctrl Pts',(0.287114675507523,-0.748764903609333,
-1.82306077335325));
#59253=CARTESIAN_POINT('Ctrl Pts',(0.157386216555084,-0.786329000232956,
-1.82832973512594));
#59254=CARTESIAN_POINT('Ctrl Pts',(0.0265441942837325,-0.790721313932425,
-1.83359869689864));
#59255=CARTESIAN_POINT('Ctrl Pts',(-0.104297827987626,-0.795113627631893,
-1.83886765867134));
#59256=CARTESIAN_POINT('Ctrl Pts',(-0.236253413577895,-0.766334158407205,
-1.84413662044403));
#59257=CARTESIAN_POINT('Ctrl Pts',(-0.353384079481705,-0.707859084088112,
-1.84940558221673));
#59258=CARTESIAN_POINT('Ctrl Pts',(-0.470514745385511,-0.649384009769022,
-1.85467454398943));
#59259=CARTESIAN_POINT('Ctrl Pts',(-0.572820491602857,-0.561213330355531,
-1.85994350576213));
#59260=CARTESIAN_POINT('Ctrl Pts',(-0.647944142117717,-0.453996893439293,
-1.86521246753482));
#59261=CARTESIAN_POINT('Ctrl Pts',(-0.723067792632574,-0.346780456523059,
-1.87048142930752));
#59262=CARTESIAN_POINT('Ctrl Pts',(-0.771009347444945,-0.22051826210408,
-1.87575039108022));
#59263=CARTESIAN_POINT('Ctrl Pts',(-0.785978103166188,-0.0904611071150179,
-1.88101935285291));
#59264=CARTESIAN_POINT('Ctrl Pts',(-0.789432198034349,-0.0604499452000733,
-1.88223518496071));
#59265=CARTESIAN_POINT('Ctrl Pts',(-0.79113058227838,-0.0302367120999488,
-1.8834510170685));
#59266=CARTESIAN_POINT('Ctrl Pts',(-0.791099975804956,-2.00585267497999E-5,
-1.8846668491763));
#59267=CARTESIAN_POINT('Ctrl Pts',(-0.791108422200728,-1.97323857704162E-5,
-1.91313315082371));
#59268=CARTESIAN_POINT('Ctrl Pts',(-0.791136454109385,-0.027533729362611,
-1.91202603187119));
#59269=CARTESIAN_POINT('Ctrl Pts',(-0.789728780531539,-0.0550448721224735,
-1.91091891291868));
#59270=CARTESIAN_POINT('Ctrl Pts',(-0.786863691565349,-0.0824033887437885,
-1.90981179396617));
#59271=CARTESIAN_POINT('Ctrl Pts',(-0.773228260427633,-0.21260708357566,
-1.90454283219347));
#59272=CARTESIAN_POINT('Ctrl Pts',(-0.726582878618806,-0.339353849556038,
-1.89927387042078));
#59273=CARTESIAN_POINT('Ctrl Pts',(-0.65256168903561,-0.447334359940417,
-1.89400490864808));
#59274=CARTESIAN_POINT('Ctrl Pts',(-0.578540499452414,-0.555314870324795,
-1.88873594687538));
#59275=CARTESIAN_POINT('Ctrl Pts',(-0.477143502094848,-0.644529125113175,
-1.88346698510268));
#59276=CARTESIAN_POINT('Ctrl Pts',(-0.360618108180484,-0.704201226662264,
-1.87819802332999));
#59277=CARTESIAN_POINT('Ctrl Pts',(-0.24409271426612,-0.763873328211353,
-1.87292906155729));
#59278=CARTESIAN_POINT('Ctrl Pts',(-0.112438923794957,-0.794003276521151,
-1.86766009978459));
#59279=CARTESIAN_POINT('Ctrl Pts',(0.0184412330716377,-0.790951773816272,
-1.86239113801189));
#59280=CARTESIAN_POINT('Ctrl Pts',(0.149321389938229,-0.787900271111393,
-1.8571221762392));
#59281=CARTESIAN_POINT('Ctrl Pts',(0.279427913200253,-0.751667317391838,
-1.8518532144665));
#59282=CARTESIAN_POINT('Ctrl Pts',(0.393045662034959,-0.686629372468008,
-1.8465842526938));
#59283=CARTESIAN_POINT('Ctrl Pts',(0.506663410869671,-0.621591427544173,
-1.84131529092111));
#59284=CARTESIAN_POINT('Ctrl Pts',(0.603792385277063,-0.52774849141606,
-1.83604632914841));
#59285=CARTESIAN_POINT('Ctrl Pts',(0.67270069455318,-0.416435544986229,
-1.83077736737571));
#59286=CARTESIAN_POINT('Ctrl Pts',(0.741609003829294,-0.305122598556405,
-1.82550840560301));
#59287=CARTESIAN_POINT('Ctrl Pts',(0.782296647974136,-0.176339641824865,
-1.82023944383032));
#59288=CARTESIAN_POINT('Ctrl Pts',(0.789849099710743,-0.04564194634806,
-1.81497048205762));
#59289=CARTESIAN_POINT('Ctrl Pts',(0.797401551447349,0.085055749128749,
-1.80970152028492));
#59290=CARTESIAN_POINT('Ctrl Pts',(0.771818810775718,0.217668183350823,
-1.80443255851223));
#59291=CARTESIAN_POINT('Ctrl Pts',(0.716190933153538,0.336177534717853,
-1.79916359673953));
#59292=CARTESIAN_POINT('Ctrl Pts',(0.660563055531358,0.454686886084884,
-1.79389463496683));
#59293=CARTESIAN_POINT('Ctrl Pts',(0.574890040958628,0.559093154596869,
-1.78862567319413));
#59294=CARTESIAN_POINT('Ctrl Pts',(0.469520052271186,0.636785449029398,
-1.78335671142144));
#59295=CARTESIAN_POINT('Ctrl Pts',(0.364150063583744,0.714477743461927,
-1.77808774964874));
#59296=CARTESIAN_POINT('Ctrl Pts',(0.239083100781589,0.765456063814999,
-1.77281878787604));
#59297=CARTESIAN_POINT('Ctrl Pts',(0.109425592684985,0.783562905736258,
-1.76754982610334));
#59298=CARTESIAN_POINT('Ctrl Pts',(-0.020231915411619,0.801669747657518,
-1.76228086433065));
#59299=CARTESIAN_POINT('Ctrl Pts',(-0.154479968802673,0.786905111146965,
-1.75701190255795));
#59300=CARTESIAN_POINT('Ctrl Pts',(-0.277103184805389,0.74105236829189,
-1.75174294078525));
#59301=CARTESIAN_POINT('Ctrl Pts',(-0.399726400808106,0.695199625436816,
-1.74647397901256));
#59302=CARTESIAN_POINT('Ctrl Pts',(-0.510724779422485,0.61825877623722,
-1.74120501723986));
#59303=CARTESIAN_POINT('Ctrl Pts',(-0.596691190035183,0.519523253872919,
-1.73593605546716));
#59304=CARTESIAN_POINT('Ctrl Pts',(-0.682657600647882,0.420787731508618,
-1.73066709369446));
#59305=CARTESIAN_POINT('Ctrl Pts',(-0.743592043258899,0.300257535979611,
-1.72539813192177));
#59306=CARTESIAN_POINT('Ctrl Pts',(-0.772134446116417,0.17249111484596,
-1.72012917014907));
#59307=CARTESIAN_POINT('Ctrl Pts',(-0.784767118395946,0.115942570752923,
-1.71779716370728));
#59308=CARTESIAN_POINT('Ctrl Pts',(-0.791054555941974,0.057976531794004,
-1.71546515726549));
#59309=CARTESIAN_POINT('Ctrl Pts',(-0.791037072492376,6.75761974000038E-6,
-1.7131331508237));
#59310=CARTESIAN_POINT('Origin',(0.,0.,-1.97));
#59311=CARTESIAN_POINT('',(-0.791156699774446,9.7028961639975E-6,-1.4846668491763));
#59312=CARTESIAN_POINT('',(-0.79115108988969,1.20126448708321E-5,-1.5131331508237));
#59313=CARTESIAN_POINT('',(-0.7911,-9.68818082805471E-17,-1.97));
#59314=CARTESIAN_POINT('Ctrl Pts',(-0.791156699774446,9.7028961639975E-6,
-1.4846668491763));
#59315=CARTESIAN_POINT('Ctrl Pts',(-0.791162742476985,0.00978612533273453,
-1.4850603060844));
#59316=CARTESIAN_POINT('Ctrl Pts',(-0.790985257298765,0.0195623280860764,
-1.48545376299251));
#59317=CARTESIAN_POINT('Ctrl Pts',(-0.790622820147353,0.0293316692235354,
-1.48584721990062));
#59318=CARTESIAN_POINT('Ctrl Pts',(-0.785769258152526,0.160157393558066,
-1.49111618167332));
#59319=CARTESIAN_POINT('Ctrl Pts',(-0.747748045175354,0.289752616390813,
-1.49638514344602));
#59320=CARTESIAN_POINT('Ctrl Pts',(-0.681151639005095,0.402463955203277,
-1.50165410521871));
#59321=CARTESIAN_POINT('Ctrl Pts',(-0.614555232834838,0.515175294015737,
-1.50692306699141));
#59322=CARTESIAN_POINT('Ctrl Pts',(-0.519383633471496,0.611002748807917,
-1.51219202876411));
#59323=CARTESIAN_POINT('Ctrl Pts',(-0.407132306698205,0.678371635167473,
-1.5174609905368));
#59324=CARTESIAN_POINT('Ctrl Pts',(-0.294880979924907,0.745740521527034,
-1.5227299523095));
#59325=CARTESIAN_POINT('Ctrl Pts',(-0.165549925741656,0.784650839453969,
-1.5279989140822));
#59326=CARTESIAN_POINT('Ctrl Pts',(-0.0347606186009809,0.790402739084114,
-1.5332678758549));
#59327=CARTESIAN_POINT('Ctrl Pts',(0.0960286885396864,0.796154638714258,
-1.53853683762759));
#59328=CARTESIAN_POINT('Ctrl Pts',(0.22827624863778,0.768748120047617,-1.54380579940029));
#59329=CARTESIAN_POINT('Ctrl Pts',(0.346008312043396,0.711493526712698,
-1.54907476117299));
#59330=CARTESIAN_POINT('Ctrl Pts',(0.463740375449019,0.654238933377775,
-1.55434372294569));
#59331=CARTESIAN_POINT('Ctrl Pts',(0.566956942162166,0.567136265374568,
-1.55961268471838));
#59332=CARTESIAN_POINT('Ctrl Pts',(0.643190821142216,0.460706368694415,
-1.56488164649108));
#59333=CARTESIAN_POINT('Ctrl Pts',(0.719424700122262,0.354276472014268,
-1.57015060826378));
#59334=CARTESIAN_POINT('Ctrl Pts',(0.768675891369217,0.228519346657175,
-1.57541957003647));
#59335=CARTESIAN_POINT('Ctrl Pts',(0.784995504798797,0.0986247839180053,
-1.58068853180917));
#59336=CARTESIAN_POINT('Ctrl Pts',(0.801315118228378,-0.0312697788211682,
-1.58595749358187));
#59337=CARTESIAN_POINT('Ctrl Pts',(0.784703153840584,-0.16530177894241,
-1.59122645535457));
#59338=CARTESIAN_POINT('Ctrl Pts',(0.737166116406668,-0.2872819301298,-1.59649541712726));
#59339=CARTESIAN_POINT('Ctrl Pts',(0.689629078972751,-0.409262081317194,
-1.60176437889996));
#59340=CARTESIAN_POINT('Ctrl Pts',(0.611166968492709,-0.519190383570726,
-1.60703334067266));
#59341=CARTESIAN_POINT('Ctrl Pts',(0.511256966314024,-0.603788957295985,
-1.61230230244535));
#59342=CARTESIAN_POINT('Ctrl Pts',(0.411346964135345,-0.68838753102124,
-1.61757126421805));
#59343=CARTESIAN_POINT('Ctrl Pts',(0.289989070258022,-0.747656376218227,
-1.62284022599075));
#59344=CARTESIAN_POINT('Ctrl Pts',(0.161841707214753,-0.77443660319164,
-1.62810918776345));
#59345=CARTESIAN_POINT('Ctrl Pts',(0.0336943441714761,-0.801216830165056,
-1.63337814953614));
#59346=CARTESIAN_POINT('Ctrl Pts',(-0.101242488037751,-0.795508438914895,
-1.63864711130884));
#59347=CARTESIAN_POINT('Ctrl Pts',(-0.226670211392565,-0.758000927324264,
-1.64391607308154));
#59348=CARTESIAN_POINT('Ctrl Pts',(-0.352097934747372,-0.720493415733635,
-1.64918503485424));
#59349=CARTESIAN_POINT('Ctrl Pts',(-0.468016549247768,-0.651186783802539,
-1.65445399662693));
#59350=CARTESIAN_POINT('Ctrl Pts',(-0.560424625102388,-0.558452352610354,
-1.65972295839963));
#59351=CARTESIAN_POINT('Ctrl Pts',(-0.65283270095701,-0.465717921418167,
-1.66499192017233));
#59352=CARTESIAN_POINT('Ctrl Pts',(-0.721730238165856,-0.349555690964889,
-1.67026088194502));
#59353=CARTESIAN_POINT('Ctrl Pts',(-0.75879532886119,-0.223996516614949,
-1.67552984371772));
#59354=CARTESIAN_POINT('Ctrl Pts',(-0.780220418573089,-0.151418343349124,
-1.67857551220391));
#59355=CARTESIAN_POINT('Ctrl Pts',(-0.791009340445165,-0.0757003714371634,
-1.6816211806901));
#59356=CARTESIAN_POINT('Ctrl Pts',(-0.791040023293942,9.038082159879E-6,
-1.6846668491763));
#59357=CARTESIAN_POINT('Ctrl Pts',(-0.791037072492376,6.75761974000038E-6,
-1.7131331508237));
#59358=CARTESIAN_POINT('Ctrl Pts',(-0.79101505363789,-0.0730010326855647,
-1.7101961954928));
#59359=CARTESIAN_POINT('Ctrl Pts',(-0.780992693074769,-0.146014747479032,
-1.70725924016189));
#59360=CARTESIAN_POINT('Ctrl Pts',(-0.7610505204609,-0.216210297827144,
-1.70432228483098));
#59361=CARTESIAN_POINT('Ctrl Pts',(-0.725273828843842,-0.342142642628313,
-1.69905332305828));
#59362=CARTESIAN_POINT('Ctrl Pts',(-0.657570082505703,-0.459004685492353,
-1.69378436128558));
#59363=CARTESIAN_POINT('Ctrl Pts',(-0.566116995224823,-0.552681043005752,
-1.68851539951289));
#59364=CARTESIAN_POINT('Ctrl Pts',(-0.474663907943943,-0.646357400519152,
-1.68324643774019));
#59365=CARTESIAN_POINT('Ctrl Pts',(-0.359461479720322,-0.71684807268191,
-1.67797747596749));
#59366=CARTESIAN_POINT('Ctrl Pts',(-0.234424634550591,-0.75563872207301,
-1.6727085141948));
#59367=CARTESIAN_POINT('Ctrl Pts',(-0.10938778938086,-0.79442937146411,
-1.6674395524221));
#59368=CARTESIAN_POINT('Ctrl Pts',(0.0254834727349791,-0.801519998083552,
-1.6621705906494));
#59369=CARTESIAN_POINT('Ctrl Pts',(0.153898493773395,-0.776054148365041,
-1.6569016288767));
#59370=CARTESIAN_POINT('Ctrl Pts',(0.282313514811811,-0.75058829864653,
-1.65163266710401));
#59371=CARTESIAN_POINT('Ctrl Pts',(0.404272294772801,-0.692565972590067,
-1.64636370533131));
#59372=CARTESIAN_POINT('Ctrl Pts',(0.505043832061636,-0.608995496926544,
-1.64109474355861));
#59373=CARTESIAN_POINT('Ctrl Pts',(0.605815369350467,-0.525425021263023,
-1.63582578178591));
#59374=CARTESIAN_POINT('Ctrl Pts',(0.685399663967143,-0.416306395992444,
-1.63055682001322));
#59375=CARTESIAN_POINT('Ctrl Pts',(0.734183989617675,-0.29481970247828,
-1.62528785824052));
#59376=CARTESIAN_POINT('Ctrl Pts',(0.78296831526821,-0.173333008964113,
-1.62001889646782));
#59377=CARTESIAN_POINT('Ctrl Pts',(0.800952671952598,-0.0394782472063504,
-1.61474993469513));
#59378=CARTESIAN_POINT('Ctrl Pts',(0.785964788128907,0.0905767045204875,
-1.60948097292243));
#59379=CARTESIAN_POINT('Ctrl Pts',(0.770976904305216,0.220631656247329,
-1.60421201114973));
#59380=CARTESIAN_POINT('Ctrl Pts',(0.723016779973445,0.346886797943254,
-1.59894304937703));
#59381=CARTESIAN_POINT('Ctrl Pts',(0.647877361473669,0.454092184550919,
-1.59367408760433));
#59382=CARTESIAN_POINT('Ctrl Pts',(0.572737942973897,0.561297571158579,
-1.58840512583164));
#59383=CARTESIAN_POINT('Ctrl Pts',(0.470419230306124,0.649453202677979,
-1.58313616405894));
#59384=CARTESIAN_POINT('Ctrl Pts',(0.353279965661455,0.707911049103311,
-1.57786720228624));
#59385=CARTESIAN_POINT('Ctrl Pts',(0.236140701016785,0.766368895528643,
-1.57259824051355));
#59386=CARTESIAN_POINT('Ctrl Pts',(0.104180884395221,0.795128956859905,
-1.56732927874085));
#59387=CARTESIAN_POINT('Ctrl Pts',(-0.0266604901454559,0.790717399483225,
-1.56206031696815));
#59388=CARTESIAN_POINT('Ctrl Pts',(-0.157501864686137,0.786305842106544,
-1.55679135519546));
#59389=CARTESIAN_POINT('Ctrl Pts',(-0.287224797145929,0.74872266602192,
-1.55152239342276));
#59390=CARTESIAN_POINT('Ctrl Pts',(-0.400160479378758,0.682507419977008,
-1.54625343165006));
#59391=CARTESIAN_POINT('Ctrl Pts',(-0.513096161611586,0.616292173932096,
-1.54098446987736));
#59392=CARTESIAN_POINT('Ctrl Pts',(-0.609244593617448,0.521444857926898,
-1.53571550810467));
#59393=CARTESIAN_POINT('Ctrl Pts',(-0.67699232119762,0.409421768619803,
-1.53044654633197));
#59394=CARTESIAN_POINT('Ctrl Pts',(-0.744740048777793,0.297398679312709,
-1.52517758455927));
#59395=CARTESIAN_POINT('Ctrl Pts',(-0.784087071932273,0.168199816703719,
-1.51990862278657));
#59396=CARTESIAN_POINT('Ctrl Pts',(-0.790280792602754,0.0374306882580553,
-1.51463966101388));
#59397=CARTESIAN_POINT('Ctrl Pts',(-0.790871098859641,0.0249674470439252,
-1.51413749095049));
#59398=CARTESIAN_POINT('Ctrl Pts',(-0.791160258257041,0.0124899423751816,
-1.5136353208871));
#59399=CARTESIAN_POINT('Ctrl Pts',(-0.79115108988969,1.20126448708321E-5,
-1.5131331508237));
#59400=CARTESIAN_POINT('Origin',(0.,0.,-1.97));
#59401=CARTESIAN_POINT('',(-0.79108328723417,-1.97011904900513E-5,-1.2846668491763));
#59402=CARTESIAN_POINT('',(-0.791091395193699,-2.00455443718572E-5,-1.3131331508237));
#59403=CARTESIAN_POINT('',(-0.7911,-9.68818082805471E-17,-1.97));
#59404=CARTESIAN_POINT('Ctrl Pts',(-0.79108328723417,-1.97011904900513E-5,
-1.2846668491763));
#59405=CARTESIAN_POINT('Ctrl Pts',(-0.790992127656328,0.0952359163469633,
-1.2884994314787));
#59406=CARTESIAN_POINT('Ctrl Pts',(-0.773765886393891,0.190523615754407,
-1.29233201378111));
#59407=CARTESIAN_POINT('Ctrl Pts',(-0.74011198568934,0.27960514872973,-1.29616459608352));
#59408=CARTESIAN_POINT('Ctrl Pts',(-0.693845238540031,0.402072757998116,
-1.30143355785622));
#59409=CARTESIAN_POINT('Ctrl Pts',(-0.61652983531396,0.512810569252064,
-1.30670251962891));
#59410=CARTESIAN_POINT('Ctrl Pts',(-0.51750445034507,0.59844292495629,-1.31197148140161));
#59411=CARTESIAN_POINT('Ctrl Pts',(-0.418479065376179,0.684075280660516,
-1.31724044317431));
#59412=CARTESIAN_POINT('Ctrl Pts',(-0.297743698664468,0.744602180815023,
-1.32250940494701));
#59413=CARTESIAN_POINT('Ctrl Pts',(-0.169881579725185,0.772712779386538,
-1.32777836671971));
#59414=CARTESIAN_POINT('Ctrl Pts',(-0.0420194607859029,0.800823377958053,
-1.3330473284924));
#59415=CARTESIAN_POINT('Ctrl Pts',(0.0929694103809409,0.796517674946579,
-1.3383162902651));
#59416=CARTESIAN_POINT('Ctrl Pts',(0.218780170139753,0.760315742116927,
-1.34358525203779));
#59417=CARTESIAN_POINT('Ctrl Pts',(0.344590929898565,0.724113809287274,
-1.34885421381049));
#59418=CARTESIAN_POINT('Ctrl Pts',(0.461223578249343,0.656015646639435,
-1.35412317558319));
#59419=CARTESIAN_POINT('Ctrl Pts',(0.554590439590504,0.564246608206026,
-1.35939213735589));
#59420=CARTESIAN_POINT('Ctrl Pts',(0.647957300931661,0.472477569772619,
-1.36466109912858));
#59421=CARTESIAN_POINT('Ctrl Pts',(0.718058375263214,0.357037655553636,
-1.36993006090128));
#59422=CARTESIAN_POINT('Ctrl Pts',(0.756426383410174,0.231870474701282,
-1.37519902267398));
#59423=CARTESIAN_POINT('Ctrl Pts',(0.794794391557134,0.106703293848925,
-1.38046798444668));
#59424=CARTESIAN_POINT('Ctrl Pts',(0.801429333519501,-0.0281911536367966,
-1.38573694621937));
#59425=CARTESIAN_POINT('Ctrl Pts',(0.775529796388259,-0.156519409247474,
-1.39100590799207));
#59426=CARTESIAN_POINT('Ctrl Pts',(0.749630259257016,-0.284847664858156,
-1.39627486976477));
#59427=CARTESIAN_POINT('Ctrl Pts',(0.691196243032161,-0.406609728593785,
-1.40154383153746));
#59428=CARTESIAN_POINT('Ctrl Pts',(0.60728580115167,-0.507098359568208,
-1.40681279331016));
#59429=CARTESIAN_POINT('Ctrl Pts',(0.523375359271181,-0.607586990542628,
-1.41208175508286));
#59430=CARTESIAN_POINT('Ctrl Pts',(0.413988491735055,-0.686802188755845,
-1.41735071685556));
#59431=CARTESIAN_POINT('Ctrl Pts',(0.292337680011484,-0.735175809859585,
-1.42261967862825));
#59432=CARTESIAN_POINT('Ctrl Pts',(0.170686868287912,-0.783549430963325,
-1.42788864040095));
#59433=CARTESIAN_POINT('Ctrl Pts',(0.0367721123768919,-0.801081474957589,
-1.43315760217365));
#59434=CARTESIAN_POINT('Ctrl Pts',(-0.0932314629497926,-0.78565430366888,
-1.43842656394635));
#59435=CARTESIAN_POINT('Ctrl Pts',(-0.223235038276477,-0.770227132380172,
-1.44369552571904));
#59436=CARTESIAN_POINT('Ctrl Pts',(-0.349327433018828,-0.721840745808492,
-1.44896448749174));
#59437=CARTESIAN_POINT('Ctrl Pts',(-0.456278359790997,-0.646339577113788,
-1.45423344926444));
#59438=CARTESIAN_POINT('Ctrl Pts',(-0.563229286563166,-0.570838408419083,
-1.45950241103713));
#59439=CARTESIAN_POINT('Ctrl Pts',(-0.651038745365154,-0.468222457601353,
-1.46477137280983));
#59440=CARTESIAN_POINT('Ctrl Pts',(-0.709100519259907,-0.350886369274331,
-1.47004033458253));
#59441=CARTESIAN_POINT('Ctrl Pts',(-0.762826561179094,-0.242312290715897,
-1.47491583944712));
#59442=CARTESIAN_POINT('Ctrl Pts',(-0.791081821877995,-0.121134427923465,
-1.47979134431171));
#59443=CARTESIAN_POINT('Ctrl Pts',(-0.791156699774446,9.7028961639975E-6,
-1.4846668491763));
#59444=CARTESIAN_POINT('Ctrl Pts',(-0.79115108988969,1.20126448708321E-5,
-1.5131331508237));
#59445=CARTESIAN_POINT('Ctrl Pts',(-0.791064060214553,-0.118433303641197,
-1.5083663591144));
#59446=CARTESIAN_POINT('Ctrl Pts',(-0.764096094533504,-0.23691692026043,
-1.50359956740509));
#59447=CARTESIAN_POINT('Ctrl Pts',(-0.712658406752002,-0.343602652588724,
-1.49883277569579));
#59448=CARTESIAN_POINT('Ctrl Pts',(-0.655801882044296,-0.461527470707488,
-1.49356381392309));
#59449=CARTESIAN_POINT('Ctrl Pts',(-0.569048414442406,-0.565037712662681,
-1.48829485215039));
#59450=CARTESIAN_POINT('Ctrl Pts',(-0.462876671164885,-0.641630715343042,
-1.48302589037769));
#59451=CARTESIAN_POINT('Ctrl Pts',(-0.356704927887362,-0.718223718023404,
-1.477756928605));
#59452=CARTESIAN_POINT('Ctrl Pts',(-0.231114908934207,-0.767899481428933,
-1.4724879668323));
#59453=CARTESIAN_POINT('Ctrl Pts',(-0.101276221365059,-0.784657832794859,
-1.4672190050596));
#59454=CARTESIAN_POINT('Ctrl Pts',(0.0285624662040879,-0.801416184160784,
-1.46195004328691));
#59455=CARTESIAN_POINT('Ctrl Pts',(0.162649822389227,-0.785257123487106,
-1.45668108151421));
#59456=CARTESIAN_POINT('Ctrl Pts',(0.284789874596762,-0.738132450788793,
-1.45141211974151));
#59457=CARTESIAN_POINT('Ctrl Pts',(0.406929926804297,-0.691007778090479,
-1.44614315796881));
#59458=CARTESIAN_POINT('Ctrl Pts',(0.517122675034227,-0.612917493367531,
-1.44087419619612));
#59459=CARTESIAN_POINT('Ctrl Pts',(0.602058298128763,-0.513293866352021,
-1.43560523442342));
#59460=CARTESIAN_POINT('Ctrl Pts',(0.686993921223296,-0.413670239336515,
-1.43033627265072));
#59461=CARTESIAN_POINT('Ctrl Pts',(0.746672419182438,-0.292513270028449,
-1.42506731087802));
#59462=CARTESIAN_POINT('Ctrl Pts',(0.773885421695427,-0.164457111939861,
-1.41979834910533));
#59463=CARTESIAN_POINT('Ctrl Pts',(0.801098424208418,-0.0364009538512651,
-1.41452938733263));
#59464=CARTESIAN_POINT('Ctrl Pts',(0.795845931275253,0.0985543930178537,
-1.40926042555993));
#59465=CARTESIAN_POINT('Ctrl Pts',(0.758762374314478,0.224108114322004,
-1.40399146378723));
#59466=CARTESIAN_POINT('Ctrl Pts',(0.721678817353705,0.349661835626148,
-1.39872250201454));
#59467=CARTESIAN_POINT('Ctrl Pts',(0.652764196365327,0.465813931365325,
-1.39345354024184));
#59468=CARTESIAN_POINT('Ctrl Pts',(0.560342482710852,0.558534770314031,
-1.38818457846914));
#59469=CARTESIAN_POINT('Ctrl Pts',(0.467920769056375,0.651255609262739,
-1.38291561669645));
#59470=CARTESIAN_POINT('Ctrl Pts',(0.351991962735802,0.720545191420975,
-1.37764665492375));
#59471=CARTESIAN_POINT('Ctrl Pts',(0.226558724577076,0.758034255095584,
-1.37237769315105));
#59472=CARTESIAN_POINT('Ctrl Pts',(0.101125486418351,0.795523318770194,
-1.36710873137835));
#59473=CARTESIAN_POINT('Ctrl Pts',(-0.0338121835785264,0.801211863961177,
-1.36183976960566));
#59474=CARTESIAN_POINT('Ctrl Pts',(-0.161955606199568,0.774412789925915,
-1.35657080783296));
#59475=CARTESIAN_POINT('Ctrl Pts',(-0.29009902882061,0.747613715890653,
-1.35130184606026));
#59476=CARTESIAN_POINT('Ctrl Pts',(-0.411448204065817,0.688327022629146,
-1.34603288428757));
#59477=CARTESIAN_POINT('Ctrl Pts',(-0.511345762497513,0.603713755645957,
-1.34076392251487));
#59478=CARTESIAN_POINT('Ctrl Pts',(-0.611243320929208,0.519100488662768,
-1.33549496074217));
#59479=CARTESIAN_POINT('Ctrl Pts',(-0.689689262547392,0.409160647957897,
-1.33022599896947));
#59480=CARTESIAN_POINT('Ctrl Pts',(-0.737208358988454,0.287173506817499,
-1.32495703719678));
#59481=CARTESIAN_POINT('Ctrl Pts',(-0.77275365368526,0.195924531020277,
-1.32101574173909));
#59482=CARTESIAN_POINT('Ctrl Pts',(-0.790994270862107,0.0979346591559362,
-1.3170744462814));
#59483=CARTESIAN_POINT('Ctrl Pts',(-0.791091395193699,-2.00455443718572E-5,
-1.3131331508237));
#59484=CARTESIAN_POINT('Origin',(0.,0.,-1.97));
#59485=CARTESIAN_POINT('',(-0.791048562900586,1.32194889376214E-5,-1.0846668491763));
#59486=CARTESIAN_POINT('',(-0.791043937878947,1.12442601377988E-5,-1.1131331508237));
#59487=CARTESIAN_POINT('',(-0.7911,-9.68818082805471E-17,-1.97));
#59488=CARTESIAN_POINT('Ctrl Pts',(-0.791048562900586,1.32194889376214E-5,
-1.0846668491763));
#59489=CARTESIAN_POINT('Ctrl Pts',(-0.791078489980937,0.0497960584196038,
-1.08666959510031));
#59490=CARTESIAN_POINT('Ctrl Pts',(-0.786451603860431,0.0995734034696943,
-1.08867234102432));
#59491=CARTESIAN_POINT('Ctrl Pts',(-0.777114596853452,0.1484509815208,-1.09067508694833));
#59492=CARTESIAN_POINT('Ctrl Pts',(-0.75255015640129,0.277041476803167,
-1.09594404872103));
#59493=CARTESIAN_POINT('Ctrl Pts',(-0.695384752424045,0.399404261200396,
-1.10121301049372));
#59494=CARTESIAN_POINT('Ctrl Pts',(-0.612523206841235,0.500759534745093,
-1.10648197226642));
#59495=CARTESIAN_POINT('Ctrl Pts',(-0.529661661258425,0.602114808289789,
-1.11175093403912));
#59496=CARTESIAN_POINT('Ctrl Pts',(-0.421103974070052,0.682462570981951,
-1.11701989581181));
#59497=CARTESIAN_POINT('Ctrl Pts',(-0.29996247276581,0.732097879719245,
-1.12228885758451));
#59498=CARTESIAN_POINT('Ctrl Pts',(-0.178820971461567,0.781733188456539,
-1.12755781935721));
#59499=CARTESIAN_POINT('Ctrl Pts',(-0.0450956560414579,0.800656043238965,
-1.13282678112991));
#59500=CARTESIAN_POINT('Ctrl Pts',(0.0850612306191843,0.786580814413079,
-1.1380957429026));
#59501=CARTESIAN_POINT('Ctrl Pts',(0.215218117279826,0.772505585587193,
-1.1433647046753));
#59502=CARTESIAN_POINT('Ctrl Pts',(0.341806575180999,0.725432273152994,
-1.148633666448));
#59503=CARTESIAN_POINT('Ctrl Pts',(0.449536399092598,0.651046708345916,
-1.1539026282207));
#59504=CARTESIAN_POINT('Ctrl Pts',(0.557266223004195,0.57666114353884,-1.15917158999339));
#59505=CARTESIAN_POINT('Ctrl Pts',(0.646137412926217,0.474963326358887,
-1.16444055176609));
#59506=CARTESIAN_POINT('Ctrl Pts',(0.705415508896985,0.358237003064731,
-1.16970951353879));
#59507=CARTESIAN_POINT('Ctrl Pts',(0.764693604867754,0.241510679770572,
-1.17497847531148));
#59508=CARTESIAN_POINT('Ctrl Pts',(0.794378606887267,0.109755850362201,
-1.18024743708418));
#59509=CARTESIAN_POINT('Ctrl Pts',(0.790884960785258,-0.021113250836693,
-1.18551639885688));
#59510=CARTESIAN_POINT('Ctrl Pts',(0.78739131468325,-0.151982352035583,
-1.19078536062958));
#59511=CARTESIAN_POINT('Ctrl Pts',(0.750719020459724,-0.281965725025003,
-1.19605432240227));
#59512=CARTESIAN_POINT('Ctrl Pts',(0.685297604425638,-0.395363103900293,
-1.20132328417497));
#59513=CARTESIAN_POINT('Ctrl Pts',(0.619876188391549,-0.508760482775588,
-1.20659224594767));
#59514=CARTESIAN_POINT('Ctrl Pts',(0.525705650546899,-0.605571867536749,
-1.21186120772036));
#59515=CARTESIAN_POINT('Ctrl Pts',(0.414160541732633,-0.674103728093032,
-1.21713016949306));
#59516=CARTESIAN_POINT('Ctrl Pts',(0.302615432918367,-0.742635588649315,
-1.22239913126576));
#59517=CARTESIAN_POINT('Ctrl Pts',(0.173695753134486,-0.782887925000717,
-1.22766809303846));
#59518=CARTESIAN_POINT('Ctrl Pts',(0.0429732882671409,-0.789998789272934,
-1.23293705481115));
#59519=CARTESIAN_POINT('Ctrl Pts',(-0.0877491766002046,-0.797109653545151,
-1.23820601658385));
#59520=CARTESIAN_POINT('Ctrl Pts',(-0.220274426551013,-0.771079045738183,
-1.24347497835655));
#59521=CARTESIAN_POINT('Ctrl Pts',(-0.338595170687559,-0.71505111771415,
-1.24874394012925));
#59522=CARTESIAN_POINT('Ctrl Pts',(-0.456915914824105,-0.659023189690117,
-1.25401290190194));
#59523=CARTESIAN_POINT('Ctrl Pts',(-0.561032153146387,-0.572997941449019,
-1.25928186367464));
#59524=CARTESIAN_POINT('Ctrl Pts',(-0.638368026226707,-0.467366080977867,
-1.26455082544734));
#59525=CARTESIAN_POINT('Ctrl Pts',(-0.715703899307027,-0.361734220506716,
-1.26981978722003));
#59526=CARTESIAN_POINT('Ctrl Pts',(-0.766259407145385,-0.236495747805511,
-1.27508874899273));
#59527=CARTESIAN_POINT('Ctrl Pts',(-0.783928115528291,-0.106777807813496,
-1.28035771076543));
#59528=CARTESIAN_POINT('Ctrl Pts',(-0.788744808281546,-0.0714152081267372,
-1.28179409023572));
#59529=CARTESIAN_POINT('Ctrl Pts',(-0.791117452122437,-0.0357197077825311,
-1.28323046970601));
#59530=CARTESIAN_POINT('Ctrl Pts',(-0.79108328723417,-1.97011904900513E-5,
-1.2846668491763));
#59531=CARTESIAN_POINT('Ctrl Pts',(-0.791091395193699,-2.00455443718572E-5,
-1.3131331508237));
#59532=CARTESIAN_POINT('Ctrl Pts',(-0.791124112533671,-0.0330171053241025,
-1.3118054845087));
#59533=CARTESIAN_POINT('Ctrl Pts',(-0.789097998462795,-0.0660101745126855,
-1.31047781819369));
#59534=CARTESIAN_POINT('Ctrl Pts',(-0.784980989092685,-0.0987402366990249,
-1.30915015187868));
#59535=CARTESIAN_POINT('Ctrl Pts',(-0.768642271491913,-0.228632397499223,
-1.30388119010599));
#59536=CARTESIAN_POINT('Ctrl Pts',(-0.719372585026431,-0.354382277523696,
-1.29861222833329));
#59537=CARTESIAN_POINT('Ctrl Pts',(-0.643123053757393,-0.460800960617569,
-1.29334326656059));
#59538=CARTESIAN_POINT('Ctrl Pts',(-0.566873522488357,-0.56721964371144,
-1.2880743047879));
#59539=CARTESIAN_POINT('Ctrl Pts',(-0.463644146415765,-0.654307129874715,
-1.2828053430152));
#59540=CARTESIAN_POINT('Ctrl Pts',(-0.34590366378081,-0.71154440688078,
-1.2775363812425));
#59541=CARTESIAN_POINT('Ctrl Pts',(-0.228163181145847,-0.768781683886849,
-1.2722674194698));
#59542=CARTESIAN_POINT('Ctrl Pts',(-0.0959115919485175,-0.796168751735706,
-1.26699845769711));
#59543=CARTESIAN_POINT('Ctrl Pts',(0.0348768674995742,-0.79039761619942,
-1.26172949592441));
#59544=CARTESIAN_POINT('Ctrl Pts',(0.165665326947662,-0.784626480663134,
-1.25646053415171));
#59545=CARTESIAN_POINT('Ctrl Pts',(0.294990656646514,-0.745697141741706,
-1.25119157237902));
#59546=CARTESIAN_POINT('Ctrl Pts',(0.407232073585324,-0.678311746782928,
-1.24592261060632));
#59547=CARTESIAN_POINT('Ctrl Pts',(0.519473490524134,-0.610926351824149,
-1.24065364883362));
#59548=CARTESIAN_POINT('Ctrl Pts',(0.614630994702904,-0.515084900828019,
-1.23538468706092));
#59549=CARTESIAN_POINT('Ctrl Pts',(0.681210822849676,-0.402363768762516,
-1.23011572528823));
#59550=CARTESIAN_POINT('Ctrl Pts',(0.747790650996447,-0.289642636697016,
-1.22484676351553));
#59551=CARTESIAN_POINT('Ctrl Pts',(0.785792803111224,-0.160041823562142,
-1.21957780174283));
#59552=CARTESIAN_POINT('Ctrl Pts',(0.790627123703887,-0.0292153871106796,
-1.21430883997013));
#59553=CARTESIAN_POINT('Ctrl Pts',(0.795461444296551,0.101611049340787,
-1.20903987819744));
#59554=CARTESIAN_POINT('Ctrl Pts',(0.767127933367104,0.233663109108835,
-1.20377091642474));
#59555=CARTESIAN_POINT('Ctrl Pts',(0.709048902903408,0.350990656388148,
-1.19850195465204));
#59556=CARTESIAN_POINT('Ctrl Pts',(0.65096987243971,0.468318203667464,-1.19323299287935));
#59557=CARTESIAN_POINT('Ctrl Pts',(0.563145322441762,0.570921238458036,
-1.18796403110665));
#59558=CARTESIAN_POINT('Ctrl Pts',(0.456183292662752,0.646406676230745,
-1.18269506933395));
#59559=CARTESIAN_POINT('Ctrl Pts',(0.349221262883743,0.721892114003455,
-1.17742610756125));
#59560=CARTESIAN_POINT('Ctrl Pts',(0.22312175332367,0.770259954758303,-1.17215714578856));
#59561=CARTESIAN_POINT('Ctrl Pts',(0.0931159107439142,0.785668005423818,
-1.16688818401586));
#59562=CARTESIAN_POINT('Ctrl Pts',(-0.0368899318358343,0.801076056089331,
-1.16161922224316));
#59563=CARTESIAN_POINT('Ctrl Pts',(-0.170802107435268,0.783524316665514,
-1.15635026047047));
#59564=CARTESIAN_POINT('Ctrl Pts',(-0.292445802949988,0.735132804272293,
-1.15108129869777));
#59565=CARTESIAN_POINT('Ctrl Pts',(-0.414089498464712,0.68674129187907,
-1.14581233692507));
#59566=CARTESIAN_POINT('Ctrl Pts',(-0.523464713894725,0.60751000651644,
-1.14054337515237));
#59567=CARTESIAN_POINT('Ctrl Pts',(-0.607360375191571,0.507009035646765,
-1.13527441337968));
#59568=CARTESIAN_POINT('Ctrl Pts',(-0.691256036488417,0.406508064777091,
-1.13000545160698));
#59569=CARTESIAN_POINT('Ctrl Pts',(-0.749672143652099,0.28473740840037,
-1.12473648983428));
#59570=CARTESIAN_POINT('Ctrl Pts',(-0.775552806421482,0.15640534527973,
-1.11946752806158));
#59571=CARTESIAN_POINT('Ctrl Pts',(-0.785924102084645,0.104978154965951,
-1.11735606898229));
#59572=CARTESIAN_POINT('Ctrl Pts',(-0.791070569896215,0.0524972762412874,
-1.115244609903));
#59573=CARTESIAN_POINT('Ctrl Pts',(-0.791043937878947,1.12442601377988E-5,
-1.1131331508237));
#59574=CARTESIAN_POINT('Origin',(0.,0.,-1.97));
#59575=CARTESIAN_POINT('',(-0.791164617967662,4.43993036714635E-6,-0.884666849176296));
#59576=CARTESIAN_POINT('',(-0.79116135777148,7.11475864817537E-6,-0.913133150823704));
#59577=CARTESIAN_POINT('',(-0.7911,-9.68818082805471E-17,-1.97));
#59578=CARTESIAN_POINT('Ctrl Pts',(-0.791164617967662,4.43993036714635E-6,
-0.884666849176296));
#59579=CARTESIAN_POINT('Ctrl Pts',(-0.791165954160854,0.00430068567149038,
-0.884839758721909));
#59580=CARTESIAN_POINT('Ctrl Pts',(-0.79113168381486,0.00859691002598646,
-0.885012668267522));
#59581=CARTESIAN_POINT('Ctrl Pts',(-0.791061674373356,0.012892551912441,
-0.885185577813136));
#59582=CARTESIAN_POINT('Ctrl Pts',(-0.788928321528631,0.143790894214137,
-0.890454539585833));
#59583=CARTESIAN_POINT('Ctrl Pts',(-0.753608907198563,0.274148377270177,
-0.895723501358531));
#59584=CARTESIAN_POINT('Ctrl Pts',(-0.6893695477627,0.388219547646229,-0.900992463131228));
#59585=CARTESIAN_POINT('Ctrl Pts',(-0.625130188326837,0.50229071802228,
-0.906261424903925));
#59586=CARTESIAN_POINT('Ctrl Pts',(-0.531970883785179,0.600075575718343,
-0.911530386676622));
#59587=CARTESIAN_POINT('Ctrl Pts',(-0.421144041419974,0.669763008036159,
-0.916799348449319));
#59588=CARTESIAN_POINT('Ctrl Pts',(-0.310317199054769,0.739450440353975,
-0.922068310222016));
#59589=CARTESIAN_POINT('Ctrl Pts',(-0.181822818866018,0.781040447293544,
-0.927337271994713));
#59590=CARTESIAN_POINT('Ctrl Pts',(-0.0511813161947067,0.789509508131327,
-0.932606233767411));
#59591=CARTESIAN_POINT('Ctrl Pts',(0.0794601864766005,0.797978568969109,
-0.937875195540108));
#59592=CARTESIAN_POINT('Ctrl Pts',(0.212248811630478,0.773326683705103,
-0.943144157312806));
#59593=CARTESIAN_POINT('Ctrl Pts',(0.331145456140999,0.718531472821032,
-0.948413119085503));
#59594=CARTESIAN_POINT('Ctrl Pts',(0.450042100651527,0.663736261936958,
-0.9536820808582));
#59595=CARTESIAN_POINT('Ctrl Pts',(0.555046764518701,0.57879772543282,-0.958951042630897));
#59596=CARTESIAN_POINT('Ctrl Pts',(0.633476278303023,0.473975310944086,
-0.964220004403595));
#59597=CARTESIAN_POINT('Ctrl Pts',(0.711905792087343,0.369152896455355,
-0.969488966176292));
#59598=CARTESIAN_POINT('Ctrl Pts',(0.763760155788802,0.244446603982033,
-0.97475792794899));
#59599=CARTESIAN_POINT('Ctrl Pts',(0.782776050648192,0.114919298156625,
-0.980026889721687));
#59600=CARTESIAN_POINT('Ctrl Pts',(0.801791945507582,-0.0146080076687826,
-0.985295851494384));
#59601=CARTESIAN_POINT('Ctrl Pts',(0.787969371524902,-0.148956326846277,
-0.99056481326708));
#59602=CARTESIAN_POINT('Ctrl Pts',(0.742977912140126,-0.271898165917117,
-0.995833775039778));
#59603=CARTESIAN_POINT('Ctrl Pts',(0.697986452755349,-0.394840004987956,
-1.00110273681248));
#59604=CARTESIAN_POINT('Ctrl Pts',(0.621826107968476,-0.50637536395214,
-1.00637169858517));
#59605=CARTESIAN_POINT('Ctrl Pts',(0.523696036387599,-0.593032252098578,
-1.01164066035787));
#59606=CARTESIAN_POINT('Ctrl Pts',(0.425565964806725,-0.679689140245013,
-1.01690962213057));
#59607=CARTESIAN_POINT('Ctrl Pts',(0.30546616643185,-0.741467557573703,
-1.02217858390326));
#59608=CARTESIAN_POINT('Ctrl Pts',(0.177903102560412,-0.770905491390852,
-1.02744754567596));
#59609=CARTESIAN_POINT('Ctrl Pts',(0.0503400386889753,-0.800343425208001,
-1.03271650744866));
#59610=CARTESIAN_POINT('Ctrl Pts',(-0.0846862906790231,-0.797440875513609,
-1.03798546922136));
#59611=CARTESIAN_POINT('Ctrl Pts',(-0.210866497454535,-0.762548431778893,
-1.04325443099405));
#59612=CARTESIAN_POINT('Ctrl Pts',(-0.337046704230054,-0.727655988044175,
-1.04852339276675));
#59613=CARTESIAN_POINT('Ctrl Pts',(-0.454380788413085,-0.660773650269129,
-1.05379235453945));
#59614=CARTESIAN_POINT('Ctrl Pts',(-0.548696350265211,-0.569979916982019,
-1.05906131631214));
#59615=CARTESIAN_POINT('Ctrl Pts',(-0.643011912117332,-0.479186183694914,
-1.06433027808484));
#59616=CARTESIAN_POINT('Ctrl Pts',(-0.714308951638551,-0.364481054895748,
-1.06959923985754));
#59617=CARTESIAN_POINT('Ctrl Pts',(-0.753975732935622,-0.239719387412416,
-1.07486820163024));
#59618=CARTESIAN_POINT('Ctrl Pts',(-0.778565068620354,-0.162379950684253,
-1.07813441747892));
#59619=CARTESIAN_POINT('Ctrl Pts',(-0.790999755758863,-0.0811760594697772,
-1.08140063332761));
#59620=CARTESIAN_POINT('Ctrl Pts',(-0.791048562900586,1.32194889376214E-5,
-1.0846668491763));
#59621=CARTESIAN_POINT('Ctrl Pts',(-0.791043937878947,1.12442601377988E-5,
-1.1131331508237));
#59622=CARTESIAN_POINT('Ctrl Pts',(-0.791004112022466,-0.0784770338087006,
-1.1099756481303));
#59623=CARTESIAN_POINT('Ctrl Pts',(-0.779395894589143,-0.15697683589426,
-1.1068181454369));
#59624=CARTESIAN_POINT('Ctrl Pts',(-0.756392270823624,-0.231981723889169,
-1.10366064274349));
#59625=CARTESIAN_POINT('Ctrl Pts',(-0.718005854081292,-0.35714326007288,
-1.0983916809708));
#59626=CARTESIAN_POINT('Ctrl Pts',(-0.647887802221541,-0.472572862575744,
-1.0931227191981));
#59627=CARTESIAN_POINT('Ctrl Pts',(-0.554507445079383,-0.564328167763975,
-1.0878537574254));
#59628=CARTESIAN_POINT('Ctrl Pts',(-0.461127087937224,-0.656083472952205,
-1.0825847956527));
#59629=CARTESIAN_POINT('Ctrl Pts',(-0.344484425512659,-0.724164480825803,
-1.07731583388001));
#59630=CARTESIAN_POINT('Ctrl Pts',(-0.218668342974427,-0.760347909421159,
-1.07204687210731));
#59631=CARTESIAN_POINT('Ctrl Pts',(-0.0928522604361946,-0.796531338016516,
-1.06677791033461));
#59632=CARTESIAN_POINT('Ctrl Pts',(0.0421372422157041,-0.80081718733363,
-1.06150894856192));
#59633=CARTESIAN_POINT('Ctrl Pts',(0.169995225070644,-0.77268778367041,
-1.05623998678922));
#59634=CARTESIAN_POINT('Ctrl Pts',(0.297853207925584,-0.74455838000719,
-1.05097102501652));
#59635=CARTESIAN_POINT('Ctrl Pts',(0.418579670983564,-0.684013723363635,
-1.04570206324382));
#59636=CARTESIAN_POINT('Ctrl Pts',(0.517592460172511,-0.598366804521171,
-1.04043310147113));
#59637=CARTESIAN_POINT('Ctrl Pts',(0.616605249361455,-0.512719885678709,
-1.03516413969843));
#59638=CARTESIAN_POINT('Ctrl Pts',(0.693904364681367,-0.40197070463734,
-1.02989517792573));
#59639=CARTESIAN_POINT('Ctrl Pts',(0.740153099161143,-0.279496292251729,
-1.02462621615304));
#59640=CARTESIAN_POINT('Ctrl Pts',(0.786401833640922,-0.157021879866112,
-1.01935725438034));
#59641=CARTESIAN_POINT('Ctrl Pts',(0.801600187280563,-0.0228222361362515,
-1.01408829260764));
#59642=CARTESIAN_POINT('Ctrl Pts',(0.783912400721252,0.10689310349949,-1.00881933083494));
#59643=CARTESIAN_POINT('Ctrl Pts',(0.766224614161942,0.236608443135223,
-1.00355036906225));
#59644=CARTESIAN_POINT('Ctrl Pts',(0.715650687403683,0.361839478676839,
-0.998281407289548));
#59645=CARTESIAN_POINT('Ctrl Pts',(0.638299279420976,0.46745996349524,-0.993012445516851));
#59646=CARTESIAN_POINT('Ctrl Pts',(0.560947871438269,0.573080448313642,
-0.987743483744154));
#59647=CARTESIAN_POINT('Ctrl Pts',(0.456818982231114,0.659090382408831,
-0.982474521971457));
#59648=CARTESIAN_POINT('Ctrl Pts',(0.338489999286157,0.715100907539325,
-0.97720556019876));
#59649=CARTESIAN_POINT('Ctrl Pts',(0.220161016341194,0.771111432669822,
-0.971936598426063));
#59650=CARTESIAN_POINT('Ctrl Pts',(0.0876319396584279,0.79712254883562,
-0.966667636653365));
#59651=CARTESIAN_POINT('Ctrl Pts',(-0.0430894776459918,0.789992458506096,
-0.961398674880668));
#59652=CARTESIAN_POINT('Ctrl Pts',(-0.173810894950408,0.782862368176572,
-0.95612971310797));
#59653=CARTESIAN_POINT('Ctrl Pts',(-0.302724652876478,0.742591071351728,
-0.950860751335273));
#59654=CARTESIAN_POINT('Ctrl Pts',(-0.414259680819861,0.674042806079358,
-0.945591789562576));
#59655=CARTESIAN_POINT('Ctrl Pts',(-0.525794708763244,0.605494540806989,
-0.940322827789879));
#59656=CARTESIAN_POINT('Ctrl Pts',(-0.619951006723941,0.508669307087093,
-0.935053866017182));
#59657=CARTESIAN_POINT('Ctrl Pts',(-0.685355743849948,0.395262307780788,
-0.929784904244485));
#59658=CARTESIAN_POINT('Ctrl Pts',(-0.750760480975956,0.281855308474479,
-0.924515942471787));
#59659=CARTESIAN_POINT('Ctrl Pts',(-0.787413657267272,0.151866543581759,
-0.919246980699089));
#59660=CARTESIAN_POINT('Ctrl Pts',(-0.790888055605358,0.020996930277632,
-0.913978018926392));
#59661=CARTESIAN_POINT('Ctrl Pts',(-0.79107376001662,0.0140020315568058,
-0.913696396225496));
#59662=CARTESIAN_POINT('Ctrl Pts',(-0.79116467811953,0.0070046163970303,
-0.9134147735246));
#59663=CARTESIAN_POINT('Ctrl Pts',(-0.79116135777148,7.11475864817537E-6,
-0.913133150823704));
#59664=CARTESIAN_POINT('Origin',(0.,0.,-1.97));
#59665=CARTESIAN_POINT('',(-0.79106797157506,-1.80494624554273E-5,-0.684666849176296));
#59666=CARTESIAN_POINT('',(-0.791075294242739,-1.90178071996814E-5,-0.713133150823704));
#59667=CARTESIAN_POINT('',(-0.7911,-9.68818082805471E-17,-1.97));
#59668=CARTESIAN_POINT('Ctrl Pts',(-0.79106797157506,-1.80494624554273E-5,
-0.684666849176296));
#59669=CARTESIAN_POINT('Ctrl Pts',(-0.790991667205036,0.0897610395828043,
-0.688278884116209));
#59670=CARTESIAN_POINT('Ctrl Pts',(-0.775729031502744,0.179565416210847,
-0.691890919056122));
#59671=CARTESIAN_POINT('Ctrl Pts',(-0.74576358619739,0.264161814157916,
-0.695502953996035));
#59672=CARTESIAN_POINT('Ctrl Pts',(-0.702052274307491,0.387564603528967,
-0.700771915768733));
#59673=CARTESIAN_POINT('Ctrl Pts',(-0.627055214381976,0.499885462766481,
-0.70604087754143));
#59674=CARTESIAN_POINT('Ctrl Pts',(-0.529831055660502,0.587557523154006,
-0.711309839314127));
#59675=CARTESIAN_POINT('Ctrl Pts',(-0.432606896939028,0.675229583541531,
-0.716578801086824));
#59676=CARTESIAN_POINT('Ctrl Pts',(-0.313155639421595,0.738252845079068,
-0.721847762859521));
#59677=CARTESIAN_POINT('Ctrl Pts',(-0.18590540927956,0.769014934417917,
-0.727116724632219));
#59678=CARTESIAN_POINT('Ctrl Pts',(-0.058655179137525,0.799777023756766,
-0.732385686404916));
#59679=CARTESIAN_POINT('Ctrl Pts',(0.0763940236291114,0.798277940896928,
-0.737654648177614));
#59680=CARTESIAN_POINT('Ctrl Pts',(0.202930048128393,0.76469875514728,-0.742923609950311));
#59681=CARTESIAN_POINT('Ctrl Pts',(0.329466072627671,0.731119569397634,
-0.748192571723008));
#59682=CARTESIAN_POINT('Ctrl Pts',(0.447488918859595,0.665460280758179,
-0.753461533495704));
#59683=CARTESIAN_POINT('Ctrl Pts',(0.542742993773683,0.575651659657794,
-0.758730495268401));
#59684=CARTESIAN_POINT('Ctrl Pts',(0.637997068687777,0.485843038557404,
-0.763999457041099));
#59685=CARTESIAN_POINT('Ctrl Pts',(0.710482372284031,0.37188508499608,-0.769268418813797));
#59686=CARTESIAN_POINT('Ctrl Pts',(0.751443642143352,0.247542406951874,
-0.774537380586494));
#59687=CARTESIAN_POINT('Ctrl Pts',(0.792404912002671,0.123199728907672,
-0.779806342359191));
#59688=CARTESIAN_POINT('Ctrl Pts',(0.801842148125059,-0.0115276736194127,
-0.785075304131888));
#59689=CARTESIAN_POINT('Ctrl Pts',(0.778615457667923,-0.140366518934405,
-0.790344265904585));
#59690=CARTESIAN_POINT('Ctrl Pts',(0.755388767210788,-0.269205364249398,
-0.795613227677282));
#59691=CARTESIAN_POINT('Ctrl Pts',(0.699498150174129,-0.392155652352298,
-0.80088218944998));
#59692=CARTESIAN_POINT('Ctrl Pts',(0.617694451138065,-0.49436662062728,
-0.806151151222677));
#59693=CARTESIAN_POINT('Ctrl Pts',(0.535890752102002,-0.596577588902262,
-0.811420112995375));
#59694=CARTESIAN_POINT('Ctrl Pts',(0.428173971066533,-0.678049237349324,
-0.816689074768072));
#59695=CARTESIAN_POINT('Ctrl Pts',(0.307554865221265,-0.728940872386727,
-0.82195803654077));
#59696=CARTESIAN_POINT('Ctrl Pts',(0.186935759375997,-0.779832507424129,
-0.827226998313467));
#59697=CARTESIAN_POINT('Ctrl Pts',(0.0534143287209287,-0.800144129051871,
-0.832495960086164));
#59698=CARTESIAN_POINT('Ctrl Pts',(-0.0768818104416133,-0.787422363017722,
-0.837764921858862));
#59699=CARTESIAN_POINT('Ctrl Pts',(-0.207177949604159,-0.774700596983572,
-0.843033883631559));
#59700=CARTESIAN_POINT('Ctrl Pts',(-0.334248797274178,-0.728945443287528,
-0.848302845404255));
#59701=CARTESIAN_POINT('Ctrl Pts',(-0.442745881941299,-0.655683517088247,
-0.853571807176953));
#59702=CARTESIAN_POINT('Ctrl Pts',(-0.551242966608413,-0.582421590888971,
-0.85884076894965));
#59703=CARTESIAN_POINT('Ctrl Pts',(-0.641166288272631,-0.48165289218646,
-0.864109730722348));
#59704=CARTESIAN_POINT('Ctrl Pts',(-0.701654303425048,-0.36554894206153,
-0.869378692495045));
#59705=CARTESIAN_POINT('Ctrl Pts',(-0.76015730603301,-0.253255131794522,
-0.874474744722129));
#59706=CARTESIAN_POINT('Ctrl Pts',(-0.791125237202045,-0.126616057506534,
-0.879570796949212));
#59707=CARTESIAN_POINT('Ctrl Pts',(-0.791164617967662,4.43993036714635E-6,
-0.884666849176296));
#59708=CARTESIAN_POINT('Ctrl Pts',(-0.79116135777148,7.11475864817537E-6,
-0.913133150823704));
#59709=CARTESIAN_POINT('Ctrl Pts',(-0.791102556753278,-0.123913695655651,
-0.908145811751903));
#59710=CARTESIAN_POINT('Ctrl Pts',(-0.761488779732474,-0.247861627410726,
-0.903158472680102));
#59711=CARTESIAN_POINT('Ctrl Pts',(-0.705362811486509,-0.358340748104591,
-0.898171133608301));
#59712=CARTESIAN_POINT('Ctrl Pts',(-0.646067548644711,-0.475058351467171,
-0.892902171835604));
#59713=CARTESIAN_POINT('Ctrl Pts',(-0.557181402576256,-0.576743096476801,
-0.887633210062906));
#59714=CARTESIAN_POINT('Ctrl Pts',(-0.449440639746771,-0.651112815819442,
-0.882364248290209));
#59715=CARTESIAN_POINT('Ctrl Pts',(-0.341699876917287,-0.725482535162083,
-0.877095286517512));
#59716=CARTESIAN_POINT('Ctrl Pts',(-0.215104497326772,-0.772537228837736,
-0.871826324744815));
#59717=CARTESIAN_POINT('Ctrl Pts',(-0.0849455422535194,-0.786593314509833,
-0.866557362972118));
#59718=CARTESIAN_POINT('Ctrl Pts',(0.0452134128197299,-0.800649400181929,
-0.861288401199421));
#59719=CARTESIAN_POINT('Ctrl Pts',(0.178935943375718,-0.781706877850472,
-0.856019439426723));
#59720=CARTESIAN_POINT('Ctrl Pts',(0.300070142913725,-0.732053752747738,
-0.850750477654026));
#59721=CARTESIAN_POINT('Ctrl Pts',(0.421204342451739,-0.682400627645001,
-0.845481515881328));
#59722=CARTESIAN_POINT('Ctrl Pts',(0.52975021097177,-0.602036899770983,
-0.840212554108631));
#59723=CARTESIAN_POINT('Ctrl Pts',(0.612596848522363,-0.500669440610047,
-0.834943592335933));
#59724=CARTESIAN_POINT('Ctrl Pts',(0.695443486072952,-0.399301981449116,
-0.829674630563237));
#59725=CARTESIAN_POINT('Ctrl Pts',(0.752590892654105,-0.276930791001269,
-0.82440566879054));
#59726=CARTESIAN_POINT('Ctrl Pts',(0.777136420192834,-0.148336684573226,
-0.819136707017843));
#59727=CARTESIAN_POINT('Ctrl Pts',(0.801681947731563,-0.0197425781451788,
-0.813867745245145));
#59728=CARTESIAN_POINT('Ctrl Pts',(0.793625596227868,0.115074444263065,
-0.808598783472448));
#59729=CARTESIAN_POINT('Ctrl Pts',(0.75394046599389,0.239830276064607,-0.80332982169975));
#59730=CARTESIAN_POINT('Ctrl Pts',(0.714255335759913,0.364586107866145,
-0.798060859927053));
#59731=CARTESIAN_POINT('Ctrl Pts',(0.642941426795649,0.479280749060992,
-0.792791898154356));
#59732=CARTESIAN_POINT('Ctrl Pts',(0.548612512599131,0.57006060958461,-0.787522936381659));
#59733=CARTESIAN_POINT('Ctrl Pts',(0.454283598402605,0.660840470108236,
-0.782253974608962));
#59734=CARTESIAN_POINT('Ctrl Pts',(0.336939678973828,0.727705549960633,
-0.776985012836264));
#59735=CARTESIAN_POINT('Ctrl Pts',(0.210754342018317,0.762579435141504,
-0.771716051063566));
#59736=CARTESIAN_POINT('Ctrl Pts',(0.0845690050628165,0.797453320322372,
-0.766447089290869));
#59737=CARTESIAN_POINT('Ctrl Pts',(-0.0504577494194056,0.800336010831712,
-0.761178127518172));
#59738=CARTESIAN_POINT('Ctrl Pts',(-0.178016481991146,0.770879315924228,
-0.755909165745476));
#59739=CARTESIAN_POINT('Ctrl Pts',(-0.30557521456289,0.741422621016742,
-0.750640203972778));
#59740=CARTESIAN_POINT('Ctrl Pts',(-0.425665925224152,0.679626540692429,
-0.745371242200081));
#59741=CARTESIAN_POINT('Ctrl Pts',(-0.523783250352655,0.592955221100478,
-0.740102280427384));
#59742=CARTESIAN_POINT('Ctrl Pts',(-0.621900575481158,0.506283901508527,
-0.734833318654687));
#59743=CARTESIAN_POINT('Ctrl Pts',(-0.698044515076902,0.394737342648938,
-0.729564356881989));
#59744=CARTESIAN_POINT('Ctrl Pts',(-0.743017892061099,0.271788888031485,
-0.724295395109292));
#59745=CARTESIAN_POINT('Ctrl Pts',(-0.774776446016752,0.184967186136503,
-0.720574647014096));
#59746=CARTESIAN_POINT('Ctrl Pts',(-0.79099127576657,0.0924597375550537,
-0.7168538989189));
#59747=CARTESIAN_POINT('Ctrl Pts',(-0.791075294242739,-1.90178071996815E-5,
-0.713133150823704));
#59748=CARTESIAN_POINT('Origin',(0.,0.,-1.97));
#59749=CARTESIAN_POINT('',(-0.79106019175573,1.65874934803245E-5,-0.484666849176295));
#59750=CARTESIAN_POINT('',(-0.791054102114328,1.50443135659429E-5,-0.513133150823704));
#59751=CARTESIAN_POINT('',(-0.7911,-9.68818082805471E-17,-1.97));
#59752=CARTESIAN_POINT('Ctrl Pts',(-0.79106019175573,1.65874934803245E-5,
-0.484666849176295));
#59753=CARTESIAN_POINT('Ctrl Pts',(-0.791094293741917,0.044315349832207,
-0.486449047737811));
#59754=CARTESIAN_POINT('Ctrl Pts',(-0.787435186917273,0.0886085381329495,
-0.488231246299327));
#59755=CARTESIAN_POINT('Ctrl Pts',(-0.780032216716909,0.13226689472754,
-0.490013444860843));
#59756=CARTESIAN_POINT('Ctrl Pts',(-0.758145785074321,0.261340173610695,
-0.49528240663354));
#59757=CARTESIAN_POINT('Ctrl Pts',(-0.70353599197578,0.384864685004406,
-0.500551368406237));
#59758=CARTESIAN_POINT('Ctrl Pts',(-0.622798975472762,0.48792030774224,
-0.505820330178935));
#59759=CARTESIAN_POINT('Ctrl Pts',(-0.542061958969747,0.59097593048007,
-0.511089291951632));
#59760=CARTESIAN_POINT('Ctrl Pts',(-0.435197719062254,0.673562664562026,
-0.51635825372433));
#59761=CARTESIAN_POINT('Ctrl Pts',(-0.315114037289311,0.725705128864625,
-0.521627215497027));
#59762=CARTESIAN_POINT('Ctrl Pts',(-0.195030355516371,0.777847593167222,
-0.526896177269724));
#59763=CARTESIAN_POINT('Ctrl Pts',(-0.0617272318779785,0.799545787690465,
-0.532165139042421));
#59764=CARTESIAN_POINT('Ctrl Pts',(0.0686940859131107,0.788178858583351,
-0.537434100815118));
#59765=CARTESIAN_POINT('Ctrl Pts',(0.199115403704207,0.776811929476236,
-0.542703062587815));
#59766=CARTESIAN_POINT('Ctrl Pts',(0.326654915647992,0.732379876738765,
-0.547972024360513));
#59767=CARTESIAN_POINT('Ctrl Pts',(0.435907541811431,0.660249502498192,
-0.55324098613321));
#59768=CARTESIAN_POINT('Ctrl Pts',(0.545160167974864,0.588119128257622,
-0.558509947905907));
#59769=CARTESIAN_POINT('Ctrl Pts',(0.63612590835795,0.488290432513946,-0.563778909678605));
#59770=CARTESIAN_POINT('Ctrl Pts',(0.697817309108831,0.372821396469276,
-0.569047871451302));
#59771=CARTESIAN_POINT('Ctrl Pts',(0.759508709859716,0.2573523604246,-0.574316833223999));
#59772=CARTESIAN_POINT('Ctrl Pts',(0.7919257709784,0.12624298407893,-0.579585794996696));
#59773=CARTESIAN_POINT('Ctrl Pts',(0.791152941824015,-0.00467046040555037,
-0.584854756769393));
#59774=CARTESIAN_POINT('Ctrl Pts',(0.790380112669631,-0.135583904890027,
-0.59012371854209));
#59775=CARTESIAN_POINT('Ctrl Pts',(0.756417393242176,-0.266301417513306,
-0.595392680314788));
#59776=CARTESIAN_POINT('Ctrl Pts',(0.693367029187332,-0.381034058048786,
-0.600661642087485));
#59777=CARTESIAN_POINT('Ctrl Pts',(0.63031666513249,-0.495766698584263,
-0.605930603860182));
#59778=CARTESIAN_POINT('Ctrl Pts',(0.538178656450259,-0.594514467031945,
-0.611199565632879));
#59779=CARTESIAN_POINT('Ctrl Pts',(0.428082051440955,-0.665349943857589,
-0.616468527405576));
#59780=CARTESIAN_POINT('Ctrl Pts',(0.317985446431644,-0.736185420683236,
-0.621737489178273));
#59781=CARTESIAN_POINT('Ctrl Pts',(0.189930245095256,-0.779108605886844,
-0.627006450950971));
#59782=CARTESIAN_POINT('Ctrl Pts',(0.0593838157975924,-0.788934948508754,
-0.632275412723668));
#59783=CARTESIAN_POINT('Ctrl Pts',(-0.0711626135000637,-0.798761291130663,
-0.637544374496366));
#59784=CARTESIAN_POINT('Ctrl Pts',(-0.204200270759008,-0.775490791170876,
-0.642813336269063));
#59785=CARTESIAN_POINT('Ctrl Pts',(-0.323659973080967,-0.721934216104501,
-0.64808229804176));
#59786=CARTESIAN_POINT('Ctrl Pts',(-0.443119675402932,-0.668377641038123,
-0.653351259814458));
#59787=CARTESIAN_POINT('Ctrl Pts',(-0.549001422787913,-0.58453499086516,
-0.658620221587155));
#59788=CARTESIAN_POINT('Ctrl Pts',(-0.628516105750902,-0.480533344700359,
-0.663889183359853));
#59789=CARTESIAN_POINT('Ctrl Pts',(-0.708030788713888,-0.376531698535561,
-0.66915814513255));
#59790=CARTESIAN_POINT('Ctrl Pts',(-0.761178407254874,-0.252371056378931,
-0.674427106905247));
#59791=CARTESIAN_POINT('Ctrl Pts',(-0.781539434598224,-0.123048375548322,
-0.679696068677944));
#59792=CARTESIAN_POINT('Ctrl Pts',(-0.787942353048508,-0.082380359874697,
-0.681352995510728));
#59793=CARTESIAN_POINT('Ctrl Pts',(-0.791102974214916,-0.0412018652717124,
-0.683009922343512));
#59794=CARTESIAN_POINT('Ctrl Pts',(-0.79106797157506,-1.80494624554273E-5,
-0.684666849176296));
#59795=CARTESIAN_POINT('Ctrl Pts',(-0.791075294242739,-1.90178071996815E-5,
-0.713133150823704));
#59796=CARTESIAN_POINT('Ctrl Pts',(-0.791110254565405,-0.0384996862821712,
-0.711584937146203));
#59797=CARTESIAN_POINT('Ctrl Pts',(-0.788352301462993,-0.0769753867691262,
-0.710036723468702));
#59798=CARTESIAN_POINT('Ctrl Pts',(-0.782759138437657,-0.115034424293976,
-0.708488509791201));
#59799=CARTESIAN_POINT('Ctrl Pts',(-0.763724193457369,-0.244558931626677,
-0.703219548018504));
#59800=CARTESIAN_POINT('Ctrl Pts',(-0.711851489124143,-0.369257595916767,
-0.697950586245807));
#59801=CARTESIAN_POINT('Ctrl Pts',(-0.633406559502031,-0.474068473915013,
-0.692681624473109));
#59802=CARTESIAN_POINT('Ctrl Pts',(-0.554961629879913,-0.578879351913266,
-0.687412662700412));
#59803=CARTESIAN_POINT('Ctrl Pts',(-0.449944474968907,-0.663802443619672,
-0.682143700927715));
#59804=CARTESIAN_POINT('Ctrl Pts',(-0.331039772960799,-0.718580166925286,
-0.676874739155018));
#59805=CARTESIAN_POINT('Ctrl Pts',(-0.212135070952697,-0.773357890230898,
-0.67160577738232));
#59806=CARTESIAN_POINT('Ctrl Pts',(-0.0793428218474851,-0.797990245135722,
-0.666336815609623));
#59807=CARTESIAN_POINT('Ctrl Pts',(0.0512974335036988,-0.789501970166157,
-0.661067853836925));
#59808=CARTESIAN_POINT('Ctrl Pts',(0.18193768885489,-0.781013695196591,
-0.655798892064228));
#59809=CARTESIAN_POINT('Ctrl Pts',(0.310425950452053,-0.739404790352641,
-0.650529930291531));
#59810=CARTESIAN_POINT('Ctrl Pts',(0.42124254199886,-0.669701058973814,
-0.645260968518834));
#59811=CARTESIAN_POINT('Ctrl Pts',(0.532059133545661,-0.599997327594991,
-0.639992006746136));
#59812=CARTESIAN_POINT('Ctrl Pts',(0.625204055042095,-0.502198769681299,
-0.634723044973439));
#59813=CARTESIAN_POINT('Ctrl Pts',(0.689426636486842,-0.388118152735411,
-0.629454083200742));
#59814=CARTESIAN_POINT('Ctrl Pts',(0.753649217931591,-0.27403753578952,
-0.624185121428045));
#59815=CARTESIAN_POINT('Ctrl Pts',(0.788949459324651,-0.143674859811422,
-0.618916159655348));
#59816=CARTESIAN_POINT('Ctrl Pts',(0.791063560122737,-0.0127762054715168,
-0.61364719788265));
#59817=CARTESIAN_POINT('Ctrl Pts',(0.793177660920822,0.118122448868388,
-0.608378236109953));
#59818=CARTESIAN_POINT('Ctrl Pts',(0.762105621123936,0.249557081570111,
-0.603109274337256));
#59819=CARTESIAN_POINT('Ctrl Pts',(0.701600530652673,0.365652133821474,
-0.597840312564558));
#59820=CARTESIAN_POINT('Ctrl Pts',(0.641095440181409,0.481747186072837,
-0.592571350791861));
#59821=CARTESIAN_POINT('Ctrl Pts',(0.551157299035769,0.582502657873839,
-0.587302389019164));
#59822=CARTESIAN_POINT('Ctrl Pts',(0.442649440721279,0.65574862577778,-0.582033427246467));
#59823=CARTESIAN_POINT('Ctrl Pts',(0.334141582406789,0.728994593681721,
-0.576764465473769));
#59824=CARTESIAN_POINT('Ctrl Pts',(0.207064006923452,0.7747310576886,-0.571495503701072));
#59825=CARTESIAN_POINT('Ctrl Pts',(0.0767659984121724,0.787433660106102,
-0.566226541928375));
#59826=CARTESIAN_POINT('Ctrl Pts',(-0.053532010099107,0.800136262523604,
-0.560957580155678));
#59827=CARTESIAN_POINT('Ctrl Pts',(-0.187050451638326,0.779805003351729,
-0.55568861838298));
#59828=CARTESIAN_POINT('Ctrl Pts',(-0.307662070948674,0.728895628797348,
-0.550419656610283));
#59829=CARTESIAN_POINT('Ctrl Pts',(-0.428273690259019,0.677986254242969,
-0.545150694837586));
#59830=CARTESIAN_POINT('Ctrl Pts',(-0.535978487340491,0.596498764306088,
-0.539881733064889));
#59831=CARTESIAN_POINT('Ctrl Pts',(-0.617767152506043,0.494275766010113,
-0.534612771292192));
#59832=CARTESIAN_POINT('Ctrl Pts',(-0.6995558176716,0.392052767714133,-0.529343809519495));
#59833=CARTESIAN_POINT('Ctrl Pts',(-0.755428350921232,0.269094261059059,
-0.524074847746797));
#59834=CARTESIAN_POINT('Ctrl Pts',(-0.778636091956227,0.140252001352719,
-0.5188058859741));
#59835=CARTESIAN_POINT('Ctrl Pts',(-0.786964827547154,0.0940134160283837,
-0.516914974257301));
#59836=CARTESIAN_POINT('Ctrl Pts',(-0.79108656509169,0.0470170442338496,
-0.515024062540503));
#59837=CARTESIAN_POINT('Ctrl Pts',(-0.791054102114328,1.50443135659429E-5,
-0.513133150823704));
#59838=CARTESIAN_POINT('Origin',(0.,0.,-1.97));
#59839=CARTESIAN_POINT('',(-0.79116655976261,-1.23482099584349E-6,-0.284666849176295));
#59840=CARTESIAN_POINT('',(-0.791166451109383,1.58231152821223E-6,-0.313133150823703));
#59841=CARTESIAN_POINT('',(-0.7911,-9.68818082805471E-17,-1.97));
#59842=CARTESIAN_POINT('Ctrl Pts',(-0.79116655976261,-1.23482099584349E-6,
-0.284666849176295));
#59843=CARTESIAN_POINT('Ctrl Pts',(-0.79115461052684,0.12973093383712,-0.289888173132111));
#59844=CARTESIAN_POINT('Ctrl Pts',(-0.758584934860785,0.25946888427355,
-0.295109497087927));
#59845=CARTESIAN_POINT('Ctrl Pts',(-0.697289616848199,0.373807411251276,
-0.300330821043743));
#59846=CARTESIAN_POINT('Ctrl Pts',(-0.635435058466726,0.48918912916231,
-0.30559978281644));
#59847=CARTESIAN_POINT('Ctrl Pts',(-0.544328298014483,0.58888914215781,
-0.310868744589137));
#59848=CARTESIAN_POINT('Ctrl Pts',(-0.434973822423203,0.660865012229132,
-0.316137706361834));
#59849=CARTESIAN_POINT('Ctrl Pts',(-0.325619346831915,0.73284088230046,
-0.321406668134531));
#59850=CARTESIAN_POINT('Ctrl Pts',(-0.19801715610159,0.777092609447604,
-0.326675629907229));
#59851=CARTESIAN_POINT('Ctrl Pts',(-0.0675799010697838,0.788275172467602,
-0.331944591679926));
#59852=CARTESIAN_POINT('Ctrl Pts',(0.0628573539620148,0.799457735487599,
-0.337213553452623));
#59853=CARTESIAN_POINT('Ctrl Pts',(0.196129673295302,0.77757113438045,-0.342482515225321));
#59854=CARTESIAN_POINT('Ctrl Pts',(0.316139530039515,0.725258980018091,
-0.347751476998018));
#59855=CARTESIAN_POINT('Ctrl Pts',(0.436149386783728,0.672946825655733,
-0.353020438770715));
#59856=CARTESIAN_POINT('Ctrl Pts',(0.542896780938876,0.590209118038164,
-0.358289400543412));
#59857=CARTESIAN_POINT('Ctrl Pts',(0.623488044345385,0.487039473884327,
-0.363558362316109));
#59858=CARTESIAN_POINT('Ctrl Pts',(0.704079307751897,0.383869829730486,
-0.368827324088806));
#59859=CARTESIAN_POINT('Ctrl Pts',(0.758514440409767,0.260268249040376,
-0.374096285861504));
#59860=CARTESIAN_POINT('Ctrl Pts',(0.780218400948583,0.131164161930088,
-0.379365247634201));
#59861=CARTESIAN_POINT('Ctrl Pts',(0.801922361487399,0.00206007481979883,
-0.384634209406898));
#59862=CARTESIAN_POINT('Ctrl Pts',(0.79089514990716,-0.132546518710666,
-0.389903171179595));
#59863=CARTESIAN_POINT('Ctrl Pts',(0.748468706969074,-0.256396929090264,
-0.395172132952293));
#59864=CARTESIAN_POINT('Ctrl Pts',(0.70604226403099,-0.380247339469859,
-0.40044109472499));
#59865=CARTESIAN_POINT('Ctrl Pts',(0.632216589735061,-0.493341566698584,
-0.405710056497687));
#59866=CARTESIAN_POINT('Ctrl Pts',(0.535908845492088,-0.582019329472792,
-0.410979018270384));
#59867=CARTESIAN_POINT('Ctrl Pts',(0.439601101249111,-0.670697092247003,
-0.416247980043081));
#59868=CARTESIAN_POINT('Ctrl Pts',(0.320811287059081,-0.734958390566697,
-0.421516941815779));
#59869=CARTESIAN_POINT('Ctrl Pts',(0.19388763551772,-0.767041312675278,
-0.426785903588476));
#59870=CARTESIAN_POINT('Ctrl Pts',(0.0669639839763566,-0.79912423478386,
-0.432054865361174));
#59871=CARTESIAN_POINT('Ctrl Pts',(-0.0680935049163425,-0.799028780681332,
-0.437323827133871));
#59872=CARTESIAN_POINT('Ctrl Pts',(-0.19497167941313,-0.766766479955989,
-0.442592788906568));
#59873=CARTESIAN_POINT('Ctrl Pts',(-0.321849853909913,-0.734504179230648,
-0.447861750679266));
#59874=CARTESIAN_POINT('Ctrl Pts',(-0.440548714010772,-0.670075031882501,
-0.453130712451962));
#59875=CARTESIAN_POINT('Ctrl Pts',(-0.536731013164729,-0.581261223602832,
-0.45839967422466));
#59876=CARTESIAN_POINT('Ctrl Pts',(-0.632913312318683,-0.492447415323166,
-0.463668635997357));
#59877=CARTESIAN_POINT('Ctrl Pts',(-0.706579050525731,-0.379248946111975,
-0.468937597770054));
#59878=CARTESIAN_POINT('Ctrl Pts',(-0.748830384535933,-0.255338688320087,
-0.474206559542751));
#59879=CARTESIAN_POINT('Ctrl Pts',(-0.776790427406901,-0.17334042243865,
-0.477693322753933));
#59880=CARTESIAN_POINT('Ctrl Pts',(-0.790993473291565,-0.0866512497267257,
-0.481180085965114));
#59881=CARTESIAN_POINT('Ctrl Pts',(-0.79106019175573,1.65874934803245E-5,
-0.484666849176295));
#59882=CARTESIAN_POINT('Ctrl Pts',(-0.791054102114328,1.50443135659429E-5,
-0.513133150823704));
#59883=CARTESIAN_POINT('Ctrl Pts',(-0.790996108099315,-0.0839524445160384,
-0.509755100767805));
#59884=CARTESIAN_POINT('Ctrl Pts',(-0.777680141657789,-0.167937895294183,
-0.506377050711907));
#59885=CARTESIAN_POINT('Ctrl Pts',(-0.75140722465577,-0.247652923090808,
-0.502999000656008));
#59886=CARTESIAN_POINT('Ctrl Pts',(-0.710427667499956,-0.37198957507041,
-0.497730038883311));
#59887=CARTESIAN_POINT('Ctrl Pts',(-0.637925604367967,-0.485936866272008,
-0.492461077110613));
#59888=CARTESIAN_POINT('Ctrl Pts',(-0.542658322008323,-0.575731476589062,
-0.487192115337916));
#59889=CARTESIAN_POINT('Ctrl Pts',(-0.447391039648685,-0.665526086906111,
-0.481923153565219));
#59890=CARTESIAN_POINT('Ctrl Pts',(-0.329358538061393,-0.731168016338618,
-0.476654191792522));
#59891=CARTESIAN_POINT('Ctrl Pts',(-0.202817576535695,-0.764728591219457,
-0.471385230019825));
#59892=CARTESIAN_POINT('Ctrl Pts',(-0.0762766150099927,-0.798289166100297,
-0.466116268247127));
#59893=CARTESIAN_POINT('Ctrl Pts',(0.0587728064541182,-0.799768386429468,
-0.46084730647443));
#59894=CARTESIAN_POINT('Ctrl Pts',(0.186018510548951,-0.768987582028121,
-0.455578344701733));
#59895=CARTESIAN_POINT('Ctrl Pts',(0.313264214643783,-0.738206777626774,
-0.450309382929035));
#59896=CARTESIAN_POINT('Ctrl Pts',(0.432706201369339,-0.675165948494908,
-0.445040421156339));
#59897=CARTESIAN_POINT('Ctrl Pts',(0.529917464342802,-0.5874795899134,-0.439771459383641));
#59898=CARTESIAN_POINT('Ctrl Pts',(0.627128727316267,-0.49979323133189,
-0.434502497610944));
#59899=CARTESIAN_POINT('Ctrl Pts',(0.70210926653764,-0.387461343300735,
-0.429233535838246));
#59900=CARTESIAN_POINT('Ctrl Pts',(0.745802428249095,-0.264052126668259,
-0.423964574065549));
#59901=CARTESIAN_POINT('Ctrl Pts',(0.789495589960546,-0.140642910035794,
-0.418695612292852));
#59902=CARTESIAN_POINT('Ctrl Pts',(0.801901374162086,-0.00615636480201949,
-0.413426650520155));
#59903=CARTESIAN_POINT('Ctrl Pts',(0.781521326810997,0.123163319701733,
-0.408157688747459));
#59904=CARTESIAN_POINT('Ctrl Pts',(0.761141279459906,0.252483004205497,
-0.402888726974761));
#59905=CARTESIAN_POINT('Ctrl Pts',(0.707975400556178,0.376635827979229,
-0.397619765202064));
#59906=CARTESIAN_POINT('Ctrl Pts',(0.628445422485195,0.480625778061912,
-0.392350803429367));
#59907=CARTESIAN_POINT('Ctrl Pts',(0.548915444414215,0.584615728144593,
-0.387081841656669));
#59908=CARTESIAN_POINT('Ctrl Pts',(0.443021367175978,0.668442804536227,
-0.381812879883972));
#59909=CARTESIAN_POINT('Ctrl Pts',(0.323553789537451,0.721981809228146,
-0.376543918111275));
#59910=CARTESIAN_POINT('Ctrl Pts',(0.204086211898923,0.775520813920066,
-0.371274956338577));
#59911=CARTESIAN_POINT('Ctrl Pts',(0.0710451338601018,0.798771746912272,
-0.36600599456588));
#59912=CARTESIAN_POINT('Ctrl Pts',(-0.0594998484946793,0.788926204159485,
-0.360737032793183));
#59913=CARTESIAN_POINT('Ctrl Pts',(-0.190044830849464,0.779080661406699,
-0.355468071020486));
#59914=CARTESIAN_POINT('Ctrl Pts',(-0.318093717520211,0.736138642908918,
-0.350199109247788));
#59915=CARTESIAN_POINT('Ctrl Pts',(-0.428179902871407,0.665286974437921,
-0.34493014747509));
#59916=CARTESIAN_POINT('Ctrl Pts',(-0.538266088222596,0.594435305966928,
-0.339661185702393));
#59917=CARTESIAN_POINT('Ctrl Pts',(-0.630389572254237,0.49567398752272,
-0.334392223929696));
#59918=CARTESIAN_POINT('Ctrl Pts',(-0.693423061046085,0.380932075298852,
-0.329123262156999));
#59919=CARTESIAN_POINT('Ctrl Pts',(-0.756456549837934,0.266190163074982,
-0.323854300384302));
#59920=CARTESIAN_POINT('Ctrl Pts',(-0.790400043389989,0.135467657071449,
-0.318585338611605));
#59921=CARTESIAN_POINT('Ctrl Pts',(-0.791153618296685,0.00455410064966138,
-0.313316376838907));
#59922=CARTESIAN_POINT('Ctrl Pts',(-0.791162353384246,0.00303661198591406,
-0.313255301500506));
#59923=CARTESIAN_POINT('Ctrl Pts',(-0.791166628954472,0.00151909765194257,
-0.313194226162105));
#59924=CARTESIAN_POINT('Ctrl Pts',(-0.791166451109383,1.58231152821223E-6,
-0.313133150823703));
#59925=CARTESIAN_POINT('Origin',(0.,0.,-1.97));
#59926=CARTESIAN_POINT('',(-0.791053952037979,-1.51658468628413E-5,-0.0846668491762948));
#59927=CARTESIAN_POINT('',(-0.791061003003137,-1.6759841323199E-5,-0.113133150823703));
#59928=CARTESIAN_POINT('',(-0.7911,-9.68818082805471E-17,-1.97));
#59929=CARTESIAN_POINT('Ctrl Pts',(-0.791053952037979,-1.51658468628413E-5,
-0.0846668491762948));
#59930=CARTESIAN_POINT('Ctrl Pts',(-0.790995158012751,0.0842860903451894,
-0.0880583367537131));
#59931=CARTESIAN_POINT('Ctrl Pts',(-0.777571904683029,0.168605678640689,
-0.0914498243311313));
#59932=CARTESIAN_POINT('Ctrl Pts',(-0.751093386412371,0.248604311213447,
-0.0948413119085496));
#59933=CARTESIAN_POINT('Ctrl Pts',(-0.709956776773963,0.372888928884019,
-0.100110273681247));
#59934=CARTESIAN_POINT('Ctrl Pts',(-0.637309665005789,0.486744383675089,
-0.105379235453944));
#59935=CARTESIAN_POINT('Ctrl Pts',(-0.541928542890219,0.576418288786221,
-0.110648197226642));
#59936=CARTESIAN_POINT('Ctrl Pts',(-0.446547420774654,0.666092193897349,
-0.115917158999339));
#59937=CARTESIAN_POINT('Ctrl Pts',(-0.328432288311695,0.731584549328544,
-0.121186120772036));
#59938=CARTESIAN_POINT('Ctrl Pts',(-0.201849024586547,0.764984829366641,
-0.126455082544733));
#59939=CARTESIAN_POINT('Ctrl Pts',(-0.0752657608613988,0.798385109404738,
-0.131724044317431));
#59940=CARTESIAN_POINT('Ctrl Pts',(0.059785634125941,0.799693314049738,
-0.136993006090128));
#59941=CARTESIAN_POINT('Ctrl Pts',(0.186992304834312,0.768751387957727,
-0.142261967862825));
#59942=CARTESIAN_POINT('Ctrl Pts',(0.314198975542698,0.737809461865712,
-0.147530929635522));
#59943=CARTESIAN_POINT('Ctrl Pts',(0.433560921972116,0.674617405036678,
-0.15279989140822));
#59944=CARTESIAN_POINT('Ctrl Pts',(0.530661030277562,0.586808000298712,
-0.158068853180918));
#59945=CARTESIAN_POINT('Ctrl Pts',(0.627761138582997,0.498998595560756,
-0.163337814953615));
#59946=CARTESIAN_POINT('Ctrl Pts',(0.702599408764469,0.386571842913873,
-0.168606776726312));
#59947=CARTESIAN_POINT('Ctrl Pts',(0.746136256454843,0.263107390736065,
-0.173875738499009));
#59948=CARTESIAN_POINT('Ctrl Pts',(0.789673104145218,0.139642938558253,
-0.179144700271706));
#59949=CARTESIAN_POINT('Ctrl Pts',(0.801908529344493,0.00514078684952503,
-0.184413662044403));
#59950=CARTESIAN_POINT('Ctrl Pts',(0.781364713780323,-0.124152984456936,
-0.1896826238171));
#59951=CARTESIAN_POINT('Ctrl Pts',(0.760820898216154,-0.253446755763393,
-0.194951585589797));
#59952=CARTESIAN_POINT('Ctrl Pts',(0.707497841888538,-0.377532146667576,
-0.200220547362495));
#59953=CARTESIAN_POINT('Ctrl Pts',(0.627836232155951,-0.48142129203795,
-0.205489509135192));
#59954=CARTESIAN_POINT('Ctrl Pts',(0.548174622423359,-0.585310437408331,
-0.210758470907889));
#59955=CARTESIAN_POINT('Ctrl Pts',(0.44217445928579,-0.669003337244903,
-0.216027432680586));
#59956=CARTESIAN_POINT('Ctrl Pts',(0.322639170592942,-0.722390998837629,
-0.221296394453284));
#59957=CARTESIAN_POINT('Ctrl Pts',(0.203103881900095,-0.775778660430356,
-0.226565356225981));
#59958=CARTESIAN_POINT('Ctrl Pts',(0.0700334676519663,-0.798861083779237,
-0.231834317998678));
#59959=CARTESIAN_POINT('Ctrl Pts',(-0.0604989404678671,-0.788850219306804,
-0.237103279771376));
#59960=CARTESIAN_POINT('Ctrl Pts',(-0.191031348587693,-0.778839354834371,
-0.242372241544073));
#59961=CARTESIAN_POINT('Ctrl Pts',(-0.319025750579227,-0.735735202540627,
-0.24764120331677));
#59962=CARTESIAN_POINT('Ctrl Pts',(-0.429022117832896,-0.664744171429373,
-0.252910165089467));
#59963=CARTESIAN_POINT('Ctrl Pts',(-0.539018485086566,-0.593753140318119,
-0.258179126862164));
#59964=CARTESIAN_POINT('Ctrl Pts',(-0.631016817602374,-0.494875230389354,
-0.263448088634861));
#59965=CARTESIAN_POINT('Ctrl Pts',(-0.693904940149093,-0.380053580733699,
-0.268717050407559));
#59966=CARTESIAN_POINT('Ctrl Pts',(-0.756793062695816,-0.265231931078037,
-0.273986012180256));
#59967=CARTESIAN_POINT('Ctrl Pts',(-0.790570975273448,-0.134466541695481,
-0.279254973952954));
#59968=CARTESIAN_POINT('Ctrl Pts',(-0.791158753406913,-0.00355213559091441,
-0.284523935725651));
#59969=CARTESIAN_POINT('Ctrl Pts',(-0.791164067635465,-0.00236851028214306,
-0.284571573542532));
#59970=CARTESIAN_POINT('Ctrl Pts',(-0.791166668783906,-0.0011848727922128,
-0.284619211359413));
#59971=CARTESIAN_POINT('Ctrl Pts',(-0.79116655976261,-1.23482099584349E-6,
-0.284666849176295));
#59972=CARTESIAN_POINT('Ctrl Pts',(-0.791166451109383,1.58231152821223E-6,
-0.313133150823703));
#59973=CARTESIAN_POINT('Ctrl Pts',(-0.791151286281004,-0.129396760162562,
-0.307925264389407));
#59974=CARTESIAN_POINT('Ctrl Pts',(-0.7587555547792,-0.258802420434021,
-0.302717377955112));
#59975=CARTESIAN_POINT('Ctrl Pts',(-0.697762466787314,-0.37292402380272,
-0.297509491520816));
#59976=CARTESIAN_POINT('Ctrl Pts',(-0.636054084109908,-0.488383984993266,
-0.292240529748119));
#59977=CARTESIAN_POINT('Ctrl Pts',(-0.545073662493758,-0.588199300534319,
-0.286971567975422));
#59978=CARTESIAN_POINT('Ctrl Pts',(-0.435810429125493,-0.660313605371724,
-0.281702606202725));
#59979=CARTESIAN_POINT('Ctrl Pts',(-0.326547195757222,-0.732427910209133,
-0.276433644430027));
#59980=CARTESIAN_POINT('Ctrl Pts',(-0.199001150636833,-0.776841204342892,
-0.27116468265733));
#59981=CARTESIAN_POINT('Ctrl Pts',(-0.0685781627465269,-0.78818895144174,
-0.265895720884632));
#59982=CARTESIAN_POINT('Ctrl Pts',(0.0618448251437718,-0.799536698540587,
-0.260626759111935));
#59983=CARTESIAN_POINT('Ctrl Pts',(0.195144755803988,-0.777818898604527,
-0.255357797339238));
#59984=CARTESIAN_POINT('Ctrl Pts',(0.315220767050154,-0.725658773547022,
-0.250088835566541));
#59985=CARTESIAN_POINT('Ctrl Pts',(0.435296778296324,-0.673498648489515,
-0.244819873793844));
#59986=CARTESIAN_POINT('Ctrl Pts',(0.542148870128444,-0.590896198310561,
-0.239550912021147));
#59987=CARTESIAN_POINT('Ctrl Pts',(0.622870728608792,-0.487828702451327,
-0.23428195024845));
#59988=CARTESIAN_POINT('Ctrl Pts',(0.703592587089139,-0.384761206592094,
-0.229012988475753));
#59989=CARTESIAN_POINT('Ctrl Pts',(0.758184212217714,-0.261228665052582,
-0.223744026703055));
#59990=CARTESIAN_POINT('Ctrl Pts',(0.780051659854463,-0.132152168891571,
-0.218475064930358));
#59991=CARTESIAN_POINT('Ctrl Pts',(0.801919107491212,-0.00307567273056075,
-0.21320610315766));
#59992=CARTESIAN_POINT('Ctrl Pts',(0.791062377636135,0.131544778051948,
-0.207937141384963));
#59993=CARTESIAN_POINT('Ctrl Pts',(0.748792820183465,0.255448820028436,
-0.202668179612266));
#59994=CARTESIAN_POINT('Ctrl Pts',(0.706523262730795,0.379352862004923,
-0.197399217839568));
#59995=CARTESIAN_POINT('Ctrl Pts',(0.632840877680532,0.492540495175389,
-0.192130256066871));
#59996=CARTESIAN_POINT('Ctrl Pts',(0.536645516940195,0.581340156202204,
-0.186861294294174));
#59997=CARTESIAN_POINT('Ctrl Pts',(0.440450156199858,0.670139817229018,
-0.181592332521477));
#59998=CARTESIAN_POINT('Ctrl Pts',(0.321741819769446,0.734551506112182,
-0.176323370748779));
#59999=CARTESIAN_POINT('Ctrl Pts',(0.194858902845346,0.766795145591679,
-0.171054408976082));
#60000=CARTESIAN_POINT('Ctrl Pts',(0.0679759859212461,0.799038785071176,
-0.165785447203385));
#60001=CARTESIAN_POINT('Ctrl Pts',(-0.0670815114965426,0.799114375147006,
-0.160516485430688));
#60002=CARTESIAN_POINT('Ctrl Pts',(-0.194000444516933,0.767012786166758,
-0.155247523657991));
#60003=CARTESIAN_POINT('Ctrl Pts',(-0.320919377537324,0.734911197186511,
-0.149978561885293));
#60004=CARTESIAN_POINT('Ctrl Pts',(-0.439699746160317,0.670632429150186,
-0.144709600112596));
#60005=CARTESIAN_POINT('Ctrl Pts',(-0.535994443260468,0.581940502701097,
-0.139440638339899));
#60006=CARTESIAN_POINT('Ctrl Pts',(-0.632289140360619,0.493248576252007,
-0.134171676567201));
#60007=CARTESIAN_POINT('Ctrl Pts',(-0.706098165937928,0.380143491390153,
-0.128902714794504));
#60008=CARTESIAN_POINT('Ctrl Pts',(-0.748506399712542,0.256286843270204,
-0.123633753021807));
#60009=CARTESIAN_POINT('Ctrl Pts',(-0.776678426258576,0.174008180185989,
-0.120133552289106));
#60010=CARTESIAN_POINT('Ctrl Pts',(-0.790993223398756,0.0869848316978164,
-0.116633351556404));
#60011=CARTESIAN_POINT('Ctrl Pts',(-0.791061003003137,-1.6759841323199E-5,
-0.113133150823703));
#60012=CARTESIAN_POINT('Origin',(0.,0.,-4.318617978381));
#60013=CARTESIAN_POINT('',(-0.676660610977248,-1.2972732373197E-5,-0.0186179783810009));
#60014=CARTESIAN_POINT('',(-0.6767,-7.33509820392354E-14,0.));
#60015=CARTESIAN_POINT('',(-0.6767,-7.33509820392354E-14,-4.318617978381));
#60016=CARTESIAN_POINT('',(-0.564209944071419,-0.373617490236908,0.));
#60017=CARTESIAN_POINT('Ctrl Pts',(-0.676660610977247,-1.2972732373228E-5,
-0.0186179783810009));
#60018=CARTESIAN_POINT('Ctrl Pts',(-0.676688451778648,-0.0399322421209059,
-0.0167405041857218));
#60019=CARTESIAN_POINT('Ctrl Pts',(-0.66520014873097,-0.171869541427616,
-0.0105345113920551));
#60020=CARTESIAN_POINT('Ctrl Pts',(-0.614942795555724,-0.296874006669216,
-0.00432851859838854));
#60021=CARTESIAN_POINT('Ctrl Pts',(-0.56421801023762,-0.373640954068593,
-1.08756319922021E-15));
#60022=CARTESIAN_POINT('Origin',(0.,0.,0.));
#60023=CARTESIAN_POINT('Origin',(0.,0.,-4.318617978381));
#60024=CARTESIAN_POINT('',(-0.676756934637034,-1.05625507715145E-6,-0.218617978381));
#60025=CARTESIAN_POINT('',(-0.676666642310989,-1.43362213473885E-5,-0.179182021618993));
#60026=CARTESIAN_POINT('',(-0.6767,-7.33509820392354E-14,-4.318617978381));
#60027=CARTESIAN_POINT('Ctrl Pts',(-0.676756934637034,-1.05625507717112E-6,
-0.218617978381));
#60028=CARTESIAN_POINT('Ctrl Pts',(-0.676757027892895,-0.00101352979207305,
-0.218570340564119));
#60029=CARTESIAN_POINT('Ctrl Pts',(-0.676508707702974,-0.114010189902111,
-0.21325374097454));
#60030=CARTESIAN_POINT('Ctrl Pts',(-0.618460816691914,-0.338732633997832,
-0.202668179612265));
#60031=CARTESIAN_POINT('Ctrl Pts',(-0.382377116982208,-0.592470524209418,
-0.186861294294173));
#60032=CARTESIAN_POINT('Ctrl Pts',(-0.0539212511207285,-0.703083265419793,
-0.171054408976082));
#60033=CARTESIAN_POINT('Ctrl Pts',(0.287560543804209,-0.643849758100151,
-0.155247523657989));
#60034=CARTESIAN_POINT('Ctrl Pts',(0.559575372758286,-0.429079241151316,
-0.139440638339898));
#60035=CARTESIAN_POINT('Ctrl Pts',(0.696411596561459,-0.110654576665681,
-0.123633753021806));
#60036=CARTESIAN_POINT('Ctrl Pts',(0.665013370424364,0.234501305250519,
-0.107826867703715));
#60037=CARTESIAN_POINT('Ctrl Pts',(0.472965371062188,0.523007879069813,
-0.0920199823856229));
#60038=CARTESIAN_POINT('Ctrl Pts',(0.166661885477124,0.685169672229466,
-0.076213097067531));
#60039=CARTESIAN_POINT('Ctrl Pts',(-0.179903450085766,0.681812591898513,
-0.0604062117494397));
#60040=CARTESIAN_POINT('Ctrl Pts',(-0.483007394483508,0.513747833004724,
-0.0445993264313473));
#60041=CARTESIAN_POINT('Ctrl Pts',(-0.647289724438253,0.256278004736498,
-0.0306699153085348));
#60042=CARTESIAN_POINT('Ctrl Pts',(-0.676610319083845,0.0720975822735199,
-0.0220094659584191));
#60043=CARTESIAN_POINT('Ctrl Pts',(-0.676660610977247,-1.2972732373228E-5,
-0.0186179783810009));
#60044=CARTESIAN_POINT('',(-0.537060862935905,0.411689834101525,0.));
#60045=CARTESIAN_POINT('Origin',(0.,0.,0.));
#60046=CARTESIAN_POINT('Ctrl Pts',(-0.676666642310989,-1.43362213474128E-5,
-0.179182021618993));
#60047=CARTESIAN_POINT('Ctrl Pts',(-0.676695940449894,-0.0376212939135734,
-0.177413260578998));
#60048=CARTESIAN_POINT('Ctrl Pts',(-0.664430133622077,-0.187236698051038,
-0.170375537766307));
#60049=CARTESIAN_POINT('Ctrl Pts',(-0.555635984344507,-0.434168324449232,
-0.158068853180918));
#60050=CARTESIAN_POINT('Ctrl Pts',(-0.281672681898704,-0.646447338792661,
-0.142261967862826));
#60051=CARTESIAN_POINT('Ctrl Pts',(0.0603360297254143,-0.702561900375898,
-0.126455082544735));
#60052=CARTESIAN_POINT('Ctrl Pts',(0.38776765641086,-0.588956040974949,
-0.110648197226643));
#60053=CARTESIAN_POINT('Ctrl Pts',(0.621527851581432,-0.333074272139639,
-0.0948413119085513));
#60054=CARTESIAN_POINT('Ctrl Pts',(0.705137669332003,0.00326985369309036,
-0.0790344265904595));
#60055=CARTESIAN_POINT('Ctrl Pts',(0.618416201049889,0.338823176482188,
-0.0632275412723679));
#60056=CARTESIAN_POINT('Ctrl Pts',(0.38227975109817,0.59252757256583,-0.0474206559542765));
#60057=CARTESIAN_POINT('Ctrl Pts',(0.0538381161213402,0.703089501623881,
-0.0316137706361843));
#60058=CARTESIAN_POINT('Ctrl Pts',(-0.287697821498663,0.643811669165333,
-0.015806885318092));
#60059=CARTESIAN_POINT('Ctrl Pts',(-0.468914126304642,0.500589151378386,
-0.00526896177269799));
#60060=CARTESIAN_POINT('Ctrl Pts',(-0.537060862935893,0.41168983410154,
-8.88178419700125E-16));
#60061=CARTESIAN_POINT('Origin',(0.,0.,-4.318617978381));
#60062=CARTESIAN_POINT('',(-0.676665948377073,1.41887963584822E-5,-0.418617978380999));
#60063=CARTESIAN_POINT('',(-0.676756841696018,1.35349531268708E-6,-0.379182021618994));
#60064=CARTESIAN_POINT('',(-0.6767,-7.33509820392354E-14,-4.318617978381));
#60065=CARTESIAN_POINT('Ctrl Pts',(-0.676665948377073,1.41887963584705E-5,
-0.418617978380999));
#60066=CARTESIAN_POINT('Ctrl Pts',(-0.676608877988115,-0.0741207188599466,
-0.415131215169819));
#60067=CARTESIAN_POINT('Ctrl Pts',(-0.646100723357651,-0.260329135516356,
-0.406375490185941));
#60068=CARTESIAN_POINT('Ctrl Pts',(-0.478375468842551,-0.518064176544559,
-0.392350803429365));
#60069=CARTESIAN_POINT('Ctrl Pts',(-0.173773577942818,-0.683400558836909,
-0.376543918111274));
#60070=CARTESIAN_POINT('Ctrl Pts',(0.172807395639615,-0.68364551064267,
-0.360737032793182));
#60071=CARTESIAN_POINT('Ctrl Pts',(0.477642690529216,-0.518739858109735,
-0.34493014747509));
#60072=CARTESIAN_POINT('Ctrl Pts',(0.667092192979181,-0.228520428584966,
-0.329123262156999));
#60073=CARTESIAN_POINT('Ctrl Pts',(0.695389933124598,0.11690346918548,-0.313316376838907));
#60074=CARTESIAN_POINT('Ctrl Pts',(0.555699928310104,0.434086592632565,
-0.297509491520815));
#60075=CARTESIAN_POINT('Ctrl Pts',(0.281767574784161,0.646405920447539,
-0.281702606202724));
#60076=CARTESIAN_POINT('Ctrl Pts',(-0.0602323436566084,0.702570740201827,
-0.265895720884633));
#60077=CARTESIAN_POINT('Ctrl Pts',(-0.387681727301688,0.589013122604281,
-0.25008883556654));
#60078=CARTESIAN_POINT('Ctrl Pts',(-0.62077289895915,0.333936630716867,
-0.23432958806533));
#60079=CARTESIAN_POINT('Ctrl Pts',(-0.676746713365588,0.110970702727291,
-0.223839302336816));
#60080=CARTESIAN_POINT('Ctrl Pts',(-0.676756934637034,-1.05625507717112E-6,
-0.218617978381));
#60081=CARTESIAN_POINT('Ctrl Pts',(-0.676756841696018,1.35349531267905E-6,
-0.379182021618994));
#60082=CARTESIAN_POINT('Ctrl Pts',(-0.676743869834842,-0.11068485349773,
-0.373974135184699));
#60083=CARTESIAN_POINT('Ctrl Pts',(-0.620996840527473,-0.333367929361865,
-0.363497286977708));
#60084=CARTESIAN_POINT('Ctrl Pts',(-0.388427374670541,-0.588521666917222,
-0.347751476998018));
#60085=CARTESIAN_POINT('Ctrl Pts',(-0.0611220704120482,-0.702493893463718,
-0.331944591679926));
#60086=CARTESIAN_POINT('Ctrl Pts',(0.280948703489239,-0.646762246832194,
-0.316137706361835));
#60087=CARTESIAN_POINT('Ctrl Pts',(0.555149729438401,-0.434790013096512,
-0.300330821043743));
#60088=CARTESIAN_POINT('Ctrl Pts',(0.695241321112673,-0.117784056100728,
-0.284523935725652));
#60089=CARTESIAN_POINT('Ctrl Pts',(0.667381066683655,0.227675401785218,
-0.268717050407559));
#60090=CARTESIAN_POINT('Ctrl Pts',(0.47829926932486,0.518134527179428,-0.252910165089469));
#60091=CARTESIAN_POINT('Ctrl Pts',(0.173673060517654,0.683426108018395,
-0.237103279771376));
#60092=CARTESIAN_POINT('Ctrl Pts',(-0.172907934941646,0.683620085281621,
-0.221296394453285));
#60093=CARTESIAN_POINT('Ctrl Pts',(-0.477718990865722,0.518669602421621,
-0.205489509135192));
#60094=CARTESIAN_POINT('Ctrl Pts',(-0.645931503859681,0.260900441967383,
-0.191451384857095));
#60095=CARTESIAN_POINT('Ctrl Pts',(-0.676608664232016,0.0744060619515273,
-0.182682222351695));
#60096=CARTESIAN_POINT('Ctrl Pts',(-0.676666642310989,-1.43362213474128E-5,
-0.179182021618993));
#60097=CARTESIAN_POINT('Origin',(0.,0.,-4.318617978381));
#60098=CARTESIAN_POINT('',(-0.676672603166279,-1.54393518830496E-5,-0.618617978381001));
#60099=CARTESIAN_POINT('',(-0.676660739351239,1.28687737398769E-5,-0.579182021618993));
#60100=CARTESIAN_POINT('',(-0.6767,-7.33509820392354E-14,-4.318617978381));
#60101=CARTESIAN_POINT('Ctrl Pts',(-0.676672603166279,-1.54393518830773E-5,
-0.618617978381001));
#60102=CARTESIAN_POINT('Ctrl Pts',(-0.676702544117346,-0.0352437141061704,
-0.616961051548217));
#60103=CARTESIAN_POINT('Ctrl Pts',(-0.665401738435777,-0.182477482807531,
-0.610035162942737));
#60104=CARTESIAN_POINT('Ctrl Pts',(-0.560181318740991,-0.428287835856923,
-0.597840312564558));
#60105=CARTESIAN_POINT('Ctrl Pts',(-0.288470365174735,-0.643442638177916,
-0.582033427246467));
#60106=CARTESIAN_POINT('Ctrl Pts',(0.0529273696266406,-0.703158782746691,
-0.566226541928374));
#60107=CARTESIAN_POINT('Ctrl Pts',(0.381539257166764,-0.593010434520368,
-0.550419656610283));
#60108=CARTESIAN_POINT('Ctrl Pts',(0.617981390178772,-0.339606509952495,
-0.534612771292191));
#60109=CARTESIAN_POINT('Ctrl Pts',(0.70513562694994,-0.00416266925407728,
-0.518805885974099));
#60110=CARTESIAN_POINT('Ctrl Pts',(0.621947817852421,0.33228676181577,-0.502999000656008));
#60111=CARTESIAN_POINT('Ctrl Pts',(0.388513928898186,0.588464533562985,
-0.487192115337916));
#60112=CARTESIAN_POINT('Ctrl Pts',(0.0612253899055303,0.702484897944656,
-0.471385230019824));
#60113=CARTESIAN_POINT('Ctrl Pts',(-0.280853577732319,0.646803562207529,
-0.455578344701733));
#60114=CARTESIAN_POINT('Ctrl Pts',(-0.555085777752791,0.434871658706356,
-0.439771459383642));
#60115=CARTESIAN_POINT('Ctrl Pts',(-0.664311591163683,0.187808550285201,
-0.42745133727673));
#60116=CARTESIAN_POINT('Ctrl Pts',(-0.676695118916897,0.037906961485815,
-0.420400176942516));
#60117=CARTESIAN_POINT('Ctrl Pts',(-0.676665948377073,1.41887963584705E-5,
-0.418617978380999));
#60118=CARTESIAN_POINT('Ctrl Pts',(-0.676660739351239,1.28687737398527E-5,
-0.579182021618993));
#60119=CARTESIAN_POINT('Ctrl Pts',(-0.676611131779544,-0.0718121845582891,
-0.575803971563096));
#60120=CARTESIAN_POINT('Ctrl Pts',(-0.647454493003157,-0.255706719105382,
-0.567156959734502));
#60121=CARTESIAN_POINT('Ctrl Pts',(-0.483658336941455,-0.513135645762089,
-0.55324098613321));
#60122=CARTESIAN_POINT('Ctrl Pts',(-0.18076643772218,-0.681584237521583,
-0.537434100815119));
#60123=CARTESIAN_POINT('Ctrl Pts',(0.165793833437332,-0.685380173800492,
-0.521627215497027));
#60124=CARTESIAN_POINT('Ctrl Pts',(0.47230271632388,-0.523606457177304,
-0.505820330178935));
#60125=CARTESIAN_POINT('Ctrl Pts',(0.66471580275202,-0.235343322438281,
-0.490013444860844));
#60126=CARTESIAN_POINT('Ctrl Pts',(0.696551199677241,0.109772510552645,
-0.474206559542751));
#60127=CARTESIAN_POINT('Ctrl Pts',(0.560118320442681,0.428370219493409,
-0.458399674224661));
#60128=CARTESIAN_POINT('Ctrl Pts',(0.288375726331517,0.643485056786609,
-0.442592788906568));
#60129=CARTESIAN_POINT('Ctrl Pts',(-0.0530307867851691,0.703150989118139,
-0.426785903588478));
#60130=CARTESIAN_POINT('Ctrl Pts',(-0.381626469796513,0.59295431138796,
-0.410979018270385));
#60131=CARTESIAN_POINT('Ctrl Pts',(-0.618031330032434,0.339515615175607,
-0.395172132952294));
#60132=CARTESIAN_POINT('Ctrl Pts',(-0.67643782299757,0.114581693286516,
-0.384573134068496));
#60133=CARTESIAN_POINT('Ctrl Pts',(-0.676756993823146,0.00129942280498109,
-0.379243096957396));
#60134=CARTESIAN_POINT('Ctrl Pts',(-0.676756841696018,1.35349531267905E-6,
-0.379182021618994));
#60135=CARTESIAN_POINT('Origin',(0.,0.,-4.318617978381));
#60136=CARTESIAN_POINT('',(-0.676755273642671,3.79787743738244E-6,-0.818617978381));
#60137=CARTESIAN_POINT('',(-0.676678866911972,-1.62676655498795E-5,-0.779182021618994));
#60138=CARTESIAN_POINT('',(-0.6767,-7.33509820392354E-14,-4.318617978381));
#60139=CARTESIAN_POINT('Ctrl Pts',(-0.676755273642671,3.797877437383E-6,
-0.818617978381));
#60140=CARTESIAN_POINT('Ctrl Pts',(-0.676721587681226,-0.108306264839717,
-0.813521926153917));
#60141=CARTESIAN_POINT('Ctrl Pts',(-0.622843396402541,-0.328633681308047,
-0.803156912154136));
#60142=CARTESIAN_POINT('Ctrl Pts',(-0.394608777314782,-0.584394980364765,
-0.787522936381659));
#60143=CARTESIAN_POINT('Ctrl Pts',(-0.0685229122472805,-0.701810651605228,
-0.771716051063567));
#60144=CARTESIAN_POINT('Ctrl Pts',(0.274116269111402,-0.649687502741008,
-0.755909165745476));
#60145=CARTESIAN_POINT('Ctrl Pts',(0.550536237737494,-0.440617102649509,
-0.740102280427383));
#60146=CARTESIAN_POINT('Ctrl Pts',(0.6939612682597,-0.125105309099136,-0.724295395109291));
#60147=CARTESIAN_POINT('Ctrl Pts',(0.669743681289579,0.220628605539007,
-0.7084885097912));
#60148=CARTESIAN_POINT('Ctrl Pts',(0.483733802853534,0.513064506847101,
-0.692681624473108));
#60149=CARTESIAN_POINT('Ctrl Pts',(0.180866680953096,0.681557645346608,
-0.676874739155017));
#60150=CARTESIAN_POINT('Ctrl Pts',(-0.165693028990715,0.685404552328976,
-0.661067853836925));
#60151=CARTESIAN_POINT('Ctrl Pts',(-0.47222570233939,0.523675917204019,
-0.645260968518833));
#60152=CARTESIAN_POINT('Ctrl Pts',(-0.644507402220349,0.265654755031154,
-0.631111010033525));
#60153=CARTESIAN_POINT('Ctrl Pts',(-0.676607333077552,0.0767808058218464,
-0.622230013320914));
#60154=CARTESIAN_POINT('Ctrl Pts',(-0.676672603166279,-1.54393518830773E-5,
-0.618617978381001));
#60155=CARTESIAN_POINT('Ctrl Pts',(-0.676678866911972,-1.62676655498725E-5,
-0.779182021618994));
#60156=CARTESIAN_POINT('Ctrl Pts',(-0.676708771665283,-0.0329322939036839,
-0.777633807941494));
#60157=CARTESIAN_POINT('Ctrl Pts',(-0.666320931935935,-0.177851150494438,
-0.770816632491298));
#60158=CARTESIAN_POINT('Ctrl Pts',(-0.564540062783472,-0.422525851702685,
-0.758730495268403));
#60159=CARTESIAN_POINT('Ctrl Pts',(-0.295047803669792,-0.640453254651953,
-0.742923609950312));
#60160=CARTESIAN_POINT('Ctrl Pts',(0.045720171186077,-0.703664155539672,
-0.727116724632219));
#60161=CARTESIAN_POINT('Ctrl Pts',(0.375443366570243,-0.596888478983344,
-0.711309839314129));
#60162=CARTESIAN_POINT('Ctrl Pts',(0.614469412746345,-0.345920393506668,
-0.695502953996035));
#60163=CARTESIAN_POINT('Ctrl Pts',(0.705055963185025,-0.0113871252686242,
-0.679696068677945));
#60164=CARTESIAN_POINT('Ctrl Pts',(0.625319712405524,0.325896970102082,
-0.663889183359852));
#60165=CARTESIAN_POINT('Ctrl Pts',(0.394522821570273,0.584453010176933,
-0.648082298041761));
#60166=CARTESIAN_POINT('Ctrl Pts',(0.0684196917652833,0.701820720428935,
-0.632275412723669));
#60167=CARTESIAN_POINT('Ctrl Pts',(-0.274211819002972,0.649647178215781,
-0.616468527405578));
#60168=CARTESIAN_POINT('Ctrl Pts',(-0.550601034721718,0.440536126110014,
-0.600661642087486));
#60169=CARTESIAN_POINT('Ctrl Pts',(-0.663338570721139,0.192434988319684,
-0.588232806825291));
#60170=CARTESIAN_POINT('Ctrl Pts',(-0.676688507897296,0.0402179671760706,
-0.581072933335794));
#60171=CARTESIAN_POINT('Ctrl Pts',(-0.676660739351239,1.28687737398527E-5,
-0.579182021618993));
#60172=CARTESIAN_POINT('Origin',(0.,0.,-4.318617978381));
#60173=CARTESIAN_POINT('',(-0.676656001156398,1.13078348284983E-5,-1.018617978381));
#60174=CARTESIAN_POINT('',(-0.676752484899457,6.08590203556372E-6,-0.979182021618994));
#60175=CARTESIAN_POINT('',(-0.6767,-7.33509820392354E-14,-4.318617978381));
#60176=CARTESIAN_POINT('Ctrl Pts',(-0.676656001156398,1.13078348284897E-5,
-1.018617978381));
#60177=CARTESIAN_POINT('Ctrl Pts',(-0.67661425195553,-0.0694372891457709,
-1.01535176253231));
#60178=CARTESIAN_POINT('Ctrl Pts',(-0.648819209846495,-0.250950949327346,
-1.00681658491093));
#60179=CARTESIAN_POINT('Ctrl Pts',(-0.489039886595606,-0.508009418739415,
-0.99301244551685));
#60180=CARTESIAN_POINT('Ctrl Pts',(-0.187940247738363,-0.67964111374272,
-0.977205560198759));
#60181=CARTESIAN_POINT('Ctrl Pts',(0.158560765091847,-0.687089560379787,
-0.961398674880666));
#60182=CARTESIAN_POINT('Ctrl Pts',(0.466757706920742,-0.528555411702021,
-0.945591789562577));
#60183=CARTESIAN_POINT('Ctrl Pts',(0.662198379341202,-0.242336308891769,
-0.929784904244484));
#60184=CARTESIAN_POINT('Ctrl Pts',(0.697669504916014,0.102424812031291,
-0.913978018926392));
#60185=CARTESIAN_POINT('Ctrl Pts',(0.564602201477338,0.422442817782887,
-0.898171133608301));
#60186=CARTESIAN_POINT('Ctrl Pts',(0.295141996551584,0.640409854765639,
-0.882364248290208));
#60187=CARTESIAN_POINT('Ctrl Pts',(-0.0456166786157439,0.703670873947096,
-0.866557362972117));
#60188=CARTESIAN_POINT('Ctrl Pts',(-0.375355575368597,0.596943692695645,
-0.850750477654026));
#60189=CARTESIAN_POINT('Ctrl Pts',(-0.614418530936816,0.346010764356899,
-0.834943592335933));
#60190=CARTESIAN_POINT('Ctrl Pts',(-0.6758338184604,0.119338197594593,-0.824232759244925));
#60191=CARTESIAN_POINT('Ctrl Pts',(-0.676756416610606,0.00367876879518259,
-0.818790887926614));
#60192=CARTESIAN_POINT('Ctrl Pts',(-0.676755273642671,3.797877437383E-6,
-0.818617978381));
#60193=CARTESIAN_POINT('Ctrl Pts',(-0.676752484899457,6.08590203554811E-6,
-0.979182021618994));
#60194=CARTESIAN_POINT('Ctrl Pts',(-0.67670218702431,-0.10599468821923,
-0.974194682547194));
#60195=CARTESIAN_POINT('Ctrl Pts',(-0.624609057349418,-0.324029546701264,
-0.963938381702699));
#60196=CARTESIAN_POINT('Ctrl Pts',(-0.400575654252081,-0.580321224034726,
-0.948413119085501));
#60197=CARTESIAN_POINT('Ctrl Pts',(-0.07570992285693,-0.701071740569853,
-0.932606233767413));
#60198=CARTESIAN_POINT('Ctrl Pts',(0.267445315774999,-0.652461938288095,
-0.916799348449319));
#60199=CARTESIAN_POINT('Ctrl Pts',(0.545992866884217,-0.446234654813134,
-0.900992463131228));
#60200=CARTESIAN_POINT('Ctrl Pts',(0.69264303765959,-0.132208926424586,
-0.885185577813137));
#60201=CARTESIAN_POINT('Ctrl Pts',(0.671969040456129,0.213754968393986,
-0.869378692495044));
#60202=CARTESIAN_POINT('Ctrl Pts',(0.488965164096191,0.508081338119234,
-0.853571807176953));
#60203=CARTESIAN_POINT('Ctrl Pts',(0.187840286290136,0.679668746295639,
-0.837764921858861));
#60204=CARTESIAN_POINT('Ctrl Pts',(-0.158661817457009,0.687066230814675,
-0.821958036540769));
#60205=CARTESIAN_POINT('Ctrl Pts',(-0.466835438634391,0.528486755822397,
-0.806151151222678));
#60206=CARTESIAN_POINT('Ctrl Pts',(-0.64309559662951,0.270275607400248,
-0.791892479582085));
#60207=CARTESIAN_POINT('Ctrl Pts',(-0.67660699824453,0.0790892483926756,
-0.782902769714191));
#60208=CARTESIAN_POINT('Ctrl Pts',(-0.676678866911972,-1.62676655498725E-5,
-0.779182021618994));
#60209=CARTESIAN_POINT('Origin',(0.,0.,-4.318617978381));
#60210=CARTESIAN_POINT('',(-0.676685704046724,-1.6852225544519E-5,-1.218617978381));
#60211=CARTESIAN_POINT('',(-0.676652044953461,9.61824139306122E-6,-1.17918202161899));
#60212=CARTESIAN_POINT('',(-0.6767,-7.33509820392354E-14,-4.318617978381));
#60213=CARTESIAN_POINT('Ctrl Pts',(-0.676685704046724,-1.68522255445426E-5,
-1.218617978381));
#60214=CARTESIAN_POINT('Ctrl Pts',(-0.676714928392431,-0.0305543246826664,
-1.21718159891071));
#60215=CARTESIAN_POINT('Ctrl Pts',(-0.667240586817943,-0.173092095040201,
-1.21047625766773));
#60216=CARTESIAN_POINT('Ctrl Pts',(-0.568962098984759,-0.416552169755792,
-1.19850195465204));
#60217=CARTESIAN_POINT('Ctrl Pts',(-0.301781748310929,-0.637307897798075,
-1.18269506933395));
#60218=CARTESIAN_POINT('Ctrl Pts',(0.0383010603417563,-0.704106958484362,
-1.16688818401586));
#60219=CARTESIAN_POINT('Ctrl Pts',(0.369131349722688,-0.600812472291737,
-1.15108129869777));
#60220=CARTESIAN_POINT('Ctrl Pts',(0.610789305579622,-0.352377644578884,
-1.13527441337968));
#60221=CARTESIAN_POINT('Ctrl Pts',(0.704896781882463,-0.0188177336879362,
-1.11946752806159));
#60222=CARTESIAN_POINT('Ctrl Pts',(0.628719910943502,0.319288042044476,
-1.10366064274349));
#60223=CARTESIAN_POINT('Ctrl Pts',(0.4006610022585,0.580262304030356,-1.0878537574254));
#60224=CARTESIAN_POINT('Ctrl Pts',(0.0758130331203709,0.701060599533658,
-1.07204687210731));
#60225=CARTESIAN_POINT('Ctrl Pts',(-0.267349351956566,0.65250126759862,
-1.05623998678922));
#60226=CARTESIAN_POINT('Ctrl Pts',(-0.545927231821457,0.446314953553164,
-1.04043310147113));
#60227=CARTESIAN_POINT('Ctrl Pts',(-0.662311355964471,0.197194252937781,
-1.02789243200172));
#60228=CARTESIAN_POINT('Ctrl Pts',(-0.676681600518395,0.04259511153144,
-1.02062072430501));
#60229=CARTESIAN_POINT('Ctrl Pts',(-0.676656001156398,1.13078348284897E-5,
-1.018617978381));
#60230=CARTESIAN_POINT('Ctrl Pts',(-0.676652044953461,9.61824139304387E-6,
-1.17918202161899));
#60231=CARTESIAN_POINT('Ctrl Pts',(-0.676617978265195,-0.0671285662727804,
-1.17602451892559));
#60232=CARTESIAN_POINT('Ctrl Pts',(-0.650118825411559,-0.24632733355921,
-1.16759805445949));
#60233=CARTESIAN_POINT('Ctrl Pts',(-0.494219175919373,-0.502972150320693,
-1.15390262822069));
#60234=CARTESIAN_POINT('Ctrl Pts',(-0.194893845382005,-0.677679840984561,
-1.1380957429026));
#60235=CARTESIAN_POINT('Ctrl Pts',(0.15151266369854,-0.688678074708074,
-1.12228885758451));
#60236=CARTESIAN_POINT('Ctrl Pts',(0.461317735944786,-0.533309970230656,
-1.10648197226642));
#60237=CARTESIAN_POINT('Ctrl Pts',(0.659680691337217,-0.249108336515458,
-1.09067508694833));
#60238=CARTESIAN_POINT('Ctrl Pts',(0.698682306460244,0.0952712573866783,
-1.07486820163024));
#60239=CARTESIAN_POINT('Ctrl Pts',(0.568900826606944,0.41663584499006,-1.05906131631215));
#60240=CARTESIAN_POINT('Ctrl Pts',(0.301688011565286,0.637352274274148,
-1.04325443099405));
#60241=CARTESIAN_POINT('Ctrl Pts',(-0.0384046171462246,0.704101316023837,
-1.02744754567596));
#60242=CARTESIAN_POINT('Ctrl Pts',(-0.369219710011492,0.600758173963263,
-1.01164066035787));
#60243=CARTESIAN_POINT('Ctrl Pts',(-0.610841123852988,0.352287807416983,
-0.99583377503978));
#60244=CARTESIAN_POINT('Ctrl Pts',(-0.675222522545463,0.123962206612681,
-0.985014228793486));
#60245=CARTESIAN_POINT('Ctrl Pts',(-0.676755325096052,0.00599168741729094,
-0.979463644319891));
#60246=CARTESIAN_POINT('Ctrl Pts',(-0.676752484899457,6.08590203554811E-6,
-0.979182021618994));
#60247=CARTESIAN_POINT('Origin',(0.,0.,-4.318617978381));
#60248=CARTESIAN_POINT('',(-0.676748500489657,8.29977222931769E-6,-1.418617978381));
#60249=CARTESIAN_POINT('',(-0.676692639524177,-1.71467829109539E-5,-1.37918202161899));
#60250=CARTESIAN_POINT('',(-0.6767,-7.33509820392354E-14,-4.318617978381));
#60251=CARTESIAN_POINT('Ctrl Pts',(-0.676748500489657,8.29977222930288E-6,
-1.418617978381));
#60252=CARTESIAN_POINT('Ctrl Pts',(-0.676684450593901,-0.103617326982464,
-1.41374247351641));
#60253=CARTESIAN_POINT('Ctrl Pts',(-0.626395365481128,-0.319291283088945,
-1.40359800687913));
#60254=CARTESIAN_POINT('Ctrl Pts',(-0.406669950001241,-0.576066950948749,
-1.38818457846914));
#60255=CARTESIAN_POINT('Ctrl Pts',(-0.0830949650860008,-0.700234822746455,
-1.37237769315105));
#60256=CARTESIAN_POINT('Ctrl Pts',(0.260553557193054,-0.655244552852938,
-1.35657080783296));
#60257=CARTESIAN_POINT('Ctrl Pts',(0.541259257844153,-0.451964595966764,
-1.34076392251487));
#60258=CARTESIAN_POINT('Ctrl Pts',(0.69121109242647,-0.13950199251626,-1.32495703719678));
#60259=CARTESIAN_POINT('Ctrl Pts',(0.67418467897962,0.206660588498508,-1.30915015187868));
#60260=CARTESIAN_POINT('Ctrl Pts',(0.494293146935006,0.50289945824438,-1.29334326656059));
#60261=CARTESIAN_POINT('Ctrl Pts',(0.194993514250268,0.677651171038411,
-1.2775363812425));
#60262=CARTESIAN_POINT('Ctrl Pts',(-0.151411374329973,0.688700352789885,
-1.26172949592441));
#60263=CARTESIAN_POINT('Ctrl Pts',(-0.461239294898093,0.533377814547353,
-1.24592261060632));
#60264=CARTESIAN_POINT('Ctrl Pts',(-0.641614910060592,0.275028249089165,
-1.23155210475852));
#60265=CARTESIAN_POINT('Ctrl Pts',(-0.676607726943547,0.0814639673770342,
-1.22245056068341));
#60266=CARTESIAN_POINT('Ctrl Pts',(-0.676685704046724,-1.68522255445426E-5,
-1.218617978381));
#60267=CARTESIAN_POINT('Ctrl Pts',(-0.676692639524176,-1.71467829109401E-5,
-1.37918202161899));
#60268=CARTESIAN_POINT('Ctrl Pts',(-0.676720625649769,-0.0282425422486149,
-1.37785435530399));
#60269=CARTESIAN_POINT('Ctrl Pts',(-0.668109463888461,-0.168465967902817,
-1.37125772721629));
#60270=CARTESIAN_POINT('Ctrl Pts',(-0.573200140887612,-0.410700835561685,
-1.35939213735589));
#60271=CARTESIAN_POINT('Ctrl Pts',(-0.308295632778683,-0.634182450604112,
-1.3435852520378));
#60272=CARTESIAN_POINT('Ctrl Pts',(0.0310849148505515,-0.704462423350869,
-1.3277783667197));
#60273=CARTESIAN_POINT('Ctrl Pts',(0.362956172367475,-0.604562978344687,
-1.31197148140161));
#60274=CARTESIAN_POINT('Ctrl Pts',(0.607146855256262,-0.358617169133155,
-1.29616459608352));
#60275=CARTESIAN_POINT('Ctrl Pts',(0.704666977880717,-0.026038973272816,
-1.28035771076543));
#60276=CARTESIAN_POINT('Ctrl Pts',(0.631958267808816,0.312829547186207,
-1.26455082544734));
#60277=CARTESIAN_POINT('Ctrl Pts',(0.40658521895174,0.57612675478111,-1.24874394012925));
#60278=CARTESIAN_POINT('Ctrl Pts',(0.0829919761785184,0.700247034791744,
-1.23293705481115));
#60279=CARTESIAN_POINT('Ctrl Pts',(-0.26064992457286,0.655206223005252,
-1.21713016949306));
#60280=CARTESIAN_POINT('Ctrl Pts',(-0.541325723895911,0.45188498369963,
-1.20132328417497));
#60281=CARTESIAN_POINT('Ctrl Pts',(-0.661287168256255,0.201820668754294,
-1.18867390155028));
#60282=CARTESIAN_POINT('Ctrl Pts',(-0.676674825747406,0.0449057095593861,
-1.18129348069829));
#60283=CARTESIAN_POINT('Ctrl Pts',(-0.676652044953461,9.61824139304387E-6,
-1.17918202161899));
#60284=CARTESIAN_POINT('Origin',(0.,0.,-4.318617978381));
#60285=CARTESIAN_POINT('',(-0.67664869645179,7.73109616231909E-6,-1.618617978381));
#60286=CARTESIAN_POINT('',(-0.67674370184345,1.02755109431876E-5,-1.57918202161899));
#60287=CARTESIAN_POINT('',(-0.6767,-7.33509820392354E-14,-4.318617978381));
#60288=CARTESIAN_POINT('Ctrl Pts',(-0.67664869645179,7.73109616233197E-6,
-1.618617978381));
#60289=CARTESIAN_POINT('Ctrl Pts',(-0.676622450612112,-0.0647534336386639,
-1.61557230989481));
#60290=CARTESIAN_POINT('Ctrl Pts',(-0.651428100979576,-0.241570457659696,
-1.60725767963592));
#60291=CARTESIAN_POINT('Ctrl Pts',(-0.499493016443407,-0.497735177311859,
-1.59367408760434));
#60292=CARTESIAN_POINT('Ctrl Pts',(-0.202025718633698,-0.67558803217637,
-1.57786720228624));
#60293=CARTESIAN_POINT('Ctrl Pts',(0.144245628943018,-0.690236755570315,
-1.56206031696815));
#60294=CARTESIAN_POINT('Ctrl Pts',(0.455671062340006,-0.538142604850548,
-1.54625343165006));
#60295=CARTESIAN_POINT('Ctrl Pts',(0.657018465304896,-0.256047488677006,
-1.53044654633197));
#60296=CARTESIAN_POINT('Ctrl Pts',(0.69964765112674,0.0879019026087411,
-1.51463966101388));
#60297=CARTESIAN_POINT('Ctrl Pts',(0.573260540331073,0.410616528051086,
-1.49883277569578));
#60298=CARTESIAN_POINT('Ctrl Pts',(0.308388903263251,0.63413710233158,-1.48302589037769));
#60299=CARTESIAN_POINT('Ctrl Pts',(-0.0309813049975863,0.704466989255031,
-1.4672190050596));
#60300=CARTESIAN_POINT('Ctrl Pts',(-0.362867252535701,0.604616355424324,
-1.45141211974151));
#60301=CARTESIAN_POINT('Ctrl Pts',(-0.607094106116187,0.358706462903012,
-1.43560523442342));
#60302=CARTESIAN_POINT('Ctrl Pts',(-0.674568768752993,0.128719220117463,
-1.42467385396992));
#60303=CARTESIAN_POINT('Ctrl Pts',(-0.676753669364399,0.0083709657598824,
-1.41901143528911));
#60304=CARTESIAN_POINT('Ctrl Pts',(-0.676748500489657,8.29977222930288E-6,
-1.418617978381));
#60305=CARTESIAN_POINT('Ctrl Pts',(-0.67674370184345,1.02755109432015E-5,
-1.57918202161899));
#60306=CARTESIAN_POINT('Ctrl Pts',(-0.676669257422799,-0.101306808967324,
-1.57441522990969));
#60307=CARTESIAN_POINT('Ctrl Pts',(-0.62810275948207,-0.314683464463068,
-1.56437947642769));
#60308=CARTESIAN_POINT('Ctrl Pts',(-0.412550866549072,-0.571870055479614,
-1.54907476117299));
#60309=CARTESIAN_POINT('Ctrl Pts',(-0.0902650651626452,-0.699346692174796,
-1.5332678758549));
#60310=CARTESIAN_POINT('Ctrl Pts',(0.253826379397398,-0.65787973594469,
-1.5174609905368));
#60311=CARTESIAN_POINT('Ctrl Pts',(0.536600109875943,-0.457486502452008,
-1.50165410521871));
#60312=CARTESIAN_POINT('Ctrl Pts',(0.689745500732789,-0.146576676396754,
-1.48584721990062));
#60313=CARTESIAN_POINT('Ctrl Pts',(0.67626669160168,0.199742183012912,-1.47004033458253));
#60314=CARTESIAN_POINT('Ctrl Pts',(0.499419804901498,0.497808634232871,
-1.45423344926444));
#60315=CARTESIAN_POINT('Ctrl Pts',(0.201926353111081,0.675617736418978,
-1.43842656394635));
#60316=CARTESIAN_POINT('Ctrl Pts',(-0.144347144374269,0.690215531378164,
-1.42261967862825));
#60317=CARTESIAN_POINT('Ctrl Pts',(-0.455750204246968,0.538075579424947,
-1.40681279331016));
#60318=CARTESIAN_POINT('Ctrl Pts',(-0.640147845607731,0.279647330628739,
-1.39233357430708));
#60319=CARTESIAN_POINT('Ctrl Pts',(-0.676609560222979,0.0837724483008001,
-1.38312331707669));
#60320=CARTESIAN_POINT('Ctrl Pts',(-0.676692639524176,-1.71467829109401E-5,
-1.37918202161899));
#60321=CARTESIAN_POINT('Origin',(0.,0.,-4.318617978381));
#60322=CARTESIAN_POINT('',(-0.676699979303772,-1.71578878559266E-5,-1.818617978381));
#60323=CARTESIAN_POINT('',(-0.676646172362016,5.7804085369928E-6,-1.77918202161899));
#60324=CARTESIAN_POINT('',(-0.6767,-7.33509820392354E-14,-4.318617978381));
#60325=CARTESIAN_POINT('Ctrl Pts',(-0.676699979303772,-1.7157887855928E-5,
-1.818617978381));
#60326=CARTESIAN_POINT('Ctrl Pts',(-0.676726159812639,-0.025864218275893,
-1.81740214627321));
#60327=CARTESIAN_POINT('Ctrl Pts',(-0.668977558555818,-0.163707169183447,
-1.81091735239272));
#60328=CARTESIAN_POINT('Ctrl Pts',(-0.577497061222251,-0.404636533804186,
-1.79916359673953));
#60329=CARTESIAN_POINT('Ctrl Pts',(-0.314962747739959,-0.630897810858063,
-1.78335671142144));
#60330=CARTESIAN_POINT('Ctrl Pts',(0.0236582032229997,-0.704750927370557,
-1.76754982610334));
#60331=CARTESIAN_POINT('Ctrl Pts',(0.356563960421018,-0.608354931218841,
-1.75174294078526));
#60332=CARTESIAN_POINT('Ctrl Pts',(0.603333331681656,-0.364996535725085,
-1.73593605546716));
#60333=CARTESIAN_POINT('Ctrl Pts',(0.704353388723183,-0.033464667988367,
-1.72012917014907));
#60334=CARTESIAN_POINT('Ctrl Pts',(0.635220367882906,0.306151375035467,
-1.70432228483098));
#60335=CARTESIAN_POINT('Ctrl Pts',(0.412634971489475,0.571809374278948,
-1.68851539951289));
#60336=CARTESIAN_POINT('Ctrl Pts',(0.0903679215898715,0.69933341043949,
-1.67270851419479));
#60337=CARTESIAN_POINT('Ctrl Pts',(-0.253729618865292,0.657917062189359,
-1.65690162887671));
#60338=CARTESIAN_POINT('Ctrl Pts',(-0.53653282001449,0.457565419646962,
-1.64109474355861));
#60339=CARTESIAN_POINT('Ctrl Pts',(-0.660207093665119,0.206579842277233,
-1.62833352672671));
#60340=CARTESIAN_POINT('Ctrl Pts',(-0.676667855529483,0.0472824307012137,
-1.62084127166751));
#60341=CARTESIAN_POINT('Ctrl Pts',(-0.67664869645179,7.73109616233197E-6,
-1.618617978381));
#60342=CARTESIAN_POINT('Ctrl Pts',(-0.676646172362016,5.7804085369928E-6,
-1.77918202161899));
#60343=CARTESIAN_POINT('Ctrl Pts',(-0.676627337627041,-0.0624444429508034,
-1.77624506628809));
#60344=CARTESIAN_POINT('Ctrl Pts',(-0.652674079260861,-0.236945885371131,
-1.76803914918448));
#60345=CARTESIAN_POINT('Ctrl Pts',(-0.504566489299185,-0.492591347590416,
-1.75456427030818));
#60346=CARTESIAN_POINT('Ctrl Pts',(-0.208937049864503,-0.6734826553361,
-1.73875738499009));
#60347=CARTESIAN_POINT('Ctrl Pts',(0.137166033464237,-0.691678434757318,
-1.722950499672));
#60348=CARTESIAN_POINT('Ctrl Pts',(0.450133444915136,-0.542783068650339,
-1.70714361435391));
#60349=CARTESIAN_POINT('Ctrl Pts',(0.654360567278065,-0.262765724241526,
-1.69133672903581));
#60350=CARTESIAN_POINT('Ctrl Pts',(0.700511550093094,0.0807288426203301,
-1.67552984371772));
#60351=CARTESIAN_POINT('Ctrl Pts',(0.577437541237162,0.404721464484683,
-1.65972295839963));
#60352=CARTESIAN_POINT('Ctrl Pts',(0.314869953591033,0.630944126028784,
-1.64391607308154));
#60353=CARTESIAN_POINT('Ctrl Pts',(-0.0237618549331032,0.704747438515944,
-1.62810918776345));
#60354=CARTESIAN_POINT('Ctrl Pts',(-0.356653430191126,0.608302481153537,
-1.61230230244536));
#60355=CARTESIAN_POINT('Ctrl Pts',(-0.603387005990771,0.364907794992297,
-1.59649541712726));
#60356=CARTESIAN_POINT('Ctrl Pts',(-0.673908967110712,0.133343716310157,
-1.58545532351848));
#60357=CARTESIAN_POINT('Ctrl Pts',(-0.676751544384454,0.0106837871384544,
-1.57968419168239));
#60358=CARTESIAN_POINT('Ctrl Pts',(-0.67674370184345,1.02755109432015E-5,
-1.57918202161899));
#60359=CARTESIAN_POINT('Origin',(0.,0.,-4.318617978381));
#60360=CARTESIAN_POINT('',(-0.67673798465263,1.20914945348619E-5,-2.018617978381));
#60361=CARTESIAN_POINT('',(-0.676707204276618,-1.68789097811373E-5,-1.979182021619));
#60362=CARTESIAN_POINT('',(-0.6767,-7.33509820392354E-14,-4.318617978381));
#60363=CARTESIAN_POINT('Ctrl Pts',(-0.676737984652629,1.2091494534832E-5,
-2.018617978381));
#60364=CARTESIAN_POINT('Ctrl Pts',(-0.676655634372884,-0.0989304053447198,
-2.01396302087891));
#60365=CARTESIAN_POINT('Ctrl Pts',(-0.629829434074097,-0.309941629925032,
-2.00403910160412));
#60366=CARTESIAN_POINT('Ctrl Pts',(-0.418555422414341,-0.567490033900997,
-1.98884622055663));
#60367=CARTESIAN_POINT('Ctrl Pts',(-0.097631117047166,-0.698356459978373,
-1.97303933523854));
#60368=CARTESIAN_POINT('Ctrl Pts',(0.246878274057621,-0.660518506938096,
-1.95723244992044));
#60369=CARTESIAN_POINT('Ctrl Pts',(0.531748428856327,-0.463116819623548,
-1.94142556460235));
#60370=CARTESIAN_POINT('Ctrl Pts',(0.68816228135381,-0.153838404604709,
-1.92561867928426));
#60371=CARTESIAN_POINT('Ctrl Pts',(0.678334397630255,0.192603284502106,
-1.90981179396617));
#60372=CARTESIAN_POINT('Ctrl Pts',(0.504638933459461,0.49251713375912,-1.89400490864808));
#60373=CARTESIAN_POINT('Ctrl Pts',(0.209036101308555,0.67345192000552,-1.87819802332998));
#60374=CARTESIAN_POINT('Ctrl Pts',(-0.137064302935446,0.691698602767291,
-1.8623911380119));
#60375=CARTESIAN_POINT('Ctrl Pts',(-0.450053610696377,0.542849267945122,
-1.8465842526938));
#60376=CARTESIAN_POINT('Ctrl Pts',(-0.638610030267167,0.284397992760645,
-1.83199319948351));
#60377=CARTESIAN_POINT('Ctrl Pts',(-0.676612703275732,0.0861472775944482,
-1.8226711080459));
#60378=CARTESIAN_POINT('Ctrl Pts',(-0.676699979303772,-1.7157887855928E-5,
-1.818617978381));
#60379=CARTESIAN_POINT('Ctrl Pts',(-0.676707204276618,-1.68789097811095E-5,
-1.97918202161899));
#60380=CARTESIAN_POINT('Ctrl Pts',(-0.676731182525368,-0.0235521105545861,
-1.97807490266648));
#60381=CARTESIAN_POINT('Ctrl Pts',(-0.669796504969086,-0.159081332134532,
-1.97169882194128));
#60382=CARTESIAN_POINT('Ctrl Pts',(-0.581612569954882,-0.398698377617872,
-1.96005377944337));
#60383=CARTESIAN_POINT('Ctrl Pts',(-0.321410263880308,-0.627637650334202,
-1.94424689412528));
#60384=CARTESIAN_POINT('Ctrl Pts',(0.0164362283905885,-0.704956330733284,
-1.92844000880719));
#60385=CARTESIAN_POINT('Ctrl Pts',(0.350312164270045,-0.611976278469258,
-1.9126331234891));
#60386=CARTESIAN_POINT('Ctrl Pts',(0.599561982174783,-0.37115900551555,
-1.896826238171));
#60387=CARTESIAN_POINT('Ctrl Pts',(0.70397354377059,-0.0406795712332764,
-1.88101935285292));
#60388=CARTESIAN_POINT('Ctrl Pts',(0.638323787940124,0.29962696740183,-1.86521246753482));
#60389=CARTESIAN_POINT('Ctrl Pts',(0.41847195266759,0.567551585915519,-1.84940558221673));
#60390=CARTESIAN_POINT('Ctrl Pts',(0.0975284042101817,0.698370809969075,
-1.83359869689864));
#60391=CARTESIAN_POINT('Ctrl Pts',(-0.246975417290485,0.660482188328222,
-1.81779181158055));
#60392=CARTESIAN_POINT('Ctrl Pts',(-0.531816535259198,0.46303860602497,
-1.80198492626245));
#60393=CARTESIAN_POINT('Ctrl Pts',(-0.659131299877361,0.211206098569119,
-1.78911499627527));
#60394=CARTESIAN_POINT('Ctrl Pts',(-0.676661127551435,0.0495926166918764,
-1.78151402806078));
#60395=CARTESIAN_POINT('Ctrl Pts',(-0.676646172362016,5.7804085369928E-6,
-1.77918202161899));
#60396=CARTESIAN_POINT('Origin',(0.,0.,-4.318617978381));
#60397=CARTESIAN_POINT('',(-0.676644363004478,3.68526634802388E-6,-2.218617978381));
#60398=CARTESIAN_POINT('',(-0.676731813311252,1.36189314004012E-5,-2.17918202161899));
#60399=CARTESIAN_POINT('',(-0.6767,-7.33509820392354E-14,-4.318617978381));
#60400=CARTESIAN_POINT('Ctrl Pts',(-0.676644363004478,3.6852663480233E-6,
-2.218617978381));
#60401=CARTESIAN_POINT('Ctrl Pts',(-0.676632850481567,-0.0600690012882533,
-2.2157928572573));
#60402=CARTESIAN_POINT('Ctrl Pts',(-0.653928438313362,-0.232188141953543,
-2.20769877436091));
#60403=CARTESIAN_POINT('Ctrl Pts',(-0.509730342149469,-0.487245891210574,
-2.19433572969182));
#60404=CARTESIAN_POINT('Ctrl Pts',(-0.216023905051799,-0.671243065256971,
-2.17852884437373));
#60405=CARTESIAN_POINT('Ctrl Pts',(0.129868171994647,-0.693085736480105,
-2.16272195905564));
#60406=CARTESIAN_POINT('Ctrl Pts',(0.444387546733483,-0.547497295443183,
-2.14691507373755));
#60407=CARTESIAN_POINT('Ctrl Pts',(0.65155468882939,-0.269648044075677,
-2.13110818841945));
#60408=CARTESIAN_POINT('Ctrl Pts',(0.701323517113522,0.0733410154887558,
-2.11530130310137));
#60409=CARTESIAN_POINT('Ctrl Pts',(0.581671204052573,0.398612832941228,
-2.09949441778327));
#60410=CARTESIAN_POINT('Ctrl Pts',(0.321502571670479,0.627590373268003,
-2.08368753246518));
#60411=CARTESIAN_POINT('Ctrl Pts',(-0.0163325460192437,0.704958742161505,
-2.06788064714709));
#60412=CARTESIAN_POINT('Ctrl Pts',(-0.350222154225635,0.612027795854858,
-2.052073761829));
#60413=CARTESIAN_POINT('Ctrl Pts',(-0.599507388494239,0.371247183625977,
-2.03626687651091));
#60414=CARTESIAN_POINT('Ctrl Pts',(-0.673205160779302,0.138101219917673,
-2.02511494869491));
#60415=CARTESIAN_POINT('Ctrl Pts',(-0.676748846926544,0.0130629336506955,
-2.01923198265161));
#60416=CARTESIAN_POINT('Ctrl Pts',(-0.676737984652629,1.2091494534832E-5,
-2.018617978381));
#60417=CARTESIAN_POINT('Ctrl Pts',(-0.676731813311252,1.36189314004047E-5,
-2.17918202161899));
#60418=CARTESIAN_POINT('Ctrl Pts',(-0.676644233480705,-0.0966206972557906,
-2.17463577727218));
#60419=CARTESIAN_POINT('Ctrl Pts',(-0.631479154499264,-0.305330546356952,
-2.16482057115268));
#60420=CARTESIAN_POINT('Ctrl Pts',(-0.424347837744089,-0.563171812546191,
-2.14973640326047));
#60421=CARTESIAN_POINT('Ctrl Pts',(-0.104781208775136,-0.697319493584015,
-2.13392951794238));
#60422=CARTESIAN_POINT('Ctrl Pts',(0.240097778255422,-0.663013299053236,
-2.11812263262429));
#60423=CARTESIAN_POINT('Ctrl Pts',(0.526975516741124,-0.46854069471079,
-2.1023157473062));
#60424=CARTESIAN_POINT('Ctrl Pts',(0.68654996177012,-0.160881098448797,
-2.08650886198811));
#60425=CARTESIAN_POINT('Ctrl Pts',(0.680272164181842,0.185643099747873,
-2.07070197667002));
#60426=CARTESIAN_POINT('Ctrl Pts',(0.509658673195849,0.48732085393598,-2.05489509135192));
#60427=CARTESIAN_POINT('Ctrl Pts',(0.215925178385313,0.671274828355656,
-2.03908820603383));
#60428=CARTESIAN_POINT('Ctrl Pts',(-0.129970106632608,0.693066626830752,
-2.02328132071574));
#60429=CARTESIAN_POINT('Ctrl Pts',(-0.444468064640782,0.547431929429699,
-2.00747443539765));
#60430=CARTESIAN_POINT('Ctrl Pts',(-0.637087153110088,0.289014990482141,
-1.99277466903207));
#60431=CARTESIAN_POINT('Ctrl Pts',(-0.67661706608309,0.0884559402215986,
-1.98334386443918));
#60432=CARTESIAN_POINT('Ctrl Pts',(-0.676707204276618,-1.68789097811095E-5,
-1.97918202161899));
#60433=CARTESIAN_POINT('Origin',(0.,0.,-4.318617978381));
#60434=CARTESIAN_POINT('',(-0.676714620613759,-1.62920487620288E-5,-2.418617978381));
#60435=CARTESIAN_POINT('',(-0.676643382151003,1.59347960965173E-6,-2.379182021619));
#60436=CARTESIAN_POINT('',(-0.6767,-7.33509820392354E-14,-4.318617978381));
#60437=CARTESIAN_POINT('Ctrl Pts',(-0.676714620613759,-1.6292048762058E-5,
-2.418617978381));
#60438=CARTESIAN_POINT('Ctrl Pts',(-0.676735957233897,-0.021173474084283,
-2.4176226936357));
#60439=CARTESIAN_POINT('Ctrl Pts',(-0.670613426882276,-0.154322869409382,
-2.41135844711771));
#60440=CARTESIAN_POINT('Ctrl Pts',(-0.58578251795406,-0.392546076109294,
-2.39982523882701));
#60441=CARTESIAN_POINT('Ctrl Pts',(-0.328007668658949,-0.624215146812637,
-2.38401835350892));
#60442=CARTESIAN_POINT('Ctrl Pts',(0.00900512466355355,-0.70509041118086,
-2.36821146819083));
#60443=CARTESIAN_POINT('Ctrl Pts',(0.343842518956618,-0.61563455260972,
-2.35240458287274));
#60444=CARTESIAN_POINT('Ctrl Pts',(0.595616689811292,-0.377457731445045,
-2.33659769755465));
#60445=CARTESIAN_POINT('Ctrl Pts',(0.703505682243138,-0.0480971440006585,
-2.32079081223656));
#60446=CARTESIAN_POINT('Ctrl Pts',(0.641446380171849,0.292882436437956,
-2.30498392691846));
#60447=CARTESIAN_POINT('Ctrl Pts',(0.424430663281246,0.563109396366323,
-2.28917704160037));
#60448=CARTESIAN_POINT('Ctrl Pts',(0.104883766927401,0.697304076887924,
-2.27337015628228));
#60449=CARTESIAN_POINT('Ctrl Pts',(-0.240000262814678,0.663048606105381,
-2.25756327096419));
#60450=CARTESIAN_POINT('Ctrl Pts',(-0.526906601153319,0.468618196264782,
-2.2417563856461));
#60451=CARTESIAN_POINT('Ctrl Pts',(-0.657997905630098,0.215965030249459,
-2.2287746214517));
#60452=CARTESIAN_POINT('Ctrl Pts',(-0.676654321788626,0.0519689167976407,
-2.22106181903));
#60453=CARTESIAN_POINT('Ctrl Pts',(-0.676644363004478,3.6852663480233E-6,
-2.218617978381));
#60454=CARTESIAN_POINT('Ctrl Pts',(-0.676643382151003,1.59347960970724E-6,
-2.379182021619));
#60455=CARTESIAN_POINT('Ctrl Pts',(-0.676638604274974,-0.0577596821259404,
-2.37646561365058));
#60456=CARTESIAN_POINT('Ctrl Pts',(-0.655121282576093,-0.227562834361756,
-2.36848024390947));
#60457=CARTESIAN_POINT('Ctrl Pts',(-0.514695806561756,-0.481997722559338,
-2.35522591239567));
#60458=CARTESIAN_POINT('Ctrl Pts',(-0.222889983854245,-0.668994493954996,
-2.33941902707757));
#60459=CARTESIAN_POINT('Ctrl Pts',(0.122760141143874,-0.694379957653575,
-2.32361214175949));
#60460=CARTESIAN_POINT('Ctrl Pts',(0.438754675367169,-0.55202165961862,
-2.30780525644139));
#60461=CARTESIAN_POINT('Ctrl Pts',(0.648757729114897,-0.276309584991779,
-2.2919983711233));
#60462=CARTESIAN_POINT('Ctrl Pts',(0.702038140257588,0.0661515492510317,
-2.2761914858052));
#60463=CARTESIAN_POINT('Ctrl Pts',(0.585724776077096,0.392632225542023,
-2.26038460048712));
#60464=CARTESIAN_POINT('Ctrl Pts',(0.327915857198116,0.624263380667703,
-2.24457771516902));
#60465=CARTESIAN_POINT('Ctrl Pts',(-0.0091088264969462,0.705089077439507,
-2.22877082985093));
#60466=CARTESIAN_POINT('Ctrl Pts',(-0.343933059552939,0.615583973468446,
-2.21296394453284));
#60467=CARTESIAN_POINT('Ctrl Pts',(-0.595672196966363,0.377370125481488,
-2.19715705921475));
#60468=CARTESIAN_POINT('Ctrl Pts',(-0.672496548540618,0.14272617859532,
-2.18589641824347));
#60469=CARTESIAN_POINT('Ctrl Pts',(-0.676745735895447,0.015375596625399,
-2.17990473904488));
#60470=CARTESIAN_POINT('Ctrl Pts',(-0.676731813311252,1.36189314004047E-5,
-2.17918202161899));
#60471=CARTESIAN_POINT('Origin',(0.,0.,-4.318617978381));
#60472=CARTESIAN_POINT('',(-0.676724990071838,1.49232986133271E-5,-2.618617978381));
#60473=CARTESIAN_POINT('',(-0.676721689350739,-1.54329616245952E-5,-2.579182021619));
#60474=CARTESIAN_POINT('',(-0.6767,-7.33509820392354E-14,-4.318617978381));
#60475=CARTESIAN_POINT('Ctrl Pts',(-0.676724990071838,1.49232986133355E-5,
-2.618617978381));
#60476=CARTESIAN_POINT('Ctrl Pts',(-0.676634302193046,-0.0942450091755502,
-2.6141835682414));
#60477=CARTESIAN_POINT('Ctrl Pts',(-0.633146801927531,-0.300585558606619,
-2.60448019632911));
#60478=CARTESIAN_POINT('Ctrl Pts',(-0.430260059478938,-0.558667934847332,
-2.58950786264411));
#60479=CARTESIAN_POINT('Ctrl Pts',(-0.11212508783917,-0.696176374840788,
-2.57370097732603));
#60480=CARTESIAN_POINT('Ctrl Pts',(0.23309632806146,-0.665507086403793,
-2.55789409200792));
#60481=CARTESIAN_POINT('Ctrl Pts',(0.5220078598931,-0.474068955342181,-2.54208720668984));
#60482=CARTESIAN_POINT('Ctrl Pts',(0.684816152269453,-0.16810835136977,
-2.52628032137174));
#60483=CARTESIAN_POINT('Ctrl Pts',(0.682191044370633,0.178462766956884,
-2.51047343605366));
#60484=CARTESIAN_POINT('Ctrl Pts',(0.514766692567439,0.481922019036879,
-2.49466655073556));
#60485=CARTESIAN_POINT('Ctrl Pts',(0.222988375079262,0.668961706519075,
-2.47885966541747));
#60486=CARTESIAN_POINT('Ctrl Pts',(-0.122658013407166,0.694398006878195,
-2.46305278009938));
#60487=CARTESIAN_POINT('Ctrl Pts',(-0.43867348246843,0.552086185290324,
-2.44724589478129));
#60488=CARTESIAN_POINT('Ctrl Pts',(-0.635491633703408,0.29376333873624,
-2.4324342942085));
#60489=CARTESIAN_POINT('Ctrl Pts',(-0.676623002789058,0.0908310390861413,
-2.4228916554084));
#60490=CARTESIAN_POINT('Ctrl Pts',(-0.676714620613759,-1.6292048762058E-5,
-2.418617978381));
#60491=CARTESIAN_POINT('Ctrl Pts',(-0.676721689350739,-1.54329616246299E-5,
-2.579182021619));
#60492=CARTESIAN_POINT('Ctrl Pts',(-0.676740183597297,-0.0188610859446095,
-2.57829545002898));
#60493=CARTESIAN_POINT('Ctrl Pts',(-0.671382810041269,-0.14969739182925,
-2.57213991666627));
#60494=CARTESIAN_POINT('Ctrl Pts',(-0.589773715425885,-0.386523663489563,
-2.56071542153086));
#60495=CARTESIAN_POINT('Ctrl Pts',(-0.334386030845991,-0.620821681499372,
-2.54490853621277));
#60496=CARTESIAN_POINT('Ctrl Pts',(0.00178044071789455,-0.705145664296035,
-2.52910165089467));
#60497=CARTESIAN_POINT('Ctrl Pts',(0.337516805075675,-0.619125176467695,
-2.51329476557658));
#60498=CARTESIAN_POINT('Ctrl Pts',(0.591718070518745,-0.383540483999043,
-2.49748788025849));
#60499=CARTESIAN_POINT('Ctrl Pts',(0.702975960450328,-0.0553025937328847,
-2.4816809949404));
#60500=CARTESIAN_POINT('Ctrl Pts',(0.644413522599621,0.286294934875548,
-2.46587410962231));
#60501=CARTESIAN_POINT('Ctrl Pts',(0.430177887097737,0.558731208450694,
-2.45006722430421));
#60502=CARTESIAN_POINT('Ctrl Pts',(0.112022695449392,0.69619285657704,-2.43426033898612));
#60503=CARTESIAN_POINT('Ctrl Pts',(-0.233194205177004,0.665472794723054,
-2.41845345366803));
#60504=CARTESIAN_POINT('Ctrl Pts',(-0.522077577221963,0.473992174204058,
-2.40264656834994));
#60505=CARTESIAN_POINT('Ctrl Pts',(-0.656870050744532,0.220590971059179,
-2.38955609100026));
#60506=CARTESIAN_POINT('Ctrl Pts',(-0.676647871824783,0.054278699680794,
-2.38173457542328));
#60507=CARTESIAN_POINT('Ctrl Pts',(-0.676643382151003,1.59347960970724E-6,
-2.379182021619));
#60508=CARTESIAN_POINT('Origin',(0.,0.,-4.318617978381));
#60509=CARTESIAN_POINT('',(-0.676643190996923,-5.82392518506049E-7,-2.818617978381));
#60510=CARTESIAN_POINT('',(-0.676718026672013,1.59161084590936E-5,-2.779182021619));
#60511=CARTESIAN_POINT('',(-0.6767,-7.33509820392354E-14,-4.318617978381));
#60512=CARTESIAN_POINT('Ctrl Pts',(-0.676643190996923,-5.82392518481967E-7,
-2.818617978381));
#60513=CARTESIAN_POINT('Ctrl Pts',(-0.676644864762177,-0.0553838781273899,
-2.8160134046198));
#60514=CARTESIAN_POINT('Ctrl Pts',(-0.656321235606746,-0.222804440132633,
-2.8081398690859));
#60515=CARTESIAN_POINT('Ctrl Pts',(-0.519747440714448,-0.476546092293478,
-2.79499737177931));
#60516=CARTESIAN_POINT('Ctrl Pts',(-0.229928759127129,-0.666608090211678,
-2.77919048646121));
#60517=CARTESIAN_POINT('Ctrl Pts',(0.115434605974731,-0.695635272217317,
-2.76338360114313));
#60518=CARTESIAN_POINT('Ctrl Pts',(0.432912035103061,-0.556615441819869,
-2.74757671582503));
#60519=CARTESIAN_POINT('Ctrl Pts',(0.645809410519448,-0.28313209901727,
-2.73176983050694));
#60520=CARTESIAN_POINT('Ctrl Pts',(0.70269637882455,0.0587484416496746,
-2.71596294518884));
#60521=CARTESIAN_POINT('Ctrl Pts',(0.589830558845161,0.386436918606138,
-2.70015605987076));
#60522=CARTESIAN_POINT('Ctrl Pts',(0.334477336060517,0.620772496065396,
-2.68434917455266));
#60523=CARTESIAN_POINT('Ctrl Pts',(-0.00167673062376321,0.705145920206461,
-2.66854228923458));
#60524=CARTESIAN_POINT('Ctrl Pts',(-0.337425743707141,0.619174811901361,
-2.65273540391648));
#60525=CARTESIAN_POINT('Ctrl Pts',(-0.591661655884731,0.383627508353011,
-2.63692851859839));
#60526=CARTESIAN_POINT('Ctrl Pts',(-0.671742365813614,0.147484140385321,
-2.6255560434199));
#60527=CARTESIAN_POINT('Ctrl Pts',(-0.676742057441559,0.017754550014597,
-2.6194525300141));
#60528=CARTESIAN_POINT('Ctrl Pts',(-0.676724990071838,1.49232986133355E-5,
-2.618617978381));
#60529=CARTESIAN_POINT('Ctrl Pts',(-0.676718026672013,1.59161084591075E-5,
-2.77918202161899));
#60530=CARTESIAN_POINT('Ctrl Pts',(-0.676626289360077,-0.0919358888217675,
-2.77485632463468));
#60531=CARTESIAN_POINT('Ctrl Pts',(-0.634739434109742,-0.295971603258148,
-2.76526166587767));
#60532=CARTESIAN_POINT('Ctrl Pts',(-0.435961470998621,-0.554230253278693,
-2.75039804534796));
#60533=CARTESIAN_POINT('Ctrl Pts',(-0.11925208204733,-0.694991020641291,
-2.73459116002987));
#60534=CARTESIAN_POINT('Ctrl Pts',(0.226265443741279,-0.667860409676459,
-2.71878427471177));
#60535=CARTESIAN_POINT('Ctrl Pts',(0.517123245750236,-0.479392455665905,
-2.70297738939368));
#60536=CARTESIAN_POINT('Ctrl Pts',(0.683057801392575,-0.17511601240717,
-2.68717050407559));
#60537=CARTESIAN_POINT('Ctrl Pts',(0.683983727646747,0.17146381005654,-2.6713636187575));
#60538=CARTESIAN_POINT('Ctrl Pts',(0.519677345313422,0.47662252843591,-2.65555673343941));
#60539=CARTESIAN_POINT('Ctrl Pts',(0.229830713971266,0.666641898443312,
-2.63974984812131));
#60540=CARTESIAN_POINT('Ctrl Pts',(-0.115536915778911,0.695618285367013,
-2.62394296280322));
#60541=CARTESIAN_POINT('Ctrl Pts',(-0.432993894223229,0.556551763459652,
-2.60813607748513));
#60542=CARTESIAN_POINT('Ctrl Pts',(-0.633912379396568,0.298377915502387,
-2.59321576375706));
#60543=CARTESIAN_POINT('Ctrl Pts',(-0.67663027089625,0.0931400499671855,
-2.58356441180168));
#60544=CARTESIAN_POINT('Ctrl Pts',(-0.676721689350739,-1.54329616246299E-5,
-2.579182021619));
#60545=CARTESIAN_POINT('Origin',(0.,0.,-4.318617978381));
#60546=CARTESIAN_POINT('',(-0.676728691753018,-1.42604622804819E-5,-3.018617978381));
#60547=CARTESIAN_POINT('',(-0.676643795884942,-2.68919649207278E-6,-2.979182021619));
#60548=CARTESIAN_POINT('',(-0.6767,-7.33509820392354E-14,-4.318617978381));
#60549=CARTESIAN_POINT('Ctrl Pts',(-0.676728691753018,-1.42604622804399E-5,
-3.018617978381));
#60550=CARTESIAN_POINT('Ctrl Pts',(-0.67674408521498,-0.0164821866856739,
-3.0178432409982));
#60551=CARTESIAN_POINT('Ctrl Pts',(-0.672148927518839,-0.144939328790899,
-3.0117995418427));
#60552=CARTESIAN_POINT('Ctrl Pts',(-0.593814889478732,-0.380286020309405,
-3.0004868809145));
#60553=CARTESIAN_POINT('Ctrl Pts',(-0.340910875057239,-0.617262792882503,
-2.98467999559641));
#60554=CARTESIAN_POINT('Ctrl Pts',(-0.0056518445272595,-0.705125263242527,
-2.96887311027831));
#60555=CARTESIAN_POINT('Ctrl Pts',(0.330972521582021,-0.622648191330417,
-2.95306622496023));
#60556=CARTESIAN_POINT('Ctrl Pts',(0.587642713915593,-0.389755847924465,
-2.93725933964213));
#60557=CARTESIAN_POINT('Ctrl Pts',(0.70235402869083,-0.0627088398167523,
-2.92145245432404));
#60558=CARTESIAN_POINT('Ctrl Pts',(0.647395257884359,0.27948695904862,-2.90564556900594));
#60559=CARTESIAN_POINT('Ctrl Pts',(0.436042981348057,0.554166129086307,
-2.88983868368786));
#60560=CARTESIAN_POINT('Ctrl Pts',(0.11935429761476,0.694973475645141,-2.87403179836976));
#60561=CARTESIAN_POINT('Ctrl Pts',(-0.226167215523084,0.667893682281796,
-2.85822491305168));
#60562=CARTESIAN_POINT('Ctrl Pts',(-0.5170527342108,0.479468508094678,-2.84241802773358));
#60563=CARTESIAN_POINT('Ctrl Pts',(-0.655682860652459,0.225349490586159,
-2.82921571617669));
#60564=CARTESIAN_POINT('Ctrl Pts',(-0.676641478793513,0.0566545952765675,
-2.8212823663925));
#60565=CARTESIAN_POINT('Ctrl Pts',(-0.676643190996923,-5.82392518481967E-7,
-2.818617978381));
#60566=CARTESIAN_POINT('Ctrl Pts',(-0.676643795884942,-2.68919649208318E-6,
-2.979182021619));
#60567=CARTESIAN_POINT('Ctrl Pts',(-0.676651210036511,-0.0530741872066186,
-2.97668616101308));
#60568=CARTESIAN_POINT('Ctrl Pts',(-0.657461434917153,-0.218178597507427,
-2.96892133863446));
#60569=CARTESIAN_POINT('Ctrl Pts',(-0.524602751372391,-0.471195852164642,
-2.95588755448315));
#60570=CARTESIAN_POINT('Ctrl Pts',(-0.236746619036826,-0.664217295935056,
-2.94008066916506));
#60571=CARTESIAN_POINT('Ctrl Pts',(0.108301210750851,-0.696781476213702,
-2.92427378384697));
#60572=CARTESIAN_POINT('Ctrl Pts',(0.427186343456901,-0.56102175163586,
-2.90846689852887));
#60573=CARTESIAN_POINT('Ctrl Pts',(0.642874597533564,-0.289734067190421,
-2.89266001321078));
#60574=CARTESIAN_POINT('Ctrl Pts',(0.703261417396002,0.0515456753453884,
-2.87685312789269));
#60575=CARTESIAN_POINT('Ctrl Pts',(0.593758950657057,0.38037335127382,-2.8610462425746));
#60576=CARTESIAN_POINT('Ctrl Pts',(0.340820085951307,0.617312924582654,
-2.84523935725651));
#60577=CARTESIAN_POINT('Ctrl Pts',(0.00554813737457995,0.705126085190668,
-2.82943247193842));
#60578=CARTESIAN_POINT('Ctrl Pts',(-0.33106409388682,0.622599504965708,
-2.81362558662032));
#60579=CARTESIAN_POINT('Ctrl Pts',(-0.587700029934952,0.389669414579977,
-2.79781870130224));
#60580=CARTESIAN_POINT('Ctrl Pts',(-0.670984618310945,0.152109523970622,
-2.78633751296845));
#60581=CARTESIAN_POINT('Ctrl Pts',(-0.676738030980323,0.0200669969246454,
-2.78012528640738));
#60582=CARTESIAN_POINT('Ctrl Pts',(-0.676718026672013,1.59161084591075E-5,
-2.77918202161899));
#60583=CARTESIAN_POINT('Origin',(0.,0.,-4.318617978381));
#60584=CARTESIAN_POINT('',(-0.676710664634451,1.66436917362715E-5,-3.218617978381));
#60585=CARTESIAN_POINT('',(-0.676735096869437,-1.28530889785816E-5,-3.179182021619));
#60586=CARTESIAN_POINT('',(-0.6767,-7.33509820392354E-14,-4.318617978381));
#60587=CARTESIAN_POINT('Ctrl Pts',(-0.676710664634451,1.66436917362969E-5,
-3.218617978381));
#60588=CARTESIAN_POINT('Ctrl Pts',(-0.676619640086048,-0.0895607009637898,
-3.2144041156039));
#60589=CARTESIAN_POINT('Ctrl Pts',(-0.636348652061272,-0.291223853614914,
-3.20492129105409));
#60590=CARTESIAN_POINT('Ctrl Pts',(-0.441778804249146,-0.549604465343574,
-3.1901695047316));
#60591=CARTESIAN_POINT('Ctrl Pts',(-0.126570615394638,-0.693695509231553,
-3.17436261941351));
#60592=CARTESIAN_POINT('Ctrl Pts',(0.219213673644229,-0.67020813595241,
-3.15855573409542));
#60593=CARTESIAN_POINT('Ctrl Pts',(0.512041759331881,-0.484816271292242,
-3.14274884877732));
#60594=CARTESIAN_POINT('Ctrl Pts',(0.681174150856313,-0.182305667532811,
-3.12694196345923));
#60595=CARTESIAN_POINT('Ctrl Pts',(0.685752952950544,0.164245145222046,
-3.11113507814114));
#60596=CARTESIAN_POINT('Ctrl Pts',(0.52467204859744,0.471118691658448,-3.09532819282305));
#60597=CARTESIAN_POINT('Ctrl Pts',(0.236844307533238,0.664182470559487,
-3.07952130750496));
#60598=CARTESIAN_POINT('Ctrl Pts',(-0.108198729930143,0.696797398854864,
-3.06371442218686));
#60599=CARTESIAN_POINT('Ctrl Pts',(-0.427103826957276,0.561084575806403,
-3.04790753686878));
#60600=CARTESIAN_POINT('Ctrl Pts',(-0.632258570116134,0.30312359041971,
-3.03287538893349));
#60601=CARTESIAN_POINT('Ctrl Pts',(-0.676639394819978,0.0955156020780497,
-3.0231122027709));
#60602=CARTESIAN_POINT('Ctrl Pts',(-0.676728691753018,-1.42604622804399E-5,
-3.018617978381));
#60603=CARTESIAN_POINT('Ctrl Pts',(-0.676735096869437,-1.28530889786354E-5,
-3.179182021619));
#60604=CARTESIAN_POINT('Ctrl Pts',(-0.676747416170365,-0.0141695695630101,
-3.17851599739147));
#60605=CARTESIAN_POINT('Ctrl Pts',(-0.672869095986787,-0.140314265330913,
-3.17258101139126));
#60606=CARTESIAN_POINT('Ctrl Pts',(-0.597680051307391,-0.374181953217737,
-3.16137706361834));
#60607=CARTESIAN_POINT('Ctrl Pts',(-0.347217327542774,-0.613737488914194,
-3.14557017830025));
#60608=CARTESIAN_POINT('Ctrl Pts',(-0.0128761161877245,-0.705030342238238,
-3.12976329298216));
#60609=CARTESIAN_POINT('Ctrl Pts',(0.324575622972799,-0.6260065836846,-3.11395640766407));
#60610=CARTESIAN_POINT('Ctrl Pts',(0.583618509221664,-0.395756255210866,
-3.09814952234597));
#60611=CARTESIAN_POINT('Ctrl Pts',(0.701674658922178,-0.0699017229479336,
-3.08234263702789));
#60612=CARTESIAN_POINT('Ctrl Pts',(0.650224840739586,0.272839209663541,
-3.06653575170979));
#60613=CARTESIAN_POINT('Ctrl Pts',(0.441697964735771,0.549669433198649,
-3.0507288663917));
#60614=CARTESIAN_POINT('Ctrl Pts',(0.126468587690317,0.693714115592484,
-3.03492198107361));
#60615=CARTESIAN_POINT('Ctrl Pts',(-0.219312242355004,0.6701758860164,-3.01911509575552));
#60616=CARTESIAN_POINT('Ctrl Pts',(-0.51211305746562,0.484740955787583,
-3.00330821043742));
#60617=CARTESIAN_POINT('Ctrl Pts',(-0.654502474040477,0.229974940576465,
-2.98999718572525));
#60618=CARTESIAN_POINT('Ctrl Pts',(-0.676635558168333,0.0589639985686951,
-2.98195512278578));
#60619=CARTESIAN_POINT('Ctrl Pts',(-0.676643795884942,-2.68919649208318E-6,
-2.979182021619));
#60620=CARTESIAN_POINT('Origin',(0.,0.,-4.318617978381));
#60621=CARTESIAN_POINT('',(-0.67664523128147,-4.81506944670235E-6,-3.418617978381));
#60622=CARTESIAN_POINT('',(-0.67670343080534,1.70602472024106E-5,-3.37918202161899));
#60623=CARTESIAN_POINT('',(-0.6767,-7.33509820392354E-14,-4.318617978381));
#60624=CARTESIAN_POINT('Ctrl Pts',(-0.67664523128147,-4.81506944666546E-6,
-3.418617978381));
#60625=CARTESIAN_POINT('Ctrl Pts',(-0.676657944807875,-0.0506979848076553,
-3.4162339519823));
#60626=CARTESIAN_POINT('Ctrl Pts',(-0.658607477478239,-0.213419747977293,
-3.40858096381089));
#60627=CARTESIAN_POINT('Ctrl Pts',(-0.529539984287318,-0.465640403369804,
-3.39565901386679));
#60628=CARTESIAN_POINT('Ctrl Pts',(-0.243734273318034,-0.661685109564608,
-3.3798521285487));
#60629=CARTESIAN_POINT('Ctrl Pts',(0.100951166852987,-0.697884261264305,
-3.36404524323061));
#60630=CARTESIAN_POINT('Ctrl Pts',(0.421249485401818,-0.565493104518617,
-3.34823835791252));
#60631=CARTESIAN_POINT('Ctrl Pts',(0.639785112601671,-0.296493827764879,
-3.33243147259443));
#60632=CARTESIAN_POINT('Ctrl Pts',(0.703765643119916,0.0441304857599676,
-3.31662458727633));
#60633=CARTESIAN_POINT('Ctrl Pts',(0.597735079489259,0.374094045605343,
-3.30081770195824));
#60634=CARTESIAN_POINT('Ctrl Pts',(0.347307590733571,0.613686416362823,
-3.28501081664015));
#60635=CARTESIAN_POINT('Ctrl Pts',(0.0129798091970768,0.705028442520307,
-3.26920393132206));
#60636=CARTESIAN_POINT('Ctrl Pts',(-0.324483549622869,0.626054315721524,
-3.25339704600396));
#60637=CARTESIAN_POINT('Ctrl Pts',(-0.583560298007917,0.395842088209822,
-3.23759016068587));
#60638=CARTESIAN_POINT('Ctrl Pts',(-0.670179715173758,0.15686789833644,
-3.22599713814489));
#60639=CARTESIAN_POINT('Ctrl Pts',(-0.676733456052842,0.0224457002066953,
-3.2196730773766));
#60640=CARTESIAN_POINT('Ctrl Pts',(-0.676710664634451,1.66436917362969E-5,
-3.218617978381));
#60641=CARTESIAN_POINT('Ctrl Pts',(-0.67670343080534,1.70602472024037E-5,
-3.37918202161899));
#60642=CARTESIAN_POINT('Ctrl Pts',(-0.676614623171181,-0.0872519716669216,
-3.37507687199717));
#60643=CARTESIAN_POINT('Ctrl Pts',(-0.637884772482277,-0.2866073942538,
-3.36570276060266));
#60644=CARTESIAN_POINT('Ctrl Pts',(-0.44738674868464,-0.545049240845295,
-3.35105968743544));
#60645=CARTESIAN_POINT('Ctrl Pts',(-0.133671432891043,-0.692362279354891,
-3.33525280211735));
#60646=CARTESIAN_POINT('Ctrl Pts',(0.212335352064805,-0.672418973637837,
-3.31944591679926));
#60647=CARTESIAN_POINT('Ctrl Pts',(0.507047553541136,-0.490037096853488,
-3.30363903148117));
#60648=CARTESIAN_POINT('Ctrl Pts',(0.679270528375343,-0.18927526812906,
-3.28783214616308));
#60649=CARTESIAN_POINT('Ctrl Pts',(0.6873997784289,0.157210440049462,-3.27202526084499));
#60650=CARTESIAN_POINT('Ctrl Pts',(0.529471492723354,0.465718279905297,
-3.25621837552689));
#60651=CARTESIAN_POINT('Ctrl Pts',(0.243636952032847,0.66172094832247,-3.2404114902088));
#60652=CARTESIAN_POINT('Ctrl Pts',(-0.101053807620812,0.697869404552157,
-3.22460460489071));
#60653=CARTESIAN_POINT('Ctrl Pts',(-0.421332650367923,0.565431141323669,
-3.20879771957261));
#60654=CARTESIAN_POINT('Ctrl Pts',(-0.63062236438263,0.307735384374043,
-3.19365685848205));
#60655=CARTESIAN_POINT('Ctrl Pts',(-0.676649957364854,0.0978251520198036,
-3.18378495916417));
#60656=CARTESIAN_POINT('Ctrl Pts',(-0.676735096869437,-1.28530889786354E-5,
-3.179182021619));
#60657=CARTESIAN_POINT('Origin',(0.,0.,-4.318617978381));
#60658=CARTESIAN_POINT('',(-0.676741132471547,-1.11494260315432E-5,-3.618617978381));
#60659=CARTESIAN_POINT('',(-0.676647395625952,-6.81016621412178E-6,-3.579182021619));
#60660=CARTESIAN_POINT('',(-0.6767,-7.33509820392354E-14,-4.318617978381));
#60661=CARTESIAN_POINT('Ctrl Pts',(-0.676741132471547,-1.11494260315228E-5,
-3.618617978381));
#60662=CARTESIAN_POINT('Ctrl Pts',(-0.676750354590291,-0.011790463288482,
-3.61806378836069));
#60663=CARTESIAN_POINT('Ctrl Pts',(-0.673584757733222,-0.135556650969889,
-3.61224063656769));
#60664=CARTESIAN_POINT('Ctrl Pts',(-0.601590705440622,-0.367861663287755,
-3.60114852300198));
#60665=CARTESIAN_POINT('Ctrl Pts',(-0.353666792150765,-0.610043752821873,
-3.58534163768389));
#60666=CARTESIAN_POINT('Ctrl Pts',(-0.0203063718595239,-0.704855468490197,
-3.56953475236579));
#60667=CARTESIAN_POINT('Ctrl Pts',(0.317959528732968,-0.629392817167735,
-3.55372786704772));
#60668=CARTESIAN_POINT('Ctrl Pts',(0.579414849121761,-0.401885571804838,
-3.53792098172961));
#60669=CARTESIAN_POINT('Ctrl Pts',(0.700898925634034,-0.0772934425076206,
-3.52211409641153));
#60670=CARTESIAN_POINT('Ctrl Pts',(0.653064430829429,0.265970730335282,
-3.50630721109343));
#60671=CARTESIAN_POINT('Ctrl Pts',(0.447466908630123,0.544983436344741,
-3.49050032577534));
#60672=CARTESIAN_POINT('Ctrl Pts',(0.13377326171177,0.692342613639074,-3.47469344045725));
#60673=CARTESIAN_POINT('Ctrl Pts',(-0.212236453508304,0.672450197420986,
-3.45888655513916));
#60674=CARTESIAN_POINT('Ctrl Pts',(-0.506975476514332,0.490111667298897,
-3.44307966982107));
#60675=CARTESIAN_POINT('Ctrl Pts',(-0.653260996170914,0.234732857334829,
-3.42965681090168));
#60676=CARTESIAN_POINT('Ctrl Pts',(-0.676629846509692,0.0613395218375697,
-3.42150291375499));
#60677=CARTESIAN_POINT('Ctrl Pts',(-0.67664523128147,-4.81506944666546E-6,
-3.418617978381));
#60678=CARTESIAN_POINT('Ctrl Pts',(-0.676647395625952,-6.81016621412525E-6,
-3.579182021619));
#60679=CARTESIAN_POINT('Ctrl Pts',(-0.676664625586388,-0.0483878949866939,
-3.57690670837557));
#60680=CARTESIAN_POINT('Ctrl Pts',(-0.659695506058363,-0.208793550331727,
-3.56936243335945));
#60681=CARTESIAN_POINT('Ctrl Pts',(-0.534283043471572,-0.460190403314884,
-3.55654919657064));
#60682=CARTESIAN_POINT('Ctrl Pts',(-0.250500968703414,-0.659153125247455,
-3.54074231125254));
#60683=CARTESIAN_POINT('Ctrl Pts',(0.093795489213489,-0.698881952870262,
-3.52493542593445));
#60684=CARTESIAN_POINT('Ctrl Pts',(0.41543344724007,-0.569779456245059,
-3.50912854061636));
#60685=CARTESIAN_POINT('Ctrl Pts',(0.636713714319684,-0.303033370838706,
-3.49332165529827));
#60686=CARTESIAN_POINT('Ctrl Pts',(0.704180852995891,0.0369175313181082,
-3.47751476998018));
#60687=CARTESIAN_POINT('Ctrl Pts',(0.60153659384113,0.367950138082134,-3.46170788466208));
#60688=CARTESIAN_POINT('Ctrl Pts',(0.353577064625491,0.610095760692912,
-3.44590099934399));
#60689=CARTESIAN_POINT('Ctrl Pts',(0.0202027041935265,0.704858445780369,
-3.4300941140259));
#60690=CARTESIAN_POINT('Ctrl Pts',(-0.318052093182595,0.629346044610447,
-3.41428722870781));
#60691=CARTESIAN_POINT('Ctrl Pts',(-0.579473949242324,0.401800348424625,
-3.39848034338972));
#60692=CARTESIAN_POINT('Ctrl Pts',(-0.669372488353821,0.161493655533598,
-3.38677860769344));
#60693=CARTESIAN_POINT('Ctrl Pts',(-0.676728607817933,0.024757878266858,
-3.38034583376987));
#60694=CARTESIAN_POINT('Ctrl Pts',(-0.67670343080534,1.70602472024037E-5,
-3.37918202161899));
#60695=CARTESIAN_POINT('Origin',(0.,0.,-4.318617978381));
#60696=CARTESIAN_POINT('',(-0.676696040235193,1.73011422674059E-5,-3.818617978381));
#60697=CARTESIAN_POINT('',(-0.676746306964879,-9.26850736493456E-6,-3.779182021619));
#60698=CARTESIAN_POINT('',(-0.6767,-7.33509820392354E-14,-4.318617978381));
#60699=CARTESIAN_POINT('Ctrl Pts',(-0.676696040235193,1.73011422674348E-5,
-3.818617978381));
#60700=CARTESIAN_POINT('Ctrl Pts',(-0.676610863373156,-0.0848769969584761,
-3.8146246629664));
#60701=CARTESIAN_POINT('Ctrl Pts',(-0.639436142203106,-0.281857407337619,
-3.80536238577909));
#60702=CARTESIAN_POINT('Ctrl Pts',(-0.453106684122212,-0.54030344862574,
-3.79083114681908));
#60703=CARTESIAN_POINT('Ctrl Pts',(-0.140961456517365,-0.690914982312493,
-3.775024261501));
#60704=CARTESIAN_POINT('Ctrl Pts',(0.205236307704561,-0.674619600339438,
-3.7592173761829));
#60705=CARTESIAN_POINT('Ctrl Pts',(0.501854433527548,-0.495354136485513,
-3.74341049086481));
#60706=CARTESIAN_POINT('Ctrl Pts',(0.677237850353305,-0.196424212884838,
-3.72760360554672));
#60707=CARTESIAN_POINT('Ctrl Pts',(0.689018584600613,0.149956558745365,
-3.71179672022863));
#60708=CARTESIAN_POINT('Ctrl Pts',(0.534350721904737,0.46011182080935,-3.69598983491053));
#60709=CARTESIAN_POINT('Ctrl Pts',(0.250597912301867,0.659116276136679,
-3.68018294959245));
#60710=CARTESIAN_POINT('Ctrl Pts',(-0.0936926996039382,0.698895742478711,
-3.66437606427435));
#60711=CARTESIAN_POINT('Ctrl Pts',(-0.415349642780955,0.569840551551763,
-3.64856917895626));
#60712=CARTESIAN_POINT('Ctrl Pts',(-0.628909669716038,0.312478000882297,
-3.63331648365847));
#60713=CARTESIAN_POINT('Ctrl Pts',(-0.676662675293759,0.100201366544979,
-3.62333275013339));
#60714=CARTESIAN_POINT('Ctrl Pts',(-0.676741132471547,-1.11494260315228E-5,
-3.618617978381));
#60715=CARTESIAN_POINT('Ctrl Pts',(-0.676746306964879,-9.26850736500048E-6,
-3.779182021619));
#60716=CARTESIAN_POINT('Ctrl Pts',(-0.676752713979664,-0.0094776731315671,
-3.77873654475397));
#60717=CARTESIAN_POINT('Ctrl Pts',(-0.674256040567153,-0.130932040600602,
-3.77302210611625));
#60718=CARTESIAN_POINT('Ctrl Pts',(-0.605328161907258,-0.361678580640496,
-3.76203870570583));
#60719=CARTESIAN_POINT('Ctrl Pts',(-0.359898610147466,-0.606388132436475,
-3.74623182038774));
#60720=CARTESIAN_POINT('Ctrl Pts',(-0.0275271100694295,-0.704610414814641,
-3.73042493506964));
#60721=CARTESIAN_POINT('Ctrl Pts',(0.311494209180319,-0.632617526813099,
-3.71461804975155));
#60722=CARTESIAN_POINT('Ctrl Pts',(0.575266797655111,-0.407801041483892,
-3.69881116443346));
#60723=CARTESIAN_POINT('Ctrl Pts',(0.700070201416114,-0.0844706513202744,
-3.68300427911537));
#60724=CARTESIAN_POINT('Ctrl Pts',(0.655755231597374,0.259265605233607,
-3.66719739379728));
#60725=CARTESIAN_POINT('Ctrl Pts',(0.453027208375958,0.540370175281444,
-3.65139050847919));
#60726=CARTESIAN_POINT('Ctrl Pts',(0.140859839636748,0.690935657938768,
-3.63558362316109));
#60727=CARTESIAN_POINT('Ctrl Pts',(-0.20533552647555,0.674589430258686,
-3.61977673784301));
#60728=CARTESIAN_POINT('Ctrl Pts',(-0.501927281124956,0.495280306801541,
-3.6039698525249));
#60729=CARTESIAN_POINT('Ctrl Pts',(-0.652027592210673,0.239357621077411,
-3.59043828045024));
#60730=CARTESIAN_POINT('Ctrl Pts',(-0.676624726023924,0.0636485849035314,
-3.58217567014827));
#60731=CARTESIAN_POINT('Ctrl Pts',(-0.676647395625952,-6.81016621412525E-6,
-3.579182021619));
#60732=CARTESIAN_POINT('Ctrl Pts',(-0.292601934307088,0.610169646934154,
-4.01494887079529));
#60733=CARTESIAN_POINT('Ctrl Pts',(-0.393602898590677,0.561735448896361,
-4.0096799090226));
#60734=CARTESIAN_POINT('Ctrl Pts',(-0.570992886715937,0.413800223741275,
-3.9991419854772));
#60735=CARTESIAN_POINT('Ctrl Pts',(-0.699157014481291,0.0917216394468504,
-3.98333510015911));
#60736=CARTESIAN_POINT('Ctrl Pts',(-0.658413028863308,-0.252426258090312,
-3.96752821484101));
#60737=CARTESIAN_POINT('Ctrl Pts',(-0.458619399794603,-0.535637926938055,
-3.95172132952293));
#60738=CARTESIAN_POINT('Ctrl Pts',(-0.148032691342333,-0.689431756556144,
-3.93591444420484));
#60739=CARTESIAN_POINT('Ctrl Pts',(0.198313347812299,-0.676688375201064,
-3.92010755888674));
#60740=CARTESIAN_POINT('Ctrl Pts',(0.496752882142743,-0.50046932737395,
-3.90430067356866));
#60741=CARTESIAN_POINT('Ctrl Pts',(0.675189733576972,-0.203353101808354,
-3.88849378825056));
#60742=CARTESIAN_POINT('Ctrl Pts',(0.690518863850223,0.142889328597765,
-3.87268690293247));
#60743=CARTESIAN_POINT('Ctrl Pts',(0.539036872034762,0.454612727099145,
-3.85688001761438));
#60744=CARTESIAN_POINT('Ctrl Pts',(0.257337933699506,0.656514151291388,
-3.84107313229629));
#60745=CARTESIAN_POINT('Ctrl Pts',(-0.0865270426321366,0.699818987663747,
-3.82526624697819));
#60746=CARTESIAN_POINT('Ctrl Pts',(-0.409489369688631,0.574066239054321,
-3.8094593616601));
#60747=CARTESIAN_POINT('Ctrl Pts',(-0.633529943812292,0.309634276622324,
-3.79365247634201));
#60748=CARTESIAN_POINT('Ctrl Pts',(-0.704526500534943,-0.0295970794965726,
-3.77784559102392));
#60749=CARTESIAN_POINT('Ctrl Pts',(-0.605328161907258,-0.361678580640496,
-3.76203870570583));
#60750=CARTESIAN_POINT('Ctrl Pts',(-0.359898610147466,-0.606388132436475,
-3.74623182038774));
#60751=CARTESIAN_POINT('Ctrl Pts',(-0.0275271100694295,-0.704610414814641,
-3.73042493506964));
#60752=CARTESIAN_POINT('Ctrl Pts',(0.311494209180319,-0.632617526813099,
-3.71461804975155));
#60753=CARTESIAN_POINT('Ctrl Pts',(0.575266797655111,-0.407801041483892,
-3.69881116443346));
#60754=CARTESIAN_POINT('Ctrl Pts',(0.700070201416114,-0.0844706513202744,
-3.68300427911537));
#60755=CARTESIAN_POINT('Ctrl Pts',(0.655755231597374,0.259265605233607,
-3.66719739379728));
#60756=CARTESIAN_POINT('Ctrl Pts',(0.453027208375958,0.540370175281444,
-3.65139050847919));
#60757=CARTESIAN_POINT('Ctrl Pts',(0.140859839636748,0.690935657938768,
-3.63558362316109));
#60758=CARTESIAN_POINT('Ctrl Pts',(-0.20533552647555,0.674589430258686,
-3.61977673784301));
#60759=CARTESIAN_POINT('Ctrl Pts',(-0.501927281124956,0.495280306801541,
-3.6039698525249));
#60760=CARTESIAN_POINT('Ctrl Pts',(-0.677266731001841,0.19632461109843,
-3.58816296720682));
#60761=CARTESIAN_POINT('Ctrl Pts',(-0.688996520342533,-0.150057898161934,
-3.57235608188872));
#60762=CARTESIAN_POINT('Ctrl Pts',(-0.534283043471572,-0.460190403314884,
-3.55654919657064));
#60763=CARTESIAN_POINT('Ctrl Pts',(-0.250500968703414,-0.659153125247455,
-3.54074231125254));
#60764=CARTESIAN_POINT('Ctrl Pts',(0.093795489213489,-0.698881952870262,
-3.52493542593445));
#60765=CARTESIAN_POINT('Ctrl Pts',(0.41543344724007,-0.569779456245059,
-3.50912854061636));
#60766=CARTESIAN_POINT('Ctrl Pts',(0.636713714319684,-0.303033370838706,
-3.49332165529827));
#60767=CARTESIAN_POINT('Ctrl Pts',(0.704180852995891,0.0369175313181082,
-3.47751476998018));
#60768=CARTESIAN_POINT('Ctrl Pts',(0.60153659384113,0.367950138082134,-3.46170788466208));
#60769=CARTESIAN_POINT('Ctrl Pts',(0.353577064625491,0.610095760692912,
-3.44590099934399));
#60770=CARTESIAN_POINT('Ctrl Pts',(0.0202027041935265,0.704858445780369,
-3.4300941140259));
#60771=CARTESIAN_POINT('Ctrl Pts',(-0.318052093182595,0.629346044610447,
-3.41428722870781));
#60772=CARTESIAN_POINT('Ctrl Pts',(-0.579473949242324,0.401800348424625,
-3.39848034338972));
#60773=CARTESIAN_POINT('Ctrl Pts',(-0.700910284405168,0.0771903560019862,
-3.38267345807162));
#60774=CARTESIAN_POINT('Ctrl Pts',(-0.653025304273793,-0.266066776999244,
-3.36686657275354));
#60775=CARTESIAN_POINT('Ctrl Pts',(-0.44738674868464,-0.545049240845295,
-3.35105968743544));
#60776=CARTESIAN_POINT('Ctrl Pts',(-0.133671432891043,-0.692362279354891,
-3.33525280211735));
#60777=CARTESIAN_POINT('Ctrl Pts',(0.212335352064805,-0.672418973637837,
-3.31944591679926));
#60778=CARTESIAN_POINT('Ctrl Pts',(0.507047553541136,-0.490037096853488,
-3.30363903148117));
#60779=CARTESIAN_POINT('Ctrl Pts',(0.679270528375343,-0.18927526812906,
-3.28783214616308));
#60780=CARTESIAN_POINT('Ctrl Pts',(0.6873997784289,0.157210440049462,-3.27202526084499));
#60781=CARTESIAN_POINT('Ctrl Pts',(0.529471492723354,0.465718279905297,
-3.25621837552689));
#60782=CARTESIAN_POINT('Ctrl Pts',(0.243636952032847,0.66172094832247,-3.2404114902088));
#60783=CARTESIAN_POINT('Ctrl Pts',(-0.101053807620812,0.697869404552157,
-3.22460460489071));
#60784=CARTESIAN_POINT('Ctrl Pts',(-0.421332650367923,0.565431141323669,
-3.20879771957261));
#60785=CARTESIAN_POINT('Ctrl Pts',(-0.639828711318305,0.29639972674988,
-3.19299083425453));
#60786=CARTESIAN_POINT('Ctrl Pts',(-0.703759143294702,-0.0442339922882071,
-3.17718394893643));
#60787=CARTESIAN_POINT('Ctrl Pts',(-0.597680051307391,-0.374181953217737,
-3.16137706361834));
#60788=CARTESIAN_POINT('Ctrl Pts',(-0.347217327542774,-0.613737488914194,
-3.14557017830025));
#60789=CARTESIAN_POINT('Ctrl Pts',(-0.0128761161877245,-0.705030342238238,
-3.12976329298216));
#60790=CARTESIAN_POINT('Ctrl Pts',(0.324575622972799,-0.6260065836846,-3.11395640766407));
#60791=CARTESIAN_POINT('Ctrl Pts',(0.583618509221664,-0.395756255210866,
-3.09814952234597));
#60792=CARTESIAN_POINT('Ctrl Pts',(0.701674658922178,-0.0699017229479336,
-3.08234263702789));
#60793=CARTESIAN_POINT('Ctrl Pts',(0.650224840739586,0.272839209663541,
-3.06653575170979));
#60794=CARTESIAN_POINT('Ctrl Pts',(0.441697964735771,0.549669433198649,
-3.0507288663917));
#60795=CARTESIAN_POINT('Ctrl Pts',(0.126468587690317,0.693714115592484,
-3.03492198107361));
#60796=CARTESIAN_POINT('Ctrl Pts',(-0.219312242355004,0.6701758860164,-3.01911509575552));
#60797=CARTESIAN_POINT('Ctrl Pts',(-0.51211305746562,0.484740955787583,
-3.00330821043742));
#60798=CARTESIAN_POINT('Ctrl Pts',(-0.681200954676895,0.182205480685776,
-2.98750132511933));
#60799=CARTESIAN_POINT('Ctrl Pts',(-0.685728787366566,-0.164346000929208,
-2.97169443980124));
#60800=CARTESIAN_POINT('Ctrl Pts',(-0.524602751372391,-0.471195852164642,
-2.95588755448315));
#60801=CARTESIAN_POINT('Ctrl Pts',(-0.236746619036826,-0.664217295935056,
-2.94008066916506));
#60802=CARTESIAN_POINT('Ctrl Pts',(0.108301210750851,-0.696781476213702,
-2.92427378384697));
#60803=CARTESIAN_POINT('Ctrl Pts',(0.427186343456901,-0.56102175163586,
-2.90846689852887));
#60804=CARTESIAN_POINT('Ctrl Pts',(0.642874597533564,-0.289734067190421,
-2.89266001321078));
#60805=CARTESIAN_POINT('Ctrl Pts',(0.703261417396002,0.0515456753453884,
-2.87685312789269));
#60806=CARTESIAN_POINT('Ctrl Pts',(0.593758950657057,0.38037335127382,-2.8610462425746));
#60807=CARTESIAN_POINT('Ctrl Pts',(0.340820085951307,0.617312924582654,
-2.84523935725651));
#60808=CARTESIAN_POINT('Ctrl Pts',(0.00554813737457995,0.705126085190668,
-2.82943247193842));
#60809=CARTESIAN_POINT('Ctrl Pts',(-0.33106409388682,0.622599504965708,
-2.81362558662032));
#60810=CARTESIAN_POINT('Ctrl Pts',(-0.587700029934952,0.389669414579977,
-2.79781870130224));
#60811=CARTESIAN_POINT('Ctrl Pts',(-0.702363242396234,0.062605539493679,
-2.78201181598414));
#60812=CARTESIAN_POINT('Ctrl Pts',(-0.647354143489211,-0.279582171734887,
-2.76620493066605));
#60813=CARTESIAN_POINT('Ctrl Pts',(-0.435961470998621,-0.554230253278693,
-2.75039804534796));
#60814=CARTESIAN_POINT('Ctrl Pts',(-0.11925208204733,-0.694991020641291,
-2.73459116002987));
#60815=CARTESIAN_POINT('Ctrl Pts',(0.226265443741279,-0.667860409676459,
-2.71878427471177));
#60816=CARTESIAN_POINT('Ctrl Pts',(0.517123245750236,-0.479392455665905,
-2.70297738939368));
#60817=CARTESIAN_POINT('Ctrl Pts',(0.683057801392575,-0.17511601240717,
-2.68717050407559));
#60818=CARTESIAN_POINT('Ctrl Pts',(0.683983727646747,0.17146381005654,-2.6713636187575));
#60819=CARTESIAN_POINT('Ctrl Pts',(0.519677345313422,0.47662252843591,-2.65555673343941));
#60820=CARTESIAN_POINT('Ctrl Pts',(0.229830713971266,0.666641898443312,
-2.63974984812131));
#60821=CARTESIAN_POINT('Ctrl Pts',(-0.115536915778911,0.695618285367013,
-2.62394296280322));
#60822=CARTESIAN_POINT('Ctrl Pts',(-0.432993894223229,0.556551763459652,
-2.60813607748513));
#60823=CARTESIAN_POINT('Ctrl Pts',(-0.645851043965561,0.283037112148287,
-2.59232919216704));
#60824=CARTESIAN_POINT('Ctrl Pts',(-0.70268772906141,-0.0588517907218158,
-2.57652230684895));
#60825=CARTESIAN_POINT('Ctrl Pts',(-0.589773715425885,-0.386523663489563,
-2.56071542153086));
#60826=CARTESIAN_POINT('Ctrl Pts',(-0.334386030845991,-0.620821681499372,
-2.54490853621277));
#60827=CARTESIAN_POINT('Ctrl Pts',(0.00178044071789455,-0.705145664296035,
-2.52910165089467));
#60828=CARTESIAN_POINT('Ctrl Pts',(0.337516805075675,-0.619125176467695,
-2.51329476557658));
#60829=CARTESIAN_POINT('Ctrl Pts',(0.591718070518745,-0.383540483999043,
-2.49748788025849));
#60830=CARTESIAN_POINT('Ctrl Pts',(0.702975960450328,-0.0553025937328847,
-2.4816809949404));
#60831=CARTESIAN_POINT('Ctrl Pts',(0.644413522599621,0.286294934875548,
-2.46587410962231));
#60832=CARTESIAN_POINT('Ctrl Pts',(0.430177887097737,0.558731208450694,
-2.45006722430421));
#60833=CARTESIAN_POINT('Ctrl Pts',(0.112022695449392,0.69619285657704,-2.43426033898612));
#60834=CARTESIAN_POINT('Ctrl Pts',(-0.233194205177004,0.665472794723054,
-2.41845345366803));
#60835=CARTESIAN_POINT('Ctrl Pts',(-0.522077577221963,0.473992174204058,
-2.40264656834994));
#60836=CARTESIAN_POINT('Ctrl Pts',(-0.684840867956002,0.168007629058669,
-2.38683968303185));
#60837=CARTESIAN_POINT('Ctrl Pts',(-0.682164787761207,-0.178563098604814,
-2.37103279771376));
#60838=CARTESIAN_POINT('Ctrl Pts',(-0.514695806561756,-0.481997722559338,
-2.35522591239567));
#60839=CARTESIAN_POINT('Ctrl Pts',(-0.222889983854245,-0.668994493954996,
-2.33941902707757));
#60840=CARTESIAN_POINT('Ctrl Pts',(0.122760141143874,-0.694379957653575,
-2.32361214175949));
#60841=CARTESIAN_POINT('Ctrl Pts',(0.438754675367169,-0.55202165961862,
-2.30780525644139));
#60842=CARTESIAN_POINT('Ctrl Pts',(0.648757729114897,-0.276309584991779,
-2.2919983711233));
#60843=CARTESIAN_POINT('Ctrl Pts',(0.702038140257588,0.0661515492510317,
-2.2761914858052));
#60844=CARTESIAN_POINT('Ctrl Pts',(0.585724776077096,0.392632225542023,
-2.26038460048712));
#60845=CARTESIAN_POINT('Ctrl Pts',(0.327915857198116,0.624263380667703,
-2.24457771516902));
#60846=CARTESIAN_POINT('Ctrl Pts',(-0.0091088264969462,0.705089077439507,
-2.22877082985093));
#60847=CARTESIAN_POINT('Ctrl Pts',(-0.343933059552939,0.615583973468446,
-2.21296394453284));
#60848=CARTESIAN_POINT('Ctrl Pts',(-0.595672196966363,0.377370125481488,
-2.19715705921475));
#60849=CARTESIAN_POINT('Ctrl Pts',(-0.703512746902021,0.0479936744896455,
-2.18135017389665));
#60850=CARTESIAN_POINT('Ctrl Pts',(-0.641403295700533,-0.292976774009718,
-2.16554328857857));
#60851=CARTESIAN_POINT('Ctrl Pts',(-0.424347837744089,-0.563171812546191,
-2.14973640326047));
#60852=CARTESIAN_POINT('Ctrl Pts',(-0.104781208775136,-0.697319493584015,
-2.13392951794238));
#60853=CARTESIAN_POINT('Ctrl Pts',(0.240097778255422,-0.663013299053236,
-2.11812263262429));
#60854=CARTESIAN_POINT('Ctrl Pts',(0.526975516741124,-0.46854069471079,
-2.1023157473062));
#60855=CARTESIAN_POINT('Ctrl Pts',(0.68654996177012,-0.160881098448797,
-2.08650886198811));
#60856=CARTESIAN_POINT('Ctrl Pts',(0.680272164181842,0.185643099747873,
-2.07070197667002));
#60857=CARTESIAN_POINT('Ctrl Pts',(0.509658673195849,0.48732085393598,-2.05489509135192));
#60858=CARTESIAN_POINT('Ctrl Pts',(0.215925178385313,0.671274828355656,
-2.03908820603383));
#60859=CARTESIAN_POINT('Ctrl Pts',(-0.129970106632608,0.693066626830752,
-2.02328132071574));
#60860=CARTESIAN_POINT('Ctrl Pts',(-0.444468064640782,0.547431929429699,
-2.00747443539765));
#60861=CARTESIAN_POINT('Ctrl Pts',(-0.651594339017406,0.269552212391435,
-1.99166755007956));
#60862=CARTESIAN_POINT('Ctrl Pts',(-0.701312721149553,-0.0734441624532127,
-1.97586066476146));
#60863=CARTESIAN_POINT('Ctrl Pts',(-0.581612569954882,-0.398698377617872,
-1.96005377944337));
#60864=CARTESIAN_POINT('Ctrl Pts',(-0.321410263880308,-0.627637650334202,
-1.94424689412528));
#60865=CARTESIAN_POINT('Ctrl Pts',(0.0164362283905885,-0.704956330733284,
-1.92844000880719));
#60866=CARTESIAN_POINT('Ctrl Pts',(0.350312164270045,-0.611976278469258,
-1.9126331234891));
#60867=CARTESIAN_POINT('Ctrl Pts',(0.599561982174783,-0.37115900551555,
-1.896826238171));
#60868=CARTESIAN_POINT('Ctrl Pts',(0.70397354377059,-0.0406795712332764,
-1.88101935285292));
#60869=CARTESIAN_POINT('Ctrl Pts',(0.638323787940124,0.29962696740183,-1.86521246753482));
#60870=CARTESIAN_POINT('Ctrl Pts',(0.41847195266759,0.567551585915519,-1.84940558221673));
#60871=CARTESIAN_POINT('Ctrl Pts',(0.0975284042101817,0.698370809969075,
-1.83359869689864));
#60872=CARTESIAN_POINT('Ctrl Pts',(-0.246975417290485,0.660482188328222,
-1.81779181158055));
#60873=CARTESIAN_POINT('Ctrl Pts',(-0.531816535259198,0.46303860602497,
-1.80198492626245));
#60874=CARTESIAN_POINT('Ctrl Pts',(-0.688184898228003,0.153737190346249,
-1.78617804094436));
#60875=CARTESIAN_POINT('Ctrl Pts',(-0.678306061339454,-0.192703048742882,
-1.77037115562627));
#60876=CARTESIAN_POINT('Ctrl Pts',(-0.504566489299185,-0.492591347590416,
-1.75456427030818));
#60877=CARTESIAN_POINT('Ctrl Pts',(-0.208937049864503,-0.6734826553361,
-1.73875738499009));
#60878=CARTESIAN_POINT('Ctrl Pts',(0.137166033464237,-0.691678434757318,
-1.722950499672));
#60879=CARTESIAN_POINT('Ctrl Pts',(0.450133444915136,-0.542783068650339,
-1.70714361435391));
#60880=CARTESIAN_POINT('Ctrl Pts',(0.654360567278065,-0.262765724241526,
-1.69133672903581));
#60881=CARTESIAN_POINT('Ctrl Pts',(0.700511550093094,0.0807288426203301,
-1.67552984371772));
#60882=CARTESIAN_POINT('Ctrl Pts',(0.577437541237162,0.404721464484683,
-1.65972295839963));
#60883=CARTESIAN_POINT('Ctrl Pts',(0.314869953591033,0.630944126028784,
-1.64391607308154));
#60884=CARTESIAN_POINT('Ctrl Pts',(-0.0237618549331032,0.704747438515944,
-1.62810918776345));
#60885=CARTESIAN_POINT('Ctrl Pts',(-0.356653430191126,0.608302481153537,
-1.61230230244536));
#60886=CARTESIAN_POINT('Ctrl Pts',(-0.603387005990771,0.364907794992297,
-1.59649541712726));
#60887=CARTESIAN_POINT('Ctrl Pts',(-0.704358301283286,0.0333610739930403,
-1.58068853180917));
#60888=CARTESIAN_POINT('Ctrl Pts',(-0.63517533194991,-0.306244796734519,
-1.56488164649108));
#60889=CARTESIAN_POINT('Ctrl Pts',(-0.412550866549072,-0.571870055479614,
-1.54907476117299));
#60890=CARTESIAN_POINT('Ctrl Pts',(-0.0902650651626452,-0.699346692174796,
-1.5332678758549));
#60891=CARTESIAN_POINT('Ctrl Pts',(0.253826379397398,-0.65787973594469,
-1.5174609905368));
#60892=CARTESIAN_POINT('Ctrl Pts',(0.536600109875943,-0.457486502452008,
-1.50165410521871));
#60893=CARTESIAN_POINT('Ctrl Pts',(0.689745500732789,-0.146576676396754,
-1.48584721990062));
#60894=CARTESIAN_POINT('Ctrl Pts',(0.67626669160168,0.199742183012912,-1.47004033458253));
#60895=CARTESIAN_POINT('Ctrl Pts',(0.499419804901498,0.497808634232871,
-1.45423344926444));
#60896=CARTESIAN_POINT('Ctrl Pts',(0.201926353111081,0.675617736418978,
-1.43842656394635));
#60897=CARTESIAN_POINT('Ctrl Pts',(-0.144347144374269,0.690215531378164,
-1.42261967862825));
#60898=CARTESIAN_POINT('Ctrl Pts',(-0.455750204246968,0.538075579424947,
-1.40681279331016));
#60899=CARTESIAN_POINT('Ctrl Pts',(-0.657056115104094,0.255950853581234,
-1.39100590799207));
#60900=CARTESIAN_POINT('Ctrl Pts',(-0.699634713626303,-0.088004802901243,
-1.37519902267398));
#60901=CARTESIAN_POINT('Ctrl Pts',(-0.573200140887612,-0.410700835561685,
-1.35939213735589));
#60902=CARTESIAN_POINT('Ctrl Pts',(-0.308295632778683,-0.634182450604112,
-1.3435852520378));
#60903=CARTESIAN_POINT('Ctrl Pts',(0.0310849148505515,-0.704462423350869,
-1.3277783667197));
#60904=CARTESIAN_POINT('Ctrl Pts',(0.362956172367475,-0.604562978344687,
-1.31197148140161));
#60905=CARTESIAN_POINT('Ctrl Pts',(0.607146855256262,-0.358617169133155,
-1.29616459608352));
#60906=CARTESIAN_POINT('Ctrl Pts',(0.704666977880717,-0.026038973272816,
-1.28035771076543));
#60907=CARTESIAN_POINT('Ctrl Pts',(0.631958267808816,0.312829547186207,
-1.26455082544734));
#60908=CARTESIAN_POINT('Ctrl Pts',(0.40658521895174,0.57612675478111,-1.24874394012925));
#60909=CARTESIAN_POINT('Ctrl Pts',(0.0829919761785184,0.700247034791744,
-1.23293705481115));
#60910=CARTESIAN_POINT('Ctrl Pts',(-0.26064992457286,0.655206223005252,
-1.21713016949306));
#60911=CARTESIAN_POINT('Ctrl Pts',(-0.541325723895911,0.45188498369963,
-1.20132328417497));
#60912=CARTESIAN_POINT('Ctrl Pts',(-0.691231600716771,0.139400330039688,
-1.18551639885688));
#60913=CARTESIAN_POINT('Ctrl Pts',(-0.674154275250033,-0.206759742229352,
-1.16970951353879));
#60914=CARTESIAN_POINT('Ctrl Pts',(-0.494219175919373,-0.502972150320693,
-1.15390262822069));
#60915=CARTESIAN_POINT('Ctrl Pts',(-0.194893845382005,-0.677679840984561,
-1.1380957429026));
#60916=CARTESIAN_POINT('Ctrl Pts',(0.15151266369854,-0.688678074708074,
-1.12228885758451));
#60917=CARTESIAN_POINT('Ctrl Pts',(0.461317735944786,-0.533309970230656,
-1.10648197226642));
#60918=CARTESIAN_POINT('Ctrl Pts',(0.659680691337217,-0.249108336515458,
-1.09067508694833));
#60919=CARTESIAN_POINT('Ctrl Pts',(0.698682306460244,0.0952712573866783,
-1.07486820163024));
#60920=CARTESIAN_POINT('Ctrl Pts',(0.568900826606944,0.41663584499006,-1.05906131631215));
#60921=CARTESIAN_POINT('Ctrl Pts',(0.301688011565286,0.637352274274148,
-1.04325443099405));
#60922=CARTESIAN_POINT('Ctrl Pts',(-0.0384046171462246,0.704101316023837,
-1.02744754567596));
#60923=CARTESIAN_POINT('Ctrl Pts',(-0.369219710011492,0.600758173963263,
-1.01164066035787));
#60924=CARTESIAN_POINT('Ctrl Pts',(-0.610841123852988,0.352287807416983,
-0.99583377503978));
#60925=CARTESIAN_POINT('Ctrl Pts',(-0.704899540221332,0.0187140599657082,
-0.980026889721685));
#60926=CARTESIAN_POINT('Ctrl Pts',(-0.62867294300644,-0.319380507508313,
-0.964220004403597));
#60927=CARTESIAN_POINT('Ctrl Pts',(-0.400575654252081,-0.580321224034726,
-0.948413119085501));
#60928=CARTESIAN_POINT('Ctrl Pts',(-0.07570992285693,-0.701071740569853,
-0.932606233767413));
#60929=CARTESIAN_POINT('Ctrl Pts',(0.267445315774999,-0.652461938288095,
-0.916799348449319));
#60930=CARTESIAN_POINT('Ctrl Pts',(0.545992866884217,-0.446234654813134,
-0.900992463131228));
#60931=CARTESIAN_POINT('Ctrl Pts',(0.69264303765959,-0.132208926424586,
-0.885185577813137));
#60932=CARTESIAN_POINT('Ctrl Pts',(0.671969040456129,0.213754968393986,
-0.869378692495044));
#60933=CARTESIAN_POINT('Ctrl Pts',(0.488965164096191,0.508081338119234,
-0.853571807176953));
#60934=CARTESIAN_POINT('Ctrl Pts',(0.187840286290136,0.679668746295639,
-0.837764921858861));
#60935=CARTESIAN_POINT('Ctrl Pts',(-0.158661817457009,0.687066230814675,
-0.821958036540769));
#60936=CARTESIAN_POINT('Ctrl Pts',(-0.466835438634391,0.528486755822397,
-0.806151151222678));
#60937=CARTESIAN_POINT('Ctrl Pts',(-0.662234012485122,0.242238912135313,
-0.790344265904586));
#60938=CARTESIAN_POINT('Ctrl Pts',(-0.697654431468708,-0.102527421194134,
-0.774537380586495));
#60939=CARTESIAN_POINT('Ctrl Pts',(-0.564540062783472,-0.422525851702685,
-0.758730495268403));
#60940=CARTESIAN_POINT('Ctrl Pts',(-0.295047803669792,-0.640453254651953,
-0.742923609950312));
#60941=CARTESIAN_POINT('Ctrl Pts',(0.045720171186077,-0.703664155539672,
-0.727116724632219));
#60942=CARTESIAN_POINT('Ctrl Pts',(0.375443366570243,-0.596888478983344,
-0.711309839314129));
#60943=CARTESIAN_POINT('Ctrl Pts',(0.614469412746345,-0.345920393506668,
-0.695502953996035));
#60944=CARTESIAN_POINT('Ctrl Pts',(0.705055963185025,-0.0113871252686242,
-0.679696068677945));
#60945=CARTESIAN_POINT('Ctrl Pts',(0.625319712405524,0.325896970102082,
-0.663889183359852));
#60946=CARTESIAN_POINT('Ctrl Pts',(0.394522821570273,0.584453010176933,
-0.648082298041761));
#60947=CARTESIAN_POINT('Ctrl Pts',(0.0684196917652833,0.701820720428935,
-0.632275412723669));
#60948=CARTESIAN_POINT('Ctrl Pts',(-0.274211819002972,0.649647178215781,
-0.616468527405578));
#60949=CARTESIAN_POINT('Ctrl Pts',(-0.550601034721718,0.440536126110014,
-0.600661642087486));
#60950=CARTESIAN_POINT('Ctrl Pts',(-0.693979659105578,0.125003242327362,
-0.584854756769395));
#60951=CARTESIAN_POINT('Ctrl Pts',(-0.669711223257026,-0.220727105920912,
-0.569047871451302));
#60952=CARTESIAN_POINT('Ctrl Pts',(-0.483658336941455,-0.513135645762089,
-0.55324098613321));
#60953=CARTESIAN_POINT('Ctrl Pts',(-0.18076643772218,-0.681584237521583,
-0.537434100815119));
#60954=CARTESIAN_POINT('Ctrl Pts',(0.165793833437332,-0.685380173800492,
-0.521627215497027));
#60955=CARTESIAN_POINT('Ctrl Pts',(0.47230271632388,-0.523606457177304,
-0.505820330178935));
#60956=CARTESIAN_POINT('Ctrl Pts',(0.66471580275202,-0.235343322438281,
-0.490013444860844));
#60957=CARTESIAN_POINT('Ctrl Pts',(0.696551199677241,0.109772510552645,
-0.474206559542751));
#60958=CARTESIAN_POINT('Ctrl Pts',(0.560118320442681,0.428370219493409,
-0.458399674224661));
#60959=CARTESIAN_POINT('Ctrl Pts',(0.288375726331517,0.643485056786609,
-0.442592788906568));
#60960=CARTESIAN_POINT('Ctrl Pts',(-0.0530307867851691,0.703150989118139,
-0.426785903588478));
#60961=CARTESIAN_POINT('Ctrl Pts',(-0.381626469796513,0.59295431138796,
-0.410979018270385));
#60962=CARTESIAN_POINT('Ctrl Pts',(-0.618031330032434,0.339515615175607,
-0.395172132952294));
#60963=CARTESIAN_POINT('Ctrl Pts',(-0.705136229868134,0.00405896059619597,
-0.379365247634201));
#60964=CARTESIAN_POINT('Ctrl Pts',(-0.621898938218708,-0.332378231093819,
-0.36355836231611));
#60965=CARTESIAN_POINT('Ctrl Pts',(-0.388427374670541,-0.588521666917222,
-0.347751476998018));
#60966=CARTESIAN_POINT('Ctrl Pts',(-0.0611220704120482,-0.702493893463718,
-0.331944591679926));
#60967=CARTESIAN_POINT('Ctrl Pts',(0.280948703489239,-0.646762246832194,
-0.316137706361835));
#60968=CARTESIAN_POINT('Ctrl Pts',(0.555149729438401,-0.434790013096512,
-0.300330821043743));
#60969=CARTESIAN_POINT('Ctrl Pts',(0.695241321112673,-0.117784056100728,
-0.284523935725652));
#60970=CARTESIAN_POINT('Ctrl Pts',(0.667381066683655,0.227675401785218,
-0.268717050407559));
#60971=CARTESIAN_POINT('Ctrl Pts',(0.47829926932486,0.518134527179428,-0.252910165089469));
#60972=CARTESIAN_POINT('Ctrl Pts',(0.173673060517654,0.683426108018395,
-0.237103279771376));
#60973=CARTESIAN_POINT('Ctrl Pts',(-0.172907934941646,0.683620085281621,
-0.221296394453285));
#60974=CARTESIAN_POINT('Ctrl Pts',(-0.477718990865722,0.518669602421621,
-0.205489509135192));
#60975=CARTESIAN_POINT('Ctrl Pts',(-0.667125769812111,0.228422310324478,
-0.189682623817101));
#60976=CARTESIAN_POINT('Ctrl Pts',(-0.695372777708953,-0.117005739123839,
-0.173875738499009));
#60977=CARTESIAN_POINT('Ctrl Pts',(-0.555635984344507,-0.434168324449232,
-0.158068853180918));
#60978=CARTESIAN_POINT('Ctrl Pts',(-0.281672681898704,-0.646447338792661,
-0.142261967862826));
#60979=CARTESIAN_POINT('Ctrl Pts',(0.0603360297254143,-0.702561900375898,
-0.126455082544735));
#60980=CARTESIAN_POINT('Ctrl Pts',(0.38776765641086,-0.588956040974949,
-0.110648197226643));
#60981=CARTESIAN_POINT('Ctrl Pts',(0.621527851581432,-0.333074272139639,
-0.0948413119085513));
#60982=CARTESIAN_POINT('Ctrl Pts',(0.705137669332003,0.00326985369309036,
-0.0790344265904595));
#60983=CARTESIAN_POINT('Ctrl Pts',(0.618416201049889,0.338823176482188,
-0.0632275412723679));
#60984=CARTESIAN_POINT('Ctrl Pts',(0.38227975109817,0.59252757256583,-0.0474206559542765));
#60985=CARTESIAN_POINT('Ctrl Pts',(0.0538381161213402,0.703089501623881,
-0.0316137706361843));
#60986=CARTESIAN_POINT('Ctrl Pts',(-0.287697821498663,0.643811669165333,
-0.015806885318092));
#60987=CARTESIAN_POINT('Ctrl Pts',(-0.468914126304642,0.500589151378386,
-0.00526896177269799));
#60988=CARTESIAN_POINT('Ctrl Pts',(-0.537060862935893,0.41168983410154,
-8.88178419700125E-16));
#60989=CARTESIAN_POINT('Ctrl Pts',(-0.309090610374634,0.644553868208609,
-3.9929325805302));
#60990=CARTESIAN_POINT('Ctrl Pts',(-0.415783171285996,0.593390310900079,
-3.9876636187575));
#60991=CARTESIAN_POINT('Ctrl Pts',(-0.603169422965529,0.437118654161456,
-3.9771256952121));
#60992=CARTESIAN_POINT('Ctrl Pts',(-0.738555843335368,0.0968903284536621,
-3.96131880989401));
#60993=CARTESIAN_POINT('Ctrl Pts',(-0.695515856557493,-0.266650958314697,
-3.94551192457592));
#60994=CARTESIAN_POINT('Ctrl Pts',(-0.484463476114247,-0.565822143893725,
-3.92970503925783));
#60995=CARTESIAN_POINT('Ctrl Pts',(-0.156374615331088,-0.728282548610733,
-3.91389815393974));
#60996=CARTESIAN_POINT('Ctrl Pts',(0.209488682519811,-0.714821053454846,
-3.89809126862164));
#60997=CARTESIAN_POINT('Ctrl Pts',(0.524745852793018,-0.528671726788554,
-3.88228438330356));
#60998=CARTESIAN_POINT('Ctrl Pts',(0.713237960522051,-0.214812436248472,
-3.86647749798546));
#60999=CARTESIAN_POINT('Ctrl Pts',(0.72943091647052,0.150941414303679,-3.85067061266737));
#61000=CARTESIAN_POINT('Ctrl Pts',(0.56941262601771,0.4802310197843,-3.83486372734927));
#61001=CARTESIAN_POINT('Ctrl Pts',(0.271839416195556,0.693509973619221,
-3.81905684203119));
#61002=CARTESIAN_POINT('Ctrl Pts',(-0.0914030062187122,0.73925511996695,
-3.80324995671309));
#61003=CARTESIAN_POINT('Ctrl Pts',(-0.432564875275732,0.60641596455938,
-3.78744307139501));
#61004=CARTESIAN_POINT('Ctrl Pts',(-0.66923056229026,0.327082757606315,
-3.77163618607691));
#61005=CARTESIAN_POINT('Ctrl Pts',(-0.744227910150822,-0.0312649312745136,
-3.75582930075882));
#61006=CARTESIAN_POINT('Ctrl Pts',(-0.639439556283001,-0.382059857240302,
-3.74002241544073));
#61007=CARTESIAN_POINT('Ctrl Pts',(-0.380179582021205,-0.640559258169556,
-3.72421553012264));
#61008=CARTESIAN_POINT('Ctrl Pts',(-0.0290783151292548,-0.74431655315994,
-3.70840864480454));
#61009=CARTESIAN_POINT('Ctrl Pts',(0.329047500904973,-0.668266728856064,
-3.69260175948646));
#61010=CARTESIAN_POINT('Ctrl Pts',(0.607684176922999,-0.430781406562343,
-3.67679487416836));
#61011=CARTESIAN_POINT('Ctrl Pts',(0.739520490092536,-0.0892307333413812,
-3.66098798885027));
#61012=CARTESIAN_POINT('Ctrl Pts',(0.692708287355583,0.273875715690588,
-3.64518110353218));
#61013=CARTESIAN_POINT('Ctrl Pts',(0.478556154062485,0.570821063440742,
-3.62937421821409));
#61014=CARTESIAN_POINT('Ctrl Pts',(0.14879755977588,0.729871197699466,-3.613567332896));
#61015=CARTESIAN_POINT('Ctrl Pts',(-0.21690657431989,0.712603828968895,
-3.5977604475779));
#61016=CARTESIAN_POINT('Ctrl Pts',(-0.530211839009143,0.523190295027787,
-3.58195356225981));
#61017=CARTESIAN_POINT('Ctrl Pts',(-0.715432000706095,0.207387876705873,
-3.56614667694172));
#61018=CARTESIAN_POINT('Ctrl Pts',(-0.727822786007864,-0.158513946410649,
-3.55033979162363));
#61019=CARTESIAN_POINT('Ctrl Pts',(-0.564390910164421,-0.48612300867384,
-3.53453290630553));
#61020=CARTESIAN_POINT('Ctrl Pts',(-0.264617175205399,-0.696297658781914,
-3.51872602098745));
#61021=CARTESIAN_POINT('Ctrl Pts',(0.0990810436029352,-0.738265281478883,
-3.50291913566935));
#61022=CARTESIAN_POINT('Ctrl Pts',(0.438843912913809,-0.601887613377435,
-3.48711225035126));
#61023=CARTESIAN_POINT('Ctrl Pts',(0.672593744327157,-0.320109878214677,
-3.47130536503317));
#61024=CARTESIAN_POINT('Ctrl Pts',(0.743862784714884,0.0389979044932149,
-3.45549847971508));
#61025=CARTESIAN_POINT('Ctrl Pts',(0.635434326137781,0.388684828883862,
-3.43969159439698));
#61026=CARTESIAN_POINT('Ctrl Pts',(0.373501805373811,0.644475818337002,
-3.4238847090789));
#61027=CARTESIAN_POINT('Ctrl Pts',(0.0213411650376951,0.744578561142801,
-3.4080778237608));
#61028=CARTESIAN_POINT('Ctrl Pts',(-0.335974934155985,0.664810892402891,
-3.39227093844271));
#61029=CARTESIAN_POINT('Ctrl Pts',(-0.612128409511927,0.424442563024784,
-3.37646405312462));
#61030=CARTESIAN_POINT('Ctrl Pts',(-0.740407913357411,0.0815401795213381,
-3.36065716780653));
#61031=CARTESIAN_POINT('Ctrl Pts',(-0.689824523429956,-0.281060146433609,
-3.34485028248844));
#61032=CARTESIAN_POINT('Ctrl Pts',(-0.472597843728988,-0.575763803257342,
-3.32904339717034));
#61033=CARTESIAN_POINT('Ctrl Pts',(-0.141204072624427,-0.731378211948458,
-3.31323651185225));
#61034=CARTESIAN_POINT('Ctrl Pts',(0.224300853407697,-0.710311062985242,
-3.29742962653416));
#61035=CARTESIAN_POINT('Ctrl Pts',(0.535620648524191,-0.517651620216892,
-3.28162274121607));
#61036=CARTESIAN_POINT('Ctrl Pts',(0.717548715876518,-0.199941289839307,
-3.26581585589798));
#61037=CARTESIAN_POINT('Ctrl Pts',(0.726136064647445,0.166069547650886,
-3.25000897057989));
#61038=CARTESIAN_POINT('Ctrl Pts',(0.559308219371084,0.491962391634354,
-3.23420208526179));
#61039=CARTESIAN_POINT('Ctrl Pts',(0.257366358127407,0.699010183575949,
-3.21839519994371));
#61040=CARTESIAN_POINT('Ctrl Pts',(-0.106748382071239,0.737195674135314,
-3.20258831462561));
#61041=CARTESIAN_POINT('Ctrl Pts',(-0.445075547369097,0.5972942626317,-3.18678142930752));
#61042=CARTESIAN_POINT('Ctrl Pts',(-0.675884277337126,0.313102415652,-3.17097454398943));
#61043=CARTESIAN_POINT('Ctrl Pts',(-0.743417310869164,-0.0467266619684013,
-3.15516765867134));
#61044=CARTESIAN_POINT('Ctrl Pts',(-0.631360460089998,-0.39526781866678,
-3.13936077335324));
#61045=CARTESIAN_POINT('Ctrl Pts',(-0.366783684998515,-0.648322764876845,
-3.12355388803515));
#61046=CARTESIAN_POINT('Ctrl Pts',(-0.0136017098490641,-0.744760144293335,
-3.10774700271706));
#61047=CARTESIAN_POINT('Ctrl Pts',(0.342866077269672,-0.661283246496049,
-3.09194011739897));
#61048=CARTESIAN_POINT('Ctrl Pts',(0.616506523336708,-0.418057873651402,
-3.07613323208088));
#61049=CARTESIAN_POINT('Ctrl Pts',(0.741215361833708,-0.0738408181182466,
-3.06032634676279));
#61050=CARTESIAN_POINT('Ctrl Pts',(0.686866248443941,0.288214218572216,
-3.04451946144469));
#61051=CARTESIAN_POINT('Ctrl Pts',(0.466588485974026,0.580644352245946,
-3.0287125761266));
#61052=CARTESIAN_POINT('Ctrl Pts',(0.133595333383524,0.732806226731728,
-3.01290569080851));
#61053=CARTESIAN_POINT('Ctrl Pts',(-0.231670904748681,0.707941573105843,
-2.99709880549042));
#61054=CARTESIAN_POINT('Ctrl Pts',(-0.540971603238765,0.512057031518881,
-2.98129192017233));
#61055=CARTESIAN_POINT('Ctrl Pts',(-0.719587925375399,0.192473106413799,
-2.96548503485424));
#61056=CARTESIAN_POINT('Ctrl Pts',(-0.724370910057438,-0.173607210971222,
-2.94967814953614));
#61057=CARTESIAN_POINT('Ctrl Pts',(-0.554165115175655,-0.497748635518974,
-2.93387126421806));
#61058=CARTESIAN_POINT('Ctrl Pts',(-0.25008774174892,-0.701647205129168,
-2.91806437889996));
#61059=CARTESIAN_POINT('Ctrl Pts',(0.114404190165603,-0.736046438963738,
-2.90225749358187));
#61060=CARTESIAN_POINT('Ctrl Pts',(0.451259107208176,-0.592636395440179,
-2.88645060826378));
#61061=CARTESIAN_POINT('Ctrl Pts',(0.679101805039518,-0.306061133485969,
-2.87064372294568));
#61062=CARTESIAN_POINT('Ctrl Pts',(0.742891537168478,0.0544503722861812,
-2.85483683762759));
#61063=CARTESIAN_POINT('Ctrl Pts',(0.627218397952841,0.401808113790799,
-2.8390299523095));
#61064=CARTESIAN_POINT('Ctrl Pts',(0.360025946664,0.652099683152305,-2.82322306699141));
#61065=CARTESIAN_POINT('Ctrl Pts',(0.00586078547844685,0.744861282543416,
-2.80741618167332));
#61066=CARTESIAN_POINT('Ctrl Pts',(-0.349720185872753,0.65768417240479,
-2.79160929635523));
#61067=CARTESIAN_POINT('Ctrl Pts',(-0.620818045512782,0.411628027962548,
-2.77580241103713));
#61068=CARTESIAN_POINT('Ctrl Pts',(-0.741942748297485,0.0661334808355267,
-2.75999552571904));
#61069=CARTESIAN_POINT('Ctrl Pts',(-0.683833781938139,-0.295337159393851,
-2.74418864040095));
#61070=CARTESIAN_POINT('Ctrl Pts',(-0.46052872989338,-0.585462183220606,
-2.72838175508286));
#61071=CARTESIAN_POINT('Ctrl Pts',(-0.125972163908432,-0.734155087811067,
-2.71257486976477));
#61072=CARTESIAN_POINT('Ctrl Pts',(0.239015932270905,-0.705495615265834,
-2.69676798444668));
#61073=CARTESIAN_POINT('Ctrl Pts',(0.546264125171852,-0.506407133232618,
-2.68096109912858));
#61074=CARTESIAN_POINT('Ctrl Pts',(0.721549408938659,-0.184984133100431,
-2.66515421381049));
#61075=CARTESIAN_POINT('Ctrl Pts',(0.72252751290008,0.181126122194099,-2.6493473284924));
#61076=CARTESIAN_POINT('Ctrl Pts',(0.548962153108043,0.50348111532969,-2.63354044317431));
#61077=CARTESIAN_POINT('Ctrl Pts',(0.24278211226609,0.704208438604838,-2.61773355785622));
#61078=CARTESIAN_POINT('Ctrl Pts',(-0.12204764094767,0.734817700098301,
-2.60192667253813));
#61079=CARTESIAN_POINT('Ctrl Pts',(-0.457393924516876,0.587914514920067,
-2.58611978722003));
#61080=CARTESIAN_POINT('Ctrl Pts',(-0.682245979894656,0.298986792277233,
-2.57031290190194));
#61081=CARTESIAN_POINT('Ctrl Pts',(-0.742285520404017,-0.0621682011737976,
-2.55450601658385));
#61082=CARTESIAN_POINT('Ctrl Pts',(-0.623008587129114,-0.408305007809151,
-2.53869913126576));
#61083=CARTESIAN_POINT('Ctrl Pts',(-0.353229320304042,-0.65580616520142,
-2.52289224594767));
#61084=CARTESIAN_POINT('Ctrl Pts',(0.00188077194203051,-0.744881964968644,
-2.50708536062958));
#61085=CARTESIAN_POINT('Ctrl Pts',(0.356536519622077,-0.654014058881325,
-2.49127847531148));
#61086=CARTESIAN_POINT('Ctrl Pts',(0.625062510333207,-0.405153720474831,
-2.47547158999339));
#61087=CARTESIAN_POINT('Ctrl Pts',(0.742589994180448,-0.05841900017742,
-2.4596647046753));
#61088=CARTESIAN_POINT('Ctrl Pts',(0.680727451462928,0.302428199517563,
-2.44385781935721));
#61089=CARTESIAN_POINT('Ctrl Pts',(0.454419230028622,0.590216775785679,
-2.42805093403912));
#61090=CARTESIAN_POINT('Ctrl Pts',(0.118335387612053,0.735424649489908,
-2.41224404872103));
#61091=CARTESIAN_POINT('Ctrl Pts',(-0.246335142604835,0.70297345366415,
-2.39643716340293));
#61092=CARTESIAN_POINT('Ctrl Pts',(-0.5514976426543,0.500702535629088,-2.38063027808484));
#61093=CARTESIAN_POINT('Ctrl Pts',(-0.723432954697622,0.177475178816966,
-2.36482339276675));
#61094=CARTESIAN_POINT('Ctrl Pts',(-0.720606072289007,-0.188625469168028,
-2.34901650744866));
#61095=CARTESIAN_POINT('Ctrl Pts',(-0.543699895163633,-0.509159211875521,
-2.33320962213057));
#61096=CARTESIAN_POINT('Ctrl Pts',(-0.235450258792885,-0.706693607352586,
-2.31740273681248));
#61097=CARTESIAN_POINT('Ctrl Pts',(0.129677908813866,-0.733509590260626,
-2.30159585149438));
#61098=CARTESIAN_POINT('Ctrl Pts',(0.463479336645923,-0.583129131102968,
-2.28578896617629));
#61099=CARTESIAN_POINT('Ctrl Pts',(0.68531646228604,-0.291880156157272,
-2.2699820808582));
#61100=CARTESIAN_POINT('Ctrl Pts',(0.741599326034383,0.0698793149937588,
-2.2541751955401));
#61101=CARTESIAN_POINT('Ctrl Pts',(0.618731482339459,0.414757798963037,
-2.23836831022202));
#61102=CARTESIAN_POINT('Ctrl Pts',(0.346394540052889,0.659441810670354,
-2.22256142490392));
#61103=CARTESIAN_POINT('Ctrl Pts',(-0.00962212621185803,0.744822189335018,
-2.20675453958584));
#61104=CARTESIAN_POINT('Ctrl Pts',(-0.363314342254702,0.650273302351158,
-2.19094765426774));
#61105=CARTESIAN_POINT('Ctrl Pts',(-0.6292394593342,0.398635650507393,-2.17514076894965));
#61106=CARTESIAN_POINT('Ctrl Pts',(-0.743157029570654,0.0506982094197591,
-2.15933388363156));
#61107=CARTESIAN_POINT('Ctrl Pts',(-0.677547592547065,-0.309486573008144,
-2.14352699831347));
#61108=CARTESIAN_POINT('Ctrl Pts',(-0.448260646294373,-0.594907616376188,
-2.12772011299537));
#61109=CARTESIAN_POINT('Ctrl Pts',(-0.11068582937702,-0.736614774637171,
-2.11191322767728));
#61110=CARTESIAN_POINT('Ctrl Pts',(0.25362774516957,-0.700375360730835,
-2.09610634235919));
#61111=CARTESIAN_POINT('Ctrl Pts',(0.556671590390294,-0.49494385488759,
-2.0802994570411));
#61112=CARTESIAN_POINT('Ctrl Pts',(0.72523835920202,-0.169947054639404,
-2.06449257172301));
#61113=CARTESIAN_POINT('Ctrl Pts',(0.718606795767678,0.196104441854739,
-2.04868568640491));
#61114=CARTESIAN_POINT('Ctrl Pts',(0.538378909742626,0.514782311839664,
-2.03287880108683));
#61115=CARTESIAN_POINT('Ctrl Pts',(0.228092973275854,0.709102442938133,
-2.01707191576873));
#61116=CARTESIAN_POINT('Ctrl Pts',(-0.137294169584562,0.732122250745553,
-2.00126503045064));
#61117=CARTESIAN_POINT('Ctrl Pts',(-0.469514686282523,0.578280760879758,
-1.98545814513255));
#61118=CARTESIAN_POINT('Ctrl Pts',(-0.688312920557029,0.284741992745893,
-1.96965125981446));
#61119=CARTESIAN_POINT('Ctrl Pts',(-0.740833028178523,-0.077582880833902,
-1.95384437449636));
#61120=CARTESIAN_POINT('Ctrl Pts',(-0.614387545573247,-0.421165790257387,
-1.93803748917828));
#61121=CARTESIAN_POINT('Ctrl Pts',(-0.339522344165966,-0.663006226856653,
-1.92223060386018));
#61122=CARTESIAN_POINT('Ctrl Pts',(0.0173624411524594,-0.744681962099172,
-1.90642371854209));
#61123=CARTESIAN_POINT('Ctrl Pts',(0.370052921667457,-0.646462306870266,
-1.890616833224));
#61124=CARTESIAN_POINT('Ctrl Pts',(0.63334844134467,-0.392074522106352,
-1.87480994790591));
#61125=CARTESIAN_POINT('Ctrl Pts',(0.743643793220054,-0.0429719425199595,
-1.85900306258782));
#61126=CARTESIAN_POINT('Ctrl Pts',(0.674294548661445,0.316511517458853,
-1.84319617726972));
#61127=CARTESIAN_POINT('Ctrl Pts',(0.442053643907026,0.599534198313297,
-1.82738929195163));
#61128=CARTESIAN_POINT('Ctrl Pts',(0.103024315466599,0.737725334702074,
-1.81158240663354));
#61129=CARTESIAN_POINT('Ctrl Pts',(-0.260892952258233,0.697701617097619,
-1.79577552131545));
#61130=CARTESIAN_POINT('Ctrl Pts',(-0.56178540951842,0.489131713029189,
-1.77996863599736));
#61131=CARTESIAN_POINT('Ctrl Pts',(-0.726965427441973,0.162400573714369,
-1.76416175067926));
#61132=CARTESIAN_POINT('Ctrl Pts',(-0.716529899286962,-0.203562232416679,
-1.74835486536118));
#61133=CARTESIAN_POINT('Ctrl Pts',(-0.532999771588644,-0.520349807845742,
-1.73254798004308));
#61134=CARTESIAN_POINT('Ctrl Pts',(-0.220711050408569,-0.711434685172289,
-1.71674109472499));
#61135=CARTESIAN_POINT('Ctrl Pts',(0.144895600593098,-0.730655831405877,
-1.7009342094069));
#61136=CARTESIAN_POINT('Ctrl Pts',(0.475499321521354,-0.57336992794476,
-1.68512732408881));
#61137=CARTESIAN_POINT('Ctrl Pts',(0.691235031046653,-0.277573073068302,
-1.66932043877072));
#61138=CARTESIAN_POINT('Ctrl Pts',(0.739986709607724,0.0852780665973542,
-1.65351355345262));
#61139=CARTESIAN_POINT('Ctrl Pts',(0.609977246038668,0.427528289536178,
-1.63770666813453));
#61140=CARTESIAN_POINT('Ctrl Pts',(0.33261347494014,0.666499028751649,-1.62189978281644));
#61141=CARTESIAN_POINT('Ctrl Pts',(-0.025100880697518,0.744461298407685,
-1.60609289749835));
#61142=CARTESIAN_POINT('Ctrl Pts',(-0.376751529995992,0.642581484081456,
-1.59028601218026));
#61143=CARTESIAN_POINT('Ctrl Pts',(-0.637389012534951,0.385471043968764,
-1.57447912686217));
#61144=CARTESIAN_POINT('Ctrl Pts',(-0.744050232551108,0.0352410340269367,
-1.55867224154407));
#61145=CARTESIAN_POINT('Ctrl Pts',(-0.670968671182005,-0.323502274073774,
-1.54286535622598));
#61146=CARTESIAN_POINT('Ctrl Pts',(-0.435798893312887,-0.604096021859034,
-1.52705847090789));
#61147=CARTESIAN_POINT('Ctrl Pts',(-0.0953516734354473,-0.738756209728018,
-1.5112515855898));
#61148=CARTESIAN_POINT('Ctrl Pts',(0.268129979123054,-0.694952511567602,
-1.49544470027171));
#61149=CARTESIAN_POINT('Ctrl Pts',(0.566838547672013,-0.483266737849533,
-1.47963781495361));
#61150=CARTESIAN_POINT('Ctrl Pts',(0.728613972869053,-0.154836551171296,
-1.46383092963552));
#61151=CARTESIAN_POINT('Ctrl Pts',(0.714375607181817,0.210998035304261,
-1.44802404431743));
#61152=CARTESIAN_POINT('Ctrl Pts',(0.527563061726648,0.525861098523415,
-1.43221715899934));
#61153=CARTESIAN_POINT('Ctrl Pts',(0.213305287545797,0.713690082139056,
-1.41641027368125));
#61154=CARTESIAN_POINT('Ctrl Pts',(-0.152481380774647,0.729110490636162,
-1.40060338836316));
#61155=CARTESIAN_POINT('Ctrl Pts',(-0.481432595934987,0.568397162739177,
-1.38479650304506));
#61156=CARTESIAN_POINT('Ctrl Pts',(-0.694082478124588,0.270374171471832,
-1.36898961772697));
#61157=CARTESIAN_POINT('Ctrl Pts',(-0.739060461736668,-0.0929640410924126,
-1.35318273240888));
#61158=CARTESIAN_POINT('Ctrl Pts',(-0.605501060112058,-0.433844609557178,
-1.33737584709079));
#61159=CARTESIAN_POINT('Ctrl Pts',(-0.325668678633513,-0.669919839082071,
-1.3215689617727));
#61160=CARTESIAN_POINT('Ctrl Pts',(0.0328366089833011,-0.744160222095434,
-1.30576207645461));
#61161=CARTESIAN_POINT('Ctrl Pts',(0.383409443693435,-0.638631253169886,
-1.28995519113651));
#61162=CARTESIAN_POINT('Ctrl Pts',(0.64136073646473,-0.37882592936607,-1.27414830581842));
#61163=CARTESIAN_POINT('Ctrl Pts',(0.744376303662479,-0.0275063189909673,
-1.25834142050033));
#61164=CARTESIAN_POINT('Ctrl Pts',(0.66757031935176,0.330458087749772,-1.24253453518224));
#61165=CARTESIAN_POINT('Ctrl Pts',(0.429497070115765,0.608592594270275,
-1.22672764986415));
#61166=CARTESIAN_POINT('Ctrl Pts',(0.0876687320402154,0.739707288365545,
-1.21092076454605));
#61167=CARTESIAN_POINT('Ctrl Pts',(-0.27533804406014,0.692128341084069,
-1.19511387922797));
#61168=CARTESIAN_POINT('Ctrl Pts',(-0.571830459038853,0.477349562851023,
-1.17930699390987));
#61169=CARTESIAN_POINT('Ctrl Pts',(-0.73018381741644,0.147255804034344,
-1.16350010859178));
#61170=CARTESIAN_POINT('Ctrl Pts',(-0.712144152147036,-0.218411047342909,
-1.14769322327369));
#61171=CARTESIAN_POINT('Ctrl Pts',(-0.522069367400179,-0.531315588573331,
-1.1318863379556));
#61172=CARTESIAN_POINT('Ctrl Pts',(-0.205876484617368,-0.715868390222842,
-1.11607945263751));
#61173=CARTESIAN_POINT('Ctrl Pts',(0.160050690754894,-0.72748639535563,
-1.10027256731941));
#61174=CARTESIAN_POINT('Ctrl Pts',(0.487313868643706,-0.563363002393797,
-1.08446568200132));
#61175=CARTESIAN_POINT('Ctrl Pts',(0.696854954225239,-0.263146065542292,
-1.06865879668323));
#61176=CARTESIAN_POINT('Ctrl Pts',(0.738054384613563,0.10063997412232,-1.05285191136514));
#61177=CARTESIAN_POINT('Ctrl Pts',(0.600959471286436,0.440114068066193,
-1.03704502604705));
#61178=CARTESIAN_POINT('Ctrl Pts',(0.318688705384841,0.673268288350774,
-1.02123814072895));
#61179=CARTESIAN_POINT('Ctrl Pts',(-0.0405687904389292,0.743778765683029,
-1.00543125541086));
#61180=CARTESIAN_POINT('Ctrl Pts',(-0.39002594360851,0.634612040817805,
-0.989624370092771));
#61181=CARTESIAN_POINT('Ctrl Pts',(-0.645263184130204,0.372139896067054,
-0.973817484774681));
#61182=CARTESIAN_POINT('Ctrl Pts',(-0.744621971333751,0.0197686328734897,
-0.958010599456587));
#61183=CARTESIAN_POINT('Ctrl Pts',(-0.664099860242016,-0.337378207158056,
-0.942203714138499));
#61184=CARTESIAN_POINT('Ctrl Pts',(-0.423148855003988,-0.61302342985196,
-0.926396828820403));
#61185=CARTESIAN_POINT('Ctrl Pts',(-0.0799763211500396,-0.740578467884366,
-0.910589943502316));
#61186=CARTESIAN_POINT('Ctrl Pts',(0.282516368493905,-0.6892294106984,-0.89478305818422));
#61187=CARTESIAN_POINT('Ctrl Pts',(0.576760604420077,-0.471380827174412,
-0.878976172866131));
#61188=CARTESIAN_POINT('Ctrl Pts',(0.731674791518147,-0.139659151134197,
-0.863169287548039));
#61189=CARTESIAN_POINT('Ctrl Pts',(0.709835775212143,0.22580046781976,-0.847362402229946));
#61190=CARTESIAN_POINT('Ctrl Pts',(0.516519282007925,0.536712688831433,
-0.831555516911855));
#61191=CARTESIAN_POINT('Ctrl Pts',(0.198425444041774,0.717969374134769,
-0.815748631593762));
#61192=CARTESIAN_POINT('Ctrl Pts',(-0.167602712938549,0.725783720990135,
-0.799941746275672));
#61193=CARTESIAN_POINT('Ctrl Pts',(-0.493142504384733,0.55826799067097,
-0.784134860957579));
#61194=CARTESIAN_POINT('Ctrl Pts',(-0.699552159880962,0.255889536019993,
-0.768327975639488));
#61195=CARTESIAN_POINT('Ctrl Pts',(-0.736968586909338,-0.108305036574953,
-0.752521090321397));
#61196=CARTESIAN_POINT('Ctrl Pts',(-0.596352970119284,-0.446335987870746,
-0.736714205003304));
#61197=CARTESIAN_POINT('Ctrl Pts',(-0.311674309132495,-0.67654401487666,
-0.720907319685214));
#61198=CARTESIAN_POINT('Ctrl Pts',(0.0482965898766236,-0.743316970373296,
-0.705100434367121));
#61199=CARTESIAN_POINT('Ctrl Pts',(0.396600315063237,-0.630524281158457,
-0.689293549049029));
#61200=CARTESIAN_POINT('Ctrl Pts',(0.649095934010409,-0.365413666260311,
-0.673486663730938));
#61201=CARTESIAN_POINT('Ctrl Pts',(0.744787209029253,-0.0120288114568608,
-0.657679778412846));
#61202=CARTESIAN_POINT('Ctrl Pts',(0.660557668712699,0.344261884825333,
-0.641872893094754));
#61203=CARTESIAN_POINT('Ctrl Pts',(0.416754933676891,0.617388050009569,
-0.626066007776663));
#61204=CARTESIAN_POINT('Ctrl Pts',(0.0722752716568935,0.74136965418445,
-0.61025912245857));
#61205=CARTESIAN_POINT('Ctrl Pts',(-0.289664177061162,0.686256033537139,
-0.59445223714048));
#61206=CARTESIAN_POINT('Ctrl Pts',(-0.581628451288467,0.465361175529743,
-0.578645351822388));
#61207=CARTESIAN_POINT('Ctrl Pts',(-0.733086734127339,0.132047413019573,
-0.562838466504297));
#61208=CARTESIAN_POINT('Ctrl Pts',(-0.707450725715331,-0.233165498570212,
-0.547031581186204));
#61209=CARTESIAN_POINT('Ctrl Pts',(-0.510913405039632,-0.542051816332592,
-0.531224695868112));
#61210=CARTESIAN_POINT('Ctrl Pts',(-0.190952970639487,-0.719992806938097,
-0.515417810550021));
#61211=CARTESIAN_POINT('Ctrl Pts',(0.17513663159763,-0.724002651453208,
-0.499610925231929));
#61212=CARTESIAN_POINT('Ctrl Pts',(0.498917873580885,-0.553112677905884,
-0.483804039913837));
#61213=CARTESIAN_POINT('Ctrl Pts',(0.702173803754348,-0.248605366715384,
-0.467997154595746));
#61214=CARTESIAN_POINT('Ctrl Pts',(0.735803185906037,0.115958400512358,
-0.452190269277653));
#61215=CARTESIAN_POINT('Ctrl Pts',(0.591682054179269,0.45250969691326,-0.436383383959563));
#61216=CARTESIAN_POINT('Ctrl Pts',(0.304626247533592,0.679746664833693,
-0.42057649864147));
#61217=CARTESIAN_POINT('Ctrl Pts',(-0.0560191725830189,0.742774886046918,
-0.40476961332338));
#61218=CARTESIAN_POINT('Ctrl Pts',(-0.403131847927991,0.626368415729021,
-0.388962728005286));
#61219=CARTESIAN_POINT('Ctrl Pts',(-0.652858572116915,0.358647966476576,
-0.373155842687196));
#61220=CARTESIAN_POINT('Ctrl Pts',(-0.744871998892771,0.00428769075343641,
-0.357348957369103));
#61221=CARTESIAN_POINT('Ctrl Pts',(-0.656944127387824,-0.351108377213285,
-0.341542072051012));
#61222=CARTESIAN_POINT('Ctrl Pts',(-0.410315996739561,-0.621685983303274,
-0.32573518673292));
#61223=CARTESIAN_POINT('Ctrl Pts',(-0.0645664154468477,-0.742080761801361,
-0.309928301414828));
#61224=CARTESIAN_POINT('Ctrl Pts',(0.296780697814228,-0.683208530777618,
-0.294121416096737));
#61225=CARTESIAN_POINT('Ctrl Pts',(0.586433473612455,-0.45929125810821,
-0.278314530778645));
#61226=CARTESIAN_POINT('Ctrl Pts',(0.734419493190546,-0.124421411904842,
-0.262507645460554));
#61227=CARTESIAN_POINT('Ctrl Pts',(0.704989260382789,0.240505344134964,
-0.246700760142461));
#61228=CARTESIAN_POINT('Ctrl Pts',(0.505252343759996,0.547332394234904,
-0.230893874824371));
#61229=CARTESIAN_POINT('Ctrl Pts',(0.183459868124781,0.721938470344044,
-0.215086989506278));
#61230=CARTESIAN_POINT('Ctrl Pts',(-0.182651626265875,0.72214337859536,
-0.199280104188187));
#61231=CARTESIAN_POINT('Ctrl Pts',(-0.504639365504918,0.547897621985701,
-0.183473218870095));
#61232=CARTESIAN_POINT('Ctrl Pts',(-0.704719577046485,0.241294342392419,
-0.167666333552003));
#61233=CARTESIAN_POINT('Ctrl Pts',(-0.734558357616299,-0.123599235284501,
-0.151859448233911));
#61234=CARTESIAN_POINT('Ctrl Pts',(-0.586947129908281,-0.458634536122048,
-0.13605256291582));
#61235=CARTESIAN_POINT('Ctrl Pts',(-0.297545473785419,-0.682875877070518,
-0.120245677597728));
#61236=CARTESIAN_POINT('Ctrl Pts',(0.0637360798710123,-0.742152601032517,
-0.104438792279637));
#61237=CARTESIAN_POINT('Ctrl Pts',(0.409619102099937,-0.622144835166141,
-0.0886319069615454));
#61238=CARTESIAN_POINT('Ctrl Pts',(0.656552129312043,-0.351843641497199,
-0.0728250216434533));
#61239=CARTESIAN_POINT('Ctrl Pts',(0.744873519473169,0.00345411617399305,
-0.0570181363253616));
#61240=CARTESIAN_POINT('Ctrl Pts',(0.653265131348944,0.357916507544478,
-0.0412112510072698));
#61241=CARTESIAN_POINT('Ctrl Pts',(0.403821942874752,0.625917629361813,
-0.0254043656891785));
#61242=CARTESIAN_POINT('Ctrl Pts',(0.0568719964643233,0.742709933615296,
-0.00959748037108637));
#61243=CARTESIAN_POINT('Ctrl Pts',(-0.303910141472772,0.680091682441782,
0.00620940494700605));
#61244=CARTESIAN_POINT('Ctrl Pts',(-0.495338330062706,0.528798303103765,
0.0167473284924));
#61245=CARTESIAN_POINT('Ctrl Pts',(-0.567325265044095,0.434889340047662,
0.0220162902650971));
#61246=CARTESIAN_POINT('Ctrl Pts',(-0.325579286442179,0.678938089483064,
-3.9709162902651));
#61247=CARTESIAN_POINT('Ctrl Pts',(-0.437963443981315,0.625045172903798,
-3.9656473284924));
#61248=CARTESIAN_POINT('Ctrl Pts',(-0.635345959215123,0.460437084581636,
-3.95510940494701));
#61249=CARTESIAN_POINT('Ctrl Pts',(-0.777954672189442,0.102059017460474,
-3.93930251962892));
#61250=CARTESIAN_POINT('Ctrl Pts',(-0.732618684251679,-0.280875658539082,
-3.92349563431082));
#61251=CARTESIAN_POINT('Ctrl Pts',(-0.510307552433891,-0.596006360849397,
-3.90768874899273));
#61252=CARTESIAN_POINT('Ctrl Pts',(-0.164716539319843,-0.767133340665321,
-3.89188186367464));
#61253=CARTESIAN_POINT('Ctrl Pts',(0.220664017227322,-0.752953731708629,
-3.87607497835654));
#61254=CARTESIAN_POINT('Ctrl Pts',(0.552738823443294,-0.556874126203156,
-3.86026809303846));
#61255=CARTESIAN_POINT('Ctrl Pts',(0.751286187467129,-0.22627177068859,
-3.84446120772036));
#61256=CARTESIAN_POINT('Ctrl Pts',(0.768342969090818,0.158993500009593,
-3.82865432240228));
#61257=CARTESIAN_POINT('Ctrl Pts',(0.599788380000657,0.505849312469457,
-3.81284743708418));
#61258=CARTESIAN_POINT('Ctrl Pts',(0.286340898691607,0.730505795947052,
-3.79704055176609));
#61259=CARTESIAN_POINT('Ctrl Pts',(-0.0962789698052883,0.778691252270154,
-3.781233666448));
#61260=CARTESIAN_POINT('Ctrl Pts',(-0.455640380862832,0.638765690064438,
-3.76542678112991));
#61261=CARTESIAN_POINT('Ctrl Pts',(-0.704931180768228,0.344531238590307,
-3.74961989581181));
#61262=CARTESIAN_POINT('Ctrl Pts',(-0.783929319766703,-0.0329327830524558,
-3.73381301049372));
#61263=CARTESIAN_POINT('Ctrl Pts',(-0.673550950658744,-0.402441133840107,
-3.71800612517563));
#61264=CARTESIAN_POINT('Ctrl Pts',(-0.400460553894944,-0.674730383902638,
-3.70219923985754));
#61265=CARTESIAN_POINT('Ctrl Pts',(-0.0306295201890803,-0.784022691505241,
-3.68639235453945));
#61266=CARTESIAN_POINT('Ctrl Pts',(0.346600792629627,-0.703915930899028,
-3.67058546922136));
#61267=CARTESIAN_POINT('Ctrl Pts',(0.640101556190887,-0.453761771640795,
-3.65477858390327));
#61268=CARTESIAN_POINT('Ctrl Pts',(0.778970778768956,-0.093990815362487,
-3.63897169858517));
#61269=CARTESIAN_POINT('Ctrl Pts',(0.729661343113795,0.288485826147569,
-3.62316481326708));
#61270=CARTESIAN_POINT('Ctrl Pts',(0.50408509974901,0.601271951600041,-3.60735792794899));
#61271=CARTESIAN_POINT('Ctrl Pts',(0.156735279915013,0.768806737460164,
-3.59155104263089));
#61272=CARTESIAN_POINT('Ctrl Pts',(-0.22847762216423,0.750618227679105,
-3.57574415731281));
#61273=CARTESIAN_POINT('Ctrl Pts',(-0.55849639689333,0.551100283254033,
-3.55993727199471));
#61274=CARTESIAN_POINT('Ctrl Pts',(-0.753597270410352,0.218451142313315,
-3.54413038667662));
#61275=CARTESIAN_POINT('Ctrl Pts',(-0.766649051673194,-0.166969994659364,
-3.52832350135853));
#61276=CARTESIAN_POINT('Ctrl Pts',(-0.594498776857272,-0.512055614032796,
-3.51251661604044));
#61277=CARTESIAN_POINT('Ctrl Pts',(-0.278733381707383,-0.733442192316373,
-3.49670973072235));
#61278=CARTESIAN_POINT('Ctrl Pts',(0.104366597992381,-0.777648610087503,
-3.48090284540425));
#61279=CARTESIAN_POINT('Ctrl Pts',(0.462254378587548,-0.633995770509813,
-3.46509596008616));
#61280=CARTESIAN_POINT('Ctrl Pts',(0.708473774334626,-0.337186385590646,
-3.44928907476807));
#61281=CARTESIAN_POINT('Ctrl Pts',(0.78354471643388,0.0410782776683208,
-3.43348218944998));
#61282=CARTESIAN_POINT('Ctrl Pts',(0.66933205843443,0.40941951968559,-3.41767530413189));
#61283=CARTESIAN_POINT('Ctrl Pts',(0.393426546122131,0.678855875981091,
-3.4018684188138));
#61284=CARTESIAN_POINT('Ctrl Pts',(0.0224796258818643,0.784298676505233,
-3.3860615334957));
#61285=CARTESIAN_POINT('Ctrl Pts',(-0.353897775129376,0.700275740195334,
-3.37025464817762));
#61286=CARTESIAN_POINT('Ctrl Pts',(-0.644782869781527,0.447084777624944,
-3.35444776285952));
#61287=CARTESIAN_POINT('Ctrl Pts',(-0.779905542309655,0.08589000304069,
-3.33864087754143));
#61288=CARTESIAN_POINT('Ctrl Pts',(-0.726623742586119,-0.296053515867974,
-3.32283399222334));
#61289=CARTESIAN_POINT('Ctrl Pts',(-0.497808938773334,-0.606478365669389,
-3.30702710690525));
#61290=CARTESIAN_POINT('Ctrl Pts',(-0.148736712357813,-0.770394144542023,
-3.29122022158715));
#61291=CARTESIAN_POINT('Ctrl Pts',(0.23626635475059,-0.748203152332651,
-3.27541333626906));
#61292=CARTESIAN_POINT('Ctrl Pts',(0.564193743507245,-0.545266143580295,
-3.25960645095097));
#61293=CARTESIAN_POINT('Ctrl Pts',(0.755826903377695,-0.210607311549555,
-3.24379956563288));
#61294=CARTESIAN_POINT('Ctrl Pts',(0.764872350865989,0.17492865525231,-3.22799268031479));
#61295=CARTESIAN_POINT('Ctrl Pts',(0.589144946018815,0.518206503363411,
-3.2121857949967));
#61296=CARTESIAN_POINT('Ctrl Pts',(0.271095764221967,0.736299418829429,
-3.19637890967861));
#61297=CARTESIAN_POINT('Ctrl Pts',(-0.112442956521666,0.776521943718472,
-3.18057202436051));
#61298=CARTESIAN_POINT('Ctrl Pts',(-0.468818444370271,0.629157383939731,
-3.16476513904242));
#61299=CARTESIAN_POINT('Ctrl Pts',(-0.711939843355949,0.32980510455412,
-3.14895825372433));
#61300=CARTESIAN_POINT('Ctrl Pts',(-0.783075478443625,-0.0492193316485955,
-3.13315136840624));
#61301=CARTESIAN_POINT('Ctrl Pts',(-0.665040868872605,-0.416353684115822,
-3.11734448308815));
#61302=CARTESIAN_POINT('Ctrl Pts',(-0.386350042454257,-0.682908040839498,
-3.10153759777006));
#61303=CARTESIAN_POINT('Ctrl Pts',(-0.0143273035104027,-0.784489946348433,
-3.08573071245196));
#61304=CARTESIAN_POINT('Ctrl Pts',(0.361156531566544,-0.696559909307498,
-3.06992382713387));
#61305=CARTESIAN_POINT('Ctrl Pts',(0.649394537451754,-0.440359492091936,
-3.05411694181578));
#61306=CARTESIAN_POINT('Ctrl Pts',(0.780756064745238,-0.0777799132885599,
-3.03831005649769));
#61307=CARTESIAN_POINT('Ctrl Pts',(0.723507656148297,0.303589227480892,
-3.0225031711796));
#61308=CARTESIAN_POINT('Ctrl Pts',(0.491479007212279,0.611619271293245,
-3.0066962858615));
#61309=CARTESIAN_POINT('Ctrl Pts',(0.140722079076732,0.771898337870972,
-2.99088940054342));
#61310=CARTESIAN_POINT('Ctrl Pts',(-0.244029567142358,0.745707260195287,
-2.97508251522532));
#61311=CARTESIAN_POINT('Ctrl Pts',(-0.569830149011909,0.539373107250178,
-2.95927562990723));
#61312=CARTESIAN_POINT('Ctrl Pts',(-0.757974896073903,0.202740732141823,
-2.94346874458914));
#61313=CARTESIAN_POINT('Ctrl Pts',(-0.763013032748309,-0.182868421013236,
-2.92766185927105));
#61314=CARTESIAN_POINT('Ctrl Pts',(-0.583727478978919,-0.524301418873305,
-2.91185497395296));
#61315=CARTESIAN_POINT('Ctrl Pts',(-0.263428864461014,-0.73907711432328,
-2.89604808863486));
#61316=CARTESIAN_POINT('Ctrl Pts',(0.120507169580355,-0.775311401713775,
-2.88024120331677));
#61317=CARTESIAN_POINT('Ctrl Pts',(0.475331870959451,-0.624251039244497,
-2.86443431799868));
#61318=CARTESIAN_POINT('Ctrl Pts',(0.715329012545471,-0.322388199781518,
-2.84862743268059));
#61319=CARTESIAN_POINT('Ctrl Pts',(0.782521656940954,0.0573550692269745,
-2.83282054736249));
#61320=CARTESIAN_POINT('Ctrl Pts',(0.660677845248626,0.423242876307776,
-2.81701366204441));
#61321=CARTESIAN_POINT('Ctrl Pts',(0.379231807376692,0.686886441721958,
-2.80120677672631));
#61322=CARTESIAN_POINT('Ctrl Pts',(0.00617343358231456,0.784596479896164,
-2.78539989140822));
#61323=CARTESIAN_POINT('Ctrl Pts',(-0.368376277858687,0.692768839843872,
-2.76959300609013));
#61324=CARTESIAN_POINT('Ctrl Pts',(-0.653936061090613,0.433586641345119,
-2.75378612077204));
#61325=CARTESIAN_POINT('Ctrl Pts',(-0.781522254198735,0.0696614221773742,
-2.73797923545394));
#61326=CARTESIAN_POINT('Ctrl Pts',(-0.720313420387067,-0.311092147052815,
-2.72217235013585));
#61327=CARTESIAN_POINT('Ctrl Pts',(-0.485095988788138,-0.616694113162519,
-2.70636546481776));
#61328=CARTESIAN_POINT('Ctrl Pts',(-0.132692245769534,-0.773319154980843,
-2.69055857949967));
#61329=CARTESIAN_POINT('Ctrl Pts',(0.251766420800531,-0.74313082085521,
-2.67475169418158));
#61330=CARTESIAN_POINT('Ctrl Pts',(0.575405004593468,-0.533421810799332,
-2.65894480886349));
#61331=CARTESIAN_POINT('Ctrl Pts',(0.760041016484745,-0.194852253793691,
-2.6431379235454));
#61332=CARTESIAN_POINT('Ctrl Pts',(0.761071298153412,0.190788434331659,
-2.6273310382273));
#61333=CARTESIAN_POINT('Ctrl Pts',(0.578246960902665,0.530339702223469,
-2.61152415290921));
#61334=CARTESIAN_POINT('Ctrl Pts',(0.255733510560913,0.741774978766363,
-2.59571726759112));
#61335=CARTESIAN_POINT('Ctrl Pts',(-0.12855836611643,0.774017114829589,
-2.57991038227303));
#61336=CARTESIAN_POINT('Ctrl Pts',(-0.481793954810521,0.619277266380483,
-2.56410349695494));
#61337=CARTESIAN_POINT('Ctrl Pts',(-0.718640915823752,0.314936472406177,
-2.54829661163684));
#61338=CARTESIAN_POINT('Ctrl Pts',(-0.781883311746624,-0.0654846116257782,
-2.53248972631876));
#61339=CARTESIAN_POINT('Ctrl Pts',(-0.656243458832344,-0.430086352128742,
-2.51668284100066));
#61340=CARTESIAN_POINT('Ctrl Pts',(-0.372072609762093,-0.690790648903465,
-2.50087595568257));
#61341=CARTESIAN_POINT('Ctrl Pts',(0.00198110316616631,-0.784618265641255,
-2.48506907036448));
#61342=CARTESIAN_POINT('Ctrl Pts',(0.375556234168478,-0.688902941294953,
-2.46926218504639));
#61343=CARTESIAN_POINT('Ctrl Pts',(0.658406950147669,-0.42676695695062,
-2.45345529972829));
#61344=CARTESIAN_POINT('Ctrl Pts',(0.782204027910568,-0.0615354066219549,
-2.4376484144102));
#61345=CARTESIAN_POINT('Ctrl Pts',(0.717041380326235,0.318561464159578,
-2.42184152909211));
#61346=CARTESIAN_POINT('Ctrl Pts',(0.478660572959506,0.621702343120665,
-2.40603464377402));
#61347=CARTESIAN_POINT('Ctrl Pts',(0.124648079774715,0.774656442402774,
-2.39022775845593));
#61348=CARTESIAN_POINT('Ctrl Pts',(-0.259476080032666,0.740474112605248,
-2.37442087313784));
#61349=CARTESIAN_POINT('Ctrl Pts',(-0.580917708086637,0.527412897054116,
-2.35861398781974));
#61350=CARTESIAN_POINT('Ctrl Pts',(-0.762025041439243,0.186942728575264,
-2.34280710250165));
#61351=CARTESIAN_POINT('Ctrl Pts',(-0.759047356816805,-0.198687839731243,
-2.32700021718356));
#61352=CARTESIAN_POINT('Ctrl Pts',(-0.572703983765511,-0.536320701191704,
-2.31119333186547));
#61353=CARTESIAN_POINT('Ctrl Pts',(-0.248010533731526,-0.744392720750176,
-2.29538644654738));
#61354=CARTESIAN_POINT('Ctrl Pts',(0.136595676483858,-0.772639222867675,
-2.27957956122929));
#61355=CARTESIAN_POINT('Ctrl Pts',(0.488203997924677,-0.614236602587317,
-2.26377267591119));
#61356=CARTESIAN_POINT('Ctrl Pts',(0.721875195457185,-0.307450727322765,
-2.2479657905931));
#61357=CARTESIAN_POINT('Ctrl Pts',(0.781160511811177,0.0736070807364849,
-2.23215890527501));
#61358=CARTESIAN_POINT('Ctrl Pts',(0.651738188601823,0.436883372384051,
-2.21635201995692));
#61359=CARTESIAN_POINT('Ctrl Pts',(0.36487322290766,0.694620240673004,-2.20054513463883));
#61360=CARTESIAN_POINT('Ctrl Pts',(-0.0101354259267691,0.784555301230531,
-2.18473824932074));
#61361=CARTESIAN_POINT('Ctrl Pts',(-0.382695624956466,0.68496263123387,
-2.16893136400264));
#61362=CARTESIAN_POINT('Ctrl Pts',(-0.662806721702037,0.419901175533298,
-2.15312447868456));
#61363=CARTESIAN_POINT('Ctrl Pts',(-0.782801312239287,0.0534027443498731,
-2.13731759336646));
#61364=CARTESIAN_POINT('Ctrl Pts',(-0.713691889393596,-0.325996372006569,
-2.12151070804837));
#61365=CARTESIAN_POINT('Ctrl Pts',(-0.472173454844658,-0.626643420206186,
-2.10570382273027));
#61366=CARTESIAN_POINT('Ctrl Pts',(-0.116590449978903,-0.775910055690326,
-2.08989693741219));
#61367=CARTESIAN_POINT('Ctrl Pts',(0.267157712083718,-0.737737422408434,
-2.07409005209409));
#61368=CARTESIAN_POINT('Ctrl Pts',(0.586367664039463,-0.521347015064389,
-2.058283166776));
#61369=CARTESIAN_POINT('Ctrl Pts',(0.76392675663392,-0.179013010830011,
-2.04247628145791));
#61370=CARTESIAN_POINT('Ctrl Pts',(0.756941427353513,0.206565783961604,
-2.02666939613982));
#61371=CARTESIAN_POINT('Ctrl Pts',(0.567099146289403,0.542243769743349,
-2.01086251082173));
#61372=CARTESIAN_POINT('Ctrl Pts',(0.240260768166395,0.746930057520609,
-1.99505562550364));
#61373=CARTESIAN_POINT('Ctrl Pts',(-0.144618232536515,0.771177874660354,
-1.97924874018554));
#61374=CARTESIAN_POINT('Ctrl Pts',(-0.494561307924264,0.609129592329817,
-1.96344185486745));
#61375=CARTESIAN_POINT('Ctrl Pts',(-0.725031502096651,0.299931773100352,
-1.94763496954936));
#61376=CARTESIAN_POINT('Ctrl Pts',(-0.780353335207492,-0.0817215992145918,
-1.93182808423127));
#61377=CARTESIAN_POINT('Ctrl Pts',(-0.647162521191612,-0.443633202896902,
-1.91602119891318));
#61378=CARTESIAN_POINT('Ctrl Pts',(-0.357634424451625,-0.698374803379104,
-1.90021431359509));
#61379=CARTESIAN_POINT('Ctrl Pts',(0.0182886539143304,-0.78440759346506,
-1.88440742827699));
#61380=CARTESIAN_POINT('Ctrl Pts',(0.389793679064869,-0.680948335271274,
-1.8686005429589));
#61381=CARTESIAN_POINT('Ctrl Pts',(0.667134900514558,-0.412990038697154,
-1.85279365764081));
#61382=CARTESIAN_POINT('Ctrl Pts',(0.783314042669518,-0.0452643138066422,
-1.83698677232272));
#61383=CARTESIAN_POINT('Ctrl Pts',(0.710265309382765,0.333396067515875,
-1.82117988700462));
#61384=CARTESIAN_POINT('Ctrl Pts',(0.465635335146463,0.631516810711076,
-1.80537300168654));
#61385=CARTESIAN_POINT('Ctrl Pts',(0.108520226723017,0.777079859435072,
-1.78956611636844));
#61386=CARTESIAN_POINT('Ctrl Pts',(-0.274810487225979,0.734921045867015,
-1.77375923105035));
#61387=CARTESIAN_POINT('Ctrl Pts',(-0.591754283777642,0.515224820033407,
-1.75795234573226));
#61388=CARTESIAN_POINT('Ctrl Pts',(-0.765745956655943,0.171063957082489,
-1.74214546041417));
#61389=CARTESIAN_POINT('Ctrl Pts',(-0.75475373723447,-0.214421416090478,
-1.72633857509608));
#61390=CARTESIAN_POINT('Ctrl Pts',(-0.561433053878104,-0.548108268101068,
-1.71053168977799));
#61391=CARTESIAN_POINT('Ctrl Pts',(-0.232485050952634,-0.749386715008478,
-1.69472480445989));
#61392=CARTESIAN_POINT('Ctrl Pts',(0.152625167721958,-0.769633228054435,
-1.6789179191418));
#61393=CARTESIAN_POINT('Ctrl Pts',(0.500865198127574,-0.603956787239182,
-1.66311103382371));
#61394=CARTESIAN_POINT('Ctrl Pts',(0.728109494815239,-0.292380421895079,
-1.64730414850562));
#61395=CARTESIAN_POINT('Ctrl Pts',(0.779461869122354,0.0898272905743789,
-1.63149726318753));
#61396=CARTESIAN_POINT('Ctrl Pts',(0.642516950840174,0.450335114587673,
-1.61569037786943));
#61397=CARTESIAN_POINT('Ctrl Pts',(0.350356996289247,0.702053931474515,
-1.59988349255134));
#61398=CARTESIAN_POINT('Ctrl Pts',(-0.0264399064619325,0.784175158299426,
-1.58407660723325));
#61399=CARTESIAN_POINT('Ctrl Pts',(-0.396849629800857,0.676860487009376,
-1.56826972191516));
#61400=CARTESIAN_POINT('Ctrl Pts',(-0.671391019079131,0.406034292945231,
-1.55246283659707));
#61401=CARTESIAN_POINT('Ctrl Pts',(-0.783742163818932,0.037120994060833,
-1.53665595127897));
#61402=CARTESIAN_POINT('Ctrl Pts',(-0.706762010414098,-0.340759751413029,
-1.52084906596088));
#61403=CARTESIAN_POINT('Ctrl Pts',(-0.459046920076702,-0.636321988238455,
-1.50504218064279));
#61404=CARTESIAN_POINT('Ctrl Pts',(-0.100438281708249,-0.778165727281241,
-1.4892352953247));
#61405=CARTESIAN_POINT('Ctrl Pts',(0.28243357884871,-0.732025287190515,
-1.47342841000661));
#61406=CARTESIAN_POINT('Ctrl Pts',(0.597076985468083,-0.509046973247059,
-1.45762152468852));
#61407=CARTESIAN_POINT('Ctrl Pts',(0.767482445005317,-0.163096425945838,
-1.44181463937043));
#61408=CARTESIAN_POINT('Ctrl Pts',(0.752484522761953,0.22225388759561,-1.42600775405233));
#61409=CARTESIAN_POINT('Ctrl Pts',(0.555706318551799,0.55391356281396,-1.41020086873424));
#61410=CARTESIAN_POINT('Ctrl Pts',(0.224684221980512,0.751762427859133,
-1.39439398341615));
#61411=CARTESIAN_POINT('Ctrl Pts',(-0.160615617175025,0.768005449894162,
-1.37858709809806));
#61412=CARTESIAN_POINT('Ctrl Pts',(-0.507114987623006,0.598718746053408,
-1.36278021277997));
#61413=CARTESIAN_POINT('Ctrl Pts',(-0.731108841145082,0.284797489362429,
-1.34697332746188));
#61414=CARTESIAN_POINT('Ctrl Pts',(-0.778486209847032,-0.0979232792835823,
-1.33116644214378));
#61415=CARTESIAN_POINT('Ctrl Pts',(-0.637801979336504,-0.456988383552671,
-1.31535955682569));
#61416=CARTESIAN_POINT('Ctrl Pts',(-0.343041724488343,-0.705657227560031,
-1.2995526715076));
#61417=CARTESIAN_POINT('Ctrl Pts',(0.0345883031160503,-0.783858020839999,
-1.28374578618951));
#61418=CARTESIAN_POINT('Ctrl Pts',(0.403862715019395,-0.672699527995084,
-1.26793890087142));
#61419=CARTESIAN_POINT('Ctrl Pts',(0.675574617673198,-0.399034689598986,
-1.25213201555332));
#61420=CARTESIAN_POINT('Ctrl Pts',(0.784085629444241,-0.0289736647091182,
-1.23632513023523));
#61421=CARTESIAN_POINT('Ctrl Pts',(0.703182370894705,0.348086628313337,
-1.22051824491714));
#61422=CARTESIAN_POINT('Ctrl Pts',(0.452408921279789,0.64105843375944,-1.20471135959905));
#61423=CARTESIAN_POINT('Ctrl Pts',(0.0923454879019127,0.779167541939348,
-1.18890447428096));
#61424=CARTESIAN_POINT('Ctrl Pts',(-0.290026163547421,0.729050459162884,
-1.17309758896287));
#61425=CARTESIAN_POINT('Ctrl Pts',(-0.602335194181794,0.502814142002418,
-1.15729070364477));
#61426=CARTESIAN_POINT('Ctrl Pts',(-0.769136034116109,0.155111278028998,
-1.14148381832668));
#61427=CARTESIAN_POINT('Ctrl Pts',(-0.750134029044039,-0.230062352456464,
-1.12567693300859));
#61428=CARTESIAN_POINT('Ctrl Pts',(-0.549919558880984,-0.559659026825969,
-1.1098700476905));
#61429=CARTESIAN_POINT('Ctrl Pts',(-0.21685912385273,-0.754056939461121,
-1.09406316237241));
#61430=CARTESIAN_POINT('Ctrl Pts',(0.168588717811249,-0.766294716003188,
-1.07825627705431));
#61431=CARTESIAN_POINT('Ctrl Pts',(0.513310001342625,-0.593416034556938,
-1.06244939173622));
#61432=CARTESIAN_POINT('Ctrl Pts',(0.734029217113261,-0.277183794569127,
-1.04664250641813));
#61433=CARTESIAN_POINT('Ctrl Pts',(0.777426462766882,0.106008690857963,
-1.03083562110004));
#61434=CARTESIAN_POINT('Ctrl Pts',(0.63301811596593,0.463592291142325,-1.01502873578195));
#61435=CARTESIAN_POINT('Ctrl Pts',(0.335689399204394,0.709184302427401,
-0.999221850463857));
#61436=CARTESIAN_POINT('Ctrl Pts',(-0.0427329637316332,0.783456215342222,
-0.983414965145766));
#61437=CARTESIAN_POINT('Ctrl Pts',(-0.410832177205529,0.668465907672345,
-0.967608079827673));
#61438=CARTESIAN_POINT('Ctrl Pts',(-0.679685244407421,0.391991984717126,
-0.951801194509583));
#61439=CARTESIAN_POINT('Ctrl Pts',(-0.784344402446169,0.02082320578127,
-0.935994309191489));
#61440=CARTESIAN_POINT('Ctrl Pts',(-0.69952677747759,-0.355375906807799,
-0.920187423873401));
#61441=CARTESIAN_POINT('Ctrl Pts',(-0.445722055755895,-0.645725635669195,
-0.904380538555305));
#61442=CARTESIAN_POINT('Ctrl Pts',(-0.0842427194431486,-0.780085195198877,
-0.888573653237217));
#61443=CARTESIAN_POINT('Ctrl Pts',(0.297587421212811,-0.725996883108706,
-0.872766767919122));
#61444=CARTESIAN_POINT('Ctrl Pts',(0.607528341955938,-0.49652699953569,
-0.856959882601033));
#61445=CARTESIAN_POINT('Ctrl Pts',(0.770706545376702,-0.147109375843807,
-0.84115299728294));
#61446=CARTESIAN_POINT('Ctrl Pts',(0.747702509968158,0.237845967245534,
-0.825346111964849));
#61447=CARTESIAN_POINT('Ctrl Pts',(0.544073399919657,0.565344039543632,
-0.809539226646757));
#61448=CARTESIAN_POINT('Ctrl Pts',(0.209010601793413,0.7562700019739,-0.793732341328665));
#61449=CARTESIAN_POINT('Ctrl Pts',(-0.176543608420089,0.764501211165595,
-0.777925456010573));
#61450=CARTESIAN_POINT('Ctrl Pts',(-0.519449570135073,0.588049225519544,
-0.762118570692482));
#61451=CARTESIAN_POINT('Ctrl Pts',(-0.736870307276803,0.269540159904672,
-0.74631168537439));
#61452=CARTESIAN_POINT('Ctrl Pts',(-0.776282742349966,-0.114082651955772,
-0.730504800056299));
#61453=CARTESIAN_POINT('Ctrl Pts',(-0.628165877455098,-0.470146124038807,
-0.714697914738207));
#61454=CARTESIAN_POINT('Ctrl Pts',(-0.328300814595196,-0.712634775101368,
-0.698891029420116));
#61455=CARTESIAN_POINT('Ctrl Pts',(0.0508730085671695,-0.782969785206921,
-0.683084144102023));
#61456=CARTESIAN_POINT('Ctrl Pts',(0.417757263556233,-0.664160083333571,
-0.667277258783932));
#61457=CARTESIAN_POINT('Ctrl Pts',(0.683722455274473,-0.384906939013955,
-0.65147037346584));
#61458=CARTESIAN_POINT('Ctrl Pts',(0.784518454873481,-0.0126704976450974,
-0.635663488147748));
#61459=CARTESIAN_POINT('Ctrl Pts',(0.695795625019874,0.362626799548583,
-0.619856602829656));
#61460=CARTESIAN_POINT('Ctrl Pts',(0.438987045783509,0.650323089842206,
-0.604049717511565));
#61461=CARTESIAN_POINT('Ctrl Pts',(0.0761308515485031,0.780918587939964,
-0.588242832193473));
#61462=CARTESIAN_POINT('Ctrl Pts',(-0.305116535119352,0.722864888858496,
-0.572435946875381));
#61463=CARTESIAN_POINT('Ctrl Pts',(-0.612655867855218,0.490186224949473,
-0.55662906155729));
#61464=CARTESIAN_POINT('Ctrl Pts',(-0.7721938091491,0.139091583711784,-0.540822176239198));
#61465=CARTESIAN_POINT('Ctrl Pts',(-0.745190228173637,-0.245603891219511,
-0.525015290921106));
#61466=CARTESIAN_POINT('Ctrl Pts',(-0.538168473137809,-0.570967986903094,
-0.509208405603014));
#61467=CARTESIAN_POINT('Ctrl Pts',(-0.201139503556795,-0.758401376354612,
-0.493401520284923));
#61468=CARTESIAN_POINT('Ctrl Pts',(0.184479429757929,-0.762625129105924,
-0.477594634966831));
#61469=CARTESIAN_POINT('Ctrl Pts',(0.525533030837889,-0.582618898634463,
-0.461787749648739));
#61470=CARTESIAN_POINT('Ctrl Pts',(0.739631804756678,-0.261867410992487,
-0.445980864330648));
#61471=CARTESIAN_POINT('Ctrl Pts',(0.775055172134831,0.122144290472071,
-0.430173979012556));
#61472=CARTESIAN_POINT('Ctrl Pts',(0.623245787915859,0.476649174333111,
-0.414367093694465));
#61473=CARTESIAN_POINT('Ctrl Pts',(0.320876768735667,0.716008272880776,
-0.398560208376372));
#61474=CARTESIAN_POINT('Ctrl Pts',(-0.0590075583808678,0.782398782975698,
-0.382753323058282));
#61475=CARTESIAN_POINT('Ctrl Pts',(-0.42463722605947,0.659782520070082,
-0.366946437740189));
#61476=CARTESIAN_POINT('Ctrl Pts',(-0.687685814201396,0.377780317777545,
-0.351139552422098));
#61477=CARTESIAN_POINT('Ctrl Pts',(-0.784607767917408,0.00451642091067697,
-0.335332667104006));
#61478=CARTESIAN_POINT('Ctrl Pts',(-0.691989316556942,-0.36983852333275,
-0.319525781785914));
#61479=CARTESIAN_POINT('Ctrl Pts',(-0.432204618808581,-0.654850299689326,
-0.303718896467823));
#61480=CARTESIAN_POINT('Ctrl Pts',(-0.0680107604816475,-0.781667630139005,
-0.287912011149731));
#61481=CARTESIAN_POINT('Ctrl Pts',(0.312612692139218,-0.719654814723043,
-0.272105125831638));
#61482=CARTESIAN_POINT('Ctrl Pts',(0.61771721778651,-0.483792503119908,
-0.256298240513548));
#61483=CARTESIAN_POINT('Ctrl Pts',(0.773597665268418,-0.131058767708956,
-0.240491355195456));
#61484=CARTESIAN_POINT('Ctrl Pts',(0.742597454081923,0.253335286484711,
-0.224684469877363));
#61485=CARTESIAN_POINT('Ctrl Pts',(0.532205418195133,0.576530261290379,
-0.208877584559272));
#61486=CARTESIAN_POINT('Ctrl Pts',(0.193246675731908,0.760450832669695,
-0.19307069924118));
#61487=CARTESIAN_POINT('Ctrl Pts',(-0.192395317590102,0.760666671909099,
-0.177263813923089));
#61488=CARTESIAN_POINT('Ctrl Pts',(-0.531559740144116,0.57712564154978,
-0.161456928604996));
#61489=CARTESIAN_POINT('Ctrl Pts',(-0.742313384280858,0.254166374460362,
-0.145650043286905));
#61490=CARTESIAN_POINT('Ctrl Pts',(-0.773743937523648,-0.130192731445162,
-0.129843157968813));
#61491=CARTESIAN_POINT('Ctrl Pts',(-0.618258275472054,-0.483100747794865,
-0.114036272650722));
#61492=CARTESIAN_POINT('Ctrl Pts',(-0.313418265672134,-0.719304415348375,
-0.0982293873326304));
#61493=CARTESIAN_POINT('Ctrl Pts',(0.0671361300166105,-0.781743301689138,
-0.0824225020145388));
#61494=CARTESIAN_POINT('Ctrl Pts',(0.431470547789015,-0.655333629357333,
-0.0666156166964473));
#61495=CARTESIAN_POINT('Ctrl Pts',(0.691576407042652,-0.370613010854759,
-0.0508087313783553));
#61496=CARTESIAN_POINT('Ctrl Pts',(0.784609369614335,0.00363837865489593,
-0.0350018460602636));
#61497=CARTESIAN_POINT('Ctrl Pts',(0.688114061647999,0.377009838606768,
-0.0191949607421719));
#61498=CARTESIAN_POINT('Ctrl Pts',(0.425364134651334,0.659307686157797,
-0.00338807542408051));
#61499=CARTESIAN_POINT('Ctrl Pts',(0.0599058768073062,0.782330365606711,
0.0124188098940116));
#61500=CARTESIAN_POINT('Ctrl Pts',(-0.320122461446881,0.716371695718231,
0.028225695212104));
#61501=CARTESIAN_POINT('Ctrl Pts',(-0.521762533820769,0.557007454829145,
0.038763618757498));
#61502=CARTESIAN_POINT('Ctrl Pts',(-0.597589667152297,0.458088845993785,
0.0440325805301951));
#61503=CARTESIAN_POINT('Ctrl Pts',(-0.342067962509724,0.713322310757519,
-3.9489));
#61504=CARTESIAN_POINT('Ctrl Pts',(-0.460143716676633,0.656700034907516,
-3.9436310382273));
#61505=CARTESIAN_POINT('Ctrl Pts',(-0.667522495464715,0.483755515001817,
-3.93309311468191));
#61506=CARTESIAN_POINT('Ctrl Pts',(-0.817353501043518,0.107227706467285,
-3.91728622936382));
#61507=CARTESIAN_POINT('Ctrl Pts',(-0.769721511945864,-0.295100358763466,
-3.90147934404572));
#61508=CARTESIAN_POINT('Ctrl Pts',(-0.536151628753535,-0.626190577805068,
-3.88567245872763));
#61509=CARTESIAN_POINT('Ctrl Pts',(-0.173058463308598,-0.805984132719911,
-3.86986557340955));
#61510=CARTESIAN_POINT('Ctrl Pts',(0.231839351934833,-0.791086409962412,
-3.85405868809145));
#61511=CARTESIAN_POINT('Ctrl Pts',(0.580731794093568,-0.58507652561776,
-3.83825180277336));
#61512=CARTESIAN_POINT('Ctrl Pts',(0.789334414412207,-0.237731105128708,
-3.82244491745526));
#61513=CARTESIAN_POINT('Ctrl Pts',(0.807255021711117,0.167045585715507,
-3.80663803213718));
#61514=CARTESIAN_POINT('Ctrl Pts',(0.630164133983604,0.531467605154613,
-3.79083114681908));
#61515=CARTESIAN_POINT('Ctrl Pts',(0.300842381187657,0.767501618274884,
-3.775024261501));
#61516=CARTESIAN_POINT('Ctrl Pts',(-0.101154933391865,0.818127384573358,
-3.7592173761829));
#61517=CARTESIAN_POINT('Ctrl Pts',(-0.478715886449932,0.671115415569497,
-3.74341049086481));
#61518=CARTESIAN_POINT('Ctrl Pts',(-0.740631799246196,0.361979719574299,
-3.72760360554672));
#61519=CARTESIAN_POINT('Ctrl Pts',(-0.823630729382582,-0.0346006348303968,
-3.71179672022863));
#61520=CARTESIAN_POINT('Ctrl Pts',(-0.707662345034486,-0.422822410439913,
-3.69598983491053));
#61521=CARTESIAN_POINT('Ctrl Pts',(-0.420741525768683,-0.708901509635718,
-3.68018294959245));
#61522=CARTESIAN_POINT('Ctrl Pts',(-0.0321807252489052,-0.823728829850542,
-3.66437606427435));
#61523=CARTESIAN_POINT('Ctrl Pts',(0.364154084354281,-0.739565132941993,
-3.64856917895626));
#61524=CARTESIAN_POINT('Ctrl Pts',(0.672518935458776,-0.476742136719247,
-3.63276229363817));
#61525=CARTESIAN_POINT('Ctrl Pts',(0.818421067445377,-0.0987508973835936,
-3.61695540832007));
#61526=CARTESIAN_POINT('Ctrl Pts',(0.766614398872004,0.303095936604549,
-3.60114852300198));
#61527=CARTESIAN_POINT('Ctrl Pts',(0.529614045435536,0.63172283975934,-3.58534163768389));
#61528=CARTESIAN_POINT('Ctrl Pts',(0.164673000054145,0.807742277220862,
-3.5695347523658));
#61529=CARTESIAN_POINT('Ctrl Pts',(-0.240048670008569,0.788632626389314,
-3.55372786704771));
#61530=CARTESIAN_POINT('Ctrl Pts',(-0.586780954777519,0.579010271480279,
-3.53792098172961));
#61531=CARTESIAN_POINT('Ctrl Pts',(-0.791762540114605,0.229514407920758,
-3.52211409641153));
#61532=CARTESIAN_POINT('Ctrl Pts',(-0.805475317338525,-0.175426042908079,
-3.50630721109343));
#61533=CARTESIAN_POINT('Ctrl Pts',(-0.62460664355012,-0.537988219391752,
-3.49050032577534));
#61534=CARTESIAN_POINT('Ctrl Pts',(-0.292849588209368,-0.770586725850833,
-3.47469344045725));
#61535=CARTESIAN_POINT('Ctrl Pts',(0.109652152381827,-0.817031938696122,
-3.45888655513916));
#61536=CARTESIAN_POINT('Ctrl Pts',(0.485664844261286,-0.666103927642191,
-3.44307966982107));
#61537=CARTESIAN_POINT('Ctrl Pts',(0.744353804342099,-0.354262892966616,
-3.42727278450297));
#61538=CARTESIAN_POINT('Ctrl Pts',(0.823226648152874,0.043158650843427,
-3.41146589918488));
#61539=CARTESIAN_POINT('Ctrl Pts',(0.703229790731081,0.430154210487319,
-3.39565901386679));
#61540=CARTESIAN_POINT('Ctrl Pts',(0.41335128687045,0.713235933625179,-3.3798521285487));
#61541=CARTESIAN_POINT('Ctrl Pts',(0.0236180867260336,0.824018791867665,
-3.36404524323061));
#61542=CARTESIAN_POINT('Ctrl Pts',(-0.371820616102767,0.735740587987778,
-3.34823835791252));
#61543=CARTESIAN_POINT('Ctrl Pts',(-0.677437330051128,0.469726992225103,
-3.33243147259442));
#61544=CARTESIAN_POINT('Ctrl Pts',(-0.819403171261899,0.0902398265600419,
-3.31662458727633));
#61545=CARTESIAN_POINT('Ctrl Pts',(-0.763422961742281,-0.31104688530234,
-3.30081770195824));
#61546=CARTESIAN_POINT('Ctrl Pts',(-0.523020033817682,-0.637192928081435,
-3.28501081664015));
#61547=CARTESIAN_POINT('Ctrl Pts',(-0.156269352091197,-0.80941007713559,
-3.26920393132206));
#61548=CARTESIAN_POINT('Ctrl Pts',(0.248231856093482,-0.786095241680057,
-3.25339704600397));
#61549=CARTESIAN_POINT('Ctrl Pts',(0.592766838490301,-0.572880666943699,
-3.23759016068587));
#61550=CARTESIAN_POINT('Ctrl Pts',(0.79410509087887,-0.221273333259802,
-3.22178327536778));
#61551=CARTESIAN_POINT('Ctrl Pts',(0.803608637084535,0.183787762853733,
-3.20597639004969));
#61552=CARTESIAN_POINT('Ctrl Pts',(0.618981672666545,0.544450615092468,
-3.1901695047316));
#61553=CARTESIAN_POINT('Ctrl Pts',(0.284825170316527,0.773588654082908,
-3.17436261941351));
#61554=CARTESIAN_POINT('Ctrl Pts',(-0.118137530972093,0.815848213301628,
-3.15855573409542));
#61555=CARTESIAN_POINT('Ctrl Pts',(-0.492561341371445,0.661020505247762,
-3.14274884877732));
#61556=CARTESIAN_POINT('Ctrl Pts',(-0.74799540937477,0.34650779345624,-3.12694196345923));
#61557=CARTESIAN_POINT('Ctrl Pts',(-0.822733646018086,-0.0517120013287895,
-3.11113507814114));
#61558=CARTESIAN_POINT('Ctrl Pts',(-0.698721277655212,-0.437439549564865,
-3.09532819282305));
#61559=CARTESIAN_POINT('Ctrl Pts',(-0.405916399909998,-0.71749331680215,
-3.07952130750496));
#61560=CARTESIAN_POINT('Ctrl Pts',(-0.0150528971717421,-0.824219748403531,
-3.06371442218686));
#61561=CARTESIAN_POINT('Ctrl Pts',(0.379446985863416,-0.731836572118947,
-3.04790753686877));
#61562=CARTESIAN_POINT('Ctrl Pts',(0.6822825515668,-0.462661110532472,-3.03210065155068));
#61563=CARTESIAN_POINT('Ctrl Pts',(0.820296767656767,-0.0817190084588727,
-3.01629376623259));
#61564=CARTESIAN_POINT('Ctrl Pts',(0.760149063852653,0.318964236389567,
-3.0004868809145));
#61565=CARTESIAN_POINT('Ctrl Pts',(0.516369528450532,0.642594190340542,
-2.9846799955964));
#61566=CARTESIAN_POINT('Ctrl Pts',(0.14784882476994,0.810990449010216,-2.96887311027832));
#61567=CARTESIAN_POINT('Ctrl Pts',(-0.256388229536036,0.783472947284729,
-2.95306622496022));
#61568=CARTESIAN_POINT('Ctrl Pts',(-0.598688694785053,0.566689182981476,
-2.93725933964213));
#61569=CARTESIAN_POINT('Ctrl Pts',(-0.796361866772409,0.213008357869846,
-2.92145245432404));
#61570=CARTESIAN_POINT('Ctrl Pts',(-0.801655155439179,-0.19212963105525,
-2.90564556900595));
#61571=CARTESIAN_POINT('Ctrl Pts',(-0.613289842782184,-0.550854202227637,
-2.88983868368786));
#61572=CARTESIAN_POINT('Ctrl Pts',(-0.276769987173107,-0.776507023517393,
-2.87403179836976));
#61573=CARTESIAN_POINT('Ctrl Pts',(0.126610148995108,-0.814576364463811,
-2.85822491305167));
#61574=CARTESIAN_POINT('Ctrl Pts',(0.499404634710725,-0.655865683048816,
-2.84241802773358));
#61575=CARTESIAN_POINT('Ctrl Pts',(0.751556220051425,-0.338715266077066,
-2.82661114241549));
#61576=CARTESIAN_POINT('Ctrl Pts',(0.82215177671343,0.0602597661677676,
-2.8108042570974));
#61577=CARTESIAN_POINT('Ctrl Pts',(0.69413729254441,0.444677638824754,-2.79499737177931));
#61578=CARTESIAN_POINT('Ctrl Pts',(0.398437668089385,0.721673200291612,
-2.77919048646121));
#61579=CARTESIAN_POINT('Ctrl Pts',(0.00648608168618137,0.82433167724891,
-2.76338360114312));
#61580=CARTESIAN_POINT('Ctrl Pts',(-0.387032369844621,0.727853507282956,
-2.74757671582503));
#61581=CARTESIAN_POINT('Ctrl Pts',(-0.687054076668443,0.455545254727689,
-2.73176983050694));
#61582=CARTESIAN_POINT('Ctrl Pts',(-0.821101760099986,0.0731893635192228,
-2.71596294518885));
#61583=CARTESIAN_POINT('Ctrl Pts',(-0.756793058835995,-0.32684713471178,
-2.70015605987076));
#61584=CARTESIAN_POINT('Ctrl Pts',(-0.509663247682897,-0.647926043104431,
-2.68434917455266));
#61585=CARTESIAN_POINT('Ctrl Pts',(-0.139412327630636,-0.81248322215062,
-2.66854228923457));
#61586=CARTESIAN_POINT('Ctrl Pts',(0.264516909330157,-0.780766026444583,
-2.65273540391648));
#61587=CARTESIAN_POINT('Ctrl Pts',(0.604545884015083,-0.560436488366046,
-2.63692851859839));
#61588=CARTESIAN_POINT('Ctrl Pts',(0.79853262403083,-0.204720374486952,
-2.6211216332803));
#61589=CARTESIAN_POINT('Ctrl Pts',(0.799615083406745,0.200450746469219,
-2.6053147479622));
#61590=CARTESIAN_POINT('Ctrl Pts',(0.607531768697286,0.557198289117249,
-2.58950786264412));
#61591=CARTESIAN_POINT('Ctrl Pts',(0.268684908855737,0.779341518927888,
-2.57370097732602));
#61592=CARTESIAN_POINT('Ctrl Pts',(-0.13506909128519,0.813216529560877,
-2.55789409200793));
#61593=CARTESIAN_POINT('Ctrl Pts',(-0.506193985104167,0.650640017840899,
-2.54208720668984));
#61594=CARTESIAN_POINT('Ctrl Pts',(-0.755035851752847,0.330886152535123,
-2.52628032137175));
#61595=CARTESIAN_POINT('Ctrl Pts',(-0.82148110308923,-0.0688010220777596,
-2.51047343605365));
#61596=CARTESIAN_POINT('Ctrl Pts',(-0.689478330535574,-0.451867696448331,
-2.49466655073557));
#61597=CARTESIAN_POINT('Ctrl Pts',(-0.390915899220144,-0.725775132605511,
-2.47885966541747));
#61598=CARTESIAN_POINT('Ctrl Pts',(0.00208143439030202,-0.824354566313865,
-2.46305278009938));
#61599=CARTESIAN_POINT('Ctrl Pts',(0.39457594871488,-0.723791823708583,
-2.44724589478129));
#61600=CARTESIAN_POINT('Ctrl Pts',(0.69175138996213,-0.448380193426408,
-2.4314390094632));
#61601=CARTESIAN_POINT('Ctrl Pts',(0.821818061640689,-0.06465181306649,
-2.4156321241451));
#61602=CARTESIAN_POINT('Ctrl Pts',(0.753355309189543,0.334694728801593,
-2.39982523882701));
#61603=CARTESIAN_POINT('Ctrl Pts',(0.50290191589039,0.653187910455651,-2.38401835350892));
#61604=CARTESIAN_POINT('Ctrl Pts',(0.130960771937376,0.813888235315641,
-2.36821146819083));
#61605=CARTESIAN_POINT('Ctrl Pts',(-0.272617017460498,0.777974771546345,
-2.35240458287274));
#61606=CARTESIAN_POINT('Ctrl Pts',(-0.610337773518973,0.554123258479144,
-2.33659769755465));
#61607=CARTESIAN_POINT('Ctrl Pts',(-0.800617128180865,0.196410278333562,
-2.32079081223656));
#61608=CARTESIAN_POINT('Ctrl Pts',(-0.797488641344603,-0.208750210294458,
-2.30498392691846));
#61609=CARTESIAN_POINT('Ctrl Pts',(-0.601708072367388,-0.563482190507886,
-2.28917704160037));
#61610=CARTESIAN_POINT('Ctrl Pts',(-0.260570808670166,-0.782091834147768,
-2.27337015628228));
#61611=CARTESIAN_POINT('Ctrl Pts',(0.143513444153849,-0.811768855474724,
-2.25756327096419));
#61612=CARTESIAN_POINT('Ctrl Pts',(0.51292865920343,-0.645344074071665,
-2.2417563856461));
#61613=CARTESIAN_POINT('Ctrl Pts',(0.75843392862833,-0.323021298488259,
-2.22594950032801));
#61614=CARTESIAN_POINT('Ctrl Pts',(0.82072169758797,0.077334846479212,-2.21014261500991));
#61615=CARTESIAN_POINT('Ctrl Pts',(0.684744894864187,0.459008945805065,
-2.19433572969182));
#61616=CARTESIAN_POINT('Ctrl Pts',(0.383351905762432,0.729798670675655,
-2.17852884437373));
#61617=CARTESIAN_POINT('Ctrl Pts',(-0.0106487256416806,0.824288413126043,
-2.16272195905564));
#61618=CARTESIAN_POINT('Ctrl Pts',(-0.402076907658228,0.719651960116582,
-2.14691507373754));
#61619=CARTESIAN_POINT('Ctrl Pts',(-0.696373984069875,0.441166700559203,
-2.13110818841946));
#61620=CARTESIAN_POINT('Ctrl Pts',(-0.822445594907919,0.0561072792799869,
-2.11530130310136));
#61621=CARTESIAN_POINT('Ctrl Pts',(-0.749836186240129,-0.342506171004995,
-2.09949441778327));
#61622=CARTESIAN_POINT('Ctrl Pts',(-0.49608626339494,-0.658379224036185,
-2.08368753246518));
#61623=CARTESIAN_POINT('Ctrl Pts',(-0.122495070580787,-0.815205336743481,
-2.06788064714709));
#61624=CARTESIAN_POINT('Ctrl Pts',(0.280687678997866,-0.775099484086033,
-2.052073761829));
#61625=CARTESIAN_POINT('Ctrl Pts',(0.616063737688632,-0.547750175241189,
-2.0362668765109));
#61626=CARTESIAN_POINT('Ctrl Pts',(0.80261515406582,-0.188078967020618,
-2.02045999119281));
#61627=CARTESIAN_POINT('Ctrl Pts',(0.795276058939349,0.21702712606847,-2.00465310587472));
#61628=CARTESIAN_POINT('Ctrl Pts',(0.59581938283618,0.569705227647034,-1.98884622055663));
#61629=CARTESIAN_POINT('Ctrl Pts',(0.252428563056937,0.784757672103085,
-1.97303933523854));
#61630=CARTESIAN_POINT('Ctrl Pts',(-0.15194229548847,0.810233498575157,
-1.95723244992045));
#61631=CARTESIAN_POINT('Ctrl Pts',(-0.519607929566004,0.639978423779874,
-1.94142556460235));
#61632=CARTESIAN_POINT('Ctrl Pts',(-0.761750083636275,0.315121553454813,
-1.92561867928426));
#61633=CARTESIAN_POINT('Ctrl Pts',(-0.819873642236459,-0.0858603175952819,
-1.90981179396617));
#61634=CARTESIAN_POINT('Ctrl Pts',(-0.679937496809979,-0.466100615536416,
-1.89400490864808));
#61635=CARTESIAN_POINT('Ctrl Pts',(-0.375746504737283,-0.733743379901555,
-1.87819802332999));
#61636=CARTESIAN_POINT('Ctrl Pts',(0.0192148666762014,-0.824133224830948,
-1.86239113801189));
#61637=CARTESIAN_POINT('Ctrl Pts',(0.409534436462281,-0.715434363672282,
-1.84658425269381));
#61638=CARTESIAN_POINT('Ctrl Pts',(0.700921359684447,-0.433905555287956,
-1.83077736737571));
#61639=CARTESIAN_POINT('Ctrl Pts',(0.82298429211898,-0.0475566850933253,
-1.81497048205762));
#61640=CARTESIAN_POINT('Ctrl Pts',(0.746236070104087,0.350280617572898,
-1.79916359673953));
#61641=CARTESIAN_POINT('Ctrl Pts',(0.489217026385898,0.663499423108855,
-1.78335671142144));
#61642=CARTESIAN_POINT('Ctrl Pts',(0.114016137979435,0.816434384168071,
-1.76754982610334));
#61643=CARTESIAN_POINT('Ctrl Pts',(-0.288728022193726,0.772140474636412,
-1.75174294078526));
#61644=CARTESIAN_POINT('Ctrl Pts',(-0.621723158036865,0.541317927037625,
-1.73593605546716));
#61645=CARTESIAN_POINT('Ctrl Pts',(-0.804526485869913,0.179727340450608,
-1.72012917014907));
#61646=CARTESIAN_POINT('Ctrl Pts',(-0.792977575181979,-0.225280599764276,
-1.70432228483098));
#61647=CARTESIAN_POINT('Ctrl Pts',(-0.589866336167564,-0.575866728356393,
-1.68851539951288));
#61648=CARTESIAN_POINT('Ctrl Pts',(-0.2442590514967,-0.787338744844668,
-1.6727085141948));
#61649=CARTESIAN_POINT('Ctrl Pts',(0.160354734850819,-0.808610624702993,
-1.6569016288767));
#61650=CARTESIAN_POINT('Ctrl Pts',(0.526231074733792,-0.634543646533604,
-1.64109474355861));
#61651=CARTESIAN_POINT('Ctrl Pts',(0.764983958583825,-0.307187770721855,
-1.62528785824052));
#61652=CARTESIAN_POINT('Ctrl Pts',(0.818937028636985,0.0943765145514026,
-1.60948097292243));
#61653=CARTESIAN_POINT('Ctrl Pts',(0.675056655641679,0.473141939639169,
-1.59367408760433));
#61654=CARTESIAN_POINT('Ctrl Pts',(0.368100517638354,0.737608834197379,
-1.57786720228624));
#61655=CARTESIAN_POINT('Ctrl Pts',(-0.0277789322263472,0.823889018191168,
-1.56206031696815));
#61656=CARTESIAN_POINT('Ctrl Pts',(-0.416947729605723,0.711139489937295,
-1.54625343165006));
#61657=CARTESIAN_POINT('Ctrl Pts',(-0.705393025623311,0.426597541921698,
-1.53044654633197));
#61658=CARTESIAN_POINT('Ctrl Pts',(-0.823434095086754,0.0390009540947295,
-1.51463966101388));
#61659=CARTESIAN_POINT('Ctrl Pts',(-0.742555349646192,-0.358017228752285,
-1.49883277569579));
#61660=CARTESIAN_POINT('Ctrl Pts',(-0.482294946840517,-0.668547954617876,
-1.48302589037769));
#61661=CARTESIAN_POINT('Ctrl Pts',(-0.105524889981051,-0.817575244834462,
-1.4672190050596));
#61662=CARTESIAN_POINT('Ctrl Pts',(0.296737178574367,-0.769098062813428,
-1.45141211974151));
#61663=CARTESIAN_POINT('Ctrl Pts',(0.627315423264153,-0.534827208644584,
-1.43560523442342));
#61664=CARTESIAN_POINT('Ctrl Pts',(0.806350917141581,-0.171356300720379,
-1.41979834910533));
#61665=CARTESIAN_POINT('Ctrl Pts',(0.79059343834209,0.23350973988696,-1.40399146378723));
#61666=CARTESIAN_POINT('Ctrl Pts',(0.583849575376949,0.581966027104503,
-1.38818457846915));
#61667=CARTESIAN_POINT('Ctrl Pts',(0.236063156415228,0.789834773579211,
-1.37237769315105));
#61668=CARTESIAN_POINT('Ctrl Pts',(-0.168749853575404,0.80690040915216,
-1.35657080783296));
#61669=CARTESIAN_POINT('Ctrl Pts',(-0.532797379311024,0.629040329367638,
-1.34076392251487));
#61670=CARTESIAN_POINT('Ctrl Pts',(-0.768135204165577,0.299220807253026,
-1.32495703719678));
#61671=CARTESIAN_POINT('Ctrl Pts',(-0.817911957957395,-0.102882517474752,
-1.30915015187868));
#61672=CARTESIAN_POINT('Ctrl Pts',(-0.67010289856095,-0.480132157548163,
-1.29334326656059));
#61673=CARTESIAN_POINT('Ctrl Pts',(-0.360414770343172,-0.741394616037992,
-1.2775363812425));
#61674=CARTESIAN_POINT('Ctrl Pts',(0.0363399972487994,-0.823555819584562,
-1.26172949592441));
#61675=CARTESIAN_POINT('Ctrl Pts',(0.424315986345355,-0.706767802820285,
-1.24592261060632));
#61676=CARTESIAN_POINT('Ctrl Pts',(0.709788498881667,-0.419243449831899,
-1.23011572528823));
#61677=CARTESIAN_POINT('Ctrl Pts',(0.823794955226002,-0.0304410104272703,
-1.21430883997013));
#61678=CARTESIAN_POINT('Ctrl Pts',(0.73879442243765,0.365715168876903,-1.19850195465204));
#61679=CARTESIAN_POINT('Ctrl Pts',(0.475320772443814,0.673524273248605,
-1.18269506933395));
#61680=CARTESIAN_POINT('Ctrl Pts',(0.0970222437636098,0.818627795513149,
-1.16688818401586));
#61681=CARTESIAN_POINT('Ctrl Pts',(-0.304714283034701,0.7659725772417,-1.15108129869777));
#61682=CARTESIAN_POINT('Ctrl Pts',(-0.632839929324736,0.528278721153811,
-1.13527441337968));
#61683=CARTESIAN_POINT('Ctrl Pts',(-0.808088250815778,0.162966752023653,
-1.11946752806158));
#61684=CARTESIAN_POINT('Ctrl Pts',(-0.788123905941042,-0.241713657570019,
-1.10366064274349));
#61685=CARTESIAN_POINT('Ctrl Pts',(-0.577769750361789,-0.588002465078608,
-1.0878537574254));
#61686=CARTESIAN_POINT('Ctrl Pts',(-0.227841763088093,-0.792245488699401,
-1.07204687210731));
#61687=CARTESIAN_POINT('Ctrl Pts',(0.177126744867603,-0.805103036650745,
-1.05623998678922));
#61688=CARTESIAN_POINT('Ctrl Pts',(0.539306134041545,-0.623469066720079,
-1.04043310147113));
#61689=CARTESIAN_POINT('Ctrl Pts',(0.771203480001284,-0.291221523595961,
-1.02462621615303));
#61690=CARTESIAN_POINT('Ctrl Pts',(0.816798540920201,0.111377407593605,
-1.00881933083494));
#61691=CARTESIAN_POINT('Ctrl Pts',(0.665076760645423,0.487070514218457,
-0.993012445516851));
#61692=CARTESIAN_POINT('Ctrl Pts',(0.352690093023949,0.745100316504026,
-0.97720556019876));
#61693=CARTESIAN_POINT('Ctrl Pts',(-0.0448971370243381,0.823133665001416,
-0.961398674880668));
#61694=CARTESIAN_POINT('Ctrl Pts',(-0.431638410802547,0.702319774526884,
-0.945591789562575));
#61695=CARTESIAN_POINT('Ctrl Pts',(-0.714107304684638,0.411844073367198,
-0.929784904244485));
#61696=CARTESIAN_POINT('Ctrl Pts',(-0.824066833558586,0.0218777786890507,
-0.913978018926392));
#61697=CARTESIAN_POINT('Ctrl Pts',(-0.734953694713166,-0.373373606457542,
-0.898171133608302));
#61698=CARTESIAN_POINT('Ctrl Pts',(-0.468295256507801,-0.67842784148643,
-0.882364248290208));
#61699=CARTESIAN_POINT('Ctrl Pts',(-0.0885091177362583,-0.819591922513389,
-0.866557362972118));
#61700=CARTESIAN_POINT('Ctrl Pts',(0.312658473931717,-0.762764355519012,
-0.850750477654025));
#61701=CARTESIAN_POINT('Ctrl Pts',(0.638296079491797,-0.521673171896967,
-0.834943592335934));
#61702=CARTESIAN_POINT('Ctrl Pts',(0.809738299235259,-0.154559600553418,
-0.819136707017843));
#61703=CARTESIAN_POINT('Ctrl Pts',(0.785569244724172,0.249891466671308,
-0.80332982169975));
#61704=CARTESIAN_POINT('Ctrl Pts',(0.571627517831392,0.593975390255831,
-0.78752293638166));
#61705=CARTESIAN_POINT('Ctrl Pts',(0.21959575954505,0.79457062981303,-0.771716051063566));
#61706=CARTESIAN_POINT('Ctrl Pts',(-0.185484503901628,0.803218701341055,
-0.755909165745476));
#61707=CARTESIAN_POINT('Ctrl Pts',(-0.545756635885414,0.617830460368116,
-0.740102280427384));
#61708=CARTESIAN_POINT('Ctrl Pts',(-0.774188454672643,0.283190783789352,
-0.724295395109292));
#61709=CARTESIAN_POINT('Ctrl Pts',(-0.815596897790595,-0.119860267336591,
-0.708488509791201));
#61710=CARTESIAN_POINT('Ctrl Pts',(-0.659978784790912,-0.493956260206867,
-0.692681624473109));
#61711=CARTESIAN_POINT('Ctrl Pts',(-0.344927320057899,-0.748725535326077,
-0.676874739155018));
#61712=CARTESIAN_POINT('Ctrl Pts',(0.0534494272577162,-0.822622600040544,
-0.661067853836925));
#61713=CARTESIAN_POINT('Ctrl Pts',(0.438914212049227,-0.697795885508685,
-0.645260968518834));
#61714=CARTESIAN_POINT('Ctrl Pts',(0.718348976538538,-0.404400211767597,
-0.629454083200741));
#61715=CARTESIAN_POINT('Ctrl Pts',(0.824249700717708,-0.0133121838333343,
-0.613647197882651));
#61716=CARTESIAN_POINT('Ctrl Pts',(0.73103358132705,0.380991714271834,-0.597840312564558));
#61717=CARTESIAN_POINT('Ctrl Pts',(0.461219157890128,0.683258129674842,
-0.582033427246467));
#61718=CARTESIAN_POINT('Ctrl Pts',(0.0799864314401131,0.820467521695479,
-0.566226541928375));
#61719=CARTESIAN_POINT('Ctrl Pts',(-0.320568893177542,0.759473744179854,
-0.550419656610283));
#61720=CARTESIAN_POINT('Ctrl Pts',(-0.643683284421967,0.515011274369203,
-0.534612771292192));
#61721=CARTESIAN_POINT('Ctrl Pts',(-0.811300884170861,0.146135754403996,
-0.5188058859741));
#61722=CARTESIAN_POINT('Ctrl Pts',(-0.782929730631943,-0.258042283868811,
-0.502999000656008));
#61723=CARTESIAN_POINT('Ctrl Pts',(-0.565423541235985,-0.599884157473597,
-0.487192115337916));
#61724=CARTESIAN_POINT('Ctrl Pts',(-0.211326036474102,-0.796809945771127,
-0.471385230019825));
#61725=CARTESIAN_POINT('Ctrl Pts',(0.193822227918228,-0.801247606758639,
-0.455578344701732));
#61726=CARTESIAN_POINT('Ctrl Pts',(0.552148188094894,-0.612125119363043,
-0.439771459383642));
#61727=CARTESIAN_POINT('Ctrl Pts',(0.777089805759007,-0.275129455269591,
-0.423964574065549));
#61728=CARTESIAN_POINT('Ctrl Pts',(0.814307158363627,0.128330180431784,
-0.408157688747458));
#61729=CARTESIAN_POINT('Ctrl Pts',(0.654809521652447,0.500788651752962,
-0.392350803429367));
#61730=CARTESIAN_POINT('Ctrl Pts',(0.337127289937743,0.75226988092786,-0.376543918111274));
#61731=CARTESIAN_POINT('Ctrl Pts',(-0.0619959441787181,0.822022679904477,
-0.360737032793183));
#61732=CARTESIAN_POINT('Ctrl Pts',(-0.446142604190946,0.693196624411143,
-0.344930147475091));
#61733=CARTESIAN_POINT('Ctrl Pts',(-0.722513056285879,0.396912669078513,
-0.329123262156999));
#61734=CARTESIAN_POINT('Ctrl Pts',(-0.824343536942043,0.00474515106791719,
-0.313316376838907));
#61735=CARTESIAN_POINT('Ctrl Pts',(-0.727034505726059,-0.388568669452214,
-0.297509491520816));
#61736=CARTESIAN_POINT('Ctrl Pts',(-0.4540932408776,-0.68801461607538,-0.281702606202724));
#61737=CARTESIAN_POINT('Ctrl Pts',(-0.0714551055164477,-0.821254498476647,
-0.265895720884633));
#61738=CARTESIAN_POINT('Ctrl Pts',(0.328444686464207,-0.756101098668467,
-0.250088835566541));
#61739=CARTESIAN_POINT('Ctrl Pts',(0.649000961960564,-0.508293748131606,
-0.23428195024845));
#61740=CARTESIAN_POINT('Ctrl Pts',(0.812775837346289,-0.13769612351307,
-0.218475064930358));
#61741=CARTESIAN_POINT('Ctrl Pts',(0.780205647781058,0.266165228834457,
-0.202668179612265));
#61742=CARTESIAN_POINT('Ctrl Pts',(0.559158492630269,0.605728128345855,
-0.186861294294174));
#61743=CARTESIAN_POINT('Ctrl Pts',(0.203033483339035,0.798963194995345,
-0.171054408976082));
#61744=CARTESIAN_POINT('Ctrl Pts',(-0.202139008914331,0.799189965222836,
-0.155247523657991));
#61745=CARTESIAN_POINT('Ctrl Pts',(-0.55848011478331,0.606353661113862,
-0.139440638339899));
#61746=CARTESIAN_POINT('Ctrl Pts',(-0.779907191515234,0.267038406528302,
-0.123633753021807));
#61747=CARTESIAN_POINT('Ctrl Pts',(-0.812929517430994,-0.136786227605823,
-0.107826867703715));
#61748=CARTESIAN_POINT('Ctrl Pts',(-0.649569421035828,-0.507566959467682,
-0.092019982385624));
#61749=CARTESIAN_POINT('Ctrl Pts',(-0.329291057558848,-0.755732953626231,
-0.0762130970675324));
#61750=CARTESIAN_POINT('Ctrl Pts',(0.0705361801622086,-0.821334002345758,
-0.0604062117494408));
#61751=CARTESIAN_POINT('Ctrl Pts',(0.453321993478091,-0.688522423548524,
-0.0445993264313493));
#61752=CARTESIAN_POINT('Ctrl Pts',(0.726600684773263,-0.389382380212319,
-0.0287924411132574));
#61753=CARTESIAN_POINT('Ctrl Pts',(0.824345219755501,0.00382264113579923,
-0.0129855557951656));
#61754=CARTESIAN_POINT('Ctrl Pts',(0.722962991947054,0.396103169669058,
0.00282132952292606));
#61755=CARTESIAN_POINT('Ctrl Pts',(0.446906326427915,0.69269774295378,0.0186282148410175));
#61756=CARTESIAN_POINT('Ctrl Pts',(0.0629397571502896,0.821950797598125,
0.0344351001591095));
#61757=CARTESIAN_POINT('Ctrl Pts',(-0.33633478142099,0.752651708994679,
0.0502419854772021));
#61758=CARTESIAN_POINT('Ctrl Pts',(-0.548186737578833,0.585216606554525,
0.060779909022596));
#61759=CARTESIAN_POINT('Ctrl Pts',(-0.6278540692605,0.481288351939907,0.0660488707952931));
#61760=CARTESIAN_POINT('',(0.724715087996802,0.317217986926636,0.));
#61761=CARTESIAN_POINT('Ctrl Pts',(0.724729084696739,0.317243391110698,
-1.2490009027033E-16));
#61762=CARTESIAN_POINT('Ctrl Pts',(0.713907354081786,0.337969935177431,
-1.34446060076413E-16));
#61763=CARTESIAN_POINT('Ctrl Pts',(0.702180150875317,0.358180103462127,
3.85806153241612E-16));
#61764=CARTESIAN_POINT('Ctrl Pts',(0.689564616760934,0.377807260377953,
-5.82867087928207E-16));
#61765=CARTESIAN_POINT('Ctrl Pts',(0.672244619169851,0.404753587613862,
-1.91276862451717E-15));
#61766=CARTESIAN_POINT('Ctrl Pts',(0.653250778881373,0.430602076305703,
-3.21975719476629E-15));
#61767=CARTESIAN_POINT('Ctrl Pts',(0.632711953898066,0.455219340276035,
-3.78863607153335E-15));
#61768=CARTESIAN_POINT('Ctrl Pts',(0.625547182264457,0.463806836139848,
-3.98708399844897E-15));
#61769=CARTESIAN_POINT('Ctrl Pts',(0.61819423311545,0.472244298684595,-4.0830565983226E-15));
#61770=CARTESIAN_POINT('Ctrl Pts',(0.610658093425067,0.480525354174928,
-4.08700850940136E-15));
#61771=CARTESIAN_POINT('Ctrl Pts',(0.604662511634519,0.487113574078511,
-4.09015256021187E-15));
#61772=CARTESIAN_POINT('Ctrl Pts',(0.598551877745966,0.493601597685676,
-2.69712728464847E-15));
#61773=CARTESIAN_POINT('Ctrl Pts',(0.592337307151538,0.499977911351174,
-2.74780198594726E-15));
#61774=CARTESIAN_POINT('Ctrl Pts',(0.565761588131446,0.52724530139582,-2.96450507149132E-15));
#61775=CARTESIAN_POINT('Ctrl Pts',(0.537247897169337,0.552518599336613,
-4.23026249514447E-15));
#61776=CARTESIAN_POINT('Ctrl Pts',(0.507012766460455,0.575566644314705,
-4.4200754167889E-15));
#61777=CARTESIAN_POINT('Ctrl Pts',(0.496246418684442,0.583773761729892,
-4.4876653983399E-15));
#61778=CARTESIAN_POINT('Ctrl Pts',(0.485261491302899,0.591698223213175,
-3.12877767334142E-15));
#61779=CARTESIAN_POINT('Ctrl Pts',(0.474066915172834,0.599327810659463,
-2.80331313717852E-15));
#61780=CARTESIAN_POINT('Ctrl Pts',(0.466141780357405,0.604729132549227,
-2.57290241891962E-15));
#61781=CARTESIAN_POINT('Ctrl Pts',(0.458111564520058,0.609982647732742,
-3.13860258315148E-15));
#61782=CARTESIAN_POINT('Ctrl Pts',(0.449979348609982,0.615083700351862,
-3.02535774210355E-15));
#61783=CARTESIAN_POINT('Ctrl Pts',(0.443252675142053,0.619303105701028,
-2.93168572501986E-15));
#61784=CARTESIAN_POINT('Ctrl Pts',(0.436464975643143,0.623412692684743,
-2.97751776474101E-15));
#61785=CARTESIAN_POINT('Ctrl Pts',(0.429618472148824,0.627410530315628,
-2.95596880306448E-15));
#61786=CARTESIAN_POINT('Ctrl Pts',(0.423599928014177,0.630924902614511,
-2.93702579412369E-15));
#61787=CARTESIAN_POINT('Ctrl Pts',(0.417535907052476,0.634352939367129,
-2.51730515131399E-15));
#61788=CARTESIAN_POINT('Ctrl Pts',(0.41142778494146,0.637693315483735,-2.60902410786912E-15));
#61789=CARTESIAN_POINT('Ctrl Pts',(0.380168859262236,0.654788024278328,
-3.07741582773577E-15));
#61790=CARTESIAN_POINT('Ctrl Pts',(0.347756368125765,0.669590917142619,
-3.72554565325771E-15));
#61791=CARTESIAN_POINT('Ctrl Pts',(0.314455649451757,0.682041649083386,
-4.48946435582798E-15));
#61792=CARTESIAN_POINT('Ctrl Pts',(0.281473214350202,0.694373378684276,
-5.24608163117986E-15));
#61793=CARTESIAN_POINT('Ctrl Pts',(0.247618206494094,0.704397831449753,
-3.41330364724715E-15));
#61794=CARTESIAN_POINT('Ctrl Pts',(0.213141916409858,0.712006350953311,
-3.27515792264421E-15));
#61795=CARTESIAN_POINT('Ctrl Pts',(0.203917316012092,0.714042113846228,
-3.23819515481135E-15));
#61796=CARTESIAN_POINT('Ctrl Pts',(0.194648258593662,0.715904633490244,
-9.99391481991553E-16));
#61797=CARTESIAN_POINT('Ctrl Pts',(0.185339650976527,0.717591192759321,
-7.7715611723761E-16));
#61798=CARTESIAN_POINT('Ctrl Pts',(0.178247624911564,0.718876145653285,
-6.0783981729064E-16));
#61799=CARTESIAN_POINT('Ctrl Pts',(0.171133535383714,0.720058667660844,
-2.77537615559827E-15));
#61800=CARTESIAN_POINT('Ctrl Pts',(0.164012249108394,0.721135991470167,
-2.692290834716E-15));
#61801=CARTESIAN_POINT('Ctrl Pts',(0.128128177472471,0.726564612544256,
-2.27362495173283E-15));
#61802=CARTESIAN_POINT('Ctrl Pts',(0.091976494893039,0.72934310385842,-1.96570673819932E-15));
#61803=CARTESIAN_POINT('Ctrl Pts',(0.0558355686356328,0.729384403288966,
-1.9151347174784E-15));
#61804=CARTESIAN_POINT('Ctrl Pts',(0.0260765608470435,0.729418409890416,
-1.88146767879442E-15));
#61805=CARTESIAN_POINT('Ctrl Pts',(-0.00367576053293546,0.727595271520012,
-2.24940245056296E-15));
#61806=CARTESIAN_POINT('Ctrl Pts',(-0.0332514200405915,0.72394427085901,
-1.68962066560141E-15));
#61807=CARTESIAN_POINT('Ctrl Pts',(-0.0500595780777836,0.721869368823837,
-1.37149079581644E-15));
#61808=CARTESIAN_POINT('Ctrl Pts',(-0.0668105374205609,0.719203620011991,
-7.85849759292755E-16));
#61809=CARTESIAN_POINT('Ctrl Pts',(-0.0834712766367304,0.715948760770118,
-6.34908792207511E-16));
#61810=CARTESIAN_POINT('Ctrl Pts',(-0.0901507004907692,0.714643861618909,
-5.74395349015123E-16));
#61811=CARTESIAN_POINT('Ctrl Pts',(-0.0968164869457153,0.713244048991127,
-2.32306328507138E-15));
#61812=CARTESIAN_POINT('Ctrl Pts',(-0.103463703234474,0.711749937291047,
-2.18575157973078E-15));
#61813=CARTESIAN_POINT('Ctrl Pts',(-0.136683088775137,0.704283131571225,
-1.49953794069666E-15));
#61814=CARTESIAN_POINT('Ctrl Pts',(-0.169254000740599,0.694507641639826,
-8.76017226149467E-16));
#61815=CARTESIAN_POINT('Ctrl Pts',(-0.200928233818616,0.682489165262991,
-9.54097911787244E-16));
#61816=CARTESIAN_POINT('Ctrl Pts',(-0.230560396894032,0.67124553227465,
-1.0271446562549E-15));
#61817=CARTESIAN_POINT('Ctrl Pts',(-0.259408473741469,0.658038049136935,
-7.82058107895715E-16));
#61818=CARTESIAN_POINT('Ctrl Pts',(-0.287249018522639,0.642884462366263,
-8.11850586757146E-16));
#61819=CARTESIAN_POINT('Ctrl Pts',(-0.301188758766257,0.635297072643733,
-8.23187715172432E-16));
#61820=CARTESIAN_POINT('Ctrl Pts',(-0.31487550720896,0.627221248807101,
-7.66959557371012E-16));
#61821=CARTESIAN_POINT('Ctrl Pts',(-0.328286140734374,0.618672793771468,
-9.74914593498966E-16));
#61822=CARTESIAN_POINT('Ctrl Pts',(-0.33584241127504,0.613856135495664,
-1.0920876196874E-15));
#61823=CARTESIAN_POINT('Ctrl Pts',(-0.34331098503277,0.608889399167942,
5.25293495758233E-16));
#61824=CARTESIAN_POINT('Ctrl Pts',(-0.350687424397269,0.603775227006381,
6.67868538251071E-16));
#61825=CARTESIAN_POINT('Ctrl Pts',(-0.356960524220523,0.59942601312452,
7.89117752088122E-16));
#61826=CARTESIAN_POINT('Ctrl Pts',(-0.363160963461047,0.594974248859294,
-2.75203808569037E-16));
#61827=CARTESIAN_POINT('Ctrl Pts',(-0.369280669163366,0.590426553784604,
-2.8796409701215E-16));
#61828=CARTESIAN_POINT('Ctrl Pts',(-0.396035202864505,0.570544640003655,
-3.43750369064118E-16));
#61829=CARTESIAN_POINT('Ctrl Pts',(-0.421285868070597,0.548807068655703,
-5.37172934782348E-16));
#61830=CARTESIAN_POINT('Ctrl Pts',(-0.444845541212416,0.525391300388644,
-8.48279779752659E-16));
#61831=CARTESIAN_POINT('Ctrl Pts',(-0.467944926988566,0.502433008005308,
-1.15330850346674E-15));
#61832=CARTESIAN_POINT('Ctrl Pts',(-0.489419406519805,0.477860456590935,
-3.48883792920152E-16));
#61833=CARTESIAN_POINT('Ctrl Pts',(-0.50905162937919,0.45181388155706,5.46437894932694E-17));
#61834=CARTESIAN_POINT('Ctrl Pts',(-0.51885910579262,0.438802050338303,
2.56230093552368E-16));
#61835=CARTESIAN_POINT('Ctrl Pts',(-0.528206121608575,0.425422027334627,
-8.75593447961903E-16));
#61836=CARTESIAN_POINT('Ctrl Pts',(-0.537060862935893,0.41168983410154,
-8.88178419700125E-16));
#61837=CARTESIAN_POINT('Ctrl Pts',(-0.791061003003137,-1.6759841323199E-5,
-0.113133150823703));
#61838=CARTESIAN_POINT('Ctrl Pts',(-0.791095254159769,-0.04398138852515,
-0.111364389783707));
#61839=CARTESIAN_POINT('Ctrl Pts',(-0.787491390648307,-0.0879404613601665,
-0.109595628743711));
#61840=CARTESIAN_POINT('Ctrl Pts',(-0.780199113712507,-0.131278910560445,
-0.107826867703715));
#61841=CARTESIAN_POINT('Ctrl Pts',(-0.75847615196594,-0.260379804893108,
-0.102557905931018));
#61842=CARTESIAN_POINT('Ctrl Pts',(-0.704022786500887,-0.38397338218039,
-0.0972889441583214));
#61843=CARTESIAN_POINT('Ctrl Pts',(-0.623416376522197,-0.487131169850458,
-0.0920199823856242));
#61844=CARTESIAN_POINT('Ctrl Pts',(-0.542809966543505,-0.590288957520528,
-0.086751020612927));
#61845=CARTESIAN_POINT('Ctrl Pts',(-0.43605051205117,-0.673010955573384,
-0.0814820588402293));
#61846=CARTESIAN_POINT('Ctrl Pts',(-0.316032911851495,-0.72530546271973,
-0.0762130970675321));
#61847=CARTESIAN_POINT('Ctrl Pts',(-0.196015311651824,-0.777599969866074,
-0.0709441352948349));
#61848=CARTESIAN_POINT('Ctrl Pts',(-0.0627395657448089,-0.799466986105916,
-0.0656751735221379));
#61849=CARTESIAN_POINT('Ctrl Pts',(0.0676959427613463,-0.788265231092965,
-0.0604062117494408));
#61850=CARTESIAN_POINT('Ctrl Pts',(0.198131451267501,-0.777063476080014,
-0.0551372499767437));
#61851=CARTESIAN_POINT('Ctrl Pts',(0.325726722372791,-0.73279294981427,
-0.0498682882040467));
#61852=CARTESIAN_POINT('Ctrl Pts',(0.435070806474632,-0.660801012792033,
-0.0445993264313496));
#61853=CARTESIAN_POINT('Ctrl Pts',(0.544414890576473,-0.588809075769796,
-0.0393303646586525));
#61854=CARTESIAN_POINT('Ctrl Pts',(0.63550778767486,-0.489095727991068,
-0.0340614028859554));
#61855=CARTESIAN_POINT('Ctrl Pts',(0.69734499205443,-0.37370488387702,-0.0287924411132583));
#61856=CARTESIAN_POINT('Ctrl Pts',(0.759182196434005,-0.258314039762962,
-0.0235234793405607));
#61857=CARTESIAN_POINT('Ctrl Pts',(0.791763708094756,-0.127245699313574,
-0.0182545175678628));
#61858=CARTESIAN_POINT('Ctrl Pts',(0.791157425957054,0.00366855899999786,
-0.0129855557951652));
#61859=CARTESIAN_POINT('Ctrl Pts',(0.79065935752875,0.111216274536829,-0.00865703719677685));
#61860=CARTESIAN_POINT('Ctrl Pts',(0.767763411681256,0.21866000266156,-0.00432851859838852));
#61861=CARTESIAN_POINT('Ctrl Pts',(0.724729084696739,0.317243391110698,
-1.2490009027033E-16));
#61862=CARTESIAN_POINT('',(-0.392911963072353,-0.550971611700039,-3.9489));
#61863=CARTESIAN_POINT('Ctrl Pts',(-0.392911963072352,-0.55097161170004,
-3.9489));
#61864=CARTESIAN_POINT('Ctrl Pts',(-0.410226675319238,-0.540659270969453,
-3.9489));
#61865=CARTESIAN_POINT('Ctrl Pts',(-0.427051408450124,-0.52958559429897,
-3.9489));
#61866=CARTESIAN_POINT('Ctrl Pts',(-0.443332390878944,-0.517780552977276,
-3.9489));
#61867=CARTESIAN_POINT('Ctrl Pts',(-0.466677690336157,-0.500853305130619,
-3.9489));
#61868=CARTESIAN_POINT('Ctrl Pts',(-0.488905894728908,-0.482423482892805,
-3.9489));
#61869=CARTESIAN_POINT('Ctrl Pts',(-0.509923806362163,-0.462642074974146,
-3.9489));
#61870=CARTESIAN_POINT('Ctrl Pts',(-0.517327269552611,-0.455674164558665,
-3.9489));
#61871=CARTESIAN_POINT('Ctrl Pts',(-0.524580430635456,-0.448538306246225,
-3.9489));
#61872=CARTESIAN_POINT('Ctrl Pts',(-0.531678725979323,-0.441240346778602,
-3.9489));
#61873=CARTESIAN_POINT('Ctrl Pts',(-0.538225005850256,-0.434509930129616,
-3.9489));
#61874=CARTESIAN_POINT('Ctrl Pts',(-0.544633942965916,-0.427647286739263,
-3.9489));
#61875=CARTESIAN_POINT('Ctrl Pts',(-0.550897879416926,-0.42066290979901,
-3.9489));
#61876=CARTESIAN_POINT('Ctrl Pts',(-0.573293465677302,-0.395691517214845,
-3.9489));
#61877=CARTESIAN_POINT('Ctrl Pts',(-0.593857165977117,-0.369147438134823,
-3.9489));
#61878=CARTESIAN_POINT('Ctrl Pts',(-0.612442003359716,-0.341256039200072,
-3.9489));
#61879=CARTESIAN_POINT('Ctrl Pts',(-0.62054720638056,-0.329092066696705,
-3.9489));
#61880=CARTESIAN_POINT('Ctrl Pts',(-0.628275646226725,-0.316671295724295,
-3.9489));
#61881=CARTESIAN_POINT('Ctrl Pts',(-0.635613055626581,-0.304010218159141,
-3.9489));
#61882=CARTESIAN_POINT('Ctrl Pts',(-0.640795026572562,-0.295068460583405,
-3.9489));
#61883=CARTESIAN_POINT('Ctrl Pts',(-0.645783514374678,-0.286003276249334,
-3.9489));
#61884=CARTESIAN_POINT('Ctrl Pts',(-0.650560922240377,-0.276844901871744,
-3.9489));
#61885=CARTESIAN_POINT('Ctrl Pts',(-0.654529773316609,-0.269236544991434,
-3.9489));
#61886=CARTESIAN_POINT('Ctrl Pts',(-0.658354827363553,-0.26156085373562,
-3.9489));
#61887=CARTESIAN_POINT('Ctrl Pts',(-0.662033934973313,-0.253821649227226,
-3.9489));
#61888=CARTESIAN_POINT('Ctrl Pts',(-0.676643520622293,-0.223089585065688,
-3.9489));
#61889=CARTESIAN_POINT('Ctrl Pts',(-0.688955077275006,-0.191358774899916,
-3.9489));
#61890=CARTESIAN_POINT('Ctrl Pts',(-0.698971541765702,-0.158905930467818,
-3.9489));
#61891=CARTESIAN_POINT('Ctrl Pts',(-0.705986454727241,-0.136177963004147,
-3.9489));
#61892=CARTESIAN_POINT('Ctrl Pts',(-0.711874862372623,-0.113094947092123,
-3.9489));
#61893=CARTESIAN_POINT('Ctrl Pts',(-0.716624788120144,-0.0897440668667491,
-3.9489));
#61894=CARTESIAN_POINT('Ctrl Pts',(-0.720306876758467,-0.0716427290053002,
-3.9489));
#61895=CARTESIAN_POINT('Ctrl Pts',(-0.723304625101438,-0.0533802762630154,
-3.9489));
#61896=CARTESIAN_POINT('Ctrl Pts',(-0.72560763940422,-0.0349959353965368,
-3.9489));
#61897=CARTESIAN_POINT('Ctrl Pts',(-0.726507866913688,-0.0278096624448529,
-3.9489));
#61898=CARTESIAN_POINT('Ctrl Pts',(-0.727301722894688,-0.0206050118170668,
-3.9489));
#61899=CARTESIAN_POINT('Ctrl Pts',(-0.727987512495698,-0.0133983183097541,
-3.9489));
#61900=CARTESIAN_POINT('Ctrl Pts',(-0.731448056449583,0.0229671786407993,
-3.9489));
#61901=CARTESIAN_POINT('Ctrl Pts',(-0.73217341076392,0.0594719055121494,
-3.9489));
#61902=CARTESIAN_POINT('Ctrl Pts',(-0.730147114733274,0.0958034382110051,
-3.9489));
#61903=CARTESIAN_POINT('Ctrl Pts',(-0.728417200964393,0.126820830393477,
-3.9489));
#61904=CARTESIAN_POINT('Ctrl Pts',(-0.724681055099625,0.157713114353514,
-3.9489));
#61905=CARTESIAN_POINT('Ctrl Pts',(-0.719015395369232,0.188308180357181,
-3.9489));
#61906=CARTESIAN_POINT('Ctrl Pts',(-0.715645853912015,0.206504003648978,
-3.9489));
#61907=CARTESIAN_POINT('Ctrl Pts',(-0.711593191576187,0.224594773207228,
-3.9489));
#61908=CARTESIAN_POINT('Ctrl Pts',(-0.706868098144863,0.24254386435619,
-3.9489));
#61909=CARTESIAN_POINT('Ctrl Pts',(-0.704394402297967,0.251940629282866,
-3.9489));
#61910=CARTESIAN_POINT('Ctrl Pts',(-0.701734975730179,0.261302326828154,
-3.9489));
#61911=CARTESIAN_POINT('Ctrl Pts',(-0.698899697272481,0.270596942138144,
-3.9489));
#61912=CARTESIAN_POINT('Ctrl Pts',(-0.688418916117528,0.304955059140368,
-3.9489));
#61913=CARTESIAN_POINT('Ctrl Pts',(-0.675523352479239,0.338465571894,-3.9489));
#61914=CARTESIAN_POINT('Ctrl Pts',(-0.660343917061696,0.370874272183928,
-3.9489));
#61915=CARTESIAN_POINT('Ctrl Pts',(-0.64790738084614,0.397426773233408,
-3.9489));
#61916=CARTESIAN_POINT('Ctrl Pts',(-0.633936685218803,0.423240167834942,
-3.9489));
#61917=CARTESIAN_POINT('Ctrl Pts',(-0.618478081309822,0.448170731169764,
-3.9489));
#61918=CARTESIAN_POINT('Ctrl Pts',(-0.609699449374064,0.462328299392362,
-3.9489));
#61919=CARTESIAN_POINT('Ctrl Pts',(-0.600440569466785,0.476201051310872,
-3.9489));
#61920=CARTESIAN_POINT('Ctrl Pts',(-0.590720974703061,0.489771952996098,
-3.9489));
#61921=CARTESIAN_POINT('Ctrl Pts',(-0.585324176843069,0.497307186198035,
-3.9489));
#61922=CARTESIAN_POINT('Ctrl Pts',(-0.579785301520311,0.504749336264221,
-3.9489));
#61923=CARTESIAN_POINT('Ctrl Pts',(-0.574107424317768,0.512095298656615,
-3.9489));
#61924=CARTESIAN_POINT('Ctrl Pts',(-0.569610147766929,0.51791381554808,
-3.9489));
#61925=CARTESIAN_POINT('Ctrl Pts',(-0.565026451224481,0.523670769178515,
-3.9489));
#61926=CARTESIAN_POINT('Ctrl Pts',(-0.560365993088301,0.529355290390339,
-3.9489));
#61927=CARTESIAN_POINT('Ctrl Pts',(-0.537332412930287,0.557450140975096,
-3.9489));
#61928=CARTESIAN_POINT('Ctrl Pts',(-0.512378533159309,0.583841839277855,
-3.9489));
#61929=CARTESIAN_POINT('Ctrl Pts',(-0.485742425179841,0.608380818598942,
-3.9489));
#61930=CARTESIAN_POINT('Ctrl Pts',(-0.4588904163952,0.633118700304628,-3.9489));
#61931=CARTESIAN_POINT('Ctrl Pts',(-0.430328032424734,0.655974654499438,
-3.9489));
#61932=CARTESIAN_POINT('Ctrl Pts',(-0.400255088118573,0.676767567817735,
-3.9489));
#61933=CARTESIAN_POINT('Ctrl Pts',(-0.381437541314102,0.689778319794161,
-3.9489));
#61934=CARTESIAN_POINT('Ctrl Pts',(-0.362027717551045,0.701980711486138,
-3.9489));
#61935=CARTESIAN_POINT('Ctrl Pts',(-0.342067962509724,0.713322310757519,
-3.9489));
#61936=CARTESIAN_POINT('Ctrl Pts',(-0.392911963072353,-0.550971611700039,
-3.9489));
#61937=CARTESIAN_POINT('Ctrl Pts',(-0.317943423445919,-0.604318458484074,
-3.94457148140162));
#61938=CARTESIAN_POINT('Ctrl Pts',(-0.12742655914631,-0.688673578978978,
-3.93497400103053));
#61939=CARTESIAN_POINT('Ctrl Pts',(0.198313347812299,-0.676688375201064,
-3.92010755888674));
#61940=CARTESIAN_POINT('Ctrl Pts',(0.496752882142743,-0.50046932737395,
-3.90430067356866));
#61941=CARTESIAN_POINT('Ctrl Pts',(0.675189733576972,-0.203353101808354,
-3.88849378825056));
#61942=CARTESIAN_POINT('Ctrl Pts',(0.690518863850223,0.142889328597765,
-3.87268690293247));
#61943=CARTESIAN_POINT('Ctrl Pts',(0.539036872034762,0.454612727099145,
-3.85688001761438));
#61944=CARTESIAN_POINT('Ctrl Pts',(0.257337933699506,0.656514151291388,
-3.84107313229629));
#61945=CARTESIAN_POINT('Ctrl Pts',(-0.0865270426321366,0.699818987663747,
-3.82526624697819));
#61946=CARTESIAN_POINT('Ctrl Pts',(-0.409489369688631,0.574066239054321,
-3.8094593616601));
#61947=CARTESIAN_POINT('Ctrl Pts',(-0.627215929976506,0.31708661902035,
-3.79409795320704));
#61948=CARTESIAN_POINT('Ctrl Pts',(-0.676676933801994,0.102511671164669,
-3.78400550652667));
#61949=CARTESIAN_POINT('Ctrl Pts',(-0.676746306964879,-9.26850736500048E-6,
-3.779182021619));
#61950=CARTESIAN_POINT('Origin',(-1.87869726832665E-16,-4.25270154953079E-17,
-3.9489));
#61951=CARTESIAN_POINT('',(-0.7911,-9.68818082805472E-17,-3.9489));
#61952=CARTESIAN_POINT('Origin',(0.,0.,-3.9489));
#61953=CARTESIAN_POINT('Origin',(0.,0.,-3.9489));
#61954=CARTESIAN_POINT('',(0.392888236737263,-0.550964357679773,-3.9489));
#61955=CARTESIAN_POINT('Ctrl Pts',(0.342093838304107,0.713335417936174,
-3.9489));
#61956=CARTESIAN_POINT('Ctrl Pts',(0.36243410985328,0.701804032951062,-3.9489));
#61957=CARTESIAN_POINT('Ctrl Pts',(0.382227029135937,0.689385557357458,
-3.9489));
#61958=CARTESIAN_POINT('Ctrl Pts',(0.401406592559599,0.67609942500637,-3.9489));
#61959=CARTESIAN_POINT('Ctrl Pts',(0.427738414049162,0.657858756142971,
-3.9489));
#61960=CARTESIAN_POINT('Ctrl Pts',(0.452915219791259,0.637983175646837,
-3.9489));
#61961=CARTESIAN_POINT('Ctrl Pts',(0.476808155612978,0.616606072714045,
-3.9489));
#61962=CARTESIAN_POINT('Ctrl Pts',(0.485142977099612,0.609148875399504,
-3.9489));
#61963=CARTESIAN_POINT('Ctrl Pts',(0.493321353159824,0.60150879667183,-3.9489));
#61964=CARTESIAN_POINT('Ctrl Pts',(0.501337086175958,0.59369104072589,-3.9489));
#61965=CARTESIAN_POINT('Ctrl Pts',(0.507714221250369,0.587471411710591,
-3.9489));
#61966=CARTESIAN_POINT('Ctrl Pts',(0.513987244720764,0.581140261137621,
-3.9489));
#61967=CARTESIAN_POINT('Ctrl Pts',(0.520145033866962,0.574709095554839,
-3.9489));
#61968=CARTESIAN_POINT('Ctrl Pts',(0.546477934368195,0.547207140002666,
-3.9489));
#61969=CARTESIAN_POINT('Ctrl Pts',(0.570750975301364,0.517837266684296,
-3.9489));
#61970=CARTESIAN_POINT('Ctrl Pts',(0.592740615567436,0.486823864488614,
-3.9489));
#61971=CARTESIAN_POINT('Ctrl Pts',(0.600570848422469,0.475780384109644,
-3.9489));
#61972=CARTESIAN_POINT('Ctrl Pts',(0.608111042112103,0.46452822046729,-3.9489));
#61973=CARTESIAN_POINT('Ctrl Pts',(0.615349294412633,0.453076721193327,
-3.9489));
#61974=CARTESIAN_POINT('Ctrl Pts',(0.62047357290034,0.444969699091146,-3.9489));
#61975=CARTESIAN_POINT('Ctrl Pts',(0.625446502357492,0.43676276545034,-3.9489));
#61976=CARTESIAN_POINT('Ctrl Pts',(0.63026353616155,0.428459160230405,-3.9489));
#61977=CARTESIAN_POINT('Ctrl Pts',(0.634248011417182,0.421590719842154,
-3.9489));
#61978=CARTESIAN_POINT('Ctrl Pts',(0.638120625423605,0.414665084097462,
-3.9489));
#61979=CARTESIAN_POINT('Ctrl Pts',(0.641879525123554,0.407684540413875,
-3.9489));
#61980=CARTESIAN_POINT('Ctrl Pts',(0.645183854741995,0.401548165653247,
-3.9489));
#61981=CARTESIAN_POINT('Ctrl Pts',(0.648400329135512,0.395369324114637,
-3.9489));
#61982=CARTESIAN_POINT('Ctrl Pts',(0.651527671538601,0.389149436432343,
-3.9489));
#61983=CARTESIAN_POINT('Ctrl Pts',(0.667532158485783,0.357318540293221,
-3.9489));
#61984=CARTESIAN_POINT('Ctrl Pts',(0.681206342360694,0.324413949743605,
-3.9489));
#61985=CARTESIAN_POINT('Ctrl Pts',(0.692499081100256,0.290702930386092,
-3.9489));
#61986=CARTESIAN_POINT('Ctrl Pts',(0.703683883584329,0.257314121723617,
-3.9489));
#61987=CARTESIAN_POINT('Ctrl Pts',(0.712532639875156,0.223132979179132,
-3.9489));
#61988=CARTESIAN_POINT('Ctrl Pts',(0.718945440041857,0.18841439839863,-3.9489));
#61989=CARTESIAN_POINT('Ctrl Pts',(0.720661271767476,0.17912497087507,-3.9489));
#61990=CARTESIAN_POINT('Ctrl Pts',(0.722202427728805,0.169797098620667,
-3.9489));
#61991=CARTESIAN_POINT('Ctrl Pts',(0.723566361944834,0.16043577942429,-3.9489));
#61992=CARTESIAN_POINT('Ctrl Pts',(0.724605514495829,0.15330358887633,-3.9489));
#61993=CARTESIAN_POINT('Ctrl Pts',(0.725541534912411,0.146152887091712,
-3.9489));
#61994=CARTESIAN_POINT('Ctrl Pts',(0.726372171175049,0.13899862758013,-3.9489));
#61995=CARTESIAN_POINT('Ctrl Pts',(0.730557736333052,0.102948408380828,
-3.9489));
#61996=CARTESIAN_POINT('Ctrl Pts',(0.732085505672932,0.0667223030632399,
-3.9489));
#61997=CARTESIAN_POINT('Ctrl Pts',(0.730878086010825,0.0306015222127752,
-3.9489));
#61998=CARTESIAN_POINT('Ctrl Pts',(0.729883877878345,0.000859109363216645,
-3.9489));
#61999=CARTESIAN_POINT('Ctrl Pts',(0.727033863426423,-0.028812453629752,
-3.9489));
#62000=CARTESIAN_POINT('Ctrl Pts',(0.722363181286008,-0.0582443055791226,
-3.9489));
#62001=CARTESIAN_POINT('Ctrl Pts',(0.719708783610423,-0.0749707359064128,
-3.9489));
#62002=CARTESIAN_POINT('Ctrl Pts',(0.716465868037568,-0.0916195872890394,
-3.9489));
#62003=CARTESIAN_POINT('Ctrl Pts',(0.712637310914196,-0.108157918201531,
-3.9489));
#62004=CARTESIAN_POINT('Ctrl Pts',(0.711102411545406,-0.114788268189906,
-3.9489));
#62005=CARTESIAN_POINT('Ctrl Pts',(0.70947312652975,-0.121401709586236,
-3.9489));
#62006=CARTESIAN_POINT('Ctrl Pts',(0.707750240343777,-0.127993333808553,
-3.9489));
#62007=CARTESIAN_POINT('Ctrl Pts',(0.699140135230816,-0.160934904691981,
-3.9489));
#62008=CARTESIAN_POINT('Ctrl Pts',(0.688245128415544,-0.193148622364025,
-3.9489));
#62009=CARTESIAN_POINT('Ctrl Pts',(0.675139455165793,-0.224388701026552,
-3.9489));
#62010=CARTESIAN_POINT('Ctrl Pts',(0.662878724445518,-0.253614684679756,
-3.9489));
#62011=CARTESIAN_POINT('Ctrl Pts',(0.648682408810677,-0.281989199846348,
-3.9489));
#62012=CARTESIAN_POINT('Ctrl Pts',(0.63257596521799,-0.309289548789184,
-3.9489));
#62013=CARTESIAN_POINT('Ctrl Pts',(0.624511476822419,-0.322958820095266,
-3.9489));
#62014=CARTESIAN_POINT('Ctrl Pts',(0.615967587212459,-0.336358375532833,
-3.9489));
#62015=CARTESIAN_POINT('Ctrl Pts',(0.606960888675029,-0.349465651586987,
-3.9489));
#62016=CARTESIAN_POINT('Ctrl Pts',(0.601886026129267,-0.356851001951248,
-3.9489));
#62017=CARTESIAN_POINT('Ctrl Pts',(0.596664204853623,-0.364143522529331,
-3.9489));
#62018=CARTESIAN_POINT('Ctrl Pts',(0.591298218799256,-0.371338869599802,
-3.9489));
#62019=CARTESIAN_POINT('Ctrl Pts',(0.586734870194414,-0.377457945699274,
-3.9489));
#62020=CARTESIAN_POINT('Ctrl Pts',(0.582071543364956,-0.38350086171868,
-3.9489));
#62021=CARTESIAN_POINT('Ctrl Pts',(0.577315132755829,-0.389459778321814,
-3.9489));
#62022=CARTESIAN_POINT('Ctrl Pts',(0.556520706295363,-0.415511409114614,
-3.9489));
#62023=CARTESIAN_POINT('Ctrl Pts',(0.533923690776528,-0.439995956565335,
-3.9489));
#62024=CARTESIAN_POINT('Ctrl Pts',(0.50970790495092,-0.462732538395585,
-3.9489));
#62025=CARTESIAN_POINT('Ctrl Pts',(0.485965238395172,-0.485024901108929,
-3.9489));
#62026=CARTESIAN_POINT('Ctrl Pts',(0.4606654197042,-0.505637555568327,-3.9489));
#62027=CARTESIAN_POINT('Ctrl Pts',(0.433956108776739,-0.524358124969866,
-3.9489));
#62028=CARTESIAN_POINT('Ctrl Pts',(0.420613178308345,-0.533710191615534,
-3.9489));
#62029=CARTESIAN_POINT('Ctrl Pts',(0.406918183931599,-0.542589349743738,
-3.9489));
#62030=CARTESIAN_POINT('Ctrl Pts',(0.392888236737269,-0.550964357679769,
-3.9489));
#62031=CARTESIAN_POINT('Origin',(0.,0.,-3.9489));
#62032=CARTESIAN_POINT('Origin',(0.,0.,-4.318617978381));
#62033=CARTESIAN_POINT('Ctrl Pts',(0.392888236737263,-0.550964357679773,
-3.9489));
#62034=CARTESIAN_POINT('Ctrl Pts',(0.484088989988678,-0.485929836599401,
-3.9436310382273));
#62035=CARTESIAN_POINT('Ctrl Pts',(0.633487089009969,-0.309770083749072,
-3.93309311468191));
#62036=CARTESIAN_POINT('Ctrl Pts',(0.704529888150662,0.0295137395378967,
-3.91728622936382));
#62037=CARTESIAN_POINT('Ctrl Pts',(0.605381802721961,0.361579326443786,
-3.90147934404573));
#62038=CARTESIAN_POINT('Ctrl Pts',(0.359987565129825,0.606340404497349,
-3.88567245872763));
#62039=CARTESIAN_POINT('Ctrl Pts',(0.0276308569381634,0.704603699753987,
-3.86986557340955));
#62040=CARTESIAN_POINT('Ctrl Pts',(-0.311401222734635,0.632664694044287,
-3.85405868809145));
#62041=CARTESIAN_POINT('Ctrl Pts',(-0.575206784816063,0.407884951603224,
-3.83825180277336));
#62042=CARTESIAN_POINT('Ctrl Pts',(-0.668516504975362,0.166252472050367,
-3.82643823286988));
#62043=CARTESIAN_POINT('Ctrl Pts',(-0.676723249594477,0.0271363966683822,
-3.81989362473909));
#62044=CARTESIAN_POINT('Ctrl Pts',(-0.676696040235193,1.73011422674348E-5,
-3.818617978381));
#62045=CARTESIAN_POINT('Ctrl Pts',(0.459308237155079,-0.644108029201231,
-4.0149488707953));
#62046=CARTESIAN_POINT('Ctrl Pts',(0.565926998640516,-0.568079050884871,
-4.0096799090226));
#62047=CARTESIAN_POINT('Ctrl Pts',(0.740581699594772,-0.362138485671492,
-3.9991419854772));
#62048=CARTESIAN_POINT('Ctrl Pts',(0.823634689694088,0.0345032057757077,
-3.98333510015911));
#62049=CARTESIAN_POINT('Ctrl Pts',(0.707725054135285,0.422706376754354,
-3.96752821484102));
#62050=CARTESIAN_POINT('Ctrl Pts',(0.42084551909888,0.708845713015883,-3.95172132952292));
#62051=CARTESIAN_POINT('Ctrl Pts',(0.0323020111183534,0.823720979570532,
-3.93591444420484));
#62052=CARTESIAN_POINT('Ctrl Pts',(-0.364045378018858,0.73962027406301,
-3.92010755888674));
#62053=CARTESIAN_POINT('Ctrl Pts',(-0.672448777106521,0.476840232323508,
-3.90430067356865));
#62054=CARTESIAN_POINT('Ctrl Pts',(-0.818406554677498,0.0988716815199221,
-3.88849378825056));
#62055=CARTESIAN_POINT('Ctrl Pts',(-0.766658961359266,-0.302983395308224,
-3.87268690293247));
#62056=CARTESIAN_POINT('Ctrl Pts',(-0.529706957010623,-0.631644832581376,
-3.85688001761438));
#62057=CARTESIAN_POINT('Ctrl Pts',(-0.16479179584882,-0.807718106261876,
-3.84107313229629));
#62058=CARTESIAN_POINT('Ctrl Pts',(0.239932677737653,-0.788667896894534,
-3.82526624697819));
#62059=CARTESIAN_POINT('Ctrl Pts',(0.586695791877696,-0.579096582494008,
-3.80945936166011));
#62060=CARTESIAN_POINT('Ctrl Pts',(0.791728777027483,-0.229630847958036,
-3.79365247634201));
#62061=CARTESIAN_POINT('Ctrl Pts',(0.805501111685453,0.175307571484335,
-3.77784559102392));
#62062=CARTESIAN_POINT('Ctrl Pts',(0.624685763408961,0.53789635206483,-3.76203870570583));
#62063=CARTESIAN_POINT('Ctrl Pts',(0.292962920676836,0.770543647187415,
-3.74623182038774));
#62064=CARTESIAN_POINT('Ctrl Pts',(-0.109531985601694,0.817048059516638,
-3.73042493506964));
#62065=CARTESIAN_POINT('Ctrl Pts',(-0.485566872179705,0.666175351459444,
-3.71461804975155));
#62066=CARTESIAN_POINT('Ctrl Pts',(-0.74430169445999,0.354372366768378,
-3.69881116443346));
#62067=CARTESIAN_POINT('Ctrl Pts',(-0.8232329888101,-0.0430375735757952,
-3.68300427911537));
#62068=CARTESIAN_POINT('Ctrl Pts',(-0.703293050205527,-0.430050778523623,
-3.66719739379728));
#62069=CARTESIAN_POINT('Ctrl Pts',(-0.413456183346354,-0.713175133526495,
-3.65139050847919));
#62070=CARTESIAN_POINT('Ctrl Pts',(-0.0237392800030705,-0.824015311249586,
-3.63558362316109));
#62071=CARTESIAN_POINT('Ctrl Pts',(0.371712403104245,-0.735795267713018,
-3.61977673784301));
#62072=CARTESIAN_POINT('Ctrl Pts',(0.677368238717631,-0.4698266231045,-3.60396985252491));
#62073=CARTESIAN_POINT('Ctrl Pts',(0.819389892225629,-0.0903603404282356,
-3.58816296720682));
#62074=CARTESIAN_POINT('Ctrl Pts',(0.763468702865619,0.310934601401261,
-3.57235608188873));
#62075=CARTESIAN_POINT('Ctrl Pts',(0.523113745259786,0.637115998954219,
-3.55654919657064));
#62076=CARTESIAN_POINT('Ctrl Pts',(0.156388395655667,0.809387086818189,
-3.54074231125254));
#62077=CARTESIAN_POINT('Ctrl Pts',(-0.24811623817114,0.786131744022086,
-3.52493542593445));
#62078=CARTESIAN_POINT('Ctrl Pts',(-0.592682576430445,0.572967843948815,
-3.50912854061636));
#62079=CARTESIAN_POINT('Ctrl Pts',(-0.794072540157967,0.221390125277976,
-3.49332165529827));
#62080=CARTESIAN_POINT('Ctrl Pts',(-0.803635661092522,-0.183669569673137,
-3.47751476998018));
#62081=CARTESIAN_POINT('Ctrl Pts',(-0.61906174312059,-0.544359573083855,
-3.46170788466209));
#62082=CARTESIAN_POINT('Ctrl Pts',(-0.284938944320829,-0.773546756578334,
-3.44590099934399));
#62083=CARTESIAN_POINT('Ctrl Pts',(0.118017538196231,-0.81586558162582,
-3.4300941140259));
#62084=CARTESIAN_POINT('Ctrl Pts',(0.49246411689282,-0.661092943674721,
-3.41428722870781));
#62085=CARTESIAN_POINT('Ctrl Pts',(0.747944440046074,-0.346617802785286,
-3.39848034338972));
#62086=CARTESIAN_POINT('Ctrl Pts',(0.822741244675879,0.0515909964307694,
-3.38267345807163));
#62087=CARTESIAN_POINT('Ctrl Pts',(0.698785608665519,0.437336780668508,
-3.36686657275354));
#62088=CARTESIAN_POINT('Ctrl Pts',(0.406021922608743,0.717433610144265,
-3.35105968743544));
#62089=CARTESIAN_POINT('Ctrl Pts',(0.0151741200765717,0.824217527527435,
-3.33525280211735));
#62090=CARTESIAN_POINT('Ctrl Pts',(-0.3793393469878,0.731892373529335,-3.31944591679926));
#62091=CARTESIAN_POINT('Ctrl Pts',(-0.682214499414893,0.46276145409014,
-3.30363903148117));
#62092=CARTESIAN_POINT('Ctrl Pts',(-0.820284741821662,0.0818396538244422,
-3.28783214616308));
#62093=CARTESIAN_POINT('Ctrl Pts',(-0.760195969456813,-0.318852433933235,
-3.27202526084498));
#62094=CARTESIAN_POINT('Ctrl Pts',(-0.516464034345362,-0.642518239298502,
-3.2562183755269));
#62095=CARTESIAN_POINT('Ctrl Pts',(-0.147968100840412,-0.810968697137697,
-3.2404114902088));
#62096=CARTESIAN_POINT('Ctrl Pts',(0.256272997221724,-0.78351064925662,
-3.22460460489071));
#62097=CARTESIAN_POINT('Ctrl Pts',(0.598605343294585,-0.566777231002363,
-3.20879771957262));
#62098=CARTESIAN_POINT('Ctrl Pts',(0.796330531612867,-0.213125481875595,
-3.19299083425453));
#62099=CARTESIAN_POINT('Ctrl Pts',(0.801683406353151,0.19201172511475,-3.17718394893643));
#62100=CARTESIAN_POINT('Ctrl Pts',(0.613370855098921,0.550763997297166,
-3.16137706361834));
#62101=CARTESIAN_POINT('Ctrl Pts',(0.27688419046779,0.776466310713176,-3.14557017830025));
#62102=CARTESIAN_POINT('Ctrl Pts',(-0.126490343206336,0.814594978918406,
-3.12976329298216));
#62103=CARTESIAN_POINT('Ctrl Pts',(-0.499308168325542,0.655939128004212,
-3.11395640766407));
#62104=CARTESIAN_POINT('Ctrl Pts',(-0.751506396787274,0.338825799182031,
-3.09814952234598));
#62105=CARTESIAN_POINT('Ctrl Pts',(-0.822160632548107,-0.0601388467766978,
-3.08234263702788));
#62106=CARTESIAN_POINT('Ctrl Pts',(-0.694202688143384,-0.444575544062011,
-3.06653575170979));
#62107=CARTESIAN_POINT('Ctrl Pts',(-0.39854380561222,-0.72161459354122,
-3.0507288663917));
#62108=CARTESIAN_POINT('Ctrl Pts',(-0.00660732112534875,-0.824330716345741,
-3.03492198107361));
#62109=CARTESIAN_POINT('Ctrl Pts',(0.386925316718677,-0.727910424355693,
-3.01911509575552));
#62110=CARTESIAN_POINT('Ctrl Pts',(0.686987071048648,-0.455646300122731,
-3.00330821043742));
#62111=CARTESIAN_POINT('Ctrl Pts',(0.821090988765058,-0.0733101273519162,
-2.98750132511934));
#62112=CARTESIAN_POINT('Ctrl Pts',(0.75684112385447,0.326735825777088,-2.97169443980124));
#62113=CARTESIAN_POINT('Ctrl Pts',(0.509758537822454,0.647851078351074,
-2.95588755448315));
#62114=CARTESIAN_POINT('Ctrl Pts',(0.139531823323549,0.812462711072661,
-2.94008066916506));
#62115=CARTESIAN_POINT('Ctrl Pts',(-0.264402075070642,0.780804923973891,
-2.92427378384697));
#62116=CARTESIAN_POINT('Ctrl Pts',(-0.604463452097174,0.560525397892281,
-2.90846689852887));
#62117=CARTESIAN_POINT('Ctrl Pts',(-0.798502507817305,0.204837817829157,
-2.89266001321079));
#62118=CARTESIAN_POINT('Ctrl Pts',(-0.799644558175188,-0.200333140504363,
-2.87685312789269));
#62119=CARTESIAN_POINT('Ctrl Pts',(-0.607613714126209,-0.55710893100837,
-2.8610462425746));
#62120=CARTESIAN_POINT('Ctrl Pts',(-0.268799529105187,-0.779301995221598,
-2.84523935725651));
#62121=CARTESIAN_POINT('Ctrl Pts',(0.134949485424267,-0.813236388135246,
-2.82943247193842));
#62122=CARTESIAN_POINT('Ctrl Pts',(0.506098287232193,-0.650714461391611,
-2.81362558662032));
#62123=CARTESIAN_POINT('Ctrl Pts',(0.754987179934878,-0.330997197476829,
-2.79781870130224));
#62124=CARTESIAN_POINT('Ctrl Pts',(0.821491215144233,0.0686802012546899,
-2.78201181598414));
#62125=CARTESIAN_POINT('Ctrl Pts',(0.689544783659541,0.451766286846917,
-2.76620493066606));
#62126=CARTESIAN_POINT('Ctrl Pts',(0.391022640102679,0.725717632092995,
-2.75039804534795));
#62127=CARTESIAN_POINT('Ctrl Pts',(-0.00196019151241356,0.824354865487413,
-2.73459116002987));
#62128=CARTESIAN_POINT('Ctrl Pts',(-0.394469492901894,0.723849850295803,
-2.71878427471178));
#62129=CARTESIAN_POINT('Ctrl Pts',(-0.691685438112023,0.448481929744459,
-2.70297738939368));
#62130=CARTESIAN_POINT('Ctrl Pts',(-0.8218085459694,0.0647726823220635,
-2.68717050407559));
#62131=CARTESIAN_POINT('Ctrl Pts',(-0.753404528430612,-0.33458392541152,
-2.6713636187575));
#62132=CARTESIAN_POINT('Ctrl Pts',(-0.502997979981963,-0.65311394008825,
-2.65555673343941));
#62133=CARTESIAN_POINT('Ctrl Pts',(-0.131080474345465,-0.81386896724774,
-2.63974984812132));
#62134=CARTESIAN_POINT('Ctrl Pts',(0.272502593659544,-0.77801486043157,
-2.62394296280322));
#62135=CARTESIAN_POINT('Ctrl Pts',(0.610256270077472,-0.554213019907206,
-2.60813607748514));
#62136=CARTESIAN_POINT('Ctrl Pts',(0.80058823416634,-0.196528028326635,
-2.59232919216704));
#62137=CARTESIAN_POINT('Ctrl Pts',(0.797519336783819,0.208632917008397,
-2.57652230684895));
#62138=CARTESIAN_POINT('Ctrl Pts',(0.6017909420572,0.56339368887257,-2.56071542153086));
#62139=CARTESIAN_POINT('Ctrl Pts',(0.260685833493737,0.782053503808537,
-2.54490853621277));
#62140=CARTESIAN_POINT('Ctrl Pts',(-0.143394051139944,0.811789956023853,
-2.52910165089467));
#62141=CARTESIAN_POINT('Ctrl Pts',(-0.512833740181423,0.645419508176711,
-2.51329476557658));
#62142=CARTESIAN_POINT('Ctrl Pts',(-0.758386413513802,0.323132843272245,
-2.49748788025849));
#62143=CARTESIAN_POINT('Ctrl Pts',(-0.820733064771053,-0.0772141372745434,
-2.4816809949404));
#62144=CARTESIAN_POINT('Ctrl Pts',(-0.684812398335245,-0.458908232318686,
-2.46587410962231));
#62145=CARTESIAN_POINT('Ctrl Pts',(-0.383459238475105,-0.729742282611901,
-2.45006722430422));
#62146=CARTESIAN_POINT('Ctrl Pts',(0.0105274924210566,-0.824289972343991,
-2.43426033898612));
#62147=CARTESIAN_POINT('Ctrl Pts',(0.401971060656972,-0.719711089950575,
-2.41845345366803));
#62148=CARTESIAN_POINT('Ctrl Pts',(0.69630909311321,-0.441269116811264,
-2.40264656834994));
#62149=CARTESIAN_POINT('Ctrl Pts',(0.822437335928101,-0.0562282409028078,
-2.38683968303185));
#62150=CARTESIAN_POINT('Ctrl Pts',(0.7498865543874,0.342395885127914,-2.37103279771376));
#62151=CARTESIAN_POINT('Ctrl Pts',(0.496183091062214,0.658306256044616,
-2.35522591239567));
#62152=CARTESIAN_POINT('Ctrl Pts',(0.122614966774459,0.815187313766863,
-2.33941902707757));
#62153=CARTESIAN_POINT('Ctrl Pts',(-0.280573678014902,0.775140759996998,
-2.32361214175948));
#62154=CARTESIAN_POINT('Ctrl Pts',(-0.615983171527093,0.547840778875538,
-2.30780525644139));
#62155=CARTESIAN_POINT('Ctrl Pts',(-0.802587485371274,0.188197010945846,
-2.2919983711233));
#62156=CARTESIAN_POINT('Ctrl Pts',(-0.795307971733777,-0.21691015813059,
-2.27619148580521));
#62157=CARTESIAN_POINT('Ctrl Pts',(-0.595903167835748,-0.569617592044745,
-2.26038460048711));
#62158=CARTESIAN_POINT('Ctrl Pts',(-0.252543980030274,-0.784720539271147,
-2.24457771516903));
#62159=CARTESIAN_POINT('Ctrl Pts',(0.151823128217758,-0.810255838819881,
-2.22877082985093));
#62160=CARTESIAN_POINT('Ctrl Pts',(0.519513799646595,-0.640054840291277,
-2.21296394453284));
#62161=CARTESIAN_POINT('Ctrl Pts',(0.761703730357511,-0.315233586032623,
-2.19715705921474));
#62162=CARTESIAN_POINT('Ctrl Pts',(0.819886263319798,0.0857397330473568,
-2.18135017389666));
#62163=CARTESIAN_POINT('Ctrl Pts',(0.680006043336776,0.46600060904359,-2.16554328857856));
#62164=CARTESIAN_POINT('Ctrl Pts',(0.375854417686602,0.733688110377292,
-2.14973640326048));
#62165=CARTESIAN_POINT('Ctrl Pts',(-0.0190936562077946,0.82413604392488,
-2.13392951794238));
#62166=CARTESIAN_POINT('Ctrl Pts',(-0.409429209705767,0.715494590366164,
-2.11812263262429));
#62167=CARTESIAN_POINT('Ctrl Pts',(-0.700857536630393,0.434008640411582,
-2.1023157473062));
#62168=CARTESIAN_POINT('Ctrl Pts',(-0.822977290722719,0.0476777260177834,
-2.08650886198811));
#62169=CARTESIAN_POINT('Ctrl Pts',(-0.746287581717071,-0.350170861121284,
-2.07070197667002));
#62170=CARTESIAN_POINT('Ctrl Pts',(-0.489314607170079,-0.66342746537472,
-2.05489509135192));
#62171=CARTESIAN_POINT('Ctrl Pts',(-0.11413621500816,-0.816417608229481,
-2.03908820603383));
#62172=CARTESIAN_POINT('Ctrl Pts',(0.288614456342509,-0.772182933114719,
-2.02328132071574));
#62173=CARTESIAN_POINT('Ctrl Pts',(0.621643537857595,-0.541409363091763,
-2.00747443539765));
#62174=CARTESIAN_POINT('Ctrl Pts',(0.804500045483962,-0.179845665557549,
-1.99166755007956));
#62175=CARTESIAN_POINT('Ctrl Pts',(0.793010701884583,0.225163969808788,
-1.97586066476146));
#62176=CARTESIAN_POINT('Ctrl Pts',(0.589951027426904,0.575779968253043,
-1.96005377944338));
#62177=CARTESIAN_POINT('Ctrl Pts',(0.244374848153105,0.787302813530905,
-1.94424689412528));
#62178=CARTESIAN_POINT('Ctrl Pts',(-0.160235806195098,0.808634202230244,
-1.92844000880719));
#62179=CARTESIAN_POINT('Ctrl Pts',(-0.526137744084377,0.634621037197269,
-1.9126331234891));
#62180=CARTESIAN_POINT('Ctrl Pts',(-0.764938772147653,0.307300278992347,
-1.89682623817101));
#62181=CARTESIAN_POINT('Ctrl Pts',(-0.818950902257319,-0.0942560676851014,
-1.88101935285291));
#62182=CARTESIAN_POINT('Ctrl Pts',(-0.675126237820197,-0.473042650942049,
-1.86521246753482));
#62183=CARTESIAN_POINT('Ctrl Pts',(-0.368208999168154,-0.737554689182519,
-1.84940558221673));
#62184=CARTESIAN_POINT('Ctrl Pts',(0.0276577576026398,-0.82389309685658,
-1.83359869689864));
#62185=CARTESIAN_POINT('Ctrl Pts',(0.416843134459967,-0.711200806985709,
-1.81779181158055));
#62186=CARTESIAN_POINT('Ctrl Pts',(0.705330277365677,-0.42670128478221,
-1.80198492626245));
#62187=CARTESIAN_POINT('Ctrl Pts',(0.823428352030309,-0.0391220612466472,
-1.78617804094437));
#62188=CARTESIAN_POINT('Ctrl Pts',(0.742607999160884,0.357908013581426,
-1.77037115562627));
#62189=CARTESIAN_POINT('Ctrl Pts',(0.482393270201465,0.668477014913655,
-1.75456427030818));
#62190=CARTESIAN_POINT('Ctrl Pts',(0.105645134874769,0.817559717745943,
-1.73875738499009));
#62191=CARTESIAN_POINT('Ctrl Pts',(-0.296624060121656,0.769141699272949,
-1.722950499672));
#62192=CARTESIAN_POINT('Ctrl Pts',(-0.627236757667293,0.534919467242084,
-1.70714361435391));
#62193=CARTESIAN_POINT('Ctrl Pts',(-0.806325707920169,0.1714748942282,-1.69133672903581));
#62194=CARTESIAN_POINT('Ctrl Pts',(-0.790627775374702,-0.233393460511612,
-1.67552984371772));
#62195=CARTESIAN_POINT('Ctrl Pts',(-0.583935163748167,-0.581880151871441,
-1.65972295839963));
#62196=CARTESIAN_POINT('Ctrl Pts',(-0.236179320246973,-0.789800047664733,
-1.64391607308154));
#62197=CARTESIAN_POINT('Ctrl Pts',(0.16863117638069,-0.806925221415217,
-1.62810918776345));
#62198=CARTESIAN_POINT('Ctrl Pts',(0.532704858012667,-0.629118685824256,
-1.61230230244535));
#62199=CARTESIAN_POINT('Ctrl Pts',(0.768091189452786,-0.299333779063673,
-1.59649541712726));
#62200=CARTESIAN_POINT('Ctrl Pts',(0.817927082616174,0.102762221300083,
-1.58068853180917));
#62201=CARTESIAN_POINT('Ctrl Pts',(0.670173508875303,0.480033597371371,
-1.56488164649108));
#62202=CARTESIAN_POINT('Ctrl Pts',(0.360523808735873,0.741341601380979,
-1.54907476117299));
#62203=CARTESIAN_POINT('Ctrl Pts',(-0.0362188715584176,0.823561157380901,
-1.53326787585489));
#62204=CARTESIAN_POINT('Ctrl Pts',(-0.424212034108152,0.706830203600099,
-1.51746099053681));
#62205=CARTESIAN_POINT('Ctrl Pts',(-0.709726832198183,0.419347839223556,
-1.50165410521871));
#62206=CARTESIAN_POINT('Ctrl Pts',(-0.823790471129699,0.0305621707253191,
-1.48584721990062));
#62207=CARTESIAN_POINT('Ctrl Pts',(-0.738848204167142,-0.365606506783623,
-1.47004033458253));
#62208=CARTESIAN_POINT('Ctrl Pts',(-0.475419827761178,-0.673454359236813,
-1.45423344926444));
#62209=CARTESIAN_POINT('Ctrl Pts',(-0.0971426435341273,-0.818613518951852,
-1.43842656394635));
#62210=CARTESIAN_POINT('Ctrl Pts',(0.304601624198931,-0.766017386969061,
-1.42261967862825));
#62211=CARTESIAN_POINT('Ctrl Pts',(0.632762226807305,-0.528371792329412,
-1.40681279331016));
#62212=CARTESIAN_POINT('Ctrl Pts',(0.808064275481866,-0.163085601122539,
-1.39100590799207));
#62213=CARTESIAN_POINT('Ctrl Pts',(0.788159449594768,0.241597741334656,
-1.37519902267398));
#62214=CARTESIAN_POINT('Ctrl Pts',(0.577856226600103,0.58791748399161,-1.35939213735589));
#62215=CARTESIAN_POINT('Ctrl Pts',(0.227958281547799,0.792211971935104,
-1.34358525203779));
#62216=CARTESIAN_POINT('Ctrl Pts',(-0.177008331952761,0.805129080969527,
-1.32777836671971));
#62217=CARTESIAN_POINT('Ctrl Pts',(-0.53921443208789,0.623548380506011,
-1.31197148140161));
#62218=CARTESIAN_POINT('Ctrl Pts',(-0.771160641766101,0.291334946744169,
-1.29616459608352));
#62219=CARTESIAN_POINT('Ctrl Pts',(-0.816814914983744,-0.111257275104306,
-1.28035771076543));
#62220=CARTESIAN_POINT('Ctrl Pts',(-0.665148391468669,-0.486972693207921,
-1.26455082544734));
#62221=CARTESIAN_POINT('Ctrl Pts',(-0.352799676501823,-0.745048437931215,
-1.24874394012924));
#62222=CARTESIAN_POINT('Ctrl Pts',(0.0447760733506051,-0.823140261352119,
-1.23293705481115));
#62223=CARTESIAN_POINT('Ctrl Pts',(0.431535112702248,-0.702383252297912,
-1.21713016949306));
#62224=CARTESIAN_POINT('Ctrl Pts',(0.714046726236198,-0.411949098014427,
-1.20132328417497));
#62225=CARTESIAN_POINT('Ctrl Pts',(0.824063608906776,-0.0219989790461579,
-1.18551639885688));
#62226=CARTESIAN_POINT('Ctrl Pts',(0.735008602848248,0.373265509178923,
-1.16970951353879));
#62227=CARTESIAN_POINT('Ctrl Pts',(0.468395033082173,0.678358960718796,
-1.1539026282207));
#62228=CARTESIAN_POINT('Ctrl Pts',(0.0886296593786528,0.819578898021391,
-1.1380957429026));
#62229=CARTESIAN_POINT('Ctrl Pts',(-0.312546286881678,0.762810333674112,
-1.12228885758451));
#62230=CARTESIAN_POINT('Ctrl Pts',(-0.638219348446799,0.521767045597627,
-1.10648197226642));
#62231=CARTESIAN_POINT('Ctrl Pts',(-0.809715560378535,0.154678692405936,
-1.09067508694833));
#62232=CARTESIAN_POINT('Ctrl Pts',(-0.785605991159775,-0.249775926096571,
-1.07486820163024));
#62233=CARTESIAN_POINT('Ctrl Pts',(-0.571714872596114,-0.593891312494082,
-1.05906131631214));
#62234=CARTESIAN_POINT('Ctrl Pts',(-0.219712620047033,-0.794538325819216,
-1.04325443099405));
#62235=CARTESIAN_POINT('Ctrl Pts',(0.18536636805697,-0.803245974902395,
-1.02744754567596));
#62236=CARTESIAN_POINT('Ctrl Pts',(0.545665763181605,-0.617910722916321,
-1.01164066035787));
#62237=CARTESIAN_POINT('Ctrl Pts',(0.774146797542223,-0.283304646023772,
-0.995833775039777));
#62238=CARTESIAN_POINT('Ctrl Pts',(0.815614519490262,0.119740311508712,
-0.980026889721687));
#62239=CARTESIAN_POINT('Ctrl Pts',(0.660051428385883,0.493859188928676,
-0.964220004403594));
#62240=CARTESIAN_POINT('Ctrl Pts',(0.345037436784345,0.748674798441101,
-0.948413119085503));
#62241=CARTESIAN_POINT('Ctrl Pts',(-0.0533284386772662,0.822630454233114,
-0.93260623376741));
#62242=CARTESIAN_POINT('Ctrl Pts',(-0.43881157924352,0.697860433414406,
-0.916799348449319));
#62243=CARTESIAN_POINT('Ctrl Pts',(-0.718289492868495,0.404505860326217,
-0.900992463131228));
#62244=CARTESIAN_POINT('Ctrl Pts',(-0.824247735858698,0.0134334111581012,
-0.885185577813136));
#62245=CARTESIAN_POINT('Ctrl Pts',(-0.731089609936848,-0.380884193483954,
-0.869378692495045));
#62246=CARTESIAN_POINT('Ctrl Pts',(-0.461319644944187,-0.683190289591489,
-0.853571807176952));
#62247=CARTESIAN_POINT('Ctrl Pts',(-0.0801071019341396,-0.820455750679614,
-0.837764921858862));
#62248=CARTESIAN_POINT('Ctrl Pts',(0.320457190031065,-0.759520885796387,
-0.82195803654077));
#62249=CARTESIAN_POINT('Ctrl Pts',(0.64360753313747,-0.515105940455199,
-0.806151151222677));
#62250=CARTESIAN_POINT('Ctrl Pts',(0.811279384247447,-0.146255076146497,
-0.790344265904585));
#62251=CARTESIAN_POINT('Ctrl Pts',(0.782967675880284,0.257927131434756,
-0.774537380586495));
#62252=CARTESIAN_POINT('Ctrl Pts',(0.565511765091529,0.599800992118718,
-0.758730495268401));
#62253=CARTESIAN_POINT('Ctrl Pts',(0.211443226395748,0.79677885803709,-0.742923609950311));
#62254=CARTESIAN_POINT('Ctrl Pts',(-0.193704381904162,0.801276106616604,
-0.727116724632219));
#62255=CARTESIAN_POINT('Ctrl Pts',(-0.552058154456458,0.612206322003997,
-0.711309839314127));
#62256=CARTESIAN_POINT('Ctrl Pts',(-0.777049334233002,0.27524374429146,
-0.695502953996036));
#62257=CARTESIAN_POINT('Ctrl Pts',(-0.81432602579586,-0.128210414222302,
-0.679696068677944));
#62258=CARTESIAN_POINT('Ctrl Pts',(-0.654883170172903,-0.50069234069219,
-0.663889183359853));
#62259=CARTESIAN_POINT('Ctrl Pts',(-0.337237928017941,-0.752220291211092,
-0.64808229804176));
#62260=CARTESIAN_POINT('Ctrl Pts',(0.0618750437588687,-0.822031791090449,
-0.632275412723669));
#62261=CARTESIAN_POINT('Ctrl Pts',(0.446040647768021,-0.693262235479634,
-0.616468527405576));
#62262=CARTESIAN_POINT('Ctrl Pts',(0.722454673814721,-0.397018930136584,
-0.600661642087485));
#62263=CARTESIAN_POINT('Ctrl Pts',(0.824342832097085,-0.00486639226674949,
-0.584854756769393));
#62264=CARTESIAN_POINT('Ctrl Pts',(0.727091648741029,0.388461736770279,
-0.569047871451302));
#62265=CARTESIAN_POINT('Ctrl Pts',(0.454194427591786,0.68794782400129,-0.55324098613321));
#62266=CARTESIAN_POINT('Ctrl Pts',(0.0715758917604166,0.821243982213708,
-0.537434100815118));
#62267=CARTESIAN_POINT('Ctrl Pts',(-0.328333479154766,0.756149398643979,
-0.521627215497028));
#62268=CARTESIAN_POINT('Ctrl Pts',(-0.648926198877239,0.508389196398115,
-0.505820330178935));
#62269=CARTESIAN_POINT('Ctrl Pts',(-0.812755578172857,0.137815662216995,
-0.490013444860843));
#62270=CARTESIAN_POINT('Ctrl Pts',(-0.780244788732774,-0.266050476900792,
-0.474206559542751));
#62271=CARTESIAN_POINT('Ctrl Pts',(-0.559247574111642,-0.60564588453435,
-0.45839967422466));
#62272=CARTESIAN_POINT('Ctrl Pts',(-0.203150993809032,-0.798933326578804,
-0.442592788906568));
#62273=CARTESIAN_POINT('Ctrl Pts',(0.202021472869058,-0.799219688886387,
-0.426785903588476));
#62274=CARTESIAN_POINT('Ctrl Pts',(0.558390915439125,-0.60643579392732,
-0.410979018270384));
#62275=CARTESIAN_POINT('Ctrl Pts',(0.779867938326921,-0.267153112241133,
-0.395172132952293));
#62276=CARTESIAN_POINT('Ctrl Pts',(0.812949573067638,0.136666668350266,
-0.379365247634201));
#62277=CARTESIAN_POINT('Ctrl Pts',(0.649644175094028,0.507471410420593,
-0.363558362316109));
#62278=CARTESIAN_POINT('Ctrl Pts',(0.329401992628576,0.755684533273304,
-0.347751476998018));
#62279=CARTESIAN_POINT('Ctrl Pts',(-0.0704149653712633,0.821344336594747,
-0.331944591679926));
#62280=CARTESIAN_POINT('Ctrl Pts',(-0.453221537562226,0.688589155153321,
-0.316137706361834));
#62281=CARTESIAN_POINT('Ctrl Pts',(-0.726541818918978,0.389489116166805,
-0.300330821043743));
#62282=CARTESIAN_POINT('Ctrl Pts',(-0.82434888785108,-0.00370115231292693,
-0.284523935725651));
#62283=CARTESIAN_POINT('Ctrl Pts',(-0.723015150118187,-0.395997320460584,
-0.268717050407559));
#62284=CARTESIAN_POINT('Ctrl Pts',(-0.447020152570759,-0.692631050246883,
-0.252910165089467));
#62285=CARTESIAN_POINT('Ctrl Pts',(-0.0630369465961534,-0.821943507128117,
-0.237103279771376));
#62286=CARTESIAN_POINT('Ctrl Pts',(0.336174296148222,-0.752696237081474,
-0.221296394453284));
#62287=CARTESIAN_POINT('Ctrl Pts',(0.65417478556092,-0.501617537571764,
-0.205489509135192));
#62288=CARTESIAN_POINT('Ctrl Pts',(0.81414395454377,-0.129361364859212,
-0.1896826238171));
#62289=CARTESIAN_POINT('Ctrl Pts',(0.777437678945939,0.274145090266998,
-0.173875738499009));
#62290=CARTESIAN_POINT('Ctrl Pts',(0.552922868401512,0.611425348207658,
-0.158068853180917));
#62291=CARTESIAN_POINT('Ctrl Pts',(0.194837029113287,0.801001518694738,
-0.142261967862825));
#62292=CARTESIAN_POINT('Ctrl Pts',(-0.210317155848737,0.797076904759738,
-0.126455082544734));
#62293=CARTESIAN_POINT('Ctrl Pts',(-0.564662553237619,0.600599838466151,
-0.110648197226641));
#62294=CARTESIAN_POINT('Ctrl Pts',(-0.782603888542138,0.25903347409295,
-0.0948413119085497));
#62295=CARTESIAN_POINT('Ctrl Pts',(-0.811482211068061,-0.14510786755727,
-0.0790344265904577));
#62296=CARTESIAN_POINT('Ctrl Pts',(-0.644341077190917,-0.514196238853462,
-0.0632275412723662));
#62297=CARTESIAN_POINT('Ctrl Pts',(-0.321518569789179,-0.759066033017091,
-0.0474206559542749));
#62298=CARTESIAN_POINT('Ctrl Pts',(0.0789236478635419,-0.820570308434437,
-0.0316137706361836));
#62299=CARTESIAN_POINT('Ctrl Pts',(0.460403265087323,-0.68383797063051,
-0.0158068853180922));
#62300=CARTESIAN_POINT('Ctrl Pts',(0.640409690535753,-0.482558394510364,
-0.0052689617726974));
#62301=CARTESIAN_POINT('Ctrl Pts',(0.701077753000062,-0.366509473613416,
0.));
#62302=CARTESIAN_POINT('Ctrl Pts',(0.437168237015807,-0.613060138694078,
-3.9929325805302));
#62303=CARTESIAN_POINT('Ctrl Pts',(0.538647662423237,-0.540695979456381,
-3.9876636187575));
#62304=CARTESIAN_POINT('Ctrl Pts',(0.704883496066505,-0.344682351697352,
-3.9771256952121));
#62305=CARTESIAN_POINT('Ctrl Pts',(0.783933089179612,0.032840050363104,
-3.96131880989402));
#62306=CARTESIAN_POINT('Ctrl Pts',(0.673610636997511,0.402330693317498,
-3.94551192457592));
#62307=CARTESIAN_POINT('Ctrl Pts',(0.400559534442527,0.674677276843038,
-3.92970503925783));
#62308=CARTESIAN_POINT('Ctrl Pts',(0.0307449597249569,0.784015219631683,
-3.91389815393974));
#62309=CARTESIAN_POINT('Ctrl Pts',(-0.34649732625745,0.703968414056769,
-3.89809126862165));
#62310=CARTESIAN_POINT('Ctrl Pts',(-0.640034779676368,0.45385513875008,
-3.88228438330356));
#62311=CARTESIAN_POINT('Ctrl Pts',(-0.778956965558928,0.0941057773502482,
-3.86647749798546));
#62312=CARTESIAN_POINT('Ctrl Pts',(-0.72970375755886,-0.28837870967082,
-3.85067061266738));
#62313=CARTESIAN_POINT('Ctrl Pts',(-0.504173532714486,-0.601197704596164,
-3.83486372734928));
#62314=CARTESIAN_POINT('Ctrl Pts',(-0.156848349405001,-0.768783731612082,
-3.81905684203119));
#62315=CARTESIAN_POINT('Ctrl Pts',(0.228367221059955,-0.750651798042835,
-3.80324995671309));
#62316=CARTESIAN_POINT('Ctrl Pts',(0.558415339094314,-0.55118243382451,
-3.78744307139501));
#62317=CARTESIAN_POINT('Ctrl Pts',(0.753565134802757,-0.218561969600303,
-3.77163618607691));
#62318=CARTESIAN_POINT('Ctrl Pts',(0.766673602657173,0.166857233904678,
-3.75582930075883));
#62319=CARTESIAN_POINT('Ctrl Pts',(0.594574082907553,0.51196817497967,-3.74002241544072));
#62320=CARTESIAN_POINT('Ctrl Pts',(0.278841251218513,0.733401190170503,
-3.72421553012264));
#62321=CARTESIAN_POINT('Ctrl Pts',(-0.104252223602443,0.777663953837329,
-3.70840864480454));
#62322=CARTESIAN_POINT('Ctrl Pts',(-0.462161129046788,0.634063751490217,
-3.69260175948646));
#62323=CARTESIAN_POINT('Ctrl Pts',(-0.708424176301216,0.33729058243504,
-3.67679487416836));
#62324=CARTESIAN_POINT('Ctrl Pts',(-0.783550751452885,-0.040963036679043,
-3.66098798885027));
#62325=CARTESIAN_POINT('Ctrl Pts',(-0.669392268617226,-0.409321073445001,
-3.64518110353218));
#62326=CARTESIAN_POINT('Ctrl Pts',(-0.393526386281157,-0.678798006624954,
-3.62937421821409));
#62327=CARTESIAN_POINT('Ctrl Pts',(-0.0225949772885551,-0.784295363663123,
-3.61356733289599));
#62328=CARTESIAN_POINT('Ctrl Pts',(0.353794778313819,-0.700327784197924,
-3.59776044757791));
#62329=CARTESIAN_POINT('Ctrl Pts',(0.644717108852341,-0.447179606004612,
-3.58195356225981));
#62330=CARTESIAN_POINT('Ctrl Pts',(0.779892903361764,-0.0860047077880307,
-3.56614667694172));
#62331=CARTESIAN_POINT('Ctrl Pts',(0.726667278853556,0.295946644379268,
-3.55033979162363));
#62332=CARTESIAN_POINT('Ctrl Pts',(0.497898133049898,0.60640514475106,-3.53453290630554));
#62333=CARTESIAN_POINT('Ctrl Pts',(0.148850017674368,0.770372262425151,
-3.51872602098745));
#62334=CARTESIAN_POINT('Ctrl Pts',(-0.236156309950195,0.748237895155053,
-3.50291913566935));
#62335=CARTESIAN_POINT('Ctrl Pts',(-0.564113543125074,0.545349118398842,
-3.48711225035126));
#62336=CARTESIAN_POINT('Ctrl Pts',(-0.755795921696723,0.210718473850929,
-3.47130536503317));
#62337=CARTESIAN_POINT('Ctrl Pts',(-0.764898072237769,-0.174816159328638,
-3.45549847971508));
#62338=CARTESIAN_POINT('Ctrl Pts',(-0.589221156842832,-0.518119849845838,
-3.43969159439699));
#62339=CARTESIAN_POINT('Ctrl Pts',(-0.271204053986564,-0.736259540907092,
-3.42388470907889));
#62340=CARTESIAN_POINT('Ctrl Pts',(0.112328747748483,-0.776538474838649,
-3.40807782376081));
#62341=CARTESIAN_POINT('Ctrl Pts',(0.468725906395819,-0.629226330622686,
-3.39227093844271));
#62342=CARTESIAN_POINT('Ctrl Pts',(0.71189133089794,-0.329909811111817,
-3.37646405312462));
#62343=CARTESIAN_POINT('Ctrl Pts',(0.783082710823891,0.0491041595405024,
-3.36065716780653));
#62344=CARTESIAN_POINT('Ctrl Pts',(0.665102098940099,0.416255868980786,
-3.34485028248844));
#62345=CARTESIAN_POINT('Ctrl Pts',(0.386450478650352,0.682851212217119,
-3.32904339717034));
#62346=CARTESIAN_POINT('Ctrl Pts',(0.0144426831167398,0.784487832525058,
-3.31323651185225));
#62347=CARTESIAN_POINT('Ctrl Pts',(-0.36105408119949,0.696613020926732,
-3.29742962653416));
#62348=CARTESIAN_POINT('Ctrl Pts',(-0.649329765612568,0.4404549987967,-3.28162274121607));
#62349=CARTESIAN_POINT('Ctrl Pts',(-0.78074461859055,0.0778947431947184,
-3.26581585589798));
#62350=CARTESIAN_POINT('Ctrl Pts',(-0.723552300765176,-0.303482814229888,
-3.25000897057988));
#62351=CARTESIAN_POINT('Ctrl Pts',(-0.491568957646624,-0.611546981313525,
-3.2342020852618));
#62352=CARTESIAN_POINT('Ctrl Pts',(-0.14083560569182,-0.771877634502317,
-3.2183951999437));
#62353=CARTESIAN_POINT('Ctrl Pts',(0.243919889362559,-0.745743144821882,
-3.20258831462561));
#62354=CARTESIAN_POINT('Ctrl Pts',(0.569750815307017,-0.53945691109899,
-3.18678142930752));
#62355=CARTESIAN_POINT('Ctrl Pts',(0.757945071360682,-0.202852210427999,
-3.17097454398943));
#62356=CARTESIAN_POINT('Ctrl Pts',(0.763039921885615,0.182756198483848,
-3.15516765867133));
#62357=CARTESIAN_POINT('Ctrl Pts',(0.583804586265094,0.524215562084261,
-3.13936077335325));
#62358=CARTESIAN_POINT('Ctrl Pts',(0.26353756282294,0.739038363995279,-3.12355388803515));
#62359=CARTESIAN_POINT('Ctrl Pts',(-0.120393138780939,0.775329118897226,
-3.10774700271706));
#62360=CARTESIAN_POINT('Ctrl Pts',(-0.475240054536119,0.624320943938275,
-3.09194011739896));
#62361=CARTESIAN_POINT('Ctrl Pts',(-0.715281590908346,0.322493404867603,
-3.07613323208088));
#62362=CARTESIAN_POINT('Ctrl Pts',(-0.782530085898503,-0.057239978504147,
-3.06032634676278));
#62363=CARTESIAN_POINT('Ctrl Pts',(-0.6607400885885,-0.423145702811142,
-3.0445194614447));
#62364=CARTESIAN_POINT('Ctrl Pts',(-0.37933282876056,-0.686830659988315,
-3.0287125761266));
#62365=CARTESIAN_POINT('Ctrl Pts',(-0.00628882892598545,-0.784595565311336,
-3.01290569080852));
#62366=CARTESIAN_POINT('Ctrl Pts',(0.368274385006458,-0.692823013347268,
-2.99709880549042));
#62367=CARTESIAN_POINT('Ctrl Pts',(0.65387228533763,-0.433682816056642,
-2.98129192017233));
#62368=CARTESIAN_POINT('Ctrl Pts',(0.781512002073648,-0.0697763648401949,
-2.96548503485424));
#62369=CARTESIAN_POINT('Ctrl Pts',(0.720359168531101,0.310986203534265,
-2.94967814953614));
#62370=CARTESIAN_POINT('Ctrl Pts',(0.485186685664321,0.616622761929485,
-2.93387126421806));
#62371=CARTESIAN_POINT('Ctrl Pts',(0.132805981420619,0.773299632596821,
-2.91806437889996));
#62372=CARTESIAN_POINT('Ctrl Pts',(-0.251657121888123,0.743167843409859,
-2.90225749358187));
#62373=CARTESIAN_POINT('Ctrl Pts',(-0.575326546135049,0.533506434626413,
-2.88645060826377));
#62374=CARTESIAN_POINT('Ctrl Pts',(-0.760012351960777,0.194964036023375,
-2.87064372294569));
#62375=CARTESIAN_POINT('Ctrl Pts',(-0.761099352151827,-0.190676497318213,
-2.85483683762759));
#62376=CARTESIAN_POINT('Ctrl Pts',(-0.578324956322288,-0.530254651436739,
-2.8390299523095));
#62377=CARTESIAN_POINT('Ctrl Pts',(-0.255842605779168,-0.741737360218292,
-2.82322306699141));
#62378=CARTESIAN_POINT('Ctrl Pts',(0.128444525607754,-0.774036016162602,
-2.80741618167332));
#62379=CARTESIAN_POINT('Ctrl Pts',(0.481702869855816,-0.619348121534364,
-2.79160929635523));
#62380=CARTESIAN_POINT('Ctrl Pts',(0.718594590129734,-0.315042164656976,
-2.77580241103714));
#62381=CARTESIAN_POINT('Ctrl Pts',(0.781892936371006,0.0653696147196846,
-2.75999552571904));
#62382=CARTESIAN_POINT('Ctrl Pts',(0.656306708721413,0.429989830766658,
-2.74418864040095));
#62383=CARTESIAN_POINT('Ctrl Pts',(0.372174205421959,0.690735920083795,
-2.72838175508286));
#62384=CARTESIAN_POINT('Ctrl Pts',(-0.0018657045495305,0.784618550393763,
-2.71257486976477));
#62385=CARTESIAN_POINT('Ctrl Pts',(-0.375454909836976,0.688958170830988,
-2.69676798444668));
#62386=CARTESIAN_POINT('Ctrl Pts',(-0.658344177369592,0.426863789280643,
-2.68096109912859));
#62387=CARTESIAN_POINT('Ctrl Pts',(-0.782194970922462,0.0616504496259641,
-2.66515421381049));
#62388=CARTESIAN_POINT('Ctrl Pts',(-0.717088227055958,-0.318456001816918,
-2.6493473284924));
#62389=CARTESIAN_POINT('Ctrl Pts',(-0.478752006480955,-0.621631938341277,
-2.63354044317431));
#62390=CARTESIAN_POINT('Ctrl Pts',(-0.1247620121767,-0.774638103112089,
-2.61773355785622));
#62391=CARTESIAN_POINT('Ctrl Pts',(0.259367171793516,-0.740512269088977,
-2.60192667253812));
#62392=CARTESIAN_POINT('Ctrl Pts',(0.580840133349348,-0.527498331718864,
-2.58611978722004));
#62393=CARTESIAN_POINT('Ctrl Pts',(0.761997540200711,-0.187054802674346,
-2.57031290190194));
#62394=CARTESIAN_POINT('Ctrl Pts',(0.75907657264609,0.19857620032456,-2.55450601658385));
#62395=CARTESIAN_POINT('Ctrl Pts',(0.572782858893946,0.536236465594007,
-2.53869913126576));
#62396=CARTESIAN_POINT('Ctrl Pts',(0.248120014022245,0.744356238045383,
-2.52289224594767));
#62397=CARTESIAN_POINT('Ctrl Pts',(-0.136482038562351,0.772659306308634,
-2.50708536062958));
#62398=CARTESIAN_POINT('Ctrl Pts',(-0.488113654277092,0.614308400547915,
-2.49127847531148));
#62399=CARTESIAN_POINT('Ctrl Pts',(-0.721829970710122,0.307556895321985,
-2.47547158999339));
#62400=CARTESIAN_POINT('Ctrl Pts',(-0.781171331062794,-0.0734921900684592,
-2.4596647046753));
#62401=CARTESIAN_POINT('Ctrl Pts',(-0.651802438208183,-0.436787513582222,
-2.44385781935721));
#62402=CARTESIAN_POINT('Ctrl Pts',(-0.36497538186972,-0.694566570678812,
-2.42805093403912));
#62403=CARTESIAN_POINT('Ctrl Pts',(0.0100200365018897,-0.784556785289615,
-2.41224404872103));
#62404=CARTESIAN_POINT('Ctrl Pts',(0.382594880090186,-0.685018910836956,
-2.39643716340293));
#62405=CARTESIAN_POINT('Ctrl Pts',(0.662744958679239,-0.419998655022524,
-2.38063027808484));
#62406=CARTESIAN_POINT('Ctrl Pts',(0.782793451366445,-0.053517875268758,
-2.36482339276675));
#62407=CARTESIAN_POINT('Ctrl Pts',(0.713739829648883,0.325891402231261,
-2.34901650744866));
#62408=CARTESIAN_POINT('Ctrl Pts',(0.472265615135225,0.626573969485186,
-2.33320962213057));
#62409=CARTESIAN_POINT('Ctrl Pts',(0.116704566825439,0.775892901473883,
-2.31740273681247));
#62410=CARTESIAN_POINT('Ctrl Pts',(-0.267049206281493,0.737776708699793,
-2.30159585149439));
#62411=CARTESIAN_POINT('Ctrl Pts',(-0.586290981402503,0.521433251338619,
-2.28578896617629));
#62412=CARTESIAN_POINT('Ctrl Pts',(-0.763900421651359,0.179125364692859,
-2.2699820808582));
#62413=CARTESIAN_POINT('Ctrl Pts',(-0.756971801857933,-0.206454454220368,
-2.25417519554011));
#62414=CARTESIAN_POINT('Ctrl Pts',(-0.567178892606987,-0.542160358433354,
-2.23836831022202));
#62415=CARTESIAN_POINT('Ctrl Pts',(-0.240370621704116,-0.746894714599756,
-2.22256142490392));
#62416=CARTESIAN_POINT('Ctrl Pts',(0.144504809476721,-0.771199138039956,
-2.20675453958584));
#62417=CARTESIAN_POINT('Ctrl Pts',(0.494471715342225,-0.609202325341912,
-2.19094765426774));
#62418=CARTESIAN_POINT('Ctrl Pts',(0.724987383181469,-0.300038405380308,
-2.17514076894965));
#62419=CARTESIAN_POINT('Ctrl Pts',(0.780365347917708,0.0816068271944897,
-2.15933388363156));
#62420=CARTESIAN_POINT('Ctrl Pts',(0.647227763575373,0.44353801700947,-2.14352699831347));
#62421=CARTESIAN_POINT('Ctrl Pts',(0.357737135681229,0.698322198007528,
-2.12772011299538));
#62422=CARTESIAN_POINT('Ctrl Pts',(-0.0181732861449447,0.784410276670422,
-2.11191322767728));
#62423=CARTESIAN_POINT('Ctrl Pts',(-0.389693524545723,0.681005658862394,
-2.09610634235919));
#62424=CARTESIAN_POINT('Ctrl Pts',(-0.667074153918342,0.413088154816381,
-2.0802994570411));
#62425=CARTESIAN_POINT('Ctrl Pts',(-0.783307378761029,0.045379520204593,
-2.06449257172301));
#62426=CARTESIAN_POINT('Ctrl Pts',(-0.710314337985374,-0.333291601646179,
-2.04868568640492));
#62427=CARTESIAN_POINT('Ctrl Pts',(-0.4657282122515,-0.631448321550146,
-2.03287880108682));
#62428=CARTESIAN_POINT('Ctrl Pts',(-0.108634515687828,-0.777063892145778,
-2.01707191576873));
#62429=CARTESIAN_POINT('Ctrl Pts',(0.274702395580879,-0.734961457722512,
-2.00126503045064));
#62430=CARTESIAN_POINT('Ctrl Pts',(0.591678501523839,-0.515311848602358,
-1.98545814513255));
#62431=CARTESIAN_POINT('Ctrl Pts',(0.765720790773911,-0.171176578573269,
-1.96965125981446));
#62432=CARTESIAN_POINT('Ctrl Pts',(0.75478526713314,0.214310408039895,-1.95384437449637));
#62433=CARTESIAN_POINT('Ctrl Pts',(0.56151366277109,0.548025690088402,-1.93803748917828));
#62434=CARTESIAN_POINT('Ctrl Pts',(0.232595265871588,0.74935251568911,-1.92223060386018));
#62435=CARTESIAN_POINT('Ctrl Pts',(-0.152511971775213,0.769655669075926,
-1.90642371854209));
#62436=CARTESIAN_POINT('Ctrl Pts',(-0.500776366288377,0.604030447446553,
-1.890616833224));
#62437=CARTESIAN_POINT('Ctrl Pts',(-0.728066486497424,0.292487506937937,
-1.87480994790591));
#62438=CARTESIAN_POINT('Ctrl Pts',(-0.779475073993619,-0.0897126495992436,
-1.85900306258782));
#62439=CARTESIAN_POINT('Ctrl Pts',(-0.642583178954215,-0.450240611896095,
-1.84319617726972));
#62440=CARTESIAN_POINT('Ctrl Pts',(-0.350460248692089,-0.7020023964077,
-1.82738929195163));
#62441=CARTESIAN_POINT('Ctrl Pts',(0.0263245728094266,-0.784179040361239,
-1.81158240663354));
#62442=CARTESIAN_POINT('Ctrl Pts',(0.396750076446984,-0.676918848396753,
-1.79577552131545));
#62443=CARTESIAN_POINT('Ctrl Pts',(0.671331295471004,-0.406133035096502,
-1.77996863599736));
#62444=CARTESIAN_POINT('Ctrl Pts',(0.7837366975946,-0.0372362634938868,
-1.76416175067927));
#62445=CARTESIAN_POINT('Ctrl Pts',(0.706812122068224,0.340655800732772,
-1.74835486536117));
#62446=CARTESIAN_POINT('Ctrl Pts',(0.459140503964136,0.63625446803542,-1.73254798004308));
#62447=CARTESIAN_POINT('Ctrl Pts',(0.100552730446469,0.778150948643792,
-1.71674109472499));
#62448=CARTESIAN_POINT('Ctrl Pts',(-0.2823259130362,0.732066820245085,-1.7009342094069));
#62449=CARTESIAN_POINT('Ctrl Pts',(-0.597002111783026,0.509134784710377,
-1.6851273240888));
#62450=CARTESIAN_POINT('Ctrl Pts',(-0.767458450942094,0.163209302899789,
-1.66932043877072));
#62451=CARTESIAN_POINT('Ctrl Pts',(-0.752517204649186,-0.222143213226177,
-1.65351355345262));
#62452=CARTESIAN_POINT('Ctrl Pts',(-0.555787781313246,-0.553831827018249,
-1.63770666813453));
#62453=CARTESIAN_POINT('Ctrl Pts',(-0.224794786375882,-0.751729375835276,
-1.62189978281644));
#62454=CARTESIAN_POINT('Ctrl Pts',(0.160502660568133,-0.768029066133584,
-1.60609289749835));
#62455=CARTESIAN_POINT('Ctrl Pts',(0.50702692612178,-0.598793325499686,
-1.59028601218026));
#62456=CARTESIAN_POINT('Ctrl Pts',(0.731066948070155,-0.284905015601451,
-1.57447912686216));
#62457=CARTESIAN_POINT('Ctrl Pts',(0.778500605453029,0.0978087817363028,
-1.55867224154408));
#62458=CARTESIAN_POINT('Ctrl Pts',(0.637869186027226,0.456894574264609,
-1.54286535622598));
#62459=CARTESIAN_POINT('Ctrl Pts',(0.343145506911666,0.705606768364512,
-1.52705847090789));
#62460=CARTESIAN_POINT('Ctrl Pts',(-0.0344730160381407,0.783863101338944,
-1.5112515855898));
#62461=CARTESIAN_POINT('Ctrl Pts',(-0.403763773584001,0.67275892087484,
-1.49544470027171));
#62462=CARTESIAN_POINT('Ctrl Pts',(-0.675515923504185,0.399134047116708,
-1.47963781495362));
#62463=CARTESIAN_POINT('Ctrl Pts',(-0.784081361494491,0.0290889847265052,
-1.46383092963552));
#62464=CARTESIAN_POINT('Ctrl Pts',(-0.703233560187567,-0.347983204050704,
-1.44802404431743));
#62465=CARTESIAN_POINT('Ctrl Pts',(-0.452503201841199,-0.640991889807458,
-1.43221715899934));
#62466=CARTESIAN_POINT('Ctrl Pts',(-0.0924600840514184,-0.779153953550054,
-1.41641027368125));
#62467=CARTESIAN_POINT('Ctrl Pts',(0.289918935196972,-0.729093108930353,
-1.40060338836316));
#62468=CARTESIAN_POINT('Ctrl Pts',(0.602261237152921,-0.502902726875197,
-1.38479650304507));
#62469=CARTESIAN_POINT('Ctrl Pts',(0.769113214463401,-0.155224398253779,
-1.36898961772697));
#62470=CARTESIAN_POINT('Ctrl Pts',(0.750167859389718,0.229952023722606,
-1.35318273240888));
#62471=CARTESIAN_POINT('Ctrl Pts',(0.550001866711737,0.559578142075867,
-1.33737584709079));
#62472=CARTESIAN_POINT('Ctrl Pts',(0.216970025781956,0.754025038302873,
-1.3215689617727));
#62473=CARTESIAN_POINT('Ctrl Pts',(-0.168476012745165,0.766319504909646,
-1.30576207645461));
#62474=CARTESIAN_POINT('Ctrl Pts',(-0.513222719691291,0.593491525186458,
-1.28995519113651));
#62475=CARTESIAN_POINT('Ctrl Pts',(-0.733988443806282,0.277291750389919,
-1.27414830581842));
#62476=CARTESIAN_POINT('Ctrl Pts',(-0.77744204755268,-0.105894349105939,
-1.25834142050033));
#62477=CARTESIAN_POINT('Ctrl Pts',(-0.633086293974033,-0.463499185390545,
-1.24253453518224));
#62478=CARTESIAN_POINT('Ctrl Pts',(-0.335793700438192,-0.709134924553501,
-1.22672764986415));
#62479=CARTESIAN_POINT('Ctrl Pts',(0.0426177356809889,-0.783462493729533,
-1.21092076454606));
#62480=CARTESIAN_POINT('Ctrl Pts',(0.410733858375728,-0.668526325629188,
-1.19511387922796));
#62481=CARTESIAN_POINT('Ctrl Pts',(0.67962758601734,-0.392091946869246,
-1.17930699390987));
#62482=CARTESIAN_POINT('Ctrl Pts',(0.784341333232005,-0.0209385639267508,
-1.16350010859178));
#62483=CARTESIAN_POINT('Ctrl Pts',(0.699579038879999,0.355273020134108,
-1.14769322327369));
#62484=CARTESIAN_POINT('Ctrl Pts',(0.445817022807615,0.645660075155983,
-1.1318863379556));
#62485=CARTESIAN_POINT('Ctrl Pts',(0.0843574506258922,0.78007279852548,
-1.1160794526375));
#62486=CARTESIAN_POINT('Ctrl Pts',(-0.297480641906641,0.726040644982282,
-1.10027256731942));
#62487=CARTESIAN_POINT('Ctrl Pts',(-0.607455309571685,0.496616348249473,
-1.08446568200132));
#62488=CARTESIAN_POINT('Ctrl Pts',(-0.770684902599366,0.147222727120785,
-1.06865879668323));
#62489=CARTESIAN_POINT('Ctrl Pts',(-0.747737485118111,-0.237735996064363,
-1.05285191136514));
#62490=CARTESIAN_POINT('Ctrl Pts',(-0.544156543929278,-0.56526401457586,
-1.03704502604705));
#62491=CARTESIAN_POINT('Ctrl Pts',(-0.209121829277477,-0.75623925512705,
-1.02123814072896));
#62492=CARTESIAN_POINT('Ctrl Pts',(0.176431167068596,-0.764527170061526,
-1.00543125541086));
#62493=CARTESIAN_POINT('Ctrl Pts',(0.519363077761318,-0.58812561917822,
-0.989624370092773));
#62494=CARTESIAN_POINT('Ctrl Pts',(0.736830658141882,-0.269648533646439,
-0.973817484774679));
#62495=CARTESIAN_POINT('Ctrl Pts',(0.77629951463218,0.113968478349572,-0.95801059945659));
#62496=CARTESIAN_POINT('Ctrl Pts',(0.628235019416367,0.470053731880079,
-0.942203714138496));
#62497=CARTESIAN_POINT('Ctrl Pts',(0.328405623373425,0.712586483882614,
-0.926396828820405));
#62498=CARTESIAN_POINT('Ctrl Pts',(-0.0507578519900923,0.782977260804441,
-0.910589943502312));
#62499=CARTESIAN_POINT('Ctrl Pts',(-0.417659577951879,0.664221519841486,
-0.894783058184222));
#62500=CARTESIAN_POINT('Ctrl Pts',(-0.683665838891269,0.385007495003111,
-0.87897617286613));
#62501=CARTESIAN_POINT('Ctrl Pts',(-0.78451658472642,0.0127858814583185,
-0.863169287548038));
#62502=CARTESIAN_POINT('Ctrl Pts',(-0.695848952886841,-0.362524461577092,
-0.847362402229947));
#62503=CARTESIAN_POINT('Ctrl Pts',(-0.439082689067719,-0.650258519849247,
-0.831555516911854));
#62504=CARTESIAN_POINT('Ctrl Pts',(-0.0762457053718529,-0.780907384321486,
-0.815748631593763));
#62505=CARTESIAN_POINT('Ctrl Pts',(0.305010216391177,-0.722909758111259,
-0.799941746275672));
#62506=CARTESIAN_POINT('Ctrl Pts',(0.612583768004145,-0.490276327853303,
-0.784134860957579));
#62507=CARTESIAN_POINT('Ctrl Pts',(0.772173345584864,-0.139205153797376,
-0.768327975639488));
#62508=CARTESIAN_POINT('Ctrl Pts',(0.745226344350049,0.245494289469506,
-0.752521090321395));
#62509=CARTESIAN_POINT('Ctrl Pts',(0.538252444345531,0.570888830361512,
-0.736714205003304));
#62510=CARTESIAN_POINT('Ctrl Pts',(0.201251044581531,0.758371787140263,
-0.720907319685213));
#62511=CARTESIAN_POINT('Ctrl Pts',(-0.184367264266346,0.762652255187394,
-0.705100434367121));
#62512=CARTESIAN_POINT('Ctrl Pts',(-0.525447337084102,0.582696187070671,
-0.689293549049029));
#62513=CARTESIAN_POINT('Ctrl Pts',(-0.739593284076573,0.261976190949299,
-0.673486663730938));
#62514=CARTESIAN_POINT('Ctrl Pts',(-0.775073130101659,-0.122030297344106,
-0.657679778412846));
#62515=CARTESIAN_POINT('Ctrl Pts',(-0.623315886362265,-0.476557505747101,
-0.641872893094754));
#62516=CARTESIAN_POINT('Ctrl Pts',(-0.320982073736872,-0.715961073533367,
-0.626066007776662));
#62517=CARTESIAN_POINT('Ctrl Pts',(0.0588924857147926,-0.782407454975863,
-0.610259122458571));
#62518=CARTESIAN_POINT('Ctrl Pts',(0.424540184234268,-0.659844968493212,
-0.594452237140478));
#62519=CARTESIAN_POINT('Ctrl Pts',(0.687630245936072,-0.377881456741887,
-0.578645351822387));
#62520=CARTESIAN_POINT('Ctrl Pts',(0.784607097048036,-0.00463181792919246,
-0.562838466504295));
#62521=CARTESIAN_POINT('Ctrl Pts',(0.692043705111493,0.369736745118777,
-0.547031581186203));
#62522=CARTESIAN_POINT('Ctrl Pts',(0.432300928027253,0.654786727188522,
-0.531224695868112));
#62523=CARTESIAN_POINT('Ctrl Pts',(0.0681257244754544,0.781657620790691,
-0.51541781055002));
#62524=CARTESIAN_POINT('Ctrl Pts',(-0.312506845347284,0.719700786498495,
-0.499610925231929));
#62525=CARTESIAN_POINT('Ctrl Pts',(-0.617646058502423,0.483883350500862,
-0.483804039913837));
#62526=CARTESIAN_POINT('Ctrl Pts',(-0.773578382646387,0.131172544297797,
-0.467997154595745));
#62527=CARTESIAN_POINT('Ctrl Pts',(-0.74263470832531,-0.253226065929806,
-0.452190269277653));
#62528=CARTESIAN_POINT('Ctrl Pts',(-0.532290205688612,-0.576451981871085,
-0.436383383959562));
#62529=CARTESIAN_POINT('Ctrl Pts',(-0.193358521853627,-0.760422403998173,
-0.42057649864147));
#62530=CARTESIAN_POINT('Ctrl Pts',(0.19228344712591,-0.760694962805148,
-0.404769613323378));
#62531=CARTESIAN_POINT('Ctrl Pts',(0.531474840469156,-0.577203815321457,
-0.388962728005286));
#62532=CARTESIAN_POINT('Ctrl Pts',(0.742276023211007,-0.254275551022411,
-0.373155842687195));
#62533=CARTESIAN_POINT('Ctrl Pts',(0.773763026419959,0.130078935295337,
-0.357348957369103));
#62534=CARTESIAN_POINT('Ctrl Pts',(0.618329426166053,0.48300980449125,-0.341542072051011));
#62535=CARTESIAN_POINT('Ctrl Pts',(0.313523853347105,0.719258328998049,
-0.32573518673292));
#62536=CARTESIAN_POINT('Ctrl Pts',(-0.0670207581330449,0.781753137797108,
-0.309928301414828));
#62537=CARTESIAN_POINT('Ctrl Pts',(-0.431374934142047,0.655397144303641,
-0.294121416096737));
#62538=CARTESIAN_POINT('Ctrl Pts',(-0.691520378694679,0.370714601824122,
-0.278314530778645));
#62539=CARTESIAN_POINT('Ctrl Pts',(-0.784612860896982,-0.00352274594854401,
-0.262507645460553));
#62540=CARTESIAN_POINT('Ctrl Pts',(-0.688163705642762,-0.376909091639667,
-0.246700760142461));
#62541=CARTESIAN_POINT('Ctrl Pts',(-0.425472474041242,-0.659244208234394,
-0.230893874824369));
#62542=CARTESIAN_POINT('Ctrl Pts',(-0.0599983814376782,-0.782323426558676,
-0.215086989506278));
#62543=CARTESIAN_POINT('Ctrl Pts',(0.319969712033551,-0.716414077421034,
-0.199280104188185));
#62544=CARTESIAN_POINT('Ctrl Pts',(0.622641647960042,-0.477438105431615,
-0.183473218870094));
#62545=CARTESIAN_POINT('Ctrl Pts',(0.774899835216333,-0.123125768794702,
-0.167666333552002));
#62546=CARTESIAN_POINT('Ctrl Pts',(0.739962909438748,0.260930495261506,
-0.151859448233911));
#62547=CARTESIAN_POINT('Ctrl Pts',(0.526270369288404,0.581952858495042,
-0.136052562915819));
#62548=CARTESIAN_POINT('Ctrl Pts',(0.185445314567899,0.762390903206315,
-0.120245677597727));
#62549=CARTESIAN_POINT('Ctrl Pts',(-0.200179253927746,0.758655467139329,
-0.104438792279636));
#62550=CARTESIAN_POINT('Ctrl Pts',(-0.53744416698625,0.57164916997901,-0.0886319069615434));
#62551=CARTESIAN_POINT('Ctrl Pts',(-0.744880092625389,0.246547303176403,
-0.0728250216434516));
#62552=CARTESIAN_POINT('Ctrl Pts',(-0.772366395559619,-0.138113244016823,
-0.0570181363253598));
#62553=CARTESIAN_POINT('Ctrl Pts',(-0.613281953089182,-0.489410476528923,
-0.0412112510072682));
#62554=CARTESIAN_POINT('Ctrl Pts',(-0.306020434541259,-0.722476830566009,
-0.0254043656891769));
#62555=CARTESIAN_POINT('Ctrl Pts',(0.0751192972481202,-0.781016420057536,
-0.00959748037108558));
#62556=CARTESIAN_POINT('Ctrl Pts',(0.438210481399638,-0.650874980768236,
0.00620940494700578));
#62557=CARTESIAN_POINT('Ctrl Pts',(0.609540070766957,-0.459297668798489,
0.0167473284924006));
#62558=CARTESIAN_POINT('Ctrl Pts',(0.667283755215036,-0.34884264523884,
0.022016290265098));
#62559=CARTESIAN_POINT('Ctrl Pts',(0.415028236876535,-0.582012248186926,
-3.9709162902651));
#62560=CARTESIAN_POINT('Ctrl Pts',(0.511368326205958,-0.513312908027891,
-3.9656473284924));
#62561=CARTESIAN_POINT('Ctrl Pts',(0.669185292538236,-0.327226217723212,
-3.95510940494702));
#62562=CARTESIAN_POINT('Ctrl Pts',(0.744231488665138,0.0311768949505003,
-3.93930251962891));
#62563=CARTESIAN_POINT('Ctrl Pts',(0.639496219859735,0.381955009880642,
-3.92349563431083));
#62564=CARTESIAN_POINT('Ctrl Pts',(0.380273549786177,0.640508840670193,
-3.90768874899273));
#62565=CARTESIAN_POINT('Ctrl Pts',(0.0291879083315599,0.744309459692835,
-3.89188186367465));
#62566=CARTESIAN_POINT('Ctrl Pts',(-0.328949274496042,0.668316554050527,
-3.87607497835654));
#62567=CARTESIAN_POINT('Ctrl Pts',(-0.607620782246216,0.430870045176653,
-3.86026809303846));
#62568=CARTESIAN_POINT('Ctrl Pts',(-0.739507376440356,0.089339873180574,
-3.84446120772036));
#62569=CARTESIAN_POINT('Ctrl Pts',(-0.692748553758454,-0.273774024033415,
-3.82865432240228));
#62570=CARTESIAN_POINT('Ctrl Pts',(-0.478640108418349,-0.570750576610951,
-3.81284743708418));
#62571=CARTESIAN_POINT('Ctrl Pts',(-0.148904902961183,-0.729849356962288,
-3.7970405517661));
#62572=CARTESIAN_POINT('Ctrl Pts',(0.216801764382258,-0.712635699191136,
-3.78123366644799));
#62573=CARTESIAN_POINT('Ctrl Pts',(0.530134886310931,-0.523268285155012,
-3.76542678112992));
#62574=CARTESIAN_POINT('Ctrl Pts',(0.715401492578031,-0.20749309124257,
-3.74961989581181));
#62575=CARTESIAN_POINT('Ctrl Pts',(0.727846093628893,0.158406896325021,
-3.73381301049373));
#62576=CARTESIAN_POINT('Ctrl Pts',(0.564462402406145,0.48603999789451,-3.71800612517562));
#62577=CARTESIAN_POINT('Ctrl Pts',(0.26471958176019,0.696258733153591,-3.70219923985755));
#62578=CARTESIAN_POINT('Ctrl Pts',(-0.0989724616031902,0.73827984815802,
-3.68639235453945));
#62579=CARTESIAN_POINT('Ctrl Pts',(-0.438755385913872,0.60195215152099,
-3.67058546922136));
#62580=CARTESIAN_POINT('Ctrl Pts',(-0.672546658142441,0.320208798101702,
-3.65477858390326));
#62581=CARTESIAN_POINT('Ctrl Pts',(-0.743868514095672,-0.0388884997822909,
-3.63897169858518));
#62582=CARTESIAN_POINT('Ctrl Pts',(-0.635491487028924,-0.388591368366378,
-3.62316481326708));
#62583=CARTESIAN_POINT('Ctrl Pts',(-0.373596589215961,-0.644420879723414,
-3.60735792794899));
#62584=CARTESIAN_POINT('Ctrl Pts',(-0.0214506745740397,-0.74457541607666,
-3.5915510426309));
#62585=CARTESIAN_POINT('Ctrl Pts',(0.335877153523394,-0.66486030068283,
-3.57574415731281));
#62586=CARTESIAN_POINT('Ctrl Pts',(0.612065978987051,-0.424532588904725,
-3.55993727199472));
#62587=CARTESIAN_POINT('Ctrl Pts',(0.7403959144979,-0.0816490751478253,
-3.54413038667662));
#62588=CARTESIAN_POINT('Ctrl Pts',(0.689865854841492,0.280958687357274,
-3.52832350135853));
#62589=CARTESIAN_POINT('Ctrl Pts',(0.472682520840011,0.575694290547901,
-3.51251661604043));
#62590=CARTESIAN_POINT('Ctrl Pts',(0.141311639693069,0.731357438032112,
-3.49670973072235));
#62591=CARTESIAN_POINT('Ctrl Pts',(-0.224196381729249,0.71034404628802,
-3.48090284540425));
#62592=CARTESIAN_POINT('Ctrl Pts',(-0.535544509819703,0.51773039284887,
-3.46509596008617));
#62593=CARTESIAN_POINT('Ctrl Pts',(-0.71751930323548,0.200046822423883,
-3.44928907476807));
#62594=CARTESIAN_POINT('Ctrl Pts',(-0.726160483383015,-0.16596274898414,
-3.43348218944998));
#62595=CARTESIAN_POINT('Ctrl Pts',(-0.559380570565075,-0.491880126607821,
-3.41767530413189));
#62596=CARTESIAN_POINT('Ctrl Pts',(-0.257469163652299,-0.69897232523585,
-3.4018684188138));
#62597=CARTESIAN_POINT('Ctrl Pts',(0.106639957300735,-0.737211368051477,
-3.38606153349571));
#62598=CARTESIAN_POINT('Ctrl Pts',(0.444987695898818,-0.597359717570652,
-3.37025464817761));
#62599=CARTESIAN_POINT('Ctrl Pts',(0.675838221749806,-0.313201819438347,
-3.35444776285952));
#62600=CARTESIAN_POINT('Ctrl Pts',(0.743424176971904,0.0466173226502346,
-3.33864087754143));
#62601=CARTESIAN_POINT('Ctrl Pts',(0.631418589214678,0.395174957293065,
-3.32283399222334));
#62602=CARTESIAN_POINT('Ctrl Pts',(0.366879034691962,0.64826881428997,-3.30702710690524));
#62603=CARTESIAN_POINT('Ctrl Pts',(0.013711246156908,0.744758137522683,
-3.29122022158716));
#62604=CARTESIAN_POINT('Ctrl Pts',(-0.342768815411179,0.661333668324127,
-3.27541333626906));
#62605=CARTESIAN_POINT('Ctrl Pts',(-0.616445031810243,0.418148543503261,
-3.25960645095098));
#62606=CARTESIAN_POINT('Ctrl Pts',(-0.741204495359439,0.0739498325649935,
-3.24379956563288));
#62607=CARTESIAN_POINT('Ctrl Pts',(-0.686908632073539,-0.288113194526541,
-3.22799268031479));
#62608=CARTESIAN_POINT('Ctrl Pts',(-0.466673880947885,-0.58057572332855,
-3.2121857949967));
#62609=CARTESIAN_POINT('Ctrl Pts',(-0.133703110543229,-0.732786571866935,
-3.1963789096786));
#62610=CARTESIAN_POINT('Ctrl Pts',(0.231566781503394,-0.707975640387146,
-3.18057202436052));
#62611=CARTESIAN_POINT('Ctrl Pts',(0.54089628731945,-0.512136591195616,
-3.16476513904242));
#62612=CARTESIAN_POINT('Ctrl Pts',(0.719559611108497,-0.192578938980405,
-3.14895825372433));
#62613=CARTESIAN_POINT('Ctrl Pts',(0.72439643741808,0.173500671852947,-3.13315136840623));
#62614=CARTESIAN_POINT('Ctrl Pts',(0.554238317431266,0.497667126871354,
-3.11734448308815));
#62615=CARTESIAN_POINT('Ctrl Pts',(0.250190935178089,0.701610417277384,
-3.10153759777005));
#62616=CARTESIAN_POINT('Ctrl Pts',(-0.114295934355541,0.736063258876045,
-3.08573071245196));
#62617=CARTESIAN_POINT('Ctrl Pts',(-0.451171940746698,0.592702759872339,
-3.06992382713387));
#62618=CARTESIAN_POINT('Ctrl Pts',(-0.679056785029417,0.306161010553175,
-3.05411694181578));
#62619=CARTESIAN_POINT('Ctrl Pts',(-0.7428995392489,-0.0543411102315957,
-3.03831005649768));
#62620=CARTESIAN_POINT('Ctrl Pts',(-0.627277489033615,-0.401715861560274,
-3.0225031711796));
#62621=CARTESIAN_POINT('Ctrl Pts',(-0.3601218519089,-0.652046726435409,
-3.0066962858615));
#62622=CARTESIAN_POINT('Ctrl Pts',(-0.00597033672662238,-0.744860414276931,
-2.99088940054342));
#62623=CARTESIAN_POINT('Ctrl Pts',(0.34962345329424,-0.657735602338842,
-2.97508251522532));
#62624=CARTESIAN_POINT('Ctrl Pts',(0.620757499626612,-0.411719331990554,
-2.95927562990723));
#62625=CARTESIAN_POINT('Ctrl Pts',(0.741933015382239,-0.0662426023284734,
-2.94346874458914));
#62626=CARTESIAN_POINT('Ctrl Pts',(0.68387721320773,0.295236581291443,-2.92766185927104));
#62627=CARTESIAN_POINT('Ctrl Pts',(0.460614833506189,0.585394445507896,
-2.91185497395296));
#62628=CARTESIAN_POINT('Ctrl Pts',(0.12608013951769,0.734136554120982,-2.89604808863486));
#62629=CARTESIAN_POINT('Ctrl Pts',(-0.238912168705604,0.705530762845827,
-2.88024120331678));
#62630=CARTESIAN_POINT('Ctrl Pts',(-0.546189640172924,0.506487471360546,
-2.86443431799868));
#62631=CARTESIAN_POINT('Ctrl Pts',(-0.721522196104249,0.185090254217592,
-2.84862743268059));
#62632=CARTESIAN_POINT('Ctrl Pts',(-0.722554146128466,-0.181019854132062,
-2.83282054736249));
#62633=CARTESIAN_POINT('Ctrl Pts',(-0.549036198518368,-0.503400371865109,
-2.81701366204441));
#62634=CARTESIAN_POINT('Ctrl Pts',(-0.242885682453148,-0.704172725214985,
-2.80120677672631));
#62635=CARTESIAN_POINT('Ctrl Pts',(0.121939565791243,-0.73483564418996,
-2.78539989140822));
#62636=CARTESIAN_POINT('Ctrl Pts',(0.457307452479438,-0.587981781677116,
-2.76959300609013));
#62637=CARTESIAN_POINT('Ctrl Pts',(0.682202000324592,-0.299087131837123,
-2.75378612077204));
#62638=CARTESIAN_POINT('Ctrl Pts',(0.742294657597777,0.0620590281846798,
-2.73797923545394));
#62639=CARTESIAN_POINT('Ctrl Pts',(0.623068633783288,0.408213374686398,
-2.72217235013586));
#62640=CARTESIAN_POINT('Ctrl Pts',(0.353325770741238,0.655754208074595,
-2.70636546481776));
#62641=CARTESIAN_POINT('Ctrl Pts',(-0.00177121758664689,0.744882235300112,
-2.69055857949967));
#62642=CARTESIAN_POINT('Ctrl Pts',(-0.356440326772058,0.654066491366174,
-2.67475169418158));
#62643=CARTESIAN_POINT('Ctrl Pts',(-0.625002916627162,0.405245648816827,
-2.65894480886349));
#62644=CARTESIAN_POINT('Ctrl Pts',(-0.742581395875524,0.0585282169298649,
-2.64313792354539));
#62645=CARTESIAN_POINT('Ctrl Pts',(-0.680771925681304,-0.302328078222316,
-2.62733103822731));
#62646=CARTESIAN_POINT('Ctrl Pts',(-0.454506032979947,-0.590149936594305,
-2.61152415290921));
#62647=CARTESIAN_POINT('Ctrl Pts',(-0.118443550007935,-0.735407238976439,
-2.59571726759112));
#62648=CARTESIAN_POINT('Ctrl Pts',(0.246231749927488,-0.703009677746384,
-2.57991038227302));
#62649=CARTESIAN_POINT('Ctrl Pts',(0.551423996621224,-0.500783643530524,
-2.56410349695494));
#62650=CARTESIAN_POINT('Ctrl Pts',(0.723406846235083,-0.177581577022058,
-2.54829661163684));
#62651=CARTESIAN_POINT('Ctrl Pts',(0.720633808508361,0.188519483640722,
-2.53248972631875));
#62652=CARTESIAN_POINT('Ctrl Pts',(0.543774775730693,0.509079242315443,
-2.51668284100066));
#62653=CARTESIAN_POINT('Ctrl Pts',(0.235554194550753,0.706658972282229,
-2.50087595568257));
#62654=CARTESIAN_POINT('Ctrl Pts',(-0.129570025984758,0.733528656593414,
-2.48506907036448));
#62655=CARTESIAN_POINT('Ctrl Pts',(-0.463393568372761,0.583197292919119,
-2.46926218504639));
#62656=CARTESIAN_POINT('Ctrl Pts',(-0.685273527906441,0.291980947371725,
-2.4534552997283));
#62657=CARTESIAN_POINT('Ctrl Pts',(-0.741609597354536,-0.0697702428623754,
-2.4376484144102));
#62658=CARTESIAN_POINT('Ctrl Pts',(-0.618792478081121,-0.414666794845758,
-2.42184152909211));
#62659=CARTESIAN_POINT('Ctrl Pts',(-0.346491525264335,-0.659390858745725,
-2.40603464377402));
#62660=CARTESIAN_POINT('Ctrl Pts',(0.00951258058272212,-0.744823598235237,
-2.39022775845593));
#62661=CARTESIAN_POINT('Ctrl Pts',(0.363218699523402,-0.650326731723339,
-2.37442087313784));
#62662=CARTESIAN_POINT('Ctrl Pts',(0.629180824245266,-0.398728193233784,
-2.35861398781975));
#62663=CARTESIAN_POINT('Ctrl Pts',(0.743149566804792,-0.0508075096347088,
-2.34280710250165));
#62664=CARTESIAN_POINT('Ctrl Pts',(0.677593104910366,0.309386919334609,
-2.32700021718356));
#62665=CARTESIAN_POINT('Ctrl Pts',(0.448348139208236,0.594841682925754,
-2.31119333186547));
#62666=CARTESIAN_POINT('Ctrl Pts',(0.11079416687642,0.736598489180904,-2.29538644654737));
#62667=CARTESIAN_POINT('Ctrl Pts',(-0.253524734548086,0.700412657402587,
-2.27957956122929));
#62668=CARTESIAN_POINT('Ctrl Pts',(-0.55659879127791,0.495025723801701,
-2.26377267591119));
#62669=CARTESIAN_POINT('Ctrl Pts',(-0.725213357931446,0.170053718439873,
-2.24796579059311));
#62670=CARTESIAN_POINT('Ctrl Pts',(-0.718635631982085,-0.195998750310146,
-2.23215890527501));
#62671=CARTESIAN_POINT('Ctrl Pts',(-0.538454617378229,-0.514703124821964,
-2.21635201995692));
#62672=CARTESIAN_POINT('Ctrl Pts',(-0.228197263377957,-0.709068889928362,
-2.20054513463883));
#62673=CARTESIAN_POINT('Ctrl Pts',(0.137186490735684,-0.732142437260031,
-2.18473824932073));
#62674=CARTESIAN_POINT('Ctrl Pts',(0.469429631037854,-0.578349810392547,
-2.16893136400265));
#62675=CARTESIAN_POINT('Ctrl Pts',(0.68827103600543,-0.284843224727992,
-2.15312447868455));
#62676=CARTESIAN_POINT('Ctrl Pts',(0.740844432515615,0.0774739213416226,
-2.13731759336646));
#62677=CARTESIAN_POINT('Ctrl Pts',(0.614449483813974,0.421075424975349,
-2.12151070804837));
#62678=CARTESIAN_POINT('Ctrl Pts',(0.339619853675854,0.662956285637765,
-2.10570382273028));
#62679=CARTESIAN_POINT('Ctrl Pts',(-0.0172529160820942,0.744684509415964,
-2.08989693741218));
#62680=CARTESIAN_POINT('Ctrl Pts',(-0.369957839385679,0.646516727358626,
-2.07409005209409));
#62681=CARTESIAN_POINT('Ctrl Pts',(-0.633290771206291,0.392167669221179,
-2.058283166776));
#62682=CARTESIAN_POINT('Ctrl Pts',(-0.743637466799339,0.0430813143914036,
-2.04247628145791));
#62683=CARTESIAN_POINT('Ctrl Pts',(-0.674341094253676,-0.316412342171074,
-2.02666939613982));
#62684=CARTESIAN_POINT('Ctrl Pts',(-0.44214181733292,-0.599469177725571,
-2.01086251082173));
#62685=CARTESIAN_POINT('Ctrl Pts',(-0.103132816367497,-0.737710176062076,
-1.99505562550363));
#62686=CARTESIAN_POINT('Ctrl Pts',(0.26079033481925,-0.697739982330304,
-1.97924874018554));
#62687=CARTESIAN_POINT('Ctrl Pts',(0.561713465190083,-0.489214334112953,
-1.96344185486745));
#62688=CARTESIAN_POINT('Ctrl Pts',(0.72694153606386,-0.162507491588989,
-1.94763496954936));
#62689=CARTESIAN_POINT('Ctrl Pts',(0.716559832381698,0.203456846271001,
-1.93182808423127));
#62690=CARTESIAN_POINT('Ctrl Pts',(0.533076298115275,0.520271411923761,
-1.91602119891318));
#62691=CARTESIAN_POINT('Ctrl Pts',(0.220815683590071,0.711402217847316,
-1.90021431359509));
#62692=CARTESIAN_POINT('Ctrl Pts',(-0.14478813735533,0.730677135921608,
-1.88440742827699));
#62693=CARTESIAN_POINT('Ctrl Pts',(-0.475414988492377,0.573439857695838,
-1.8686005429589));
#62694=CARTESIAN_POINT('Ctrl Pts',(-0.691194200847195,0.277674734883526,
-1.85279365764081));
#62695=CARTESIAN_POINT('Ctrl Pts',(-0.739999245729919,-0.0851692315133856,
-1.83698677232272));
#62696=CARTESIAN_POINT('Ctrl Pts',(-0.610040120088232,-0.42743857285014,
-1.82117988700463));
#62697=CARTESIAN_POINT('Ctrl Pts',(-0.332711498216024,-0.666450103632882,
-1.80537300168654));
#62698=CARTESIAN_POINT('Ctrl Pts',(0.0249913880162134,-0.744464983865897,
-1.78956611636844));
#62699=CARTESIAN_POINT('Ctrl Pts',(0.376657018434001,-0.642636889807798,
-1.77375923105035));
#62700=CARTESIAN_POINT('Ctrl Pts',(0.63733231357633,-0.385564785410793,
-1.75795234573226));
#62701=CARTESIAN_POINT('Ctrl Pts',(0.744045043158892,-0.0353504657411277,
-1.74214546041417));
#62702=CARTESIAN_POINT('Ctrl Pts',(0.671016244975565,0.323403587884121,
-1.72633857509608));
#62703=CARTESIAN_POINT('Ctrl Pts',(0.435887737726806,0.604031921157183,
-1.71053168977799));
#62704=CARTESIAN_POINT('Ctrl Pts',(0.0954603260181704,0.738742179541641,
-1.69472480445989));
#62705=CARTESIAN_POINT('Ctrl Pts',(-0.268027765950747,0.694991941217221,
-1.6789179191418));
#62706=CARTESIAN_POINT('Ctrl Pts',(-0.566767465898757,0.48335010217867,
-1.6631110338237));
#62707=CARTESIAN_POINT('Ctrl Pts',(-0.72859119396402,0.15494371157138,-1.64730414850562));
#62708=CARTESIAN_POINT('Ctrl Pts',(-0.714406633923669,-0.210892965940744,
-1.63149726318752));
#62709=CARTESIAN_POINT('Ctrl Pts',(-0.527640398878327,-0.525783502165053,
-1.61569037786944));
#62710=CARTESIAN_POINT('Ctrl Pts',(-0.21341025250479,-0.713658704005824,
-1.59988349255134));
#62711=CARTESIAN_POINT('Ctrl Pts',(0.152374144755576,-0.729132910851949,
-1.58407660723325));
#62712=CARTESIAN_POINT('Ctrl Pts',(0.481348994230894,-0.568467965175117,
-1.56826972191516));
#62713=CARTESIAN_POINT('Ctrl Pts',(0.694042706687525,-0.270476252139228,
-1.55246283659707));
#62714=CARTESIAN_POINT('Ctrl Pts',(0.739074128289886,0.0928553421725219,
-1.53665595127898));
#62715=CARTESIAN_POINT('Ctrl Pts',(0.605564863179149,0.433755551157848,
-1.52084906596088));
#62716=CARTESIAN_POINT('Ctrl Pts',(0.325767205087459,0.669871935348046,
-1.50504218064279));
#62717=CARTESIAN_POINT('Ctrl Pts',(-0.0327271605178637,0.744165045296987,
-1.4892352953247));
#62718=CARTESIAN_POINT('Ctrl Pts',(-0.383315513059851,0.638687638149583,
-1.47342841000661));
#62719=CARTESIAN_POINT('Ctrl Pts',(-0.641305014810186,0.378920255009859,
-1.45762152468852));
#62720=CARTESIAN_POINT('Ctrl Pts',(-0.744372251859284,0.0276157987276915,
-1.44181463937042));
#62721=CARTESIAN_POINT('Ctrl Pts',(-0.667618916207993,-0.330359901317784,
-1.42600775405234));
#62722=CARTESIAN_POINT('Ctrl Pts',(-0.42958657592122,-0.608529420378104,
-1.41020086873424));
#62723=CARTESIAN_POINT('Ctrl Pts',(-0.0877775245687094,-0.739694388148254,
-1.39439398341615));
#62724=CARTESIAN_POINT('Ctrl Pts',(0.275236246195013,-0.692168830891646,
-1.37858709809806));
#62725=CARTESIAN_POINT('Ctrl Pts',(0.571760247498537,-0.47743366142098,
-1.36278021277997));
#62726=CARTESIAN_POINT('Ctrl Pts',(0.730162153444936,-0.14736319538502,
-1.34697332746187));
#62727=CARTESIAN_POINT('Ctrl Pts',(0.712176269184669,0.218306306110557,
-1.33116644214378));
#62728=CARTESIAN_POINT('Ctrl Pts',(0.522147506823372,0.531238800160123,
-1.31535955682569));
#62729=CARTESIAN_POINT('Ctrl Pts',(0.205981770016112,0.715838104670642,
-1.2995526715076));
#62730=CARTESIAN_POINT('Ctrl Pts',(-0.159943693537569,0.727509928849765,
-1.28374578618951));
#62731=CARTESIAN_POINT('Ctrl Pts',(-0.487231007294692,0.563434669866906,
-1.26793890087142));
#62732=CARTESIAN_POINT('Ctrl Pts',(-0.696816245846464,0.26324855403567,
-1.25213201555333));
#62733=CARTESIAN_POINT('Ctrl Pts',(-0.738069180121617,-0.100531423107573,
-1.23632513023523));
#62734=CARTESIAN_POINT('Ctrl Pts',(-0.601024196479397,-0.440025677573168,
-1.22051824491714));
#62735=CARTESIAN_POINT('Ctrl Pts',(-0.31878772437456,-0.673221411175788,
-1.20471135959905));
#62736=CARTESIAN_POINT('Ctrl Pts',(0.040459398011372,-0.743784726106948,
-1.18890447428096));
#62737=CARTESIAN_POINT('Ctrl Pts',(0.389932604049209,-0.634669398960461,
-1.17309758896287));
#62738=CARTESIAN_POINT('Ctrl Pts',(0.64520844579848,-0.372234795724066,
-1.15729070364477));
#62739=CARTESIAN_POINT('Ctrl Pts',(0.744619057557235,-0.019878148807343,
-1.14148381832669));
#62740=CARTESIAN_POINT('Ctrl Pts',(0.66414947491175,0.337280531089292,-1.12567693300859));
#62741=CARTESIAN_POINT('Ctrl Pts',(0.423239012533058,0.612961189593169,
-1.1098700476905));
#62742=CARTESIAN_POINT('Ctrl Pts',(0.0800852418731312,0.740566699029569,
-1.09406316237241));
#62743=CARTESIAN_POINT('Ctrl Pts',(-0.282414996931603,0.68927095629045,
-1.07825627705432));
#62744=CARTESIAN_POINT('Ctrl Pts',(-0.576691270696571,0.471465650901319,
-1.06244939173622));
#62745=CARTESIAN_POINT('Ctrl Pts',(-0.731654244820196,0.139766761835634,
-1.04664250641813));
#62746=CARTESIAN_POINT('Ctrl Pts',(-0.709868979076448,-0.225696066032155,
-1.03083562110004));
#62747=CARTESIAN_POINT('Ctrl Pts',(-0.516598215262442,-0.536636716657638,
-1.01502873578195));
#62748=CARTESIAN_POINT('Ctrl Pts',(-0.19853103850792,-0.717940184434885,
-0.999221850463857));
#62749=CARTESIAN_POINT('Ctrl Pts',(0.167495966080221,-0.725808365220657,
-0.983414965145765));
#62750=CARTESIAN_POINT('Ctrl Pts',(0.49306039234103,-0.558340515440121,
-0.967608079827675));
#62751=CARTESIAN_POINT('Ctrl Pts',(0.699514518741541,-0.255992421269104,
-0.951801194509581));
#62752=CARTESIAN_POINT('Ctrl Pts',(0.736984509774098,0.108196645190432,
-0.935994309191491));
#62753=CARTESIAN_POINT('Ctrl Pts',(0.596418610446852,0.446248274831483,
-0.920187423873398));
#62754=CARTESIAN_POINT('Ctrl Pts',(0.311773809962505,0.676498169324127,
-0.904380538555308));
#62755=CARTESIAN_POINT('Ctrl Pts',(-0.0481872653029185,0.743324067375768,
-0.888573653237214));
#62756=CARTESIAN_POINT('Ctrl Pts',(-0.396507576660238,0.630582606268565,
-0.872766767919124));
#62757=CARTESIAN_POINT('Ctrl Pts',(-0.649042184914044,0.365509129680006,
-0.856959882601032));
#62758=CARTESIAN_POINT('Ctrl Pts',(-0.744785433594142,0.0121383517585348,
-0.841152997282939));
#62759=CARTESIAN_POINT('Ctrl Pts',(-0.660608295836836,-0.344164729670229,
-0.825346111964851));
#62760=CARTESIAN_POINT('Ctrl Pts',(-0.41684573319125,-0.617326750107006,
-0.809539226646754));
#62761=CARTESIAN_POINT('Ctrl Pts',(-0.0723843088095669,-0.741359017963356,
-0.793732341328667));
#62762=CARTESIAN_POINT('Ctrl Pts',(0.28956324275129,-0.686298630426134,
-0.777925456010572));
#62763=CARTESIAN_POINT('Ctrl Pts',(0.581560002870819,-0.465446715251406,
-0.762118570692483));
#62764=CARTESIAN_POINT('Ctrl Pts',(0.733067306922282,-0.132155231448256,
-0.746311685374389));
#62765=CARTESIAN_POINT('Ctrl Pts',(0.707485012819814,0.233061447504257,
-0.730504800056298));
#62766=CARTESIAN_POINT('Ctrl Pts',(0.510993123599533,0.541976668604306,
-0.714697914738206));
#62767=CARTESIAN_POINT('Ctrl Pts',(0.191058862767314,0.719964716243436,
-0.698891029420114));
#62768=CARTESIAN_POINT('Ctrl Pts',(-0.175030146628531,0.724028403758185,
-0.683084144102023));
#62769=CARTESIAN_POINT('Ctrl Pts',(-0.498836519711745,0.553186052137345,
-0.667277258783931));
#62770=CARTESIAN_POINT('Ctrl Pts',(-0.702137233920144,0.248708637607138,
-0.65147037346584));
#62771=CARTESIAN_POINT('Ctrl Pts',(-0.735820234407457,-0.11585018046591,
-0.635663488147748));
#62772=CARTESIAN_POINT('Ctrl Pts',(-0.591748602551628,-0.452422670802011,
-0.619856602829656));
#62773=CARTESIAN_POINT('Ctrl Pts',(-0.304726219455804,-0.679701855855642,
-0.604049717511565));
#62774=CARTESIAN_POINT('Ctrl Pts',(0.0559099276707165,-0.742783118861276,
-0.588242832193472));
#62775=CARTESIAN_POINT('Ctrl Pts',(0.403039720700516,-0.62642770150679,
-0.57243594687538));
#62776=CARTESIAN_POINT('Ctrl Pts',(0.652805818057422,-0.358743983347191,
-0.55662906155729));
#62777=CARTESIAN_POINT('Ctrl Pts',(0.744871361998988,-0.00439724359163508,
-0.540822176239196));
#62778=CARTESIAN_POINT('Ctrl Pts',(0.656995761481957,0.351011753467274,
-0.525015290921106));
#62779=CARTESIAN_POINT('Ctrl Pts',(0.410407428462719,0.621625630375753,
-0.509208405603014));
#62780=CARTESIAN_POINT('Ctrl Pts',(0.0646755571904924,0.742071259367674,
-0.493401520284922));
#62781=CARTESIAN_POINT('Ctrl Pts',(-0.296680211539802,0.683252174353012,
-0.477594634966831));
#62782=CARTESIAN_POINT('Ctrl Pts',(-0.586365918127607,0.459377504603609,
-0.461787749648739));
#62783=CARTESIAN_POINT('Ctrl Pts',(-0.734401187119916,0.124529426378599,
-0.445980864330647));
#62784=CARTESIAN_POINT('Ctrl Pts',(-0.705024627917847,-0.240401654958819,
-0.430173979012555));
#62785=CARTESIAN_POINT('Ctrl Pts',(-0.505332837265582,-0.547258079207822,
-0.414367093694464));
#62786=CARTESIAN_POINT('Ctrl Pts',(-0.183566049898222,-0.721911481417541,
-0.398560208376372));
#62787=CARTESIAN_POINT('Ctrl Pts',(0.182545421382762,-0.722170236723908,
-0.38275332305828));
#62788=CARTESIAN_POINT('Ctrl Pts',(0.504558765499186,-0.547971836715596,
-0.366946437740188));
#62789=CARTESIAN_POINT('Ctrl Pts',(0.704684108095094,-0.241397989803689,
-0.351139552422097));
#62790=CARTESIAN_POINT('Ctrl Pts',(0.734576479772278,0.123491202240409,
-0.335332667104005));
#62791=CARTESIAN_POINT('Ctrl Pts',(0.587014677238078,0.458548198561907,
-0.319525781785913));
#62792=CARTESIAN_POINT('Ctrl Pts',(0.297645714065633,0.682832124722794,
-0.303718896467822));
#62793=CARTESIAN_POINT('Ctrl Pts',(-0.0636265508948266,0.742161938999467,
-0.28791201114973));
#62794=CARTESIAN_POINT('Ctrl Pts',(-0.409528330721868,0.622205133453962,
-0.272105125831639));
#62795=CARTESIAN_POINT('Ctrl Pts',(-0.656498938470381,0.351940087481438,
-0.256298240513547));
#62796=CARTESIAN_POINT('Ctrl Pts',(-0.744876833942882,-0.00334433958416066,
-0.240491355195455));
#62797=CARTESIAN_POINT('Ctrl Pts',(-0.653312261167338,-0.35782086281875,
-0.224684469877363));
#62798=CARTESIAN_POINT('Ctrl Pts',(-0.403924795511725,-0.625857366221906,
-0.208877584559271));
#62799=CARTESIAN_POINT('Ctrl Pts',(-0.0569598162792036,-0.742703345989235,
-0.19307069924118));
#62800=CARTESIAN_POINT('Ctrl Pts',(0.30376512791888,-0.680131917760592,
-0.177263813923087));
#62801=CARTESIAN_POINT('Ctrl Pts',(0.591108510359164,-0.453258673291466,
-0.161456928604996));
#62802=CARTESIAN_POINT('Ctrl Pts',(0.735655715888896,-0.116890172730191,
-0.145650043286904));
#62803=CARTESIAN_POINT('Ctrl Pts',(0.702488139931555,0.247715900256012,
-0.129843157968813));
#62804=CARTESIAN_POINT('Ctrl Pts',(0.499617870175296,0.552480368782428,
-0.114036272650721));
#62805=CARTESIAN_POINT('Ctrl Pts',(0.176053600022512,0.72378028771789,-0.0982293873326291));
#62806=CARTESIAN_POINT('Ctrl Pts',(-0.190041352006756,0.720234029518921,
-0.0824225020145375));
#62807=CARTESIAN_POINT('Ctrl Pts',(-0.510225780734878,0.542698501491867,
-0.0666156166964455));
#62808=CARTESIAN_POINT('Ctrl Pts',(-0.707156296708642,0.234061132259856,
-0.0508087313783536));
#62809=CARTESIAN_POINT('Ctrl Pts',(-0.733250580051175,-0.131118620476376,
-0.0350018460602618));
#62810=CARTESIAN_POINT('Ctrl Pts',(-0.582222828987448,-0.464624714204384,
-0.0191949607421702));
#62811=CARTESIAN_POINT('Ctrl Pts',(-0.290522299293338,-0.685887628114927,
-0.00338807542407897));
#62812=CARTESIAN_POINT('Ctrl Pts',(0.0713149466326984,-0.741462531680634,
0.0124188098940124));
#62813=CARTESIAN_POINT('Ctrl Pts',(0.416017697711953,-0.617911990905962,
0.0282256952121038));
#62814=CARTESIAN_POINT('Ctrl Pts',(0.57867045099816,-0.436036943086615,
0.0387636187574986));
#62815=CARTESIAN_POINT('Ctrl Pts',(0.63348975743001,-0.331175816864263,
0.044032580530196));
#62816=CARTESIAN_POINT('Ctrl Pts',(0.392888236737263,-0.550964357679773,
-3.9489));
#62817=CARTESIAN_POINT('Ctrl Pts',(0.484088989988678,-0.485929836599401,
-3.9436310382273));
#62818=CARTESIAN_POINT('Ctrl Pts',(0.633487089009969,-0.309770083749072,
-3.93309311468191));
#62819=CARTESIAN_POINT('Ctrl Pts',(0.704529888150662,0.0295137395378967,
-3.91728622936382));
#62820=CARTESIAN_POINT('Ctrl Pts',(0.605381802721961,0.361579326443786,
-3.90147934404573));
#62821=CARTESIAN_POINT('Ctrl Pts',(0.359987565129825,0.606340404497349,
-3.88567245872763));
#62822=CARTESIAN_POINT('Ctrl Pts',(0.0276308569381634,0.704603699753987,
-3.86986557340955));
#62823=CARTESIAN_POINT('Ctrl Pts',(-0.311401222734635,0.632664694044287,
-3.85405868809145));
#62824=CARTESIAN_POINT('Ctrl Pts',(-0.575206784816063,0.407884951603224,
-3.83825180277336));
#62825=CARTESIAN_POINT('Ctrl Pts',(-0.700057787321786,0.0845739690108998,
-3.82244491745527));
#62826=CARTESIAN_POINT('Ctrl Pts',(-0.655793349958048,-0.25916933839601,
-3.80663803213718));
#62827=CARTESIAN_POINT('Ctrl Pts',(-0.453106684122212,-0.54030344862574,
-3.79083114681908));
#62828=CARTESIAN_POINT('Ctrl Pts',(-0.140961456517365,-0.690914982312493,
-3.775024261501));
#62829=CARTESIAN_POINT('Ctrl Pts',(0.205236307704561,-0.674619600339438,
-3.7592173761829));
#62830=CARTESIAN_POINT('Ctrl Pts',(0.501854433527548,-0.495354136485513,
-3.74341049086481));
#62831=CARTESIAN_POINT('Ctrl Pts',(0.677237850353305,-0.196424212884838,
-3.72760360554672));
#62832=CARTESIAN_POINT('Ctrl Pts',(0.689018584600613,0.149956558745365,
-3.71179672022863));
#62833=CARTESIAN_POINT('Ctrl Pts',(0.534350721904737,0.46011182080935,-3.69598983491053));
#62834=CARTESIAN_POINT('Ctrl Pts',(0.250597912301867,0.659116276136679,
-3.68018294959245));
#62835=CARTESIAN_POINT('Ctrl Pts',(-0.0936926996039382,0.698895742478711,
-3.66437606427435));
#62836=CARTESIAN_POINT('Ctrl Pts',(-0.415349642780955,0.569840551551763,
-3.64856917895626));
#62837=CARTESIAN_POINT('Ctrl Pts',(-0.636669139983667,0.303127013768365,
-3.63276229363816));
#62838=CARTESIAN_POINT('Ctrl Pts',(-0.704186276738458,-0.0368139628855383,
-3.61695540832008));
#62839=CARTESIAN_POINT('Ctrl Pts',(-0.601590705440622,-0.367861663287755,
-3.60114852300198));
#62840=CARTESIAN_POINT('Ctrl Pts',(-0.353666792150765,-0.610043752821873,
-3.58534163768389));
#62841=CARTESIAN_POINT('Ctrl Pts',(-0.0203063718595239,-0.704855468490197,
-3.56953475236579));
#62842=CARTESIAN_POINT('Ctrl Pts',(0.317959528732968,-0.629392817167735,
-3.55372786704772));
#62843=CARTESIAN_POINT('Ctrl Pts',(0.579414849121761,-0.401885571804838,
-3.53792098172961));
#62844=CARTESIAN_POINT('Ctrl Pts',(0.700898925634034,-0.0772934425076206,
-3.52211409641153));
#62845=CARTESIAN_POINT('Ctrl Pts',(0.653064430829429,0.265970730335282,
-3.50630721109343));
#62846=CARTESIAN_POINT('Ctrl Pts',(0.447466908630123,0.544983436344741,
-3.49050032577534));
#62847=CARTESIAN_POINT('Ctrl Pts',(0.13377326171177,0.692342613639074,-3.47469344045725));
#62848=CARTESIAN_POINT('Ctrl Pts',(-0.212236453508304,0.672450197420986,
-3.45888655513916));
#62849=CARTESIAN_POINT('Ctrl Pts',(-0.506975476514332,0.490111667298897,
-3.44307966982107));
#62850=CARTESIAN_POINT('Ctrl Pts',(-0.679242684774237,0.189375170996836,
-3.42727278450297));
#62851=CARTESIAN_POINT('Ctrl Pts',(-0.687422894528262,-0.157109338639641,
-3.41146589918489));
#62852=CARTESIAN_POINT('Ctrl Pts',(-0.529539984287318,-0.465640403369804,
-3.39565901386679));
#62853=CARTESIAN_POINT('Ctrl Pts',(-0.243734273318034,-0.661685109564608,
-3.3798521285487));
#62854=CARTESIAN_POINT('Ctrl Pts',(0.100951166852987,-0.697884261264305,
-3.36404524323061));
#62855=CARTESIAN_POINT('Ctrl Pts',(0.421249485401818,-0.565493104518617,
-3.34823835791252));
#62856=CARTESIAN_POINT('Ctrl Pts',(0.639785112601671,-0.296493827764879,
-3.33243147259443));
#62857=CARTESIAN_POINT('Ctrl Pts',(0.703765643119916,0.0441304857599676,
-3.31662458727633));
#62858=CARTESIAN_POINT('Ctrl Pts',(0.597735079489259,0.374094045605343,
-3.30081770195824));
#62859=CARTESIAN_POINT('Ctrl Pts',(0.347307590733571,0.613686416362823,
-3.28501081664015));
#62860=CARTESIAN_POINT('Ctrl Pts',(0.0129798091970768,0.705028442520307,
-3.26920393132206));
#62861=CARTESIAN_POINT('Ctrl Pts',(-0.324483549622869,0.626054315721524,
-3.25339704600396));
#62862=CARTESIAN_POINT('Ctrl Pts',(-0.583560298007917,0.395842088209822,
-3.23759016068587));
#62863=CARTESIAN_POINT('Ctrl Pts',(-0.701664372128327,0.0700049219352693,
-3.22178327536779));
#62864=CARTESIAN_POINT('Ctrl Pts',(-0.650264963381902,-0.272743574823193,
-3.20597639004969));
#62865=CARTESIAN_POINT('Ctrl Pts',(-0.441778804249146,-0.549604465343574,
-3.1901695047316));
#62866=CARTESIAN_POINT('Ctrl Pts',(-0.126570615394638,-0.693695509231553,
-3.17436261941351));
#62867=CARTESIAN_POINT('Ctrl Pts',(0.219213673644229,-0.67020813595241,
-3.15855573409542));
#62868=CARTESIAN_POINT('Ctrl Pts',(0.512041759331881,-0.484816271292242,
-3.14274884877732));
#62869=CARTESIAN_POINT('Ctrl Pts',(0.681174150856313,-0.182305667532811,
-3.12694196345923));
#62870=CARTESIAN_POINT('Ctrl Pts',(0.685752952950544,0.164245145222046,
-3.11113507814114));
#62871=CARTESIAN_POINT('Ctrl Pts',(0.52467204859744,0.471118691658448,-3.09532819282305));
#62872=CARTESIAN_POINT('Ctrl Pts',(0.236844307533238,0.664182470559487,
-3.07952130750496));
#62873=CARTESIAN_POINT('Ctrl Pts',(-0.108198729930143,0.696797398854864,
-3.06371442218686));
#62874=CARTESIAN_POINT('Ctrl Pts',(-0.427103826957276,0.561084575806403,
-3.04790753686878));
#62875=CARTESIAN_POINT('Ctrl Pts',(-0.64283197915049,0.289828616238747,
-3.03210065155068));
#62876=CARTESIAN_POINT('Ctrl Pts',(-0.703268992599295,-0.0514422419590443,
-3.01629376623259));
#62877=CARTESIAN_POINT('Ctrl Pts',(-0.593814889478732,-0.380286020309405,
-3.0004868809145));
#62878=CARTESIAN_POINT('Ctrl Pts',(-0.340910875057239,-0.617262792882503,
-2.98467999559641));
#62879=CARTESIAN_POINT('Ctrl Pts',(-0.0056518445272595,-0.705125263242527,
-2.96887311027831));
#62880=CARTESIAN_POINT('Ctrl Pts',(0.330972521582021,-0.622648191330417,
-2.95306622496023));
#62881=CARTESIAN_POINT('Ctrl Pts',(0.587642713915593,-0.389755847924465,
-2.93725933964213));
#62882=CARTESIAN_POINT('Ctrl Pts',(0.70235402869083,-0.0627088398167523,
-2.92145245432404));
#62883=CARTESIAN_POINT('Ctrl Pts',(0.647395257884359,0.27948695904862,-2.90564556900594));
#62884=CARTESIAN_POINT('Ctrl Pts',(0.436042981348057,0.554166129086307,
-2.88983868368786));
#62885=CARTESIAN_POINT('Ctrl Pts',(0.11935429761476,0.694973475645141,-2.87403179836976));
#62886=CARTESIAN_POINT('Ctrl Pts',(-0.226167215523084,0.667893682281796,
-2.85822491305168));
#62887=CARTESIAN_POINT('Ctrl Pts',(-0.5170527342108,0.479468508094678,-2.84241802773358));
#62888=CARTESIAN_POINT('Ctrl Pts',(-0.683032040247721,0.175216472411809,
-2.82661114241549));
#62889=CARTESIAN_POINT('Ctrl Pts',(-0.684008940105105,-0.171363210945912,
-2.8108042570974));
#62890=CARTESIAN_POINT('Ctrl Pts',(-0.519747440714448,-0.476546092293478,
-2.79499737177931));
#62891=CARTESIAN_POINT('Ctrl Pts',(-0.229928759127129,-0.666608090211678,
-2.77919048646121));
#62892=CARTESIAN_POINT('Ctrl Pts',(0.115434605974731,-0.695635272217317,
-2.76338360114313));
#62893=CARTESIAN_POINT('Ctrl Pts',(0.432912035103061,-0.556615441819869,
-2.74757671582503));
#62894=CARTESIAN_POINT('Ctrl Pts',(0.645809410519448,-0.28313209901727,
-2.73176983050694));
#62895=CARTESIAN_POINT('Ctrl Pts',(0.70269637882455,0.0587484416496746,
-2.71596294518884));
#62896=CARTESIAN_POINT('Ctrl Pts',(0.589830558845161,0.386436918606138,
-2.70015605987076));
#62897=CARTESIAN_POINT('Ctrl Pts',(0.334477336060517,0.620772496065396,
-2.68434917455266));
#62898=CARTESIAN_POINT('Ctrl Pts',(-0.00167673062376321,0.705145920206461,
-2.66854228923458));
#62899=CARTESIAN_POINT('Ctrl Pts',(-0.337425743707141,0.619174811901361,
-2.65273540391648));
#62900=CARTESIAN_POINT('Ctrl Pts',(-0.591661655884731,0.383627508353011,
-2.63692851859839));
#62901=CARTESIAN_POINT('Ctrl Pts',(-0.702967820828586,0.0554059842337657,
-2.6211216332803));
#62902=CARTESIAN_POINT('Ctrl Pts',(-0.64445562430665,-0.286200154627713,
-2.60531474796221));
#62903=CARTESIAN_POINT('Ctrl Pts',(-0.430260059478938,-0.558667934847332,
-2.58950786264411));
#62904=CARTESIAN_POINT('Ctrl Pts',(-0.11212508783917,-0.696176374840788,
-2.57370097732603));
#62905=CARTESIAN_POINT('Ctrl Pts',(0.23309632806146,-0.665507086403793,
-2.55789409200792));
#62906=CARTESIAN_POINT('Ctrl Pts',(0.5220078598931,-0.474068955342181,-2.54208720668984));
#62907=CARTESIAN_POINT('Ctrl Pts',(0.684816152269453,-0.16810835136977,
-2.52628032137174));
#62908=CARTESIAN_POINT('Ctrl Pts',(0.682191044370633,0.178462766956884,
-2.51047343605366));
#62909=CARTESIAN_POINT('Ctrl Pts',(0.514766692567439,0.481922019036879,
-2.49466655073556));
#62910=CARTESIAN_POINT('Ctrl Pts',(0.222988375079262,0.668961706519075,
-2.47885966541747));
#62911=CARTESIAN_POINT('Ctrl Pts',(-0.122658013407166,0.694398006878195,
-2.46305278009938));
#62912=CARTESIAN_POINT('Ctrl Pts',(-0.43867348246843,0.552086185290324,
-2.44724589478129));
#62913=CARTESIAN_POINT('Ctrl Pts',(-0.648717085102761,0.276404999421464,
-2.4314390094632));
#62914=CARTESIAN_POINT('Ctrl Pts',(-0.702047863646276,-0.0660482956562912,
-2.4156321241451));
#62915=CARTESIAN_POINT('Ctrl Pts',(-0.58578251795406,-0.392546076109294,
-2.39982523882701));
#62916=CARTESIAN_POINT('Ctrl Pts',(-0.328007668658949,-0.624215146812637,
-2.38401835350892));
#62917=CARTESIAN_POINT('Ctrl Pts',(0.00900512466355355,-0.70509041118086,
-2.36821146819083));
#62918=CARTESIAN_POINT('Ctrl Pts',(0.343842518956618,-0.61563455260972,
-2.35240458287274));
#62919=CARTESIAN_POINT('Ctrl Pts',(0.595616689811292,-0.377457731445045,
-2.33659769755465));
#62920=CARTESIAN_POINT('Ctrl Pts',(0.703505682243138,-0.0480971440006585,
-2.32079081223656));
#62921=CARTESIAN_POINT('Ctrl Pts',(0.641446380171849,0.292882436437956,
-2.30498392691846));
#62922=CARTESIAN_POINT('Ctrl Pts',(0.424430663281246,0.563109396366323,
-2.28917704160037));
#62923=CARTESIAN_POINT('Ctrl Pts',(0.104883766927401,0.697304076887924,
-2.27337015628228));
#62924=CARTESIAN_POINT('Ctrl Pts',(-0.240000262814678,0.663048606105381,
-2.25756327096419));
#62925=CARTESIAN_POINT('Ctrl Pts',(-0.526906601153319,0.468618196264782,
-2.2417563856461));
#62926=CARTESIAN_POINT('Ctrl Pts',(-0.686526294211532,0.160982072186887,
-2.22594950032801));
#62927=CARTESIAN_POINT('Ctrl Pts',(-0.680299462106238,-0.185543046399923,
-2.21014261500991));
#62928=CARTESIAN_POINT('Ctrl Pts',(-0.509730342149469,-0.487245891210574,
-2.19433572969182));
#62929=CARTESIAN_POINT('Ctrl Pts',(-0.216023905051799,-0.671243065256971,
-2.17852884437373));
#62930=CARTESIAN_POINT('Ctrl Pts',(0.129868171994647,-0.693085736480105,
-2.16272195905564));
#62931=CARTESIAN_POINT('Ctrl Pts',(0.444387546733483,-0.547497295443183,
-2.14691507373755));
#62932=CARTESIAN_POINT('Ctrl Pts',(0.65155468882939,-0.269648044075677,
-2.13110818841945));
#62933=CARTESIAN_POINT('Ctrl Pts',(0.701323517113522,0.0733410154887558,
-2.11530130310137));
#62934=CARTESIAN_POINT('Ctrl Pts',(0.581671204052573,0.398612832941228,
-2.09949441778327));
#62935=CARTESIAN_POINT('Ctrl Pts',(0.321502571670479,0.627590373268003,
-2.08368753246518));
#62936=CARTESIAN_POINT('Ctrl Pts',(-0.0163325460192437,0.704958742161505,
-2.06788064714709));
#62937=CARTESIAN_POINT('Ctrl Pts',(-0.350222154225635,0.612027795854858,
-2.052073761829));
#62938=CARTESIAN_POINT('Ctrl Pts',(-0.599507388494239,0.371247183625977,
-2.03626687651091));
#62939=CARTESIAN_POINT('Ctrl Pts',(-0.70396755483765,0.040783108578214,
-2.02045999119281));
#62940=CARTESIAN_POINT('Ctrl Pts',(-0.638367850521979,-0.299533082695969,
-2.00465310587472));
#62941=CARTESIAN_POINT('Ctrl Pts',(-0.418555422414341,-0.567490033900997,
-1.98884622055663));
#62942=CARTESIAN_POINT('Ctrl Pts',(-0.097631117047166,-0.698356459978373,
-1.97303933523854));
#62943=CARTESIAN_POINT('Ctrl Pts',(0.246878274057621,-0.660518506938096,
-1.95723244992044));
#62944=CARTESIAN_POINT('Ctrl Pts',(0.531748428856327,-0.463116819623548,
-1.94142556460235));
#62945=CARTESIAN_POINT('Ctrl Pts',(0.68816228135381,-0.153838404604709,
-1.92561867928426));
#62946=CARTESIAN_POINT('Ctrl Pts',(0.678334397630255,0.192603284502106,
-1.90981179396617));
#62947=CARTESIAN_POINT('Ctrl Pts',(0.504638933459461,0.49251713375912,-1.89400490864808));
#62948=CARTESIAN_POINT('Ctrl Pts',(0.209036101308555,0.67345192000552,-1.87819802332998));
#62949=CARTESIAN_POINT('Ctrl Pts',(-0.137064302935446,0.691698602767291,
-1.8623911380119));
#62950=CARTESIAN_POINT('Ctrl Pts',(-0.450053610696377,0.542849267945122,
-1.8465842526938));
#62951=CARTESIAN_POINT('Ctrl Pts',(-0.654321915196967,0.262861962829116,
-1.83077736737571));
#62952=CARTESIAN_POINT('Ctrl Pts',(-0.700523417466219,-0.0806258134275274,
-1.81497048205762));
#62953=CARTESIAN_POINT('Ctrl Pts',(-0.577497061222251,-0.404636533804186,
-1.79916359673953));
#62954=CARTESIAN_POINT('Ctrl Pts',(-0.314962747739959,-0.630897810858063,
-1.78335671142144));
#62955=CARTESIAN_POINT('Ctrl Pts',(0.0236582032229997,-0.704750927370557,
-1.76754982610334));
#62956=CARTESIAN_POINT('Ctrl Pts',(0.356563960421018,-0.608354931218841,
-1.75174294078526));
#62957=CARTESIAN_POINT('Ctrl Pts',(0.603333331681656,-0.364996535725085,
-1.73593605546716));
#62958=CARTESIAN_POINT('Ctrl Pts',(0.704353388723183,-0.033464667988367,
-1.72012917014907));
#62959=CARTESIAN_POINT('Ctrl Pts',(0.635220367882906,0.306151375035467,
-1.70432228483098));
#62960=CARTESIAN_POINT('Ctrl Pts',(0.412634971489475,0.571809374278948,
-1.68851539951289));
#62961=CARTESIAN_POINT('Ctrl Pts',(0.0903679215898715,0.69933341043949,
-1.67270851419479));
#62962=CARTESIAN_POINT('Ctrl Pts',(-0.253729618865292,0.657917062189359,
-1.65690162887671));
#62963=CARTESIAN_POINT('Ctrl Pts',(-0.53653282001449,0.457565419646962,
-1.64109474355861));
#62964=CARTESIAN_POINT('Ctrl Pts',(-0.689723936985944,0.14667812024297,
-1.62528785824052));
#62965=CARTESIAN_POINT('Ctrl Pts',(-0.676296063198152,-0.19964271865531,
-1.60948097292243));
#62966=CARTESIAN_POINT('Ctrl Pts',(-0.499493016443407,-0.497735177311859,
-1.59367408760434));
#62967=CARTESIAN_POINT('Ctrl Pts',(-0.202025718633698,-0.67558803217637,
-1.57786720228624));
#62968=CARTESIAN_POINT('Ctrl Pts',(0.144245628943018,-0.690236755570315,
-1.56206031696815));
#62969=CARTESIAN_POINT('Ctrl Pts',(0.455671062340006,-0.538142604850548,
-1.54625343165006));
#62970=CARTESIAN_POINT('Ctrl Pts',(0.657018465304896,-0.256047488677006,
-1.53044654633197));
#62971=CARTESIAN_POINT('Ctrl Pts',(0.69964765112674,0.0879019026087411,
-1.51463966101388));
#62972=CARTESIAN_POINT('Ctrl Pts',(0.573260540331073,0.410616528051086,
-1.49883277569578));
#62973=CARTESIAN_POINT('Ctrl Pts',(0.308388903263251,0.63413710233158,-1.48302589037769));
#62974=CARTESIAN_POINT('Ctrl Pts',(-0.0309813049975863,0.704466989255031,
-1.4672190050596));
#62975=CARTESIAN_POINT('Ctrl Pts',(-0.362867252535701,0.604616355424324,
-1.45141211974151));
#62976=CARTESIAN_POINT('Ctrl Pts',(-0.607094106116187,0.358706462903012,
-1.43560523442342));
#62977=CARTESIAN_POINT('Ctrl Pts',(-0.704663142224076,0.0261426127288773,
-1.41979834910533));
#62978=CARTESIAN_POINT('Ctrl Pts',(-0.632004272228418,-0.312736598584864,
-1.40399146378724));
#62979=CARTESIAN_POINT('Ctrl Pts',(-0.406669950001241,-0.576066950948749,
-1.38818457846914));
#62980=CARTESIAN_POINT('Ctrl Pts',(-0.0830949650860008,-0.700234822746455,
-1.37237769315105));
#62981=CARTESIAN_POINT('Ctrl Pts',(0.260553557193054,-0.655244552852938,
-1.35657080783296));
#62982=CARTESIAN_POINT('Ctrl Pts',(0.541259257844153,-0.451964595966764,
-1.34076392251487));
#62983=CARTESIAN_POINT('Ctrl Pts',(0.69121109242647,-0.13950199251626,-1.32495703719678));
#62984=CARTESIAN_POINT('Ctrl Pts',(0.67418467897962,0.206660588498508,-1.30915015187868));
#62985=CARTESIAN_POINT('Ctrl Pts',(0.494293146935006,0.50289945824438,-1.29334326656059));
#62986=CARTESIAN_POINT('Ctrl Pts',(0.194993514250268,0.677651171038411,
-1.2775363812425));
#62987=CARTESIAN_POINT('Ctrl Pts',(-0.151411374329973,0.688700352789885,
-1.26172949592441));
#62988=CARTESIAN_POINT('Ctrl Pts',(-0.461239294898093,0.533377814547353,
-1.24592261060632));
#62989=CARTESIAN_POINT('Ctrl Pts',(-0.659644047886644,0.24920535768142,
-1.23011572528823));
#62990=CARTESIAN_POINT('Ctrl Pts',(-0.698696312690555,-0.0951684971092057,
-1.21430883997013));
#62991=CARTESIAN_POINT('Ctrl Pts',(-0.568962098984759,-0.416552169755792,
-1.19850195465204));
#62992=CARTESIAN_POINT('Ctrl Pts',(-0.301781748310929,-0.637307897798075,
-1.18269506933395));
#62993=CARTESIAN_POINT('Ctrl Pts',(0.0383010603417563,-0.704106958484362,
-1.16688818401586));
#62994=CARTESIAN_POINT('Ctrl Pts',(0.369131349722688,-0.600812472291737,
-1.15108129869777));
#62995=CARTESIAN_POINT('Ctrl Pts',(0.610789305579622,-0.352377644578884,
-1.13527441337968));
#62996=CARTESIAN_POINT('Ctrl Pts',(0.704896781882463,-0.0188177336879362,
-1.11946752806159));
#62997=CARTESIAN_POINT('Ctrl Pts',(0.628719910943502,0.319288042044476,
-1.10366064274349));
#62998=CARTESIAN_POINT('Ctrl Pts',(0.4006610022585,0.580262304030356,-1.0878537574254));
#62999=CARTESIAN_POINT('Ctrl Pts',(0.0758130331203709,0.701060599533658,
-1.07204687210731));
#63000=CARTESIAN_POINT('Ctrl Pts',(-0.267349351956566,0.65250126759862,
-1.05623998678922));
#63001=CARTESIAN_POINT('Ctrl Pts',(-0.545927231821457,0.446314953553164,
-1.04043310147113));
#63002=CARTESIAN_POINT('Ctrl Pts',(-0.692623587041027,0.132310796550484,
-1.02462621615303));
#63003=CARTESIAN_POINT('Ctrl Pts',(-0.672000473034784,-0.213656135999947,
-1.00881933083494));
#63004=CARTESIAN_POINT('Ctrl Pts',(-0.489039886595606,-0.508009418739415,
-0.99301244551685));
#63005=CARTESIAN_POINT('Ctrl Pts',(-0.187940247738363,-0.67964111374272,
-0.977205560198759));
#63006=CARTESIAN_POINT('Ctrl Pts',(0.158560765091847,-0.687089560379787,
-0.961398674880666));
#63007=CARTESIAN_POINT('Ctrl Pts',(0.466757706920742,-0.528555411702021,
-0.945591789562577));
#63008=CARTESIAN_POINT('Ctrl Pts',(0.662198379341202,-0.242336308891769,
-0.929784904244484));
#63009=CARTESIAN_POINT('Ctrl Pts',(0.697669504916014,0.102424812031291,
-0.913978018926392));
#63010=CARTESIAN_POINT('Ctrl Pts',(0.564602201477338,0.422442817782887,
-0.898171133608301));
#63011=CARTESIAN_POINT('Ctrl Pts',(0.295141996551584,0.640409854765639,
-0.882364248290208));
#63012=CARTESIAN_POINT('Ctrl Pts',(-0.0456166786157439,0.703670873947096,
-0.866557362972117));
#63013=CARTESIAN_POINT('Ctrl Pts',(-0.375355575368597,0.596943692695645,
-0.850750477654026));
#63014=CARTESIAN_POINT('Ctrl Pts',(-0.614418530936816,0.346010764356899,
-0.834943592335933));
#63015=CARTESIAN_POINT('Ctrl Pts',(-0.705054282461865,0.0114908220587519,
-0.819136707017843));
#63016=CARTESIAN_POINT('Ctrl Pts',(-0.62536763878683,-0.325804997763367,
-0.80332982169975));
#63017=CARTESIAN_POINT('Ctrl Pts',(-0.394608777314782,-0.584394980364765,
-0.787522936381659));
#63018=CARTESIAN_POINT('Ctrl Pts',(-0.0685229122472805,-0.701810651605228,
-0.771716051063567));
#63019=CARTESIAN_POINT('Ctrl Pts',(0.274116269111402,-0.649687502741008,
-0.755909165745476));
#63020=CARTESIAN_POINT('Ctrl Pts',(0.550536237737494,-0.440617102649509,
-0.740102280427383));
#63021=CARTESIAN_POINT('Ctrl Pts',(0.6939612682597,-0.125105309099136,-0.724295395109291));
#63022=CARTESIAN_POINT('Ctrl Pts',(0.669743681289579,0.220628605539007,
-0.7084885097912));
#63023=CARTESIAN_POINT('Ctrl Pts',(0.483733802853534,0.513064506847101,
-0.692681624473108));
#63024=CARTESIAN_POINT('Ctrl Pts',(0.180866680953096,0.681557645346608,
-0.676874739155017));
#63025=CARTESIAN_POINT('Ctrl Pts',(-0.165693028990715,0.685404552328976,
-0.661067853836925));
#63026=CARTESIAN_POINT('Ctrl Pts',(-0.47222570233939,0.523675917204019,
-0.645260968518833));
#63027=CARTESIAN_POINT('Ctrl Pts',(-0.664681183763715,0.235441084264976,
-0.629454083200741));
#63028=CARTESIAN_POINT('Ctrl Pts',(-0.696567338713257,-0.109670063587713,
-0.613647197882651));
#63029=CARTESIAN_POINT('Ctrl Pts',(-0.560181318740991,-0.428287835856923,
-0.597840312564558));
#63030=CARTESIAN_POINT('Ctrl Pts',(-0.288470365174735,-0.643442638177916,
-0.582033427246467));
#63031=CARTESIAN_POINT('Ctrl Pts',(0.0529273696266406,-0.703158782746691,
-0.566226541928374));
#63032=CARTESIAN_POINT('Ctrl Pts',(0.381539257166764,-0.593010434520368,
-0.550419656610283));
#63033=CARTESIAN_POINT('Ctrl Pts',(0.617981390178772,-0.339606509952495,
-0.534612771292191));
#63034=CARTESIAN_POINT('Ctrl Pts',(0.70513562694994,-0.00416266925407728,
-0.518805885974099));
#63035=CARTESIAN_POINT('Ctrl Pts',(0.621947817852421,0.33228676181577,-0.502999000656008));
#63036=CARTESIAN_POINT('Ctrl Pts',(0.388513928898186,0.588464533562985,
-0.487192115337916));
#63037=CARTESIAN_POINT('Ctrl Pts',(0.0612253899055303,0.702484897944656,
-0.471385230019824));
#63038=CARTESIAN_POINT('Ctrl Pts',(-0.280853577732319,0.646803562207529,
-0.455578344701733));
#63039=CARTESIAN_POINT('Ctrl Pts',(-0.555085777752791,0.434871658706356,
-0.439771459383642));
#63040=CARTESIAN_POINT('Ctrl Pts',(-0.695223991593445,0.1178863084594,-0.423964574065549));
#63041=CARTESIAN_POINT('Ctrl Pts',(-0.667414547510384,-0.227577243987833,
-0.408157688747458));
#63042=CARTESIAN_POINT('Ctrl Pts',(-0.478375468842551,-0.518064176544559,
-0.392350803429365));
#63043=CARTESIAN_POINT('Ctrl Pts',(-0.173773577942818,-0.683400558836909,
-0.376543918111274));
#63044=CARTESIAN_POINT('Ctrl Pts',(0.172807395639615,-0.68364551064267,
-0.360737032793182));
#63045=CARTESIAN_POINT('Ctrl Pts',(0.477642690529216,-0.518739858109735,
-0.34493014747509));
#63046=CARTESIAN_POINT('Ctrl Pts',(0.667092192979181,-0.228520428584966,
-0.329123262156999));
#63047=CARTESIAN_POINT('Ctrl Pts',(0.695389933124598,0.11690346918548,-0.313316376838907));
#63048=CARTESIAN_POINT('Ctrl Pts',(0.555699928310104,0.434086592632565,
-0.297509491520815));
#63049=CARTESIAN_POINT('Ctrl Pts',(0.281767574784161,0.646405920447539,
-0.281702606202724));
#63050=CARTESIAN_POINT('Ctrl Pts',(-0.0602323436566084,0.702570740201827,
-0.265895720884633));
#63051=CARTESIAN_POINT('Ctrl Pts',(-0.387681727301688,0.589013122604281,
-0.25008883556654));
#63052=CARTESIAN_POINT('Ctrl Pts',(-0.621477498246083,0.333165573138756,
-0.234281950248449));
#63053=CARTESIAN_POINT('Ctrl Pts',(-0.705140806988782,-0.00316593321977806,
-0.218475064930357));
#63054=CARTESIAN_POINT('Ctrl Pts',(-0.618460816691914,-0.338732633997832,
-0.202668179612265));
#63055=CARTESIAN_POINT('Ctrl Pts',(-0.382377116982208,-0.592470524209418,
-0.186861294294173));
#63056=CARTESIAN_POINT('Ctrl Pts',(-0.0539212511207285,-0.703083265419793,
-0.171054408976082));
#63057=CARTESIAN_POINT('Ctrl Pts',(0.287560543804209,-0.643849758100151,
-0.155247523657989));
#63058=CARTESIAN_POINT('Ctrl Pts',(0.559575372758286,-0.429079241151316,
-0.139440638339898));
#63059=CARTESIAN_POINT('Ctrl Pts',(0.696411596561459,-0.110654576665681,
-0.123633753021806));
#63060=CARTESIAN_POINT('Ctrl Pts',(0.665013370424364,0.234501305250519,
-0.107826867703715));
#63061=CARTESIAN_POINT('Ctrl Pts',(0.472965371062188,0.523007879069813,
-0.0920199823856229));
#63062=CARTESIAN_POINT('Ctrl Pts',(0.166661885477124,0.685169672229466,
-0.076213097067531));
#63063=CARTESIAN_POINT('Ctrl Pts',(-0.179903450085766,0.681812591898513,
-0.0604062117494397));
#63064=CARTESIAN_POINT('Ctrl Pts',(-0.483007394483508,0.513747833004724,
-0.0445993264313473));
#63065=CARTESIAN_POINT('Ctrl Pts',(-0.669432500791895,0.221574961343309,
-0.0287924411132557));
#63066=CARTESIAN_POINT('Ctrl Pts',(-0.694134764542732,-0.12412399693593,
-0.0129855557951638));
#63067=CARTESIAN_POINT('Ctrl Pts',(-0.551163704885714,-0.439838951879844,
0.00282132952292781));
#63068=CARTESIAN_POINT('Ctrl Pts',(-0.275024164045417,-0.649298425663846,
0.018628214841019));
#63069=CARTESIAN_POINT('Ctrl Pts',(0.0675105960172764,-0.701908643303733,
0.0344351001591104));
#63070=CARTESIAN_POINT('Ctrl Pts',(0.393824914024269,-0.584949001043688,
0.0502419854772018));
#63071=CARTESIAN_POINT('Ctrl Pts',(0.547800831229363,-0.41277621737474,
0.0607799090225966));
#63072=CARTESIAN_POINT('Ctrl Pts',(0.599695759644983,-0.313508988489687,
0.066048870795294));
#63073=CARTESIAN_POINT('',(0.701077753000062,-0.366509473613416,0.));
#63074=CARTESIAN_POINT('Ctrl Pts',(-0.564218010237599,-0.373640954068625,
7.21644966006352E-16));
#63075=CARTESIAN_POINT('Ctrl Pts',(-0.554510060806831,-0.391301626549833,
7.52778991897534E-16));
#63076=CARTESIAN_POINT('Ctrl Pts',(-0.544024301133767,-0.408498917022784,
8.63432540169627E-16));
#63077=CARTESIAN_POINT('Ctrl Pts',(-0.532788826860589,-0.425178050450441,
1.02695629777827E-15));
#63078=CARTESIAN_POINT('Ctrl Pts',(-0.516678281161148,-0.449094258594393,
1.27490859920589E-15));
#63079=CARTESIAN_POINT('Ctrl Pts',(-0.499027462499214,-0.471945953324106,
4.1283124830284E-16));
#63080=CARTESIAN_POINT('Ctrl Pts',(-0.479984048942617,-0.493634775998338,
5.20417042793042E-16));
#63081=CARTESIAN_POINT('Ctrl Pts',(-0.473276092698443,-0.501274565632376,
5.58313652021744E-16));
#63082=CARTESIAN_POINT('Ctrl Pts',(-0.466395095773147,-0.508769945555998,
3.16844864503691E-16));
#63083=CARTESIAN_POINT('Ctrl Pts',(-0.459346743724129,-0.516116152859011,
1.66533453693773E-16));
#63084=CARTESIAN_POINT('Ctrl Pts',(-0.452846524820441,-0.522891063540167,
2.79113946377707E-17));
#63085=CARTESIAN_POINT('Ctrl Pts',(-0.446209412880882,-0.52953328200918,
7.68010458298948E-16));
#63086=CARTESIAN_POINT('Ctrl Pts',(-0.439445630221723,-0.536034792396529,
7.7715611723761E-16));
#63087=CARTESIAN_POINT('Ctrl Pts',(-0.415262930686365,-0.559279784163135,
8.09854790940117E-16));
#63088=CARTESIAN_POINT('Ctrl Pts',(-0.389445190687811,-0.580748321127649,
2.21695987855779E-15));
#63089=CARTESIAN_POINT('Ctrl Pts',(-0.3622125634703,-0.600285727779798,
2.12330153459561E-15));
#63090=CARTESIAN_POINT('Ctrl Pts',(-0.35033589474735,-0.608806363877806,
2.08245534243448E-15));
#63091=CARTESIAN_POINT('Ctrl Pts',(-0.338189563353738,-0.616959334419476,
1.92489464226297E-15));
#63092=CARTESIAN_POINT('Ctrl Pts',(-0.325789558314903,-0.62472981087111,
1.79023462720806E-15));
#63093=CARTESIAN_POINT('Ctrl Pts',(-0.31703217919042,-0.630217631888256,
1.69513234289035E-15));
#63094=CARTESIAN_POINT('Ctrl Pts',(-0.308144761904281,-0.635516349767648,
1.35230555608436E-15));
#63095=CARTESIAN_POINT('Ctrl Pts',(-0.299156917123911,-0.640607333528386,
1.32532873564628E-15));
#63096=CARTESIAN_POINT('Ctrl Pts',(-0.29169022892703,-0.64483668876156,
1.30291763357715E-15));
#63097=CARTESIAN_POINT('Ctrl Pts',(-0.284151278188811,-0.648924659296807,
1.20875487286781E-15));
#63098=CARTESIAN_POINT('Ctrl Pts',(-0.276543809476503,-0.652868964991246,
1.22124532708767E-15));
#63099=CARTESIAN_POINT('Ctrl Pts',(-0.246334864268026,-0.668531640595291,
1.2639055129074E-15));
#63100=CARTESIAN_POINT('Ctrl Pts',(-0.21504836953113,-0.68193216733753,
1.1331870985744E-15));
#63101=CARTESIAN_POINT('Ctrl Pts',(-0.182960974453157,-0.693063919212634,
7.84095011141517E-16));
#63102=CARTESIAN_POINT('Ctrl Pts',(-0.160488941038507,-0.700859911984657,
5.39612433652176E-16));
#63103=CARTESIAN_POINT('Ctrl Pts',(-0.137623149403411,-0.707542338895848,
9.78508102310067E-16));
#63104=CARTESIAN_POINT('Ctrl Pts',(-0.114450318277965,-0.713096218066307,
1.1518563880486E-15));
#63105=CARTESIAN_POINT('Ctrl Pts',(-0.0964870036737186,-0.717401521905654,
1.28623400362656E-15));
#63106=CARTESIAN_POINT('Ctrl Pts',(-0.0783390261237154,-0.721028460504329,
1.29037321294563E-15));
#63107=CARTESIAN_POINT('Ctrl Pts',(-0.0600452300518944,-0.723965290929148,
9.5062846483529E-16));
#63108=CARTESIAN_POINT('Ctrl Pts',(-0.0528943522626845,-0.725113271117244,
8.17825346022505E-16));
#63109=CARTESIAN_POINT('Ctrl Pts',(-0.0457214326365342,-0.726155578268713,
1.34239484214797E-15));
#63110=CARTESIAN_POINT('Ctrl Pts',(-0.0385427376555631,-0.727089954163797,
1.29757316003065E-15));
#63111=CARTESIAN_POINT('Ctrl Pts',(-0.00231851625636514,-0.73180488346269,
1.07139966459643E-15));
#63112=CARTESIAN_POINT('Ctrl Pts',(0.0341393528175536,-0.73379106608169,
8.24934566925163E-16));
#63113=CARTESIAN_POINT('Ctrl Pts',(0.0705191993603075,-0.733021256094104,
9.36750677027476E-16));
#63114=CARTESIAN_POINT('Ctrl Pts',(0.10157783972999,-0.732364044647945,
1.04023535002902E-15));
#63115=CARTESIAN_POINT('Ctrl Pts',(0.132580760956565,-0.729697475366545,
2.00043039592424E-15));
#63116=CARTESIAN_POINT('Ctrl Pts',(0.163353306654297,-0.725092274746165,
1.85615411929518E-15));
#63117=CARTESIAN_POINT('Ctrl Pts',(0.181654685473116,-0.72235342038169,
1.77034858279218E-15));
#63118=CARTESIAN_POINT('Ctrl Pts',(0.199874675175882,-0.718928222955073,
-3.04629698038031E-17));
#63119=CARTESIAN_POINT('Ctrl Pts',(0.217976303857617,-0.714826100584156,
-1.83880688453542E-16));
#63120=CARTESIAN_POINT('Ctrl Pts',(0.227452922574193,-0.712678545227596,
-2.64198390775961E-16));
#63121=CARTESIAN_POINT('Ctrl Pts',(0.236900911941713,-0.710344158497489,
2.17105674296715E-16));
#63122=CARTESIAN_POINT('Ctrl Pts',(0.246287934957814,-0.707831707209637,
2.4980018054066E-16));
#63123=CARTESIAN_POINT('Ctrl Pts',(0.280987647322768,-0.698544275308181,
3.70657449201143E-16));
#63124=CARTESIAN_POINT('Ctrl Pts',(0.314923694096686,-0.686814217748739,
-5.34659704257165E-17));
#63125=CARTESIAN_POINT('Ctrl Pts',(0.347837497670182,-0.672763584846155,
6.93889390390723E-17));
#63126=CARTESIAN_POINT('Ctrl Pts',(0.37480383187388,-0.661251877857368,
1.70044171418847E-16));
#63127=CARTESIAN_POINT('Ctrl Pts',(0.40108450851066,-0.64818139147437,-3.8699560848025E-16));
#63128=CARTESIAN_POINT('Ctrl Pts',(0.426534291574676,-0.633593383890318,
-6.17561557447743E-16));
#63129=CARTESIAN_POINT('Ctrl Pts',(0.440986713378868,-0.625309146717957,
-7.48495339467814E-16));
#63130=CARTESIAN_POINT('Ctrl Pts',(0.455171082616751,-0.616535108140792,
-8.13090200322811E-16));
#63131=CARTESIAN_POINT('Ctrl Pts',(0.469069700451425,-0.607290200982864,
-8.70831184940357E-16));
#63132=CARTESIAN_POINT('Ctrl Pts',(0.476786897224892,-0.602156973453421,
-9.02891821867551E-16));
#63133=CARTESIAN_POINT('Ctrl Pts',(0.48441597550879,-0.596878537328559,
7.76292981169644E-16));
#63134=CARTESIAN_POINT('Ctrl Pts',(0.491953726322627,-0.591457859074385,
8.95117313604032E-16));
#63135=CARTESIAN_POINT('Ctrl Pts',(0.497924153838461,-0.587164301565985,
9.89234521964725E-16));
#63136=CARTESIAN_POINT('Ctrl Pts',(0.50383604081433,-0.582782248651759,
-6.48491678049708E-16));
#63137=CARTESIAN_POINT('Ctrl Pts',(0.509678190852515,-0.578320977422655,
-6.05418493115906E-16));
#63138=CARTESIAN_POINT('Ctrl Pts',(0.538552106605361,-0.556271839900029,
-3.92535991835301E-16));
#63139=CARTESIAN_POINT('Ctrl Pts',(0.565790235250783,-0.532244703810416,
-1.52188196534005E-15));
#63140=CARTESIAN_POINT('Ctrl Pts',(0.591234871672643,-0.506472330067542,
-1.00874170128051E-15));
#63141=CARTESIAN_POINT('Ctrl Pts',(0.616885738234245,-0.480491069856402,
-4.91442407922625E-16));
#63142=CARTESIAN_POINT('Ctrl Pts',(0.64071489582184,-0.452735434439652,
-5.70549400489371E-16));
#63143=CARTESIAN_POINT('Ctrl Pts',(0.662534433530974,-0.423398860723195,
-6.21464685268691E-16));
#63144=CARTESIAN_POINT('Ctrl Pts',(0.676187576319825,-0.405042081802127,
-6.53323914483071E-16));
#63145=CARTESIAN_POINT('Ctrl Pts',(0.689053304273939,-0.386065449904219,
-6.46391670435626E-17));
#63146=CARTESIAN_POINT('Ctrl Pts',(0.701077753000062,-0.366509473613416,
-3.46944695195361E-18));
#63147=CARTESIAN_POINT('Ctrl Pts',(0.701077753000062,-0.366509473613416,
-3.14469315649998E-20));
#63148=CARTESIAN_POINT('Ctrl Pts',(0.640409690535754,-0.482558394510364,
-0.00526896177269737));
#63149=CARTESIAN_POINT('Ctrl Pts',(0.550406477811535,-0.583198182570441,
-0.010537923545395));
#63150=CARTESIAN_POINT('Ctrl Pts',(0.44182493524546,-0.656306799567799,
-0.0158068853180924));
#63151=CARTESIAN_POINT('Ctrl Pts',(0.333243392679392,-0.729415416565154,
-0.0210758470907895));
#63152=CARTESIAN_POINT('Ctrl Pts',(0.206083520271465,-0.774992862499796,
-0.0263448088634866));
#63153=CARTESIAN_POINT('Ctrl Pts',(0.0757632144587173,-0.787530872897559,
-0.0316137706361836));
#63154=CARTESIAN_POINT('Ctrl Pts',(-0.0545570913540345,-0.800068883295322,
-0.0368827324088808));
#63155=CARTESIAN_POINT('Ctrl Pts',(-0.188037830571603,-0.779567458156207,
-0.0421516941815777));
#63156=CARTESIAN_POINT('Ctrl Pts',(-0.308581951414016,-0.728505113226044,
-0.0474206559542749));
#63157=CARTESIAN_POINT('Ctrl Pts',(-0.429126072256424,-0.677442768295882,
-0.0526896177269719));
#63158=CARTESIAN_POINT('Ctrl Pts',(-0.536733574723672,-0.595819503574671,
-0.0579585794996691));
#63159=CARTESIAN_POINT('Ctrl Pts',(-0.618394181603484,-0.493493142664703,
-0.0632275412723662));
#63160=CARTESIAN_POINT('Ctrl Pts',(-0.700054788483297,-0.391166781754735,
-0.0684965030450632));
#63161=CARTESIAN_POINT('Ctrl Pts',(-0.755768499775678,-0.268137324656005,
-0.0737654648177603));
#63162=CARTESIAN_POINT('Ctrl Pts',(-0.778812301667548,-0.139265705831607,
-0.0790344265904574));
#63163=CARTESIAN_POINT('Ctrl Pts',(-0.787023434197926,-0.0933452476304458,
-0.0809119007857365));
#63164=CARTESIAN_POINT('Ctrl Pts',(-0.791086499485871,-0.0466830157260825,
-0.0827893749810157));
#63165=CARTESIAN_POINT('Ctrl Pts',(-0.791053952037979,-1.51658468628413E-5,
-0.0846668491762948));
#63166=CARTESIAN_POINT('Origin',(0.,0.,0.914655896708346));
#63167=CARTESIAN_POINT('',(1.2,-0.692820323027552,0.858179306876173));
#63168=CARTESIAN_POINT('',(-2.54538057293978E-16,-1.3856406460551,0.858179306876173));
#63169=CARTESIAN_POINT('Ctrl Pts',(1.2,-0.692820323027552,0.858179306876173));
#63170=CARTESIAN_POINT('Ctrl Pts',(0.599999999999999,-1.03923048454133,
1.05817930687617));
#63171=CARTESIAN_POINT('Ctrl Pts',(-2.54538057293978E-16,-1.3856406460551,
0.858179306876173));
#63172=CARTESIAN_POINT('',(1.2,0.692820323027551,0.858179306876173));
#63173=CARTESIAN_POINT('Ctrl Pts',(1.2,0.692820323027551,0.858179306876173));
#63174=CARTESIAN_POINT('Ctrl Pts',(1.2,-6.66133814775094E-16,1.05817930687617));
#63175=CARTESIAN_POINT('Ctrl Pts',(1.2,-0.692820323027552,0.858179306876173));
#63176=CARTESIAN_POINT('',(8.48460190979925E-17,1.3856406460551,0.858179306876173));
#63177=CARTESIAN_POINT('Ctrl Pts',(8.48460190979925E-17,1.3856406460551,
0.858179306876173));
#63178=CARTESIAN_POINT('Ctrl Pts',(0.6,1.03923048454133,1.05817930687617));
#63179=CARTESIAN_POINT('Ctrl Pts',(1.2,0.692820323027551,0.858179306876173));
#63180=CARTESIAN_POINT('',(-1.2,0.692820323027551,0.858179306876173));
#63181=CARTESIAN_POINT('Ctrl Pts',(-1.2,0.692820323027551,0.858179306876173));
#63182=CARTESIAN_POINT('Ctrl Pts',(-0.600000000000001,1.03923048454133,
1.05817930687617));
#63183=CARTESIAN_POINT('Ctrl Pts',(8.48460190979925E-17,1.3856406460551,
0.858179306876173));
#63184=CARTESIAN_POINT('',(-1.2,-1.11389921653139E-16,0.965358983848622));
#63185=CARTESIAN_POINT('Ctrl Pts',(-1.2,-7.58222274085957E-17,0.965358983848622));
#63186=CARTESIAN_POINT('Ctrl Pts',(-1.2,0.321539030917347,0.965358983848622));
#63187=CARTESIAN_POINT('Ctrl Pts',(-1.2,0.692820323027551,0.858179306876173));
#63188=CARTESIAN_POINT('',(-1.14,-1.39609735102798E-16,1.));
#63189=CARTESIAN_POINT('',(-1.28782032302755,-1.5771250364726E-16,0.914655896708346));
#63190=CARTESIAN_POINT('Origin',(0.,0.,1.));
#63191=CARTESIAN_POINT('',(-1.2,-0.692820323027551,0.858179306876173));
#63192=CARTESIAN_POINT('Ctrl Pts',(-1.2,-0.692820323027551,0.858179306876173));
#63193=CARTESIAN_POINT('Ctrl Pts',(-1.2,-0.321539030917347,0.965358983848622));
#63194=CARTESIAN_POINT('Ctrl Pts',(-1.2,-7.58222274085957E-17,0.965358983848622));
#63195=CARTESIAN_POINT('Ctrl Pts',(-2.54538057293978E-16,-1.3856406460551,
0.858179306876173));
#63196=CARTESIAN_POINT('Ctrl Pts',(-0.599999999999999,-1.03923048454133,
1.05817930687617));
#63197=CARTESIAN_POINT('Ctrl Pts',(-1.2,-0.692820323027551,0.858179306876173));
#63198=CARTESIAN_POINT('Origin',(8.48460190979926E-17,1.3856406460551,0.05));
#63199=CARTESIAN_POINT('',(8.48460190979926E-17,1.3856406460551,0.05));
#63200=CARTESIAN_POINT('',(8.48460190979926E-17,1.3856406460551,0.05));
#63201=CARTESIAN_POINT('',(-1.2,0.692820323027551,0.05));
#63202=CARTESIAN_POINT('',(8.48460190979926E-17,1.3856406460551,0.05));
#63203=CARTESIAN_POINT('',(-1.2,0.692820323027551,0.05));
#63204=CARTESIAN_POINT('Origin',(1.2,0.692820323027551,0.05));
#63205=CARTESIAN_POINT('',(1.2,0.692820323027551,0.05));
#63206=CARTESIAN_POINT('',(1.2,0.692820323027551,0.05));
#63207=CARTESIAN_POINT('',(1.2,0.692820323027551,0.05));
#63208=CARTESIAN_POINT('Origin',(1.2,-0.692820323027552,0.05));
#63209=CARTESIAN_POINT('',(1.2,-0.692820323027552,0.05));
#63210=CARTESIAN_POINT('',(1.2,-0.692820323027552,0.05));
#63211=CARTESIAN_POINT('',(1.2,-0.692820323027552,0.05));
#63212=CARTESIAN_POINT('Origin',(0.,0.,0.05));
#63213=CARTESIAN_POINT('',(-2.54538057293978E-16,-1.3856406460551,0.05));
#63214=CARTESIAN_POINT('',(-2.54538057293978E-16,-1.3856406460551,0.05));
#63215=CARTESIAN_POINT('',(-1.2,-0.692820323027551,0.05));
#63216=CARTESIAN_POINT('',(-1.2,-0.692820323027551,0.05));
#63217=CARTESIAN_POINT('',(-1.2,0.692820323027551,0.05));
#63218=CARTESIAN_POINT('',(-1.125,-1.37772764904077E-16,0.05));
#63219=CARTESIAN_POINT('Origin',(0.,0.,0.05));
#63220=CARTESIAN_POINT('Origin',(-2.54538057293978E-16,-1.3856406460551,
0.05));
#63221=CARTESIAN_POINT('',(-2.54538057293978E-16,-1.3856406460551,0.05));
#63222=CARTESIAN_POINT('Origin',(-1.2,-0.692820323027551,0.05));
#63223=CARTESIAN_POINT('',(-1.2,-0.692820323027551,0.05));
#63224=CARTESIAN_POINT('Origin',(-1.2,0.692820323027551,0.05));
#63225=CARTESIAN_POINT('Origin',(0.,0.,1.));
#63226=CARTESIAN_POINT('Origin',(0.74,0.,-4.));
#63227=CARTESIAN_POINT('',(-0.74,-9.06238631369041E-17,-4.));
#63228=CARTESIAN_POINT('Origin',(0.,0.,-4.));
#63229=CARTESIAN_POINT('Origin',(0.,0.,-3.97));
#63230=CARTESIAN_POINT('',(-0.77,-9.42978035343462E-17,-3.97));
#63231=CARTESIAN_POINT('Origin',(0.,0.,-1.97));
#63232=CARTESIAN_POINT('Origin',(0.,0.,0.));
#63233=CARTESIAN_POINT('Origin',(1.125,0.,0.));
#63234=CARTESIAN_POINT('',(-1.125,-1.37772764904077E-16,0.));
#63235=CARTESIAN_POINT('Origin',(0.,0.,0.));
#63236=CARTESIAN_POINT('Origin',(0.,0.,0.025));
#63237=CARTESIAN_POINT('',(-1.125,-1.37772764904077E-16,0.025));
#63238=CARTESIAN_POINT('',(0.,0.,0.));
#63239=CARTESIAN_POINT('Origin',(33.6,-2.66251887604146E-17,1.78232233047034));
#63240=CARTESIAN_POINT('',(32.7303553390593,-3.94430452610506E-31,1.76464466094067));
#63241=CARTESIAN_POINT('Origin',(33.6,-5.32503775208292E-17,1.76464466094067));
#63242=CARTESIAN_POINT('',(32.645,-1.16953769318572E-16,1.8));
#63243=CARTESIAN_POINT('',(32.6876776695297,5.8476884659286E-17,1.78232233047034));
#63244=CARTESIAN_POINT('Origin',(33.6,0.,1.8));
#63245=CARTESIAN_POINT('Origin',(33.6,0.,1.75));
#63246=CARTESIAN_POINT('',(32.7596446609407,-2.05827695225079E-16,1.73535533905933));
#63247=CARTESIAN_POINT('',(32.745,-1.04707301327099E-16,1.75));
#63248=CARTESIAN_POINT('Origin',(33.6,-5.14569238062698E-17,1.73535533905933));
#63249=CARTESIAN_POINT('Origin',(33.6,0.,1.8));
#63250=CARTESIAN_POINT('',(30.5,-5.4,1.8));
#63251=CARTESIAN_POINT('',(30.5,5.4,1.8));
#63252=CARTESIAN_POINT('',(30.5,2.7,1.8));
#63253=CARTESIAN_POINT('',(31.2,-6.1,1.8));
#63254=CARTESIAN_POINT('Origin',(31.2,-5.4,1.8));
#63255=CARTESIAN_POINT('',(36.,-6.1,1.8));
#63256=CARTESIAN_POINT('',(32.4,-6.1,1.8));
#63257=CARTESIAN_POINT('',(36.7,-5.4,1.8));
#63258=CARTESIAN_POINT('Origin',(36.,-5.4,1.8));
#63259=CARTESIAN_POINT('',(36.7,5.4,1.8));
#63260=CARTESIAN_POINT('',(36.7,-2.7,1.8));
#63261=CARTESIAN_POINT('',(36.,6.1,1.8));
#63262=CARTESIAN_POINT('Origin',(36.,5.4,1.8));
#63263=CARTESIAN_POINT('',(31.2,6.1,1.8));
#63264=CARTESIAN_POINT('',(34.8,6.1,1.8));
#63265=CARTESIAN_POINT('Origin',(31.2,5.4,1.8));
#63266=CARTESIAN_POINT('Origin',(33.6,-2.57284619031349E-17,1.69267766952966));
#63267=CARTESIAN_POINT('',(32.795,9.85840673313619E-17,1.65));
#63268=CARTESIAN_POINT('',(32.7773223304703,-1.52205881278221E-16,1.69267766952966));
#63269=CARTESIAN_POINT('Origin',(33.6,0.,1.65));
#63270=CARTESIAN_POINT('Origin',(33.6,0.,0.99));
#63271=CARTESIAN_POINT('',(32.795,-9.85840673313619E-17,0.350000000000001));
#63272=CARTESIAN_POINT('Origin',(33.6,0.,0.350000000000001));
#63273=CARTESIAN_POINT('',(32.795,-9.85840673313619E-17,0.99));
#63274=CARTESIAN_POINT('Origin',(33.6,2.57284619031349E-17,0.307322330470336));
#63275=CARTESIAN_POINT('',(32.7596446609407,2.05827695225079E-16,0.264644660940671));
#63276=CARTESIAN_POINT('Origin',(33.6,5.14569238062698E-17,0.264644660940671));
#63277=CARTESIAN_POINT('',(32.7773223304703,1.52205881278221E-16,0.307322330470336));
#63278=CARTESIAN_POINT('Origin',(33.6,0.,0.25));
#63279=CARTESIAN_POINT('',(32.7303553390593,3.82104500966428E-31,0.235355339059325));
#63280=CARTESIAN_POINT('Origin',(33.6,5.32503775208292E-17,0.235355339059325));
#63281=CARTESIAN_POINT('',(32.745,1.04707301327099E-16,0.25));
#63282=CARTESIAN_POINT('Origin',(33.6,2.66251887604146E-17,0.217677669529663));
#63283=CARTESIAN_POINT('',(32.645,1.16953769318572E-16,0.2));
#63284=CARTESIAN_POINT('',(32.6876776695297,-5.8476884659286E-17,0.217677669529663));
#63285=CARTESIAN_POINT('Origin',(33.6,0.,0.2));
#63286=CARTESIAN_POINT('Origin',(33.6,0.,0.2));
#63287=CARTESIAN_POINT('',(30.55,5.4,0.2));
#63288=CARTESIAN_POINT('',(30.55,-5.4,0.2));
#63289=CARTESIAN_POINT('',(30.55,1.35,0.2));
#63290=CARTESIAN_POINT('',(31.2,6.05,0.2));
#63291=CARTESIAN_POINT('Origin',(31.2,5.4,0.2));
#63292=CARTESIAN_POINT('',(36.,6.04999999999999,0.2));
#63293=CARTESIAN_POINT('',(34.2,6.05,0.2));
#63294=CARTESIAN_POINT('',(36.65,5.4,0.2));
#63295=CARTESIAN_POINT('Origin',(36.,5.4,0.2));
#63296=CARTESIAN_POINT('',(36.65,-5.4,0.2));
#63297=CARTESIAN_POINT('',(36.65,-1.35,0.2));
#63298=CARTESIAN_POINT('',(36.,-6.05,0.2));
#63299=CARTESIAN_POINT('Origin',(36.,-5.4,0.2));
#63300=CARTESIAN_POINT('',(31.2,-6.05,0.2));
#63301=CARTESIAN_POINT('',(33.,-6.05,0.2));
#63302=CARTESIAN_POINT('Origin',(31.2,-5.4,0.2));
#63303=CARTESIAN_POINT('Origin',(36.,5.4,1.69267766952966));
#63304=CARTESIAN_POINT('',(36.,6.2,1.65));
#63305=CARTESIAN_POINT('',(36.,6.16464466094067,1.73535533905933));
#63306=CARTESIAN_POINT('',(36.,6.2,1.65));
#63307=CARTESIAN_POINT('',(36.7646446609407,5.4,1.73535533905933));
#63308=CARTESIAN_POINT('Origin',(36.,5.4,1.73535533905932));
#63309=CARTESIAN_POINT('',(36.8,5.4,1.65));
#63310=CARTESIAN_POINT('',(36.7646446609407,5.4,1.73535533905933));
#63311=CARTESIAN_POINT('Origin',(36.,5.4,1.65));
#63312=CARTESIAN_POINT('Origin',(35.4,6.18232233047034,1.69267766952966));
#63313=CARTESIAN_POINT('',(31.2,6.2,1.65));
#63314=CARTESIAN_POINT('',(31.2,6.16464466094067,1.73535533905933));
#63315=CARTESIAN_POINT('',(31.2,6.2,1.65));
#63316=CARTESIAN_POINT('',(35.4,6.16464466094067,1.73535533905933));
#63317=CARTESIAN_POINT('',(35.4,6.2,1.65));
#63318=CARTESIAN_POINT('Origin',(31.2,5.4,1.69267766952966));
#63319=CARTESIAN_POINT('',(30.4,5.4,1.65));
#63320=CARTESIAN_POINT('',(30.4353553390593,5.4,1.73535533905933));
#63321=CARTESIAN_POINT('',(30.4,5.4,1.65));
#63322=CARTESIAN_POINT('Origin',(31.2,5.4,1.73535533905933));
#63323=CARTESIAN_POINT('Origin',(31.2,5.4,1.65));
#63324=CARTESIAN_POINT('Origin',(30.4176776695297,4.05,1.69267766952966));
#63325=CARTESIAN_POINT('',(30.4,-5.4,1.65));
#63326=CARTESIAN_POINT('',(30.4353553390593,-5.4,1.73535533905933));
#63327=CARTESIAN_POINT('',(30.4,-5.4,1.65));
#63328=CARTESIAN_POINT('',(30.4353553390593,4.05,1.73535533905933));
#63329=CARTESIAN_POINT('',(30.4,4.05,1.65));
#63330=CARTESIAN_POINT('Origin',(31.2,-5.4,1.69267766952966));
#63331=CARTESIAN_POINT('',(31.2,-6.2,1.65));
#63332=CARTESIAN_POINT('',(31.2,-6.16464466094067,1.73535533905933));
#63333=CARTESIAN_POINT('',(31.2,-6.2,1.65));
#63334=CARTESIAN_POINT('Origin',(31.2,-5.4,1.73535533905933));
#63335=CARTESIAN_POINT('Origin',(31.2,-5.4,1.65));
#63336=CARTESIAN_POINT('Origin',(31.8,-6.18232233047034,1.69267766952966));
#63337=CARTESIAN_POINT('',(36.,-6.2,1.65));
#63338=CARTESIAN_POINT('',(36.,-6.16464466094067,1.73535533905933));
#63339=CARTESIAN_POINT('',(36.,-6.2,1.65));
#63340=CARTESIAN_POINT('',(31.8,-6.16464466094067,1.73535533905933));
#63341=CARTESIAN_POINT('',(31.8,-6.2,1.65));
#63342=CARTESIAN_POINT('Origin',(36.,-5.4,1.69267766952966));
#63343=CARTESIAN_POINT('',(36.8,-5.4,1.65));
#63344=CARTESIAN_POINT('',(36.7646446609407,-5.4,1.73535533905932));
#63345=CARTESIAN_POINT('',(36.8,-5.4,1.65));
#63346=CARTESIAN_POINT('Origin',(36.,-5.4,1.73535533905932));
#63347=CARTESIAN_POINT('Origin',(36.,-5.4,1.65));
#63348=CARTESIAN_POINT('Origin',(36.7823223304703,-4.05,1.69267766952967));
#63349=CARTESIAN_POINT('',(36.7646446609407,-4.05,1.73535533905933));
#63350=CARTESIAN_POINT('',(36.8,-4.05,1.65));
#63351=CARTESIAN_POINT('Origin',(30.4,5.4,0.2));
#63352=CARTESIAN_POINT('',(30.4,5.4,0.350000000000003));
#63353=CARTESIAN_POINT('',(30.4,5.4,0.2));
#63354=CARTESIAN_POINT('',(30.4,-5.4,0.350000000000003));
#63355=CARTESIAN_POINT('',(30.4,4.05,0.350000000000003));
#63356=CARTESIAN_POINT('',(30.4,-5.4,0.2));
#63357=CARTESIAN_POINT('Origin',(31.2,5.4,0.2));
#63358=CARTESIAN_POINT('',(31.2,6.2,0.350000000000001));
#63359=CARTESIAN_POINT('',(31.2,6.2,0.2));
#63360=CARTESIAN_POINT('Origin',(31.2,5.4,0.350000000000001));
#63361=CARTESIAN_POINT('Origin',(36.,6.2,0.2));
#63362=CARTESIAN_POINT('',(36.,6.2,0.35));
#63363=CARTESIAN_POINT('',(36.,6.2,0.2));
#63364=CARTESIAN_POINT('',(35.4,6.2,0.35));
#63365=CARTESIAN_POINT('Origin',(36.,5.4,0.2));
#63366=CARTESIAN_POINT('',(36.8,5.4,0.350000000000001));
#63367=CARTESIAN_POINT('',(36.8,5.4,0.2));
#63368=CARTESIAN_POINT('Origin',(36.,5.4,0.350000000000001));
#63369=CARTESIAN_POINT('Origin',(32.4,-6.15,1.75));
#63370=CARTESIAN_POINT('',(36.,-6.2,1.7));
#63371=CARTESIAN_POINT('',(31.2,-6.2,1.7));
#63372=CARTESIAN_POINT('Origin',(36.,-5.4,1.75));
#63373=CARTESIAN_POINT('',(36.8,-5.4,1.7));
#63374=CARTESIAN_POINT('Origin',(36.75,-2.7,1.75));
#63375=CARTESIAN_POINT('',(36.8,5.4,1.7));
#63376=CARTESIAN_POINT('Origin',(36.,5.4,1.75));
#63377=CARTESIAN_POINT('',(36.,6.2,1.7));
#63378=CARTESIAN_POINT('Origin',(30.5073223304703,1.35,0.217677669529665));
#63379=CARTESIAN_POINT('',(30.4646446609407,-5.4,0.235355339059329));
#63380=CARTESIAN_POINT('',(30.55,-5.4,0.2));
#63381=CARTESIAN_POINT('',(30.4646446609407,5.4,0.235355339059329));
#63382=CARTESIAN_POINT('',(30.4646446609407,1.35,0.23535533905933));
#63383=CARTESIAN_POINT('',(30.4646446609407,5.4,0.235355339059329));
#63384=CARTESIAN_POINT('Origin',(31.2,-5.4,0.217677669529663));
#63385=CARTESIAN_POINT('',(31.2,-6.13535533905933,0.235355339059327));
#63386=CARTESIAN_POINT('',(31.2,-6.05,0.2));
#63387=CARTESIAN_POINT('Origin',(31.2,-5.4,0.235355339059327));
#63388=CARTESIAN_POINT('Origin',(33.,-6.09267766952966,0.217677669529664));
#63389=CARTESIAN_POINT('',(36.,-6.13535533905933,0.235355339059327));
#63390=CARTESIAN_POINT('',(36.,-6.05,0.2));
#63391=CARTESIAN_POINT('',(33.,-6.13535533905933,0.235355339059327));
#63392=CARTESIAN_POINT('Origin',(36.,-5.4,0.217677669529663));
#63393=CARTESIAN_POINT('',(36.7353553390593,-5.4,0.235355339059329));
#63394=CARTESIAN_POINT('',(36.65,-5.4,0.2));
#63395=CARTESIAN_POINT('Origin',(36.,-5.4,0.235355339059325));
#63396=CARTESIAN_POINT('Origin',(36.6926776695297,-1.35,0.217677669529663));
#63397=CARTESIAN_POINT('',(36.7353553390593,5.4,0.235355339059326));
#63398=CARTESIAN_POINT('',(36.65,5.4,0.2));
#63399=CARTESIAN_POINT('',(36.7353553390593,-1.35,0.235355339059326));
#63400=CARTESIAN_POINT('Origin',(36.,5.4,0.217677669529663));
#63401=CARTESIAN_POINT('',(36.,6.13535533905932,0.235355339059322));
#63402=CARTESIAN_POINT('',(36.,6.04999999999999,0.2));
#63403=CARTESIAN_POINT('Origin',(36.,5.4,0.235355339059326));
#63404=CARTESIAN_POINT('Origin',(34.2,6.09267766952966,0.217677669529664));
#63405=CARTESIAN_POINT('',(31.2,6.13535533905933,0.235355339059327));
#63406=CARTESIAN_POINT('',(31.2,6.05,0.2));
#63407=CARTESIAN_POINT('',(34.2,6.13535533905933,0.235355339059327));
#63408=CARTESIAN_POINT('Origin',(31.2,5.4,0.217677669529663));
#63409=CARTESIAN_POINT('Origin',(31.2,5.4,0.235355339059326));
#63410=CARTESIAN_POINT('Origin',(36.,5.4,0.25));
#63411=CARTESIAN_POINT('',(36.,6.16464466094067,0.264644660940673));
#63412=CARTESIAN_POINT('',(36.,6.1,0.2));
#63413=CARTESIAN_POINT('',(36.7646446609407,5.4,0.264644660940674));
#63414=CARTESIAN_POINT('Origin',(36.,5.4,0.264644660940677));
#63415=CARTESIAN_POINT('',(36.7,5.4,0.2));
#63416=CARTESIAN_POINT('Origin',(34.8,6.15,0.25));
#63417=CARTESIAN_POINT('',(31.2,6.16464466094067,0.264644660940674));
#63418=CARTESIAN_POINT('',(31.2,6.1,0.2));
#63419=CARTESIAN_POINT('',(35.4,6.16464466094067,0.264644660940673));
#63420=CARTESIAN_POINT('Origin',(31.2,5.4,0.25));
#63421=CARTESIAN_POINT('',(30.4353553390593,5.4,0.264644660940674));
#63422=CARTESIAN_POINT('',(30.4,5.4,0.3));
#63423=CARTESIAN_POINT('Origin',(31.2,5.4,0.264644660940674));
#63424=CARTESIAN_POINT('Origin',(30.45,2.7,0.25));
#63425=CARTESIAN_POINT('',(30.4353553390593,-5.4,0.264644660940674));
#63426=CARTESIAN_POINT('',(30.5,-5.4,0.2));
#63427=CARTESIAN_POINT('',(30.4353553390593,4.05,0.264644660940673));
#63428=CARTESIAN_POINT('Origin',(30.4176776695297,4.05,0.307322330470338));
#63429=CARTESIAN_POINT('',(30.4,5.4,0.350000000000003));
#63430=CARTESIAN_POINT('',(30.4353553390593,-5.4,0.264644660940674));
#63431=CARTESIAN_POINT('Origin',(31.2,5.4,0.307322330470338));
#63432=CARTESIAN_POINT('',(31.2,6.2,0.350000000000001));
#63433=CARTESIAN_POINT('Origin',(35.4,6.18232233047034,0.307322330470336));
#63434=CARTESIAN_POINT('',(36.,6.2,0.35));
#63435=CARTESIAN_POINT('Origin',(36.,5.4,0.307322330470339));
#63436=CARTESIAN_POINT('',(36.8,5.4,0.350000000000001));
#63437=CARTESIAN_POINT('Origin',(36.7823223304703,-4.05,0.307322330470338));
#63438=CARTESIAN_POINT('',(36.8,-5.4,0.350000000000001));
#63439=CARTESIAN_POINT('',(36.7646446609407,-5.4,0.264644660940673));
#63440=CARTESIAN_POINT('',(36.8,-5.4,0.350000000000001));
#63441=CARTESIAN_POINT('',(36.7646446609407,-4.05,0.264644660940674));
#63442=CARTESIAN_POINT('',(36.8,-4.05,0.350000000000001));
#63443=CARTESIAN_POINT('Origin',(36.,-5.4,0.307322330470338));
#63444=CARTESIAN_POINT('',(36.,-6.2,0.350000000000001));
#63445=CARTESIAN_POINT('',(36.,-6.16464466094067,0.264644660940674));
#63446=CARTESIAN_POINT('',(36.,-6.2,0.350000000000001));
#63447=CARTESIAN_POINT('Origin',(36.,-5.4,0.264644660940675));
#63448=CARTESIAN_POINT('Origin',(36.,-5.4,0.350000000000001));
#63449=CARTESIAN_POINT('Origin',(31.8,-6.18232233047034,0.307322330470336));
#63450=CARTESIAN_POINT('',(31.2,-6.2,0.35));
#63451=CARTESIAN_POINT('',(31.2,-6.16464466094067,0.264644660940673));
#63452=CARTESIAN_POINT('',(31.2,-6.2,0.35));
#63453=CARTESIAN_POINT('',(31.8,-6.16464466094067,0.264644660940673));
#63454=CARTESIAN_POINT('',(31.8,-6.2,0.35));
#63455=CARTESIAN_POINT('Origin',(31.2,-5.4,0.307322330470338));
#63456=CARTESIAN_POINT('Origin',(31.2,-5.4,0.264644660940674));
#63457=CARTESIAN_POINT('Origin',(31.2,-5.4,0.350000000000002));
#63458=CARTESIAN_POINT('Origin',(36.,-5.4,0.25));
#63459=CARTESIAN_POINT('',(36.7,-5.4,0.2));
#63460=CARTESIAN_POINT('',(36.,-6.1,0.2));
#63461=CARTESIAN_POINT('Origin',(32.4,-6.15,0.25));
#63462=CARTESIAN_POINT('',(31.2,-6.1,0.2));
#63463=CARTESIAN_POINT('Origin',(31.2,-5.4,0.25));
#63464=CARTESIAN_POINT('Origin',(36.75,-2.7,0.25));
#63465=CARTESIAN_POINT('Origin',(30.45,2.7,1.75));
#63466=CARTESIAN_POINT('',(30.4,-5.4,1.7));
#63467=CARTESIAN_POINT('',(30.5,5.4,1.8));
#63468=CARTESIAN_POINT('Origin',(31.2,-5.4,1.75));
#63469=CARTESIAN_POINT('Origin',(34.8,6.15,1.75));
#63470=CARTESIAN_POINT('',(31.2,6.2,1.7));
#63471=CARTESIAN_POINT('Origin',(31.2,5.4,1.75));
#63472=CARTESIAN_POINT('Origin',(36.,-5.4,0.2));
#63473=CARTESIAN_POINT('',(36.,-6.2,0.2));
#63474=CARTESIAN_POINT('',(36.8,-5.4,0.2));
#63475=CARTESIAN_POINT('Origin',(31.2,-6.2,0.2));
#63476=CARTESIAN_POINT('',(31.2,-6.2,0.2));
#63477=CARTESIAN_POINT('Origin',(31.2,-5.4,0.2));
#63478=CARTESIAN_POINT('Origin',(36.8,-5.4,0.2));
#63479=CARTESIAN_POINT('',(0.,0.,0.));
#63480=CARTESIAN_POINT('Origin',(8.34,0.,26.5));
#63481=CARTESIAN_POINT('',(8.3,-1.49,26.5));
#63482=CARTESIAN_POINT('Origin',(8.3,0.,26.5));
#63483=CARTESIAN_POINT('',(8.37,-1.56,26.5));
#63484=CARTESIAN_POINT('',(8.34,-1.53,26.5));
#63485=CARTESIAN_POINT('Origin',(8.37,0.,26.5));
#63486=CARTESIAN_POINT('Origin',(8.26,0.,26.5));
#63487=CARTESIAN_POINT('',(8.23,-1.56,26.5));
#63488=CARTESIAN_POINT('Origin',(8.23,0.,26.5));
#63489=CARTESIAN_POINT('',(8.26,-1.53,26.5));
#63490=CARTESIAN_POINT('Origin',(8.3,0.,26.5));
#63491=CARTESIAN_POINT('',(8.15,-1.56,26.5));
#63492=CARTESIAN_POINT('',(8.3,-1.56,26.5));
#63493=CARTESIAN_POINT('Origin',(8.15,0.,26.5));
#63494=CARTESIAN_POINT('Origin',(7.975,0.,26.5));
#63495=CARTESIAN_POINT('',(8.15,-1.05,26.5));
#63496=CARTESIAN_POINT('Origin',(8.15,0.,26.5));
#63497=CARTESIAN_POINT('',(7.8,-1.05,26.5));
#63498=CARTESIAN_POINT('',(7.975,-1.05,26.5));
#63499=CARTESIAN_POINT('Origin',(7.8,0.,26.5));
#63500=CARTESIAN_POINT('Origin',(7.8,1.7,26.5));
#63501=CARTESIAN_POINT('',(7.8,-1.7,26.5));
#63502=CARTESIAN_POINT('Origin',(7.8,0.,26.5));
#63503=CARTESIAN_POINT('Origin',(7.825,0.,26.5));
#63504=CARTESIAN_POINT('',(7.85,-1.75,26.5));
#63505=CARTESIAN_POINT('Origin',(7.85,0.,26.5));
#63506=CARTESIAN_POINT('',(7.825,-1.725,26.5));
#63507=CARTESIAN_POINT('Origin',(8.,0.,26.5));
#63508=CARTESIAN_POINT('',(8.15,-1.75,26.5));
#63509=CARTESIAN_POINT('Origin',(8.15,0.,26.5));
#63510=CARTESIAN_POINT('',(8.,-1.75,26.5));
#63511=CARTESIAN_POINT('Origin',(8.15,1.56,26.5));
#63512=CARTESIAN_POINT('Origin',(8.3,0.,26.5));
#63513=CARTESIAN_POINT('',(8.45,-1.56,26.5));
#63514=CARTESIAN_POINT('Origin',(8.45,0.,26.5));
#63515=CARTESIAN_POINT('',(8.3,-1.56,26.5));
#63516=CARTESIAN_POINT('Origin',(8.45,1.72,26.5));
#63517=CARTESIAN_POINT('',(8.45,-1.72,26.5));
#63518=CARTESIAN_POINT('Origin',(8.45,0.,26.5));
#63519=CARTESIAN_POINT('Origin',(8.6,0.,26.5));
#63520=CARTESIAN_POINT('',(8.75,-1.72,26.5));
#63521=CARTESIAN_POINT('Origin',(8.75,0.,26.5));
#63522=CARTESIAN_POINT('',(8.6,-1.72,26.5));
#63523=CARTESIAN_POINT('Origin',(8.775,0.,26.5));
#63524=CARTESIAN_POINT('',(8.8,-1.67,26.5));
#63525=CARTESIAN_POINT('Origin',(8.8,0.,26.5));
#63526=CARTESIAN_POINT('',(8.775,-1.695,26.5));
#63527=CARTESIAN_POINT('Origin',(8.8,1.,26.5));
#63528=CARTESIAN_POINT('',(8.8,-1.,26.5));
#63529=CARTESIAN_POINT('Origin',(8.8,0.,26.5));
#63530=CARTESIAN_POINT('Origin',(8.625,0.,26.5));
#63531=CARTESIAN_POINT('',(8.45,-1.,26.5));
#63532=CARTESIAN_POINT('',(8.625,-1.,26.5));
#63533=CARTESIAN_POINT('Origin',(8.45,0.,26.5));
#63534=CARTESIAN_POINT('Origin',(8.45,1.24,26.5));
#63535=CARTESIAN_POINT('',(8.45,-1.24,26.5));
#63536=CARTESIAN_POINT('Origin',(8.45,0.,26.5));
#63537=CARTESIAN_POINT('Origin',(8.3,0.,26.5));
#63538=CARTESIAN_POINT('',(8.15,-1.24,26.5));
#63539=CARTESIAN_POINT('',(8.3,-1.24,26.5));
#63540=CARTESIAN_POINT('Origin',(8.15,0.,26.5));
#63541=CARTESIAN_POINT('Origin',(8.15,1.05,26.5));
#63542=CARTESIAN_POINT('',(0.,0.,0.));
#63543=CARTESIAN_POINT('Origin',(0.,0.,-1.97));
#63544=CARTESIAN_POINT('',(-0.591686266410893,1.49359204264163E-5,-3.89198748077951));
#63545=CARTESIAN_POINT('',(-0.591672685651915,9.86808882838178E-6,-3.91716251922049));
#63546=CARTESIAN_POINT('',(-0.591675,-7.2459289488551E-17,-1.97));
#63547=CARTESIAN_POINT('',(0.258403420312052,0.532281296094751,-3.948325));
#63548=CARTESIAN_POINT('Ctrl Pts',(-0.591686266410893,1.49359204264163E-5,
-3.89198748077951));
#63549=CARTESIAN_POINT('Ctrl Pts',(-0.591706039082766,0.0191956542142459,
-3.89289044879051));
#63550=CARTESIAN_POINT('Ctrl Pts',(-0.590791776357017,0.0383744891623322,
-3.89379341680151));
#63551=CARTESIAN_POINT('Ctrl Pts',(-0.588929556550066,0.0574608246427564,
-3.89469638481251));
#63552=CARTESIAN_POINT('Ctrl Pts',(-0.579367464989497,0.155464984376378,
-3.89933292812776));
#63553=CARTESIAN_POINT('Ctrl Pts',(-0.544811556310261,0.251030305027336,
-3.90396947144302));
#63554=CARTESIAN_POINT('Ctrl Pts',(-0.489482341063839,0.332485605744252,
-3.90860601475827));
#63555=CARTESIAN_POINT('Ctrl Pts',(-0.434153125817416,0.413940906461167,
-3.91324255807352));
#63556=CARTESIAN_POINT('Ctrl Pts',(-0.358050604003807,0.481286187244039,
-3.91787910138878));
#63557=CARTESIAN_POINT('Ctrl Pts',(-0.270469482917255,0.5262949306221,-3.92251564470403));
#63558=CARTESIAN_POINT('Ctrl Pts',(-0.182888361830704,0.57130367400016,
-3.92715218801928));
#63559=CARTESIAN_POINT('Ctrl Pts',(-0.0838286414712106,0.593975879973408,
-3.93178873133454));
#63560=CARTESIAN_POINT('Ctrl Pts',(0.0146109189770026,0.591545050739007,
-3.93642527464979));
#63561=CARTESIAN_POINT('Ctrl Pts',(0.0988262243084228,0.589465469874856,
-3.94039184976653));
#63562=CARTESIAN_POINT('Ctrl Pts',(0.18258764403161,0.569013359286537,-3.94435842488326));
#63563=CARTESIAN_POINT('Ctrl Pts',(0.258414858989722,0.532291148796136,
-3.948325));
#63564=CARTESIAN_POINT('',(-0.258391981634415,0.53227144339335,-3.948325));
#63565=CARTESIAN_POINT('Origin',(0.,0.,-3.948325));
#63566=CARTESIAN_POINT('Ctrl Pts',(-0.258391981634415,0.53227144339335,
-3.948325));
#63567=CARTESIAN_POINT('Ctrl Pts',(-0.346999241769788,0.489256914213254,
-3.94368845668475));
#63568=CARTESIAN_POINT('Ctrl Pts',(-0.424612905004657,0.423710754820817,
-3.93905191336949));
#63569=CARTESIAN_POINT('Ctrl Pts',(-0.481782348966959,0.343551262433901,
-3.93441537005424));
#63570=CARTESIAN_POINT('Ctrl Pts',(-0.538951792929262,0.263391770046983,
-3.92977882673899));
#63571=CARTESIAN_POINT('Ctrl Pts',(-0.575677017618998,0.168618944665585,
-3.92514228342374));
#63572=CARTESIAN_POINT('Ctrl Pts',(-0.587468894991019,0.0708530052396791,
-3.92050574010848));
#63573=CARTESIAN_POINT('Ctrl Pts',(-0.590303107755304,0.0473546712008031,
-3.91939133314582));
#63574=CARTESIAN_POINT('Ctrl Pts',(-0.591696932244061,0.0236834263079573,
-3.91827692618316));
#63575=CARTESIAN_POINT('Ctrl Pts',(-0.591672685651915,9.86808882838178E-6,
-3.91716251922049));
#63576=CARTESIAN_POINT('Origin',(0.,0.,-1.97));
#63577=CARTESIAN_POINT('',(-0.591677080768459,-1.5385395483597E-5,-3.71698748077951));
#63578=CARTESIAN_POINT('',(-0.591691313069437,-1.42991252893039E-5,-3.74216251922049));
#63579=CARTESIAN_POINT('',(-0.591675,-7.2459289488551E-17,-1.97));
#63580=CARTESIAN_POINT('Ctrl Pts',(-0.591677080768459,-1.5385395483597E-5,
-3.71698748077951));
#63581=CARTESIAN_POINT('Ctrl Pts',(-0.591598027752696,0.076411593433387,
-3.72058526234081));
#63582=CARTESIAN_POINT('Ctrl Pts',(-0.576722878987479,0.152868446627701,
-3.72418304390211));
#63583=CARTESIAN_POINT('Ctrl Pts',(-0.547848301688052,0.223611254898452,
-3.72778082546341));
#63584=CARTESIAN_POINT('Ctrl Pts',(-0.510636974074789,0.314779128545468,
-3.73241736877866));
#63585=CARTESIAN_POINT('Ctrl Pts',(-0.450175303298876,0.396457078729179,
-3.73705391209391));
#63586=CARTESIAN_POINT('Ctrl Pts',(-0.37384776457188,0.458669384024616,
-3.74169045540916));
#63587=CARTESIAN_POINT('Ctrl Pts',(-0.297520225844884,0.520881689320052,
-3.74632699872441));
#63588=CARTESIAN_POINT('Ctrl Pts',(-0.205326819166806,0.563628349727214,
-3.75096354203967));
#63589=CARTESIAN_POINT('Ctrl Pts',(-0.108527569532848,0.58168850920162,
-3.75560008535492));
#63590=CARTESIAN_POINT('Ctrl Pts',(-0.0117283198988895,0.599748668676025,
-3.76023662867017));
#63591=CARTESIAN_POINT('Ctrl Pts',(0.0896767726909481,0.593122327217673,
-3.76487317198543));
#63592=CARTESIAN_POINT('Ctrl Pts',(0.183302615594723,0.562618792667065,
-3.76950971530068));
#63593=CARTESIAN_POINT('Ctrl Pts',(0.276928458498497,0.532115258116456,
-3.77414625861593));
#63594=CARTESIAN_POINT('Ctrl Pts',(0.362775051716209,0.477734530473591,
-3.77878280193118));
#63595=CARTESIAN_POINT('Ctrl Pts',(0.430357537219162,0.406118388435549,
-3.78341934524644));
#63596=CARTESIAN_POINT('Ctrl Pts',(0.497940022722115,0.334502246397506,
-3.78805588856169));
#63597=CARTESIAN_POINT('Ctrl Pts',(0.547258400510309,0.245650689964286,
-3.79269243187695));
#63598=CARTESIAN_POINT('Ctrl Pts',(0.572289179306194,0.150415591036874,
-3.7973289751922));
#63599=CARTESIAN_POINT('Ctrl Pts',(0.597319958102079,0.0551804921094613,
-3.80196551850745));
#63600=CARTESIAN_POINT('Ctrl Pts',(0.598063137905655,-0.0464381493121438,
-3.8066020618227));
#63601=CARTESIAN_POINT('Ctrl Pts',(0.574427950870245,-0.142029165052077,
-3.81123860513796));
#63602=CARTESIAN_POINT('Ctrl Pts',(0.550792763834835,-0.237620180792009,
-3.81587514845321));
#63603=CARTESIAN_POINT('Ctrl Pts',(0.502779209960441,-0.327183570850269,
-3.82051169176847));
#63604=CARTESIAN_POINT('Ctrl Pts',(0.436251415392235,-0.399780514746208,
-3.82514823508372));
#63605=CARTESIAN_POINT('Ctrl Pts',(0.369723620824028,-0.472377458642147,
-3.82978477839897));
#63606=CARTESIAN_POINT('Ctrl Pts',(0.284681585562009,-0.528007956375765,
-3.83442132171422));
#63607=CARTESIAN_POINT('Ctrl Pts',(0.191511904253478,-0.559877610775289,
-3.83905786502948));
#63608=CARTESIAN_POINT('Ctrl Pts',(0.0983422229449468,-0.591747265174813,
-3.84369440834473));
#63609=CARTESIAN_POINT('Ctrl Pts',(-0.00295510441009569,-0.599856076240243,
-3.84833095165998));
#63610=CARTESIAN_POINT('Ctrl Pts',(-0.100008149214248,-0.583213629709318,
-3.85296749497523));
#63611=CARTESIAN_POINT('Ctrl Pts',(-0.1970611940184,-0.566571183178393,
-3.85760403829049));
#63612=CARTESIAN_POINT('Ctrl Pts',(-0.289869956271661,-0.525177479051112,
-3.86224058160574));
#63613=CARTESIAN_POINT('Ctrl Pts',(-0.367099250476545,-0.464088219954072,
-3.86687712492099));
#63614=CARTESIAN_POINT('Ctrl Pts',(-0.444328544681429,-0.402998960857032,
-3.87151366823625));
#63615=CARTESIAN_POINT('Ctrl Pts',(-0.505978370837935,-0.322214146790233,
-3.8761502115515));
#63616=CARTESIAN_POINT('Ctrl Pts',(-0.544519146695237,-0.231600240348692,
-3.88078675486675));
#63617=CARTESIAN_POINT('Ctrl Pts',(-0.575554096476506,-0.158633415645678,
-3.88452033017101));
#63618=CARTESIAN_POINT('Ctrl Pts',(-0.591604510735713,-0.0792931406306882,
-3.88825390547526));
#63619=CARTESIAN_POINT('Ctrl Pts',(-0.591686266410893,1.49359204264163E-5,
-3.89198748077951));
#63620=CARTESIAN_POINT('Ctrl Pts',(-0.591672685651915,9.86808882838178E-6,
-3.91716251922049));
#63621=CARTESIAN_POINT('Ctrl Pts',(-0.591596053141098,-0.074811541676493,
-3.9136403828679));
#63622=CARTESIAN_POINT('Ctrl Pts',(-0.577354221098841,-0.149656059400805,
-3.91011824651531));
#63623=CARTESIAN_POINT('Ctrl Pts',(-0.549651763576913,-0.219137766588835,
-3.90659611016272));
#63624=CARTESIAN_POINT('Ctrl Pts',(-0.513184224736479,-0.310603545521029,
-3.90195956684747));
#63625=CARTESIAN_POINT('Ctrl Pts',(-0.453390617001303,-0.392776049915004,
-3.89732302353222));
#63626=CARTESIAN_POINT('Ctrl Pts',(-0.377572641459037,-0.455609324446237,
-3.89268648021696));
#63627=CARTESIAN_POINT('Ctrl Pts',(-0.301754665916771,-0.518442598977469,
-3.88804993690171));
#63628=CARTESIAN_POINT('Ctrl Pts',(-0.209912322567414,-0.56193664364596,
-3.88341339358646));
#63629=CARTESIAN_POINT('Ctrl Pts',(-0.113263366397263,-0.580784325059894,
-3.8787768502712));
#63630=CARTESIAN_POINT('Ctrl Pts',(-0.0166144102271124,-0.599632006473828,
-3.87414030695595));
#63631=CARTESIAN_POINT('Ctrl Pts',(0.0848411587638334,-0.593833324633207,
-3.8695037636407));
#63632=CARTESIAN_POINT('Ctrl Pts',(0.17871239403648,-0.56409394180932,-3.86486722032545));
#63633=CARTESIAN_POINT('Ctrl Pts',(0.272583629309127,-0.534354558985432,
-3.86023067701019));
#63634=CARTESIAN_POINT('Ctrl Pts',(0.358870530863474,-0.48067447517828,
-3.85559413369494));
#63635=CARTESIAN_POINT('Ctrl Pts',(0.427034304402794,-0.409611207177925,
-3.85095759037968));
#63636=CARTESIAN_POINT('Ctrl Pts',(0.495198077942114,-0.33854793917757,
-3.84632104706443));
#63637=CARTESIAN_POINT('Ctrl Pts',(0.545238723466406,-0.250101486984014,
-3.84168450374918));
#63638=CARTESIAN_POINT('Ctrl Pts',(0.571044617305461,-0.155073571731536,
-3.83704796043393));
#63639=CARTESIAN_POINT('Ctrl Pts',(0.596850511144516,-0.0600456564790578,
-3.83241141711867));
#63640=CARTESIAN_POINT('Ctrl Pts',(0.598421653298335,0.0415637218323413,
-3.82777487380342));
#63641=CARTESIAN_POINT('Ctrl Pts',(0.5755661108858,0.137344177102385,-3.82313833048817));
#63642=CARTESIAN_POINT('Ctrl Pts',(0.552710568473265,0.233124632372429,
-3.81850178717291));
#63643=CARTESIAN_POINT('Ctrl Pts',(0.505428341494376,0.323076164601118,
-3.81386524385766));
#63644=CARTESIAN_POINT('Ctrl Pts',(0.439494257526417,0.396212735327201,
-3.80922870054241));
#63645=CARTESIAN_POINT('Ctrl Pts',(0.373560173558458,0.469349306053284,
-3.80459215722716));
#63646=CARTESIAN_POINT('Ctrl Pts',(0.288974232601431,0.525670915276761,
-3.7999556139119));
#63647=CARTESIAN_POINT('Ctrl Pts',(0.196067312291794,0.558298643565172,
-3.79531907059665));
#63648=CARTESIAN_POINT('Ctrl Pts',(0.103160391982157,0.590926371853582,
-3.7906825272814));
#63649=CARTESIAN_POINT('Ctrl Pts',(0.00193249231991062,0.599860219206927,
-3.78604598396614));
#63650=CARTESIAN_POINT('Ctrl Pts',(-0.0952529299216813,0.584009097814957,
-3.78140944065089));
#63651=CARTESIAN_POINT('Ctrl Pts',(-0.192438352163274,0.568157976422986,
-3.77677289733564));
#63652=CARTESIAN_POINT('Ctrl Pts',(-0.285581296984212,0.527521886285701,
-3.77213635402039));
#63653=CARTESIAN_POINT('Ctrl Pts',(-0.363305770565049,0.467063885351627,
-3.76749981070513));
#63654=CARTESIAN_POINT('Ctrl Pts',(-0.441030244145885,0.406605884417554,
-3.76286326738988));
#63655=CARTESIAN_POINT('Ctrl Pts',(-0.503336246486619,0.326325972686693,
-3.75822672407463));
#63656=CARTESIAN_POINT('Ctrl Pts',(-0.542614043818136,0.236029134685033,
-3.75359018075937));
#63657=CARTESIAN_POINT('Ctrl Pts',(-0.574883297252459,0.161844436261137,
-3.74978096024641));
#63658=CARTESIAN_POINT('Ctrl Pts',(-0.591609234805437,0.0808986268811383,
-3.74597173973345));
#63659=CARTESIAN_POINT('Ctrl Pts',(-0.591691313069437,-1.42991252893039E-5,
-3.74216251922049));
#63660=CARTESIAN_POINT('Origin',(0.,0.,-1.97));
#63661=CARTESIAN_POINT('',(-0.591640224643815,1.16845008508032E-5,-3.54198748077951));
#63662=CARTESIAN_POINT('',(-0.591631758215553,8.49683898327695E-6,-3.56716251922049));
#63663=CARTESIAN_POINT('',(-0.591675,-7.2459289488551E-17,-1.97));
#63664=CARTESIAN_POINT('Ctrl Pts',(-0.591640224643815,1.16845008508032E-5,
-3.54198748077951));
#63665=CARTESIAN_POINT('Ctrl Pts',(-0.59166519960911,0.0351971653384486,
-3.54364353257585));
#63666=CARTESIAN_POINT('Ctrl Pts',(-0.588577633489791,0.0703783135634807,
-3.54529958437219));
#63667=CARTESIAN_POINT('Ctrl Pts',(-0.582337221164469,0.104991027297213,
-3.54695563616854));
#63668=CARTESIAN_POINT('Ctrl Pts',(-0.564865580413074,0.201898229619839,
-3.55159217948379));
#63669=CARTESIAN_POINT('Ctrl Pts',(-0.522679908086348,0.294349677665667,
-3.55622872279904));
#63670=CARTESIAN_POINT('Ctrl Pts',(-0.460932543627806,0.371053830584308,
-3.5608652661143));
#63671=CARTESIAN_POINT('Ctrl Pts',(-0.399185179169264,0.44775798350295,
-3.56550180942955));
#63672=CARTESIAN_POINT('Ctrl Pts',(-0.317876122578908,0.508714841294403,
-3.5701383527448));
#63673=CARTESIAN_POINT('Ctrl Pts',(-0.226936040746222,0.546479449180746,
-3.57477489606005));
#63674=CARTESIAN_POINT('Ctrl Pts',(-0.135995958913538,0.584244057067088,
-3.57941143937531));
#63675=CARTESIAN_POINT('Ctrl Pts',(-0.0354248518385249,0.598816415048318,
-3.58404798269056));
#63676=CARTESIAN_POINT('Ctrl Pts',(0.0624940465446171,0.588416730823486,
-3.58868452600582));
#63677=CARTESIAN_POINT('Ctrl Pts',(0.16041294492776,0.578017046598654,-3.59332106932107));
#63678=CARTESIAN_POINT('Ctrl Pts',(0.255679634619035,0.542645320167759,
-3.59795761263632));
#63679=CARTESIAN_POINT('Ctrl Pts',(0.336658735739967,0.486621670927618,
-3.60259415595157));
#63680=CARTESIAN_POINT('Ctrl Pts',(0.417637836860899,0.430598021687478,
-3.60723069926683));
#63681=CARTESIAN_POINT('Ctrl Pts',(0.48432934941149,0.353922449638093,-3.61186724258208));
#63682=CARTESIAN_POINT('Ctrl Pts',(0.528587917594161,0.265959711873829,
-3.61650378589733));
#63683=CARTESIAN_POINT('Ctrl Pts',(0.572846485776831,0.177996974109566,
-3.62114032921259));
#63684=CARTESIAN_POINT('Ctrl Pts',(0.594672109591582,0.0787470706304238,
-3.62577687252784));
#63685=CARTESIAN_POINT('Ctrl Pts',(0.591399120429623,-0.0196681295900901,
-3.63041341584309));
#63686=CARTESIAN_POINT('Ctrl Pts',(0.588126131267663,-0.118083329810605,
-3.63504995915834));
#63687=CARTESIAN_POINT('Ctrl Pts',(0.559754529128993,-0.215663826772493,
-3.6396865024736));
#63688=CARTESIAN_POINT('Ctrl Pts',(0.509749474498588,-0.300491644167661,
-3.64432304578885));
#63689=CARTESIAN_POINT('Ctrl Pts',(0.459744419868183,-0.38531946156283,
-3.6489595891041));
#63690=CARTESIAN_POINT('Ctrl Pts',(0.388105912746044,-0.45739459939128,
-3.65359613241935));
#63691=CARTESIAN_POINT('Ctrl Pts',(0.303583509214952,-0.507914173753984,
-3.65823267573461));
#63692=CARTESIAN_POINT('Ctrl Pts',(0.21906110568386,-0.558433748116688,
-3.66286921904986));
#63693=CARTESIAN_POINT('Ctrl Pts',(0.121654805743816,-0.587397759013646,
-3.66750576236512));
#63694=CARTESIAN_POINT('Ctrl Pts',(0.0232613101835599,-0.591268692231257,
-3.67214230568037));
#63695=CARTESIAN_POINT('Ctrl Pts',(-0.0751321853766959,-0.595139625448867,
-3.67677884899562));
#63696=CARTESIAN_POINT('Ctrl Pts',(-0.174512876557163,-0.573917480987128,
-3.68141539231087));
#63697=CARTESIAN_POINT('Ctrl Pts',(-0.262742920653841,-0.53019422159853,
-3.68605193562613));
#63698=CARTESIAN_POINT('Ctrl Pts',(-0.350972964750519,-0.486470962209931,
-3.69068847894138));
#63699=CARTESIAN_POINT('Ctrl Pts',(-0.428052361763407,-0.420246587894471,
-3.69532502225664));
#63700=CARTESIAN_POINT('Ctrl Pts',(-0.484567033507559,-0.339609400635107,
-3.69996156557189));
#63701=CARTESIAN_POINT('Ctrl Pts',(-0.541081705251711,-0.258972213375742,
-3.70459810888714));
#63702=CARTESIAN_POINT('Ctrl Pts',(-0.577031651727126,-0.163922213172471,
-3.70923465220239));
#63703=CARTESIAN_POINT('Ctrl Pts',(-0.588026132739526,-0.0660683145156767,
-3.71387119551764));
#63704=CARTESIAN_POINT('Ctrl Pts',(-0.59048931395099,-0.0441453256662729,
-3.7149099572716));
#63705=CARTESIAN_POINT('Ctrl Pts',(-0.591699905180646,-0.022081600707655,
-3.71594871902555));
#63706=CARTESIAN_POINT('Ctrl Pts',(-0.591677080768459,-1.5385395483597E-5,
-3.71698748077951));
#63707=CARTESIAN_POINT('Ctrl Pts',(-0.591691313069437,-1.42991252893039E-5,
-3.74216251922049));
#63708=CARTESIAN_POINT('Ctrl Pts',(-0.591709139608791,-0.0175877392707435,
-3.7413351964182));
#63709=CARTESIAN_POINT('Ctrl Pts',(-0.590941853822676,-0.0351596282650225,
-3.74050787361591));
#63710=CARTESIAN_POINT('Ctrl Pts',(-0.589378180522454,-0.0526603608866166,
-3.73968055081362));
#63711=CARTESIAN_POINT('Ctrl Pts',(-0.580614927572954,-0.150739254184145,
-3.73504400749836));
#63712=CARTESIAN_POINT('Ctrl Pts',(-0.546838829351652,-0.24658327650674,
-3.73040746418311));
#63713=CARTESIAN_POINT('Ctrl Pts',(-0.492175123108772,-0.328486532400379,
-3.72577092086785));
#63714=CARTESIAN_POINT('Ctrl Pts',(-0.437511416865892,-0.410389788294018,
-3.7211343775526));
#63715=CARTESIAN_POINT('Ctrl Pts',(-0.361960102601434,-0.4783522777587,
-3.71649783423735));
#63716=CARTESIAN_POINT('Ctrl Pts',(-0.274748626586135,-0.524073416078952,
-3.7118612909221));
#63717=CARTESIAN_POINT('Ctrl Pts',(-0.187537150570835,-0.569794554399205,
-3.70722474760684));
#63718=CARTESIAN_POINT('Ctrl Pts',(-0.0886655128046928,-0.593274341575028,
-3.70258820429159));
#63719=CARTESIAN_POINT('Ctrl Pts',(0.00979061725475591,-0.591645077227593,
-3.69795166097634));
#63720=CARTESIAN_POINT('Ctrl Pts',(0.108246747314204,-0.590015812880158,
-3.69331511766108));
#63721=CARTESIAN_POINT('Ctrl Pts',(0.206287369666958,-0.563277497009465,
-3.68867857434583));
#63722=CARTESIAN_POINT('Ctrl Pts',(0.291938310620198,-0.514695809401822,
-3.68404203103058));
#63723=CARTESIAN_POINT('Ctrl Pts',(0.377589251573439,-0.466114121794178,
-3.67940548771533));
#63724=CARTESIAN_POINT('Ctrl Pts',(0.450850511127164,-0.395689062449585,
-3.67476894440007));
#63725=CARTESIAN_POINT('Ctrl Pts',(0.502774338650679,-0.312021983009729,
-3.67013240108482));
#63726=CARTESIAN_POINT('Ctrl Pts',(0.554698166174194,-0.228354903569872,
-3.66549585776957));
#63727=CARTESIAN_POINT('Ctrl Pts',(0.585284561667497,-0.131445804034753,
-3.66085931445431));
#63728=CARTESIAN_POINT('Ctrl Pts',(0.590797861247265,-0.0331306598224494,
-3.65622277113906));
#63729=CARTESIAN_POINT('Ctrl Pts',(0.596311160827033,0.0651844843898538,
-3.65158622782381));
#63730=CARTESIAN_POINT('Ctrl Pts',(0.576751364493266,0.164905673279341,
-3.64694968450856));
#63731=CARTESIAN_POINT('Ctrl Pts',(0.534507404432907,0.253853477572184,
-3.6423131411933));
#63732=CARTESIAN_POINT('Ctrl Pts',(0.492263444372549,0.342801281865026,
-3.63767659787805));
#63733=CARTESIAN_POINT('Ctrl Pts',(0.427335320585598,0.420975701561225,
-3.6330400545628));
#63734=CARTESIAN_POINT('Ctrl Pts',(0.347653017699086,0.478828918051121,
-3.62840351124754));
#63735=CARTESIAN_POINT('Ctrl Pts',(0.267970714812574,0.536682134541016,
-3.62376696793229));
#63736=CARTESIAN_POINT('Ctrl Pts',(0.173534232826499,0.574214147824609,
-3.61913042461704));
#63737=CARTESIAN_POINT('Ctrl Pts',(0.0758775543535335,0.586840992277037,
-3.61449388130178));
#63738=CARTESIAN_POINT('Ctrl Pts',(-0.0217791241194331,0.599467836729464,
-3.60985733798653));
#63739=CARTESIAN_POINT('Ctrl Pts',(-0.122655999079291,0.587189512350725,
-3.60522079467128));
#63740=CARTESIAN_POINT('Ctrl Pts',(-0.214432491687569,0.551505630055761,
-3.60058425135602));
#63741=CARTESIAN_POINT('Ctrl Pts',(-0.306208984295846,0.515821747760798,
-3.59594770804077));
#63742=CARTESIAN_POINT('Ctrl Pts',(-0.388885094552543,0.456732307549611,
-3.59131116472552));
#63743=CARTESIAN_POINT('Ctrl Pts',(-0.452363190715939,0.381454187496397,
-3.58667462141027));
#63744=CARTESIAN_POINT('Ctrl Pts',(-0.515841286879337,0.306176067443183,
-3.58203807809501));
#63745=CARTESIAN_POINT('Ctrl Pts',(-0.560121368949433,0.214709267547942,
-3.57740153477976));
#63746=CARTESIAN_POINT('Ctrl Pts',(-0.579795297128556,0.118225068835626,
-3.57276499146451));
#63747=CARTESIAN_POINT('Ctrl Pts',(-0.587719493313795,0.0793634997371216,
-3.5708975007165));
#63748=CARTESIAN_POINT('Ctrl Pts',(-0.591651859745899,0.0396879634509739,
-3.5690300099685));
#63749=CARTESIAN_POINT('Ctrl Pts',(-0.591631758215553,8.49683898327695E-6,
-3.56716251922049));
#63750=CARTESIAN_POINT('Origin',(0.,0.,-1.97));
#63751=CARTESIAN_POINT('',(-0.591720711673068,-6.25964164063797E-6,-3.36698748077951));
#63752=CARTESIAN_POINT('',(-0.591725682421883,-1.68028488189446E-6,-3.39216251922049));
#63753=CARTESIAN_POINT('',(-0.591675,-7.2459289488551E-17,-1.97));
#63754=CARTESIAN_POINT('Ctrl Pts',(-0.591720711673068,-6.25964164063797E-6,
-3.36698748077951));
#63755=CARTESIAN_POINT('Ctrl Pts',(-0.591670632807954,0.0923986416864466,
-3.37133834612615));
#63756=CARTESIAN_POINT('Ctrl Pts',(-0.569664035056796,0.18482655914794,
-3.37568921147279));
#63757=CARTESIAN_POINT('Ctrl Pts',(-0.527928364019782,0.267266528824463,
-3.38004007681943));
#63758=CARTESIAN_POINT('Ctrl Pts',(-0.483452327384057,0.355119509751242,
-3.38467662013468));
#63759=CARTESIAN_POINT('Ctrl Pts',(-0.416571337426255,0.431629864460194,
-3.38931316344994));
#63760=CARTESIAN_POINT('Ctrl Pts',(-0.335453891732765,0.487453014646359,
-3.39394970676519));
#63761=CARTESIAN_POINT('Ctrl Pts',(-0.254336446039275,0.543276164832523,
-3.39858625008044));
#63762=CARTESIAN_POINT('Ctrl Pts',(-0.158982544610098,0.578412110495901,
-3.40322279339569));
#63763=CARTESIAN_POINT('Ctrl Pts',(-0.0610382189134935,0.588569529281247,
-3.40785933671095));
#63764=CARTESIAN_POINT('Ctrl Pts',(0.036906106783112,0.598726948066594,
-3.4124958800262));
#63765=CARTESIAN_POINT('Ctrl Pts',(0.137440856747144,0.583905839973908,
-3.41713242334146));
#63766=CARTESIAN_POINT('Ctrl Pts',(0.22828723751356,0.545916378353781,-3.42176896665671));
#63767=CARTESIAN_POINT('Ctrl Pts',(0.319133618279975,0.507926916733654,
-3.42640550997196));
#63768=CARTESIAN_POINT('Ctrl Pts',(0.400291629848773,0.446769101586084,
-3.43104205328721));
#63769=CARTESIAN_POINT('Ctrl Pts',(0.461849053186801,0.369912431579334,
-3.43567859660246));
#63770=CARTESIAN_POINT('Ctrl Pts',(0.523406476524829,0.293055761572585,
-3.44031513991772));
#63771=CARTESIAN_POINT('Ctrl Pts',(0.565363311632086,0.200500236706655,
-3.44495168323297));
#63772=CARTESIAN_POINT('Ctrl Pts',(0.582595168057379,0.103550109235457,
-3.44958822654822));
#63773=CARTESIAN_POINT('Ctrl Pts',(0.599827024482672,0.00659998176425772,
-3.45422476986348));
#63774=CARTESIAN_POINT('Ctrl Pts',(0.592333902226001,-0.0947447483122083,
-3.45886131317873));
#63775=CARTESIAN_POINT('Ctrl Pts',(0.561030972416062,-0.188106360754677,
-3.46349785649398));
#63776=CARTESIAN_POINT('Ctrl Pts',(0.529728042606125,-0.281467973197144,
-3.46813439980924));
#63777=CARTESIAN_POINT('Ctrl Pts',(0.474615305242921,-0.366846468005612,
-3.47277094312449));
#63778=CARTESIAN_POINT('Ctrl Pts',(0.402423944515183,-0.43381415819141,
-3.47740748643974));
#63779=CARTESIAN_POINT('Ctrl Pts',(0.330232583787443,-0.500781848377208,
-3.482044029755));
#63780=CARTESIAN_POINT('Ctrl Pts',(0.240962599695169,-0.549338733940336,
-3.48668057307025));
#63781=CARTESIAN_POINT('Ctrl Pts',(0.145516965565382,-0.57355432846342,
-3.4913171163855));
#63782=CARTESIAN_POINT('Ctrl Pts',(0.0500713314355945,-0.597769922986504,
-3.49595365970075));
#63783=CARTESIAN_POINT('Ctrl Pts',(-0.0515499527317057,-0.597644226469546,
-3.50059020301601));
#63784=CARTESIAN_POINT('Ctrl Pts',(-0.146935389813492,-0.573192590833864,
-3.50522674633126));
#63785=CARTESIAN_POINT('Ctrl Pts',(-0.242320826895278,-0.548740955198182,
-3.50986328964651));
#63786=CARTESIAN_POINT('Ctrl Pts',(-0.331470416891551,-0.499963380443776,
-3.51449983296176));
#63787=CARTESIAN_POINT('Ctrl Pts',(-0.403495890786381,-0.43281730682239,
-3.51913637627702));
#63788=CARTESIAN_POINT('Ctrl Pts',(-0.475521364681212,-0.365671233201003,
-3.52377291959227));
#63789=CARTESIAN_POINT('Ctrl Pts',(-0.530422722474602,-0.280156660712634,
-3.52840946290753));
#63790=CARTESIAN_POINT('Ctrl Pts',(-0.561494596783265,-0.186717896168737,
-3.53304600622278));
#63791=CARTESIAN_POINT('Ctrl Pts',(-0.581468411661466,-0.126653010255906,
-3.53602649774169));
#63792=CARTESIAN_POINT('Ctrl Pts',(-0.591595275764553,-0.0633136459368033,
-3.5390069892606));
#63793=CARTESIAN_POINT('Ctrl Pts',(-0.591640224643815,1.16845008508032E-5,
-3.54198748077951));
#63794=CARTESIAN_POINT('Ctrl Pts',(-0.591631758215553,8.49683898327695E-6,
-3.56716251922049));
#63795=CARTESIAN_POINT('Ctrl Pts',(-0.591601952341403,-0.0588268837412697,
-3.56439346665324));
#63796=CARTESIAN_POINT('Ctrl Pts',(-0.582882265224252,-0.117670905521185,
-3.561624414086));
#63797=CARTESIAN_POINT('Ctrl Pts',(-0.565601016486239,-0.173882844534329,
-3.55885536151875));
#63798=CARTESIAN_POINT('Ctrl Pts',(-0.536665033376649,-0.268004961662577,
-3.55421881820349));
#63799=CARTESIAN_POINT('Ctrl Pts',(-0.483725292869318,-0.354747598389681,
-3.54958227488824));
#63800=CARTESIAN_POINT('Ctrl Pts',(-0.413247580575901,-0.423516458501507,
-3.54494573157299));
#63801=CARTESIAN_POINT('Ctrl Pts',(-0.342769868282486,-0.492285318613332,
-3.54030918825774));
#63802=CARTESIAN_POINT('Ctrl Pts',(-0.254754184202987,-0.54308040210988,
-3.53567264494248));
#63803=CARTESIAN_POINT('Ctrl Pts',(-0.159950307959673,-0.569697860674586,
-3.53103610162723));
#63804=CARTESIAN_POINT('Ctrl Pts',(-0.0651464317163584,-0.596315319239292,
-3.52639955831198));
#63805=CARTESIAN_POINT('Ctrl Pts',(0.0364456366907705,-0.598755152872157,
-3.52176301499672));
#63806=CARTESIAN_POINT('Ctrl Pts',(0.132417968400244,-0.576719372934783,
-3.51712647168147));
#63807=CARTESIAN_POINT('Ctrl Pts',(0.228390300109719,-0.554683592997408,
-3.51248992836622));
#63808=CARTESIAN_POINT('Ctrl Pts',(0.318742895121539,-0.508172199489795,
-3.50785338505096));
#63809=CARTESIAN_POINT('Ctrl Pts',(0.392440555620253,-0.442865853027787,
-3.50321684173571));
#63810=CARTESIAN_POINT('Ctrl Pts',(0.466138216118966,-0.37755950656578,
-3.49858029842046));
#63811=CARTESIAN_POINT('Ctrl Pts',(0.523180942104573,-0.293458207149378,
-3.49394375510521));
#63812=CARTESIAN_POINT('Ctrl Pts',(0.556601830577751,-0.20083365173957,
-3.48930721178995));
#63813=CARTESIAN_POINT('Ctrl Pts',(0.59002271905093,-0.10820909632976,-3.4846706684747));
#63814=CARTESIAN_POINT('Ctrl Pts',(0.599821770011678,-0.00706128492654368,
-3.48003412515945));
#63815=CARTESIAN_POINT('Ctrl Pts',(0.584802178146975,0.0902561128572957,
-3.4753975818442));
#63816=CARTESIAN_POINT('Ctrl Pts',(0.569782586282271,0.187573510641134,
-3.47076103852894));
#63817=CARTESIAN_POINT('Ctrl Pts',(0.529944351592118,0.281060494805596,
-3.46612449521369));
#63818=CARTESIAN_POINT('Ctrl Pts',(0.470153109649757,0.35929904948416,-3.46148795189844));
#63819=CARTESIAN_POINT('Ctrl Pts',(0.410361867707395,0.437537604162725,
-3.45685140858318));
#63820=CARTESIAN_POINT('Ctrl Pts',(0.330617618512825,0.500527729355392,
-3.45221486526793));
#63821=CARTESIAN_POINT('Ctrl Pts',(0.240659911487869,0.540576137538651,
-3.44757832195268));
#63822=CARTESIAN_POINT('Ctrl Pts',(0.150702204462913,0.580624545721909,
-3.44294177863742));
#63823=CARTESIAN_POINT('Ctrl Pts',(0.0505310396075721,0.597731236895759,
-3.43830523532217));
#63824=CARTESIAN_POINT('Ctrl Pts',(-0.0476191960144642,0.58980688843425,
-3.43366869200692));
#63825=CARTESIAN_POINT('Ctrl Pts',(-0.1457694316365,0.581882539972741,-3.42903214869166));
#63826=CARTESIAN_POINT('Ctrl Pts',(-0.24189873802523,0.548927151875873,
-3.42439560537641));
#63827=CARTESIAN_POINT('Ctrl Pts',(-0.324266379768199,0.494965724495729,
-3.41975906206116));
#63828=CARTESIAN_POINT('Ctrl Pts',(-0.406634021511169,0.441004297115584,
-3.41512251874591));
#63829=CARTESIAN_POINT('Ctrl Pts',(-0.475239998608377,0.366036830452165,
-3.41048597543065));
#63830=CARTESIAN_POINT('Ctrl Pts',(-0.521705132481815,0.279219462458633,
-3.4058494321154));
#63831=CARTESIAN_POINT('Ctrl Pts',(-0.567426279806072,0.193792189545821,
-3.4012871278171));
#63832=CARTESIAN_POINT('Ctrl Pts',(-0.591709933354533,0.0968914518041998,
-3.39672482351879));
#63833=CARTESIAN_POINT('Ctrl Pts',(-0.591725682421883,-1.68028488189446E-6,
-3.39216251922049));
#63834=CARTESIAN_POINT('Origin',(0.,0.,-1.97));
#63835=CARTESIAN_POINT('',(-0.591624439693044,-1.80568084665045E-6,-3.19198748077951));
#63836=CARTESIAN_POINT('',(-0.591627593882854,-5.87472452489096E-6,-3.21716251922049));
#63837=CARTESIAN_POINT('',(-0.591675,-7.2459289488551E-17,-1.97));
#63838=CARTESIAN_POINT('Ctrl Pts',(-0.591624439693044,-1.80568084665045E-6,
-3.19198748077951));
#63839=CARTESIAN_POINT('Ctrl Pts',(-0.591619011968859,0.0511880591375139,
-3.19439661636119));
#63840=CARTESIAN_POINT('Ctrl Pts',(-0.585043627760961,0.102379292407691,
-3.19680575194288));
#63841=CARTESIAN_POINT('Ctrl Pts',(-0.571915327198982,0.15183087130542,
-3.19921488752456));
#63842=CARTESIAN_POINT('Ctrl Pts',(-0.546649030576224,0.247003757925056,
-3.20385143083982));
#63843=CARTESIAN_POINT('Ctrl Pts',(-0.497111001113603,0.335733036251805,
-3.20848797415507));
#63844=CARTESIAN_POINT('Ctrl Pts',(-0.429351557060823,0.407181771959315,
-3.21312451747032));
#63845=CARTESIAN_POINT('Ctrl Pts',(-0.361592113008042,0.478630507666826,
-3.21776106078557));
#63846=CARTESIAN_POINT('Ctrl Pts',(-0.275611254365102,0.532798700755097,
-3.22239760410083));
#63847=CARTESIAN_POINT('Ctrl Pts',(-0.181910237718421,0.563070528779219,
-3.22703414741608));
#63848=CARTESIAN_POINT('Ctrl Pts',(-0.0882092210717391,0.59334235680334,
-3.23167069073133));
#63849=CARTESIAN_POINT('Ctrl Pts',(0.0132119535786834,0.599717819763311,
-3.23630723404658));
#63850=CARTESIAN_POINT('Ctrl Pts',(0.109966229449395,0.581418251646062,
-3.24094377736184));
#63851=CARTESIAN_POINT('Ctrl Pts',(0.206720505320107,0.563118683528813,
-3.24558032067709));
#63852=CARTESIAN_POINT('Ctrl Pts',(0.298807882411109,0.520144084334345,
-3.25021686399235));
#63853=CARTESIAN_POINT('Ctrl Pts',(0.374981285612127,0.457743148946173,
-3.2548534073076));
#63854=CARTESIAN_POINT('Ctrl Pts',(0.451154688813143,0.395342213558001,
-3.25948995062285));
#63855=CARTESIAN_POINT('Ctrl Pts',(0.511414118124177,0.313514941976128,
-3.2641264939381));
#63856=CARTESIAN_POINT('Ctrl Pts',(0.548399799068281,0.222255293184099,
-3.26876303725335));
#63857=CARTESIAN_POINT('Ctrl Pts',(0.585385480012385,0.130995644392071,
-3.27339958056861));
#63858=CARTESIAN_POINT('Ctrl Pts',(0.599097412589559,0.0303036183898887,
-3.27803612388387));
#63859=CARTESIAN_POINT('Ctrl Pts',(0.587860892399763,-0.0675227824769924,
-3.28267266719912));
#63860=CARTESIAN_POINT('Ctrl Pts',(0.576624372209967,-0.165349183343875,
-3.28730921051437));
#63861=CARTESIAN_POINT('Ctrl Pts',(0.5404393992532,-0.260309959075456,-3.29194575382962));
#63862=CARTESIAN_POINT('Ctrl Pts',(0.483725418643049,-0.340807092539295,
-3.29658229714487));
#63863=CARTESIAN_POINT('Ctrl Pts',(0.427011438032899,-0.421304226003134,
-3.30121884046013));
#63864=CARTESIAN_POINT('Ctrl Pts',(0.349768449769366,-0.487337717199232,
-3.30585538377538));
#63865=CARTESIAN_POINT('Ctrl Pts',(0.261430512223809,-0.530842577648852,
-3.31049192709064));
#63866=CARTESIAN_POINT('Ctrl Pts',(0.173092574678252,-0.574347438098472,
-3.31512847040589));
#63867=CARTESIAN_POINT('Ctrl Pts',(0.073659687850671,-0.595323667801614,
-3.31976501372114));
#63868=CARTESIAN_POINT('Ctrl Pts',(-0.0247239306483499,-0.591209338745403,
-3.32440155703639));
#63869=CARTESIAN_POINT('Ctrl Pts',(-0.123107549147369,-0.587095009689192,
-3.32903810035165));
#63870=CARTESIAN_POINT('Ctrl Pts',(-0.220441899317829,-0.557890121873629,
-3.3336746436669));
#63871=CARTESIAN_POINT('Ctrl Pts',(-0.304839067943404,-0.507161608978714,
-3.33831118698215));
#63872=CARTESIAN_POINT('Ctrl Pts',(-0.389236236568979,-0.456433096083798,
-3.34294773029741));
#63873=CARTESIAN_POINT('Ctrl Pts',(-0.46069622364967,-0.38418095810953,
-3.34758427361266));
#63874=CARTESIAN_POINT('Ctrl Pts',(-0.510491276615423,-0.299229696831776,
-3.35222081692791));
#63875=CARTESIAN_POINT('Ctrl Pts',(-0.560286329581176,-0.214278435554019,
-3.35685736024317));
#63876=CARTESIAN_POINT('Ctrl Pts',(-0.58841644843199,-0.116628050972775,
-3.36149390355842));
#63877=CARTESIAN_POINT('Ctrl Pts',(-0.591445966200572,-0.0182050551098478,
-3.36613044687367));
#63878=CARTESIAN_POINT('Ctrl Pts',(-0.591632628207839,-0.012140778425441,
-3.36641612484229));
#63879=CARTESIAN_POINT('Ctrl Pts',(-0.591723999853077,-0.00607356864757978,
-3.3667018028109));
#63880=CARTESIAN_POINT('Ctrl Pts',(-0.591720711673068,-6.25964164063797E-6,
-3.36698748077951));
#63881=CARTESIAN_POINT('Ctrl Pts',(-0.591725682421883,-1.68028488189446E-6,
-3.39216251922049));
#63882=CARTESIAN_POINT('Ctrl Pts',(-0.591725938694854,-0.00157835084546417,
-3.39208828020354));
#63883=CARTESIAN_POINT('Ctrl Pts',(-0.591719769153025,-0.00315501939217195,
-3.39201404118659));
#63884=CARTESIAN_POINT('Ctrl Pts',(-0.591707161601071,-0.0047316364567862,
-3.39193980216964));
#63885=CARTESIAN_POINT('Ctrl Pts',(-0.590919766197223,-0.10319809805503,
-3.38730325885439));
#63886=CARTESIAN_POINT('Ctrl Pts',(-0.565020684739859,-0.201463751927878,
-3.38266671553913));
#63887=CARTESIAN_POINT('Ctrl Pts',(-0.517173096848594,-0.287526940250111,
-3.37803017222388));
#63888=CARTESIAN_POINT('Ctrl Pts',(-0.469325508957329,-0.373590128572344,
-3.37339362890863));
#63889=CARTESIAN_POINT('Ctrl Pts',(-0.399529414632163,-0.447450851343963,
-3.36875708559337));
#63890=CARTESIAN_POINT('Ctrl Pts',(-0.316309347203035,-0.500088142576432,
-3.36412054227812));
#63891=CARTESIAN_POINT('Ctrl Pts',(-0.233089279773905,-0.552725433808902,
-3.35948399896287));
#63892=CARTESIAN_POINT('Ctrl Pts',(-0.136445239240813,-0.584139293502221,
-3.35484745564762));
#63893=CARTESIAN_POINT('Ctrl Pts',(-0.0381808279776381,-0.590492995596474,
-3.35021091233237));
#63894=CARTESIAN_POINT('Ctrl Pts',(0.0600835832855345,-0.596846697690727,
-3.34557436901711));
#63895=CARTESIAN_POINT('Ctrl Pts',(0.159968365278788,-0.578140242185915,
-3.34093782570186));
#63896=CARTESIAN_POINT('Ctrl Pts',(0.249274108257385,-0.536658338634592,
-3.3363012823866));
#63897=CARTESIAN_POINT('Ctrl Pts',(0.338579851235984,-0.495176435083269,
-3.33166473907135));
#63898=CARTESIAN_POINT('Ctrl Pts',(0.417306555199926,-0.430919083485436,
-3.3270281957561));
#63899=CARTESIAN_POINT('Ctrl Pts',(0.475838948429704,-0.351734343831918,
-3.32239165244085));
#63900=CARTESIAN_POINT('Ctrl Pts',(0.53437134165948,-0.272549604178401,
-3.31775510912559));
#63901=CARTESIAN_POINT('Ctrl Pts',(0.572709424155094,-0.1784374764692,-3.31311856581034));
#63902=CARTESIAN_POINT('Ctrl Pts',(0.586170781159679,-0.0808923283643585,
-3.30848202249509));
#63903=CARTESIAN_POINT('Ctrl Pts',(0.599632138164264,0.0166528197404849,
-3.30384547917983));
#63904=CARTESIAN_POINT('Ctrl Pts',(0.58821676967782,0.11763098824097,-3.29920893586458));
#63905=CARTESIAN_POINT('Ctrl Pts',(0.553318889661415,0.209709226829473,
-3.29457239254933));
#63906=CARTESIAN_POINT('Ctrl Pts',(0.518421009645009,0.301787465417976,
-3.28993584923408));
#63907=CARTESIAN_POINT('Ctrl Pts',(0.460040618098642,0.384965774094497,
-3.28529930591882));
#63908=CARTESIAN_POINT('Ctrl Pts',(0.385307993562448,0.449085185204808,
-3.28066276260357));
#63909=CARTESIAN_POINT('Ctrl Pts',(0.310575369026254,0.513204596315118,
-3.27602621928831));
#63910=CARTESIAN_POINT('Ctrl Pts',(0.219490511500231,0.558265109859217,
-3.27138967597306));
#63911=CARTESIAN_POINT('Ctrl Pts',(0.123178053549291,0.578763268182565,
-3.26675313265781));
#63912=CARTESIAN_POINT('Ctrl Pts',(0.0268655955983512,0.599261426505914,
-3.26211658934256));
#63913=CARTESIAN_POINT('Ctrl Pts',(-0.0746744627775051,0.595197229608512,
-3.2574800460273));
#63914=CARTESIAN_POINT('Ctrl Pts',(-0.169040544952571,0.567067057441793,
-3.25284350271205));
#63915=CARTESIAN_POINT('Ctrl Pts',(-0.263406627127637,0.538936885275074,
-3.2482069593968));
#63916=CARTESIAN_POINT('Ctrl Pts',(-0.350598733101911,0.486740737839038,
-3.24357041608154));
#63917=CARTESIAN_POINT('Ctrl Pts',(-0.419967670815699,0.416853582140291,
-3.23893387276629));
#63918=CARTESIAN_POINT('Ctrl Pts',(-0.489336608529489,0.346966426441542,
-3.23429732945104));
#63919=CARTESIAN_POINT('Ctrl Pts',(-0.540882377982793,0.259388262480081,
-3.22966078613579));
#63920=CARTESIAN_POINT('Ctrl Pts',(-0.568309445966046,0.164815433437894,
-3.22502424282053));
#63921=CARTESIAN_POINT('Ctrl Pts',(-0.583811226278298,0.111362865331991,
-3.22240366828719));
#63922=CARTESIAN_POINT('Ctrl Pts',(-0.591608260843235,0.0556758437625984,
-3.21978309375384));
#63923=CARTESIAN_POINT('Ctrl Pts',(-0.591627593882854,-5.87472452489096E-6,
-3.21716251922049));
#63924=CARTESIAN_POINT('Origin',(0.,0.,-1.97));
#63925=CARTESIAN_POINT('',(-0.591712848140847,9.68948221328342E-6,-3.01698748077951));
#63926=CARTESIAN_POINT('',(-0.591700856122533,1.27964970961225E-5,-3.04216251922049));
#63927=CARTESIAN_POINT('',(-0.591675,-7.2459289488551E-17,-1.97));
#63928=CARTESIAN_POINT('Ctrl Pts',(-0.591712848140847,9.68948221328342E-6,
-3.01698748077951));
#63929=CARTESIAN_POINT('Ctrl Pts',(-0.591720547203392,0.0099369683863286,
-3.01745488659624));
#63930=CARTESIAN_POINT('Ctrl Pts',(-0.591475882675022,0.0198638677682085,
-3.01792229241297));
#63931=CARTESIAN_POINT('Ctrl Pts',(-0.5909763364076,0.0297779242515645,
-3.0183896982297));
#63932=CARTESIAN_POINT('Ctrl Pts',(-0.586020968237206,0.128122768645358,
-3.02302624154495));
#63933=CARTESIAN_POINT('Ctrl Pts',(-0.555984929782598,0.225203856347231,
-3.0276627848602));
#63934=CARTESIAN_POINT('Ctrl Pts',(-0.504536667156429,0.309164206306557,
-3.03229932817546));
#63935=CARTESIAN_POINT('Ctrl Pts',(-0.453088404530261,0.393124556265883,
-3.03693587149071));
#63936=CARTESIAN_POINT('Ctrl Pts',(-0.380227917732533,0.463964168482661,
-3.04157241480596));
#63937=CARTESIAN_POINT('Ctrl Pts',(-0.294854009112401,0.513031059758399,
-3.04620895812121));
#63938=CARTESIAN_POINT('Ctrl Pts',(-0.209480100492271,0.562097951034135,
-3.05084550143647));
#63939=CARTESIAN_POINT('Ctrl Pts',(-0.111592770049739,0.589392121368831,
-3.05548204475172));
#63940=CARTESIAN_POINT('Ctrl Pts',(-0.0131474691464297,0.591580002215698,
-3.06011858806697));
#63941=CARTESIAN_POINT('Ctrl Pts',(0.0852978317568821,0.593767883062565,
-3.06475513138223));
#63942=CARTESIAN_POINT('Ctrl Pts',(0.18430110312097,0.570849474421601,-3.06939167469748));
#63943=CARTESIAN_POINT('Ctrl Pts',(0.271770598342017,0.525623911978235,
-3.07402821801273));
#63944=CARTESIAN_POINT('Ctrl Pts',(0.359240093563065,0.480398349534868,
-3.07866476132798));
#63945=CARTESIAN_POINT('Ctrl Pts',(0.435175812641071,0.412865633289098,
-3.08330130464324));
#63946=CARTESIAN_POINT('Ctrl Pts',(0.49030336028971,0.331273859299371,-3.08793784795849));
#63947=CARTESIAN_POINT('Ctrl Pts',(0.545430907938349,0.249682085309644,
-3.09257439127375));
#63948=CARTESIAN_POINT('Ctrl Pts',(0.579750284157621,0.15403125357596,-3.097210934589));
#63949=CARTESIAN_POINT('Ctrl Pts',(0.589069898153335,0.0560036610955033,
-3.10184747790425));
#63950=CARTESIAN_POINT('Ctrl Pts',(0.598389512149049,-0.0420239313849538,
-3.1064840212195));
#63951=CARTESIAN_POINT('Ctrl Pts',(0.582709363921205,-0.142428284612183,
-3.11112056453476));
#63952=CARTESIAN_POINT('Ctrl Pts',(0.543944545531601,-0.232946531102958,
-3.11575710785001));
#63953=CARTESIAN_POINT('Ctrl Pts',(0.505179727141996,-0.323464777593732,
-3.12039365116526));
#63954=CARTESIAN_POINT('Ctrl Pts',(0.443330238590631,-0.404096917348053,
-3.12503019448051));
#63955=CARTESIAN_POINT('Ctrl Pts',(0.365950055951575,-0.464994958591511,
-3.12966673779577));
#63956=CARTESIAN_POINT('Ctrl Pts',(0.28856987331252,-0.525892999834967,
-3.13430328111102));
#63957=CARTESIAN_POINT('Ctrl Pts',(0.195658996585775,-0.567056942567562,
-3.13893982442627));
#63958=CARTESIAN_POINT('Ctrl Pts',(0.0985650788603642,-0.583459236104572,
-3.14357636774153));
#63959=CARTESIAN_POINT('Ctrl Pts',(0.00147116113495045,-0.599861529641583,
-3.14821291105678));
#63960=CARTESIAN_POINT('Ctrl Pts',(-0.0998057975891291,-0.591502173983006,
-3.15284945437203));
#63961=CARTESIAN_POINT('Ctrl Pts',(-0.192896354314448,-0.559402137517078,
-3.15748599768729));
#63962=CARTESIAN_POINT('Ctrl Pts',(-0.285986911039766,-0.52730210105115,
-3.16212254100254));
#63963=CARTESIAN_POINT('Ctrl Pts',(-0.370891065766324,-0.471461383777871,
-3.16675908431779));
#63964=CARTESIAN_POINT('Ctrl Pts',(-0.437239064945378,-0.398700081580343,
-3.17139562763305));
#63965=CARTESIAN_POINT('Ctrl Pts',(-0.503587064124432,-0.325938779382816,
-3.1760321709483));
#63966=CARTESIAN_POINT('Ctrl Pts',(-0.551378907755982,-0.23625689226104,
-3.18066871426355));
#63967=CARTESIAN_POINT('Ctrl Pts',(-0.574777547680309,-0.14060770124389,
-3.1853052575788));
#63968=CARTESIAN_POINT('Ctrl Pts',(-0.586018316498532,-0.0946575756232986,
-3.18753266531237));
#63969=CARTESIAN_POINT('Ctrl Pts',(-0.591629457988783,-0.0473302755451445,
-3.18976007304594));
#63970=CARTESIAN_POINT('Ctrl Pts',(-0.591624439693044,-1.80568084665045E-6,
-3.19198748077951));
#63971=CARTESIAN_POINT('Ctrl Pts',(-0.591627593882854,-5.87472452489096E-6,
-3.21716251922049));
#63972=CARTESIAN_POINT('Ctrl Pts',(-0.591642466500989,-0.0428409876986071,
-3.21514655043859));
#63973=CARTESIAN_POINT('Ctrl Pts',(-0.587054499469894,-0.0856729623114073,
-3.21313058165668));
#63974=CARTESIAN_POINT('Ctrl Pts',(-0.577830478761204,-0.127482121445141,
-3.21111461287477));
#63975=CARTESIAN_POINT('Ctrl Pts',(-0.556616077059905,-0.223639353163076,
-3.20647806955952));
#63976=CARTESIAN_POINT('Ctrl Pts',(-0.510878907144102,-0.314386322476033,
-3.20184152624427));
#63977=CARTESIAN_POINT('Ctrl Pts',(-0.446205069971652,-0.388639664734763,
-3.19720498292902));
#63978=CARTESIAN_POINT('Ctrl Pts',(-0.381531232799202,-0.462893006993493,
-3.19256843961376));
#63979=CARTESIAN_POINT('Ctrl Pts',(-0.297920728370106,-0.520652722197995,
-3.18793189629851));
#63980=CARTESIAN_POINT('Ctrl Pts',(-0.205585310488494,-0.554864338000655,
-3.18329535298325));
#63981=CARTESIAN_POINT('Ctrl Pts',(-0.113249892606884,-0.589075953803315,
-3.178658809668));
#63982=CARTESIAN_POINT('Ctrl Pts',(-0.0121895612727601,-0.599739470204133,
-3.17402226635275));
#63983=CARTESIAN_POINT('Ctrl Pts',(0.0852526982634587,-0.585552500560244,
-3.1693857230375));
#63984=CARTESIAN_POINT('Ctrl Pts',(0.182694957799679,-0.571365530916356,
-3.16474917972224));
#63985=CARTESIAN_POINT('Ctrl Pts',(0.276519145537995,-0.532328075227762,
-3.16011263640699));
#63986=CARTESIAN_POINT('Ctrl Pts',(0.355266061314518,-0.473207966069491,
-3.15547609309174));
#63987=CARTESIAN_POINT('Ctrl Pts',(0.434012977091042,-0.414087856911221,
-3.15083954977648));
#63988=CARTESIAN_POINT('Ctrl Pts',(0.497682620905773,-0.334885094283273,
-3.14620300646123));
#63989=CARTESIAN_POINT('Ctrl Pts',(0.538498712351454,-0.2452730932438,-3.14156646314598));
#63990=CARTESIAN_POINT('Ctrl Pts',(0.579314803797134,-0.155661092204328,
-3.13692991983072));
#63991=CARTESIAN_POINT('Ctrl Pts',(0.597277342873764,-0.0556398527533296,
-3.13229337651547));
#63992=CARTESIAN_POINT('Ctrl Pts',(0.59019247812691,0.0425745491575879,
-3.12765683320022));
#63993=CARTESIAN_POINT('Ctrl Pts',(0.583107613380057,0.140788951068506,
-3.12302028988497));
#63994=CARTESIAN_POINT('Ctrl Pts',(0.55097534480972,0.237196515439342,-3.11838374656972));
#63995=CARTESIAN_POINT('Ctrl Pts',(0.497720141213799,0.320022521869433,
-3.11374720325446));
#63996=CARTESIAN_POINT('Ctrl Pts',(0.444464937617877,0.402848528299525,
-3.10911065993921));
#63997=CARTESIAN_POINT('Ctrl Pts',(0.37008679899637,0.47209297678887,-3.10447411662396));
#63998=CARTESIAN_POINT('Ctrl Pts',(0.283669885828859,0.519298709171704,
-3.0998375733087));
#63999=CARTESIAN_POINT('Ctrl Pts',(0.197252972661348,0.566504441554536,
-3.09520102999345));
#64000=CARTESIAN_POINT('Ctrl Pts',(0.0987972849478337,0.591671457830858,
-3.09056448667819));
#64001=CARTESIAN_POINT('Ctrl Pts',(0.000327690262219633,0.591725989029253,
-3.08592794336294));
#64002=CARTESIAN_POINT('Ctrl Pts',(-0.0981419044233951,0.591780520227648,
-3.08129140004769));
#64003=CARTESIAN_POINT('Ctrl Pts',(-0.196625406081108,0.566722566348117,
-3.07665485673244));
#64004=CARTESIAN_POINT('Ctrl Pts',(-0.283094550085985,0.519612576046009,
-3.07201831341718));
#64005=CARTESIAN_POINT('Ctrl Pts',(-0.36956369409086,0.472502585743902,
-3.06738177010193));
#64006=CARTESIAN_POINT('Ctrl Pts',(-0.444018480442898,0.403340559019219,
-3.06274522678668));
#64007=CARTESIAN_POINT('Ctrl Pts',(-0.497365387305842,0.320573587470437,
-3.05810868347143));
#64008=CARTESIAN_POINT('Ctrl Pts',(-0.550712294168785,0.237806615921655,
-3.05347214015617));
#64009=CARTESIAN_POINT('Ctrl Pts',(-0.582951321542635,0.141434699548774,
-3.04883559684092));
#64010=CARTESIAN_POINT('Ctrl Pts',(-0.590144961662373,0.0432282048906904,
-3.04419905352567));
#64011=CARTESIAN_POINT('Ctrl Pts',(-0.591198195640563,0.0288496127827775,
-3.04352020875727));
#64012=CARTESIAN_POINT('Ctrl Pts',(-0.591714546116039,0.0144316938796439,
-3.04284136398888));
#64013=CARTESIAN_POINT('Ctrl Pts',(-0.591700856122533,1.27964970961225E-5,
-3.04216251922049));
#64014=CARTESIAN_POINT('Origin',(0.,0.,-1.97));
#64015=CARTESIAN_POINT('',(-0.591649561283706,-1.37437984600031E-5,-2.84198748077951));
#64016=CARTESIAN_POINT('',(-0.591662271106711,-1.51681700886687E-5,-2.86716251922049));
#64017=CARTESIAN_POINT('',(-0.591675,-7.2459289488551E-17,-1.97));
#64018=CARTESIAN_POINT('Ctrl Pts',(-0.591649561283706,-1.37437984600031E-5,
-2.84198748077951));
#64019=CARTESIAN_POINT('Ctrl Pts',(-0.591592208586822,0.0671696477833834,
-2.84514970014654));
#64020=CARTESIAN_POINT('Ctrl Pts',(-0.580167345362705,0.134372049477458,
-2.84831191951356));
#64021=CARTESIAN_POINT('Ctrl Pts',(-0.557732407245809,0.197672246090027,
-2.85147413888059));
#64022=CARTESIAN_POINT('Ctrl Pts',(-0.524837610813068,0.290484941666613,
-2.85611068219584));
#64023=CARTESIAN_POINT('Ctrl Pts',(-0.468272995893203,0.374908549350676,
-2.8607472255111));
#64024=CARTESIAN_POINT('Ctrl Pts',(-0.394947071477179,0.440632007119412,
-2.86538376882635));
#64025=CARTESIAN_POINT('Ctrl Pts',(-0.321621147061154,0.506355464888148,
-2.8700203121416));
#64026=CARTESIAN_POINT('Ctrl Pts',(-0.231533913148968,0.553378772741556,
-2.87465685545685));
#64027=CARTESIAN_POINT('Ctrl Pts',(-0.135688157726274,0.575958747497883,
-2.87929339877211));
#64028=CARTESIAN_POINT('Ctrl Pts',(-0.0398424023035795,0.598538722254211,
-2.88392994208736));
#64029=CARTESIAN_POINT('Ctrl Pts',(0.0617618746296242,0.596675363913459,
-2.88856648540261));
#64030=CARTESIAN_POINT('Ctrl Pts',(0.156715253125765,0.570596253408843,
-2.89320302871787));
#64031=CARTESIAN_POINT('Ctrl Pts',(0.251668631621909,0.544517142904226,
-2.89783957203312));
#64032=CARTESIAN_POINT('Ctrl Pts',(0.339971111680989,0.494222280235743,
-2.90247611534837));
#64033=CARTESIAN_POINT('Ctrl Pts',(0.410837885905719,0.425854419339521,
-2.90711265866362));
#64034=CARTESIAN_POINT('Ctrl Pts',(0.481704660130446,0.357486558443301,
-2.91174920197888));
#64035=CARTESIAN_POINT('Ctrl Pts',(0.535135728520824,0.271045699319343,
-2.91638574529413));
#64036=CARTESIAN_POINT('Ctrl Pts',(0.564605297223316,0.177089280629439,
-2.92102228860939));
#64037=CARTESIAN_POINT('Ctrl Pts',(0.594074865925808,0.0831328619395355,
-2.92565883192464));
#64038=CARTESIAN_POINT('Ctrl Pts',(0.599582934940414,-0.0183391163163137,
-2.93029537523989));
#64039=CARTESIAN_POINT('Ctrl Pts',(0.580456777256368,-0.114933392465516,
-2.93493191855514));
#64040=CARTESIAN_POINT('Ctrl Pts',(0.561330619572321,-0.21152766861472,
-2.93956846187039));
#64041=CARTESIAN_POINT('Ctrl Pts',(0.517570235189621,-0.303244242657277,
-2.94420500518565));
#64042=CARTESIAN_POINT('Ctrl Pts',(0.454520290723326,-0.378881327446028,
-2.9488415485009));
#64043=CARTESIAN_POINT('Ctrl Pts',(0.391470346257031,-0.45451841223478,
-2.95347809181616));
#64044=CARTESIAN_POINT('Ctrl Pts',(0.309130841707141,-0.514076007769726,
-2.95811463513141));
#64045=CARTESIAN_POINT('Ctrl Pts',(0.217558297537912,-0.550280057914955,
-2.96275117844666));
#64046=CARTESIAN_POINT('Ctrl Pts',(0.125985753368682,-0.586484108060185,
-2.96738772176191));
#64047=CARTESIAN_POINT('Ctrl Pts',(0.0251801695801122,-0.599334612815697,
-2.97202426507717));
#64048=CARTESIAN_POINT('Ctrl Pts',(-0.0725465821226823,-0.587262078112317,
-2.97666080839242));
#64049=CARTESIAN_POINT('Ctrl Pts',(-0.170273333825474,-0.575189543408938,
-2.98129735170767));
#64050=CARTESIAN_POINT('Ctrl Pts',(-0.26492125344249,-0.538193969246669,
-2.98593389502292));
#64051=CARTESIAN_POINT('Ctrl Pts',(-0.34493053446614,-0.48079380337041,
-2.99057043833818));
#64052=CARTESIAN_POINT('Ctrl Pts',(-0.424939815489789,-0.423393637494151,
-2.99520698165343));
#64053=CARTESIAN_POINT('Ctrl Pts',(-0.490310457920072,-0.345588879903902,
-2.99984352496868));
#64054=CARTESIAN_POINT('Ctrl Pts',(-0.533058430192123,-0.256882200565921,
-3.00448006828394));
#64055=CARTESIAN_POINT('Ctrl Pts',(-0.57149701731779,-0.177117962845787,
-3.00864920578246));
#64056=CARTESIAN_POINT('Ctrl Pts',(-0.591644174518881,-0.0885390389592056,
-3.01281834328099));
#64057=CARTESIAN_POINT('Ctrl Pts',(-0.591712848140847,9.68948221328342E-6,
-3.01698748077951));
#64058=CARTESIAN_POINT('Ctrl Pts',(-0.591700856122533,1.27964970961225E-5,
-3.04216251922049));
#64059=CARTESIAN_POINT('Ctrl Pts',(-0.591621042783862,-0.0840500877960021,
-3.03820482067363));
#64060=CARTESIAN_POINT('Ctrl Pts',(-0.573525431531148,-0.168146230091878,
-3.03424712212677));
#64061=CARTESIAN_POINT('Ctrl Pts',(-0.538770040159903,-0.244676515627578,
-3.03028942357991));
#64062=CARTESIAN_POINT('Ctrl Pts',(-0.498053225672066,-0.334333668544475,
-3.02565288026465));
#64063=CARTESIAN_POINT('Ctrl Pts',(-0.434471343830764,-0.413606901434981,
-3.0210163369494));
#64064=CARTESIAN_POINT('Ctrl Pts',(-0.355789956250539,-0.472814192368202,
-3.01637979363415));
#64065=CARTESIAN_POINT('Ctrl Pts',(-0.277108568670313,-0.532021483301424,
-3.01174325031889));
#64066=CARTESIAN_POINT('Ctrl Pts',(-0.183327675351164,-0.571162832277359,
-3.00710670700364));
#64067=CARTESIAN_POINT('Ctrl Pts',(-0.0859011887009397,-0.585457717733161,
-3.00247016368839));
#64068=CARTESIAN_POINT('Ctrl Pts',(0.0115252979492829,-0.599752603188962,
-2.99783362037314));
#64069=CARTESIAN_POINT('Ctrl Pts',(0.11259737793058,-0.58920102512463,-2.99319707705788));
#64070=CARTESIAN_POINT('Ctrl Pts',(0.20497063107364,-0.555091698614589,
-2.98856053374263));
#64071=CARTESIAN_POINT('Ctrl Pts',(0.2973438842167,-0.520982372104548,-2.98392399042738));
#64072=CARTESIAN_POINT('Ctrl Pts',(0.381018310521524,-0.463315297148798,
-2.97928744711212));
#64073=CARTESIAN_POINT('Ctrl Pts',(0.44577434909727,-0.389133631494966,
-2.97465090379687));
#64074=CARTESIAN_POINT('Ctrl Pts',(0.510530387673018,-0.314951965841133,
-2.97001436048162));
#64075=CARTESIAN_POINT('Ctrl Pts',(0.556368038519687,-0.224255709489217,
-2.96537781716636));
#64076=CARTESIAN_POINT('Ctrl Pts',(0.577688928459145,-0.128122033270162,
-2.96074127385111));
#64077=CARTESIAN_POINT('Ctrl Pts',(0.599009818398603,-0.031988357051106,
-2.95610473053586));
#64078=CARTESIAN_POINT('Ctrl Pts',(0.59581394743085,0.0695827390350898,
-2.95146818722061));
#64079=CARTESIAN_POINT('Ctrl Pts',(0.568491642677283,0.164185887577588,
-2.94683164390535));
#64080=CARTESIAN_POINT('Ctrl Pts',(0.541169337923717,0.258789036120085,
-2.9421951005901));
#64081=CARTESIAN_POINT('Ctrl Pts',(0.489720599384338,0.346424237118884,
-2.93755855727485));
#64082=CARTESIAN_POINT('Ctrl Pts',(0.420429109415626,0.416388181183784,
-2.9329220139596));
#64083=CARTESIAN_POINT('Ctrl Pts',(0.351137619446914,0.486352125248683,
-2.92828547064434));
#64084=CARTESIAN_POINT('Ctrl Pts',(0.264003378048868,0.538644812379682,
-2.92364892732909));
#64085=CARTESIAN_POINT('Ctrl Pts',(0.169668510001653,0.566879484712028,
-2.91901238401383));
#64086=CARTESIAN_POINT('Ctrl Pts',(0.0753336419544367,0.595114157044375,
-2.91437584069858));
#64087=CARTESIAN_POINT('Ctrl Pts',(-0.0262018527419497,0.599290814578069,
-2.90973929738333));
#64088=CARTESIAN_POINT('Ctrl Pts',(-0.122536954845961,0.578899342002247,
-2.90510275406808));
#64089=CARTESIAN_POINT('Ctrl Pts',(-0.218872056949972,0.558507869426425,
-2.90046621075283));
#64090=CARTESIAN_POINT('Ctrl Pts',(-0.310006766461608,0.513548266741087,
-2.89582966743757));
#64091=CARTESIAN_POINT('Ctrl Pts',(-0.384810362152732,0.449511666871328,
-2.89119312412232));
#64092=CARTESIAN_POINT('Ctrl Pts',(-0.459613957843854,0.385475067001569,
-2.88655658080706));
#64093=CARTESIAN_POINT('Ctrl Pts',(-0.518086439714465,0.30236146994739,
-2.88192003749181));
#64094=CARTESIAN_POINT('Ctrl Pts',(-0.553086281789371,0.210321939820753,
-2.87728349417656));
#64095=CARTESIAN_POINT('Ctrl Pts',(-0.57855299272904,0.143351805962961,
-2.87390983585787));
#64096=CARTESIAN_POINT('Ctrl Pts',(-0.59159244086834,0.071655960936958,
-2.87053617753918));
#64097=CARTESIAN_POINT('Ctrl Pts',(-0.591662271106711,-1.51681700886687E-5,
-2.86716251922049));
#64098=CARTESIAN_POINT('Origin',(0.,0.,-1.97));
#64099=CARTESIAN_POINT('',(-0.591664998266214,1.53149428433475E-5,-2.66698748077951));
#64100=CARTESIAN_POINT('',(-0.591651969453636,1.41180927115857E-5,-2.69216251922049));
#64101=CARTESIAN_POINT('',(-0.591675,-7.2459289488551E-17,-1.97));
#64102=CARTESIAN_POINT('Ctrl Pts',(-0.591664998266214,1.53149428433474E-5,
-2.66698748077951));
#64103=CARTESIAN_POINT('Ctrl Pts',(-0.591690704561656,0.0259434623775831,
-2.66820797038158));
#64104=CARTESIAN_POINT('Ctrl Pts',(-0.590018051085986,0.0518683175442941,
-2.66942845998365));
#64105=CARTESIAN_POINT('Ctrl Pts',(-0.586620331737737,0.0775650782142885,
-2.67064894958572));
#64106=CARTESIAN_POINT('Ctrl Pts',(-0.573712665089448,0.175185036390063,
-2.67528549290097));
#64107=CARTESIAN_POINT('Ctrl Pts',(-0.535909194301578,0.269513180609145,
-2.67992203621623));
#64108=CARTESIAN_POINT('Ctrl Pts',(-0.477827039426967,0.34902876007421,
-2.68455857953148));
#64109=CARTESIAN_POINT('Ctrl Pts',(-0.419744884552355,0.428544339539276,
-2.68919512284673));
#64110=CARTESIAN_POINT('Ctrl Pts',(-0.341384045591001,0.493247354250325,
-2.69383166616199));
#64111=CARTESIAN_POINT('Ctrl Pts',(-0.252315109406633,0.535235313232974,
-2.69846820947724));
#64112=CARTESIAN_POINT('Ctrl Pts',(-0.163246173222264,0.577223272215623,
-2.70310475279249));
#64113=CARTESIAN_POINT('Ctrl Pts',(-0.0634691398148823,0.596496175469871,
-2.70774129610775));
#64114=CARTESIAN_POINT('Ctrl Pts',(0.0348297409247821,0.590700130449955,
-2.712377839423));
#64115=CARTESIAN_POINT('Ctrl Pts',(0.133128621664444,0.584904085430038,
-2.71701438273825));
#64116=CARTESIAN_POINT('Ctrl Pts',(0.229949349736388,0.554039092135958,
-2.72165092605351));
#64117=CARTESIAN_POINT('Ctrl Pts',(0.313466743066199,0.50187484092944,-2.72628746936876));
#64118=CARTESIAN_POINT('Ctrl Pts',(0.396984136396013,0.449710589722921,
-2.73092401268401));
#64119=CARTESIAN_POINT('Ctrl Pts',(0.467198194983692,0.376247080603962,
-2.73556055599926));
#64120=CARTESIAN_POINT('Ctrl Pts',(0.515533337509855,0.290456765943627,
-2.74019709931452));
#64121=CARTESIAN_POINT('Ctrl Pts',(0.563868480036017,0.204666451283292,
-2.74483364262977));
#64122=CARTESIAN_POINT('Ctrl Pts',(0.590324706500662,0.106549331081582,
-2.74947018594502));
#64123=CARTESIAN_POINT('Ctrl Pts',(0.591670790479691,0.00808892203070965,
-2.75410672926028));
#64124=CARTESIAN_POINT('Ctrl Pts',(0.59301687445872,-0.0903714870201624,
-2.75874327257553));
#64125=CARTESIAN_POINT('Ctrl Pts',(0.569252815952134,-0.189175184920196,
-2.76337981589078));
#64126=CARTESIAN_POINT('Ctrl Pts',(0.523281033938426,-0.276254799934433,
-2.76801635920603));
#64127=CARTESIAN_POINT('Ctrl Pts',(0.477309251924718,-0.363334414948667,
-2.77265290252129));
#64128=CARTESIAN_POINT('Ctrl Pts',(0.409129746403889,-0.438689947077106,
-2.77728944583654));
#64129=CARTESIAN_POINT('Ctrl Pts',(0.327069608925263,-0.49311786206135,
-2.78192598915179));
#64130=CARTESIAN_POINT('Ctrl Pts',(0.245009471446634,-0.547545777045597,
-2.78656253246705));
#64131=CARTESIAN_POINT('Ctrl Pts',(0.149068702010206,-0.581046074885647,
-2.7911990757823));
#64132=CARTESIAN_POINT('Ctrl Pts',(0.0509650091019394,-0.589527202776699,
-2.79583561909755));
#64133=CARTESIAN_POINT('Ctrl Pts',(-0.0471386838063262,-0.598008330667752,
-2.80047216241281));
#64134=CARTESIAN_POINT('Ctrl Pts',(-0.147405300186431,-0.581470288609808,
-2.80510870572806));
#64135=CARTESIAN_POINT('Ctrl Pts',(-0.237588795020007,-0.541932947372111,
-2.80974524904331));
#64136=CARTESIAN_POINT('Ctrl Pts',(-0.327772289853581,-0.502395606134414,
-2.81438179235857));
#64137=CARTESIAN_POINT('Ctrl Pts',(-0.407872663140626,-0.439858965716965,
-2.81901833567382));
#64138=CARTESIAN_POINT('Ctrl Pts',(-0.468106870307834,-0.361960927362451,
-2.82365487898907));
#64139=CARTESIAN_POINT('Ctrl Pts',(-0.528341077475043,-0.284062889007937,
-2.82829142230432));
#64140=CARTESIAN_POINT('Ctrl Pts',(-0.568709118522414,-0.190803452716357,
-2.83292796561958));
#64141=CARTESIAN_POINT('Ctrl Pts',(-0.584280650073291,-0.0935728428360127,
-2.83756450893483));
#64142=CARTESIAN_POINT('Ctrl Pts',(-0.589232071922516,-0.0626555393837431,
-2.83903883288306));
#64143=CARTESIAN_POINT('Ctrl Pts',(-0.591676300875334,-0.0313367077158365,
-2.84051315683128));
#64144=CARTESIAN_POINT('Ctrl Pts',(-0.591649561283706,-1.37437984600031E-5,
-2.84198748077951));
#64145=CARTESIAN_POINT('Ctrl Pts',(-0.591662271106711,-1.51681700886687E-5,
-2.86716251922049));
#64146=CARTESIAN_POINT('Ctrl Pts',(-0.591688411145806,-0.0268443207059845,
-2.86589963422393));
#64147=CARTESIAN_POINT('Ctrl Pts',(-0.589897142504733,-0.0536700098456575,
-2.86463674922736));
#64148=CARTESIAN_POINT('Ctrl Pts',(-0.586260015865897,-0.08024305122859,
-2.8633738642308));
#64149=CARTESIAN_POINT('Ctrl Pts',(-0.572906705588316,-0.177803048952202,
-2.85873732091555));
#64150=CARTESIAN_POINT('Ctrl Pts',(-0.534672882753952,-0.271957581200331,
-2.85410077760029));
#64151=CARTESIAN_POINT('Ctrl Pts',(-0.476228228384843,-0.351207101242258,
-2.84946423428504));
#64152=CARTESIAN_POINT('Ctrl Pts',(-0.417783574015732,-0.430456621284187,
-2.84482769096979));
#64153=CARTESIAN_POINT('Ctrl Pts',(-0.339128088111874,-0.494801129119914,
-2.84019114765453));
#64154=CARTESIAN_POINT('Ctrl Pts',(-0.249868344187915,-0.536381919947294,
-2.83555460433928));
#64155=CARTESIAN_POINT('Ctrl Pts',(-0.160608600263956,-0.577962710774674,
-2.83091806102403));
#64156=CARTESIAN_POINT('Ctrl Pts',(-0.0607445983199012,-0.596779784593707,
-2.82628151770878));
#64157=CARTESIAN_POINT('Ctrl Pts',(0.0375267898670622,-0.590534921504079,
-2.82164497439352));
#64158=CARTESIAN_POINT('Ctrl Pts',(0.135798178054023,-0.584290058414453,
-2.81700843107827));
#64159=CARTESIAN_POINT('Ctrl Pts',(0.232476952483891,-0.552983258416165,
-2.81237188776302));
#64160=CARTESIAN_POINT('Ctrl Pts',(0.315755268564591,-0.500438171852686,
-2.80773534444776));
#64161=CARTESIAN_POINT('Ctrl Pts',(0.39903358464529,-0.447893085289208,
-2.80309880113251));
#64162=CARTESIAN_POINT('Ctrl Pts',(0.468911442376825,-0.374109712160539,
-2.79846225781726));
#64163=CARTESIAN_POINT('Ctrl Pts',(0.516854322270441,-0.288099571370592,
-2.793825714502));
#64164=CARTESIAN_POINT('Ctrl Pts',(0.564797202164058,-0.202089430580642,
-2.78918917118675));
#64165=CARTESIAN_POINT('Ctrl Pts',(0.590805104219755,-0.103852522129414,
-2.7845526278715));
#64166=CARTESIAN_POINT('Ctrl Pts',(0.591701558033863,-0.00538699302526537,
-2.77991608455625));
#64167=CARTESIAN_POINT('Ctrl Pts',(0.592598011847971,0.0930785360788831,
-2.77527954124099));
#64168=CARTESIAN_POINT('Ctrl Pts',(0.568383017420491,0.191772685835952,
-2.77064299792574));
#64169=CARTESIAN_POINT('Ctrl Pts',(0.52201406870688,0.278641464153569,-2.76600645461049));
#64170=CARTESIAN_POINT('Ctrl Pts',(0.475645119993269,0.365510242471186,
-2.76136991129523));
#64171=CARTESIAN_POINT('Ctrl Pts',(0.407122216993528,0.440553649349351,
-2.75673336797998));
#64172=CARTESIAN_POINT('Ctrl Pts',(0.32481439204583,0.494606271890535,-2.75209682466473));
#64173=CARTESIAN_POINT('Ctrl Pts',(0.242506567098132,0.548658894431719,
-2.74746028134948));
#64174=CARTESIAN_POINT('Ctrl Pts',(0.146413820202477,0.581720732635921,
-2.74282373803422));
#64175=CARTESIAN_POINT('Ctrl Pts',(0.0482724215842585,0.589753784886496,
-2.73818719471897));
#64176=CARTESIAN_POINT('Ctrl Pts',(-0.0498689770339597,0.59778683713707,
-2.73355065140372));
#64177=CARTESIAN_POINT('Ctrl Pts',(-0.150059027374741,0.580791103434017,
-2.72891410808846));
#64178=CARTESIAN_POINT('Ctrl Pts',(-0.240061035799051,0.540842354632699,
-2.72427756477321));
#64179=CARTESIAN_POINT('Ctrl Pts',(-0.330063044223363,0.500893605831381,
-2.71964102145796));
#64180=CARTESIAN_POINT('Ctrl Pts',(-0.409877010731205,0.437991841931797,
-2.7150044781427));
#64181=CARTESIAN_POINT('Ctrl Pts',(-0.469754870989334,0.359819558466949,
-2.71036793482745));
#64182=CARTESIAN_POINT('Ctrl Pts',(-0.529632731247464,0.2816472750021,-2.7057313915122));
#64183=CARTESIAN_POINT('Ctrl Pts',(-0.569574485255881,0.188204471971986,
-2.70109484819695));
#64184=CARTESIAN_POINT('Ctrl Pts',(-0.584701854128169,0.090903769188283,
-2.69645830488169));
#64185=CARTESIAN_POINT('Ctrl Pts',(-0.58937372063696,0.0608538709902104,
-2.69502637632796));
#64186=CARTESIAN_POINT('Ctrl Pts',(-0.591678808869539,0.0304360090776029,
-2.69359444777423));
#64187=CARTESIAN_POINT('Ctrl Pts',(-0.591651969453636,1.41180927115857E-5,
-2.69216251922049));
#64188=CARTESIAN_POINT('Origin',(0.,0.,-1.97));
#64189=CARTESIAN_POINT('',(-0.591698200799366,-1.32858733848662E-5,-2.49198748077951));
#64190=CARTESIAN_POINT('',(-0.591710646980237,-1.03961135234074E-5,-2.51716251922049));
#64191=CARTESIAN_POINT('',(-0.591675,-7.2459289488551E-17,-1.97));
#64192=CARTESIAN_POINT('Ctrl Pts',(-0.591698200799366,-1.32858733848662E-5,
-2.49198748077951));
#64193=CARTESIAN_POINT('Ctrl Pts',(-0.591617318058343,0.0831501844531302,
-2.49590278393188));
#64194=CARTESIAN_POINT('Ctrl Pts',(-0.573918730141509,0.166346986995152,
-2.49981808708425));
#64195=CARTESIAN_POINT('Ctrl Pts',(-0.539881730934194,0.24221368988969,
-2.50373339023661));
#64196=CARTESIAN_POINT('Ctrl Pts',(-0.499574757245456,0.332055840156694,
-2.50836993355187));
#64197=CARTESIAN_POINT('Ctrl Pts',(-0.436355536734211,0.411618591198725,
-2.51300647686712));
#64198=CARTESIAN_POINT('Ctrl Pts',(-0.357945337439186,0.471184560837925,
-2.51764302018237));
#64199=CARTESIAN_POINT('Ctrl Pts',(-0.279535138144161,0.530750530477125,
-2.52227956349763));
#64200=CARTESIAN_POINT('Ctrl Pts',(-0.185933960065355,0.570319718713494,
-2.52691610681288));
#64201=CARTESIAN_POINT('Ctrl Pts',(-0.0885737661223129,0.585059349913657,
-2.53155265012813));
#64202=CARTESIAN_POINT('Ctrl Pts',(0.00878642782072664,0.599798981113819,
-2.53618919344339));
#64203=CARTESIAN_POINT('Ctrl Pts',(0.109905637628004,0.589709055277775,
-2.54082573675864));
#64204=CARTESIAN_POINT('Ctrl Pts',(0.202433686937452,0.556021903668723,
-2.54546228007389));
#64205=CARTESIAN_POINT('Ctrl Pts',(0.294961736246904,0.522334752059669,
-2.55009882338915));
#64206=CARTESIAN_POINT('Ctrl Pts',(0.378898625058528,0.465050374677606,
-2.5547353667044));
#64207=CARTESIAN_POINT('Ctrl Pts',(0.443992736670785,0.39116518857136,-2.55937191001965));
#64208=CARTESIAN_POINT('Ctrl Pts',(0.509086848283043,0.317280002465114,
-2.5640084533349));
#64209=CARTESIAN_POINT('Ctrl Pts',(0.555338182695934,0.226794007634685,
-2.56864499665016));
#64210=CARTESIAN_POINT('Ctrl Pts',(0.577097841563945,0.1307586946582,-2.57328153996541));
#64211=CARTESIAN_POINT('Ctrl Pts',(0.598857500431956,0.0347233816817167,
-2.57791808328066));
#64212=CARTESIAN_POINT('Ctrl Pts',(0.596125483755088,-0.0668612494408195,
-2.58255462659592));
#64213=CARTESIAN_POINT('Ctrl Pts',(0.569235465894994,-0.161588178199368,
-2.58719116991117));
#64214=CARTESIAN_POINT('Ctrl Pts',(0.542345448034899,-0.256315106957918,
-2.59182771322642));
#64215=CARTESIAN_POINT('Ctrl Pts',(0.491297428991578,-0.344184333352478,
-2.59646425654168));
#64216=CARTESIAN_POINT('Ctrl Pts',(0.42232614931849,-0.414463965343548,
-2.60110079985693));
#64217=CARTESIAN_POINT('Ctrl Pts',(0.353354869645401,-0.484743597334618,
-2.60573734317218));
#64218=CARTESIAN_POINT('Ctrl Pts',(0.266460329342544,-0.537433634922199,
-2.61037388648743));
#64219=CARTESIAN_POINT('Ctrl Pts',(0.172255377340268,-0.566098789915544,
-2.61501042980269));
#64220=CARTESIAN_POINT('Ctrl Pts',(0.078050425337992,-0.594763944908889,
-2.61964697311794));
#64221=CARTESIAN_POINT('Ctrl Pts',(-0.0234649383637043,-0.599404217307997,
-2.62428351643319));
#64222=CARTESIAN_POINT('Ctrl Pts',(-0.119892153218662,-0.579452868284448,
-2.62892005974845));
#64223=CARTESIAN_POINT('Ctrl Pts',(-0.21631936807362,-0.559501519260899,
-2.6335566030637));
#64224=CARTESIAN_POINT('Ctrl Pts',(-0.30765843408184,-0.514958548814693,
-2.63819314637895));
#64225=CARTESIAN_POINT('Ctrl Pts',(-0.382753670971514,-0.451264204567913,
-2.6428296896942));
#64226=CARTESIAN_POINT('Ctrl Pts',(-0.457848907861189,-0.387569860321132,
-2.64746623300946));
#64227=CARTESIAN_POINT('Ctrl Pts',(-0.516700315632318,-0.304724142273775,
-2.65210277632471));
#64228=CARTESIAN_POINT('Ctrl Pts',(-0.552120088263528,-0.212845397183861,
-2.65673931963997));
#64229=CARTESIAN_POINT('Ctrl Pts',(-0.578216220142391,-0.145152138006409,
-2.66015537335315));
#64230=CARTESIAN_POINT('Ctrl Pts',(-0.591593048381636,-0.0725555157877893,
-2.66357142706633));
#64231=CARTESIAN_POINT('Ctrl Pts',(-0.591664998266214,1.53149428433474E-5,
-2.66698748077951));
#64232=CARTESIAN_POINT('Ctrl Pts',(-0.591651969453636,1.41180927115857E-5,
-2.69216251922049));
#64233=CARTESIAN_POINT('Ctrl Pts',(-0.591591903615735,-0.0680691956098775,
-2.68895790445897));
#64234=CARTESIAN_POINT('Ctrl Pts',(-0.57985234370179,-0.13617268898052,
-2.68575328969745));
#64235=CARTESIAN_POINT('Ctrl Pts',(-0.556823927312267,-0.200217050837582,
-2.68254867493593));
#64236=CARTESIAN_POINT('Ctrl Pts',(-0.523505647887919,-0.292878565542456,
-2.67791213162068));
#64237=CARTESIAN_POINT('Ctrl Pts',(-0.466556105303064,-0.377042992414913,
-2.67327558830543));
#64238=CARTESIAN_POINT('Ctrl Pts',(-0.392930821619261,-0.442430924433598,
-2.66863904499017));
#64239=CARTESIAN_POINT('Ctrl Pts',(-0.319305537935459,-0.507818856452282,
-2.66400250167492));
#64240=CARTESIAN_POINT('Ctrl Pts',(-0.229004513152709,-0.554430293617193,
-2.65936595835967));
#64241=CARTESIAN_POINT('Ctrl Pts',(-0.133056646565889,-0.576572356498467,
-2.65472941504442));
#64242=CARTESIAN_POINT('Ctrl Pts',(-0.0371087799790665,-0.598714419379742,
-2.65009287172916));
#64243=CARTESIAN_POINT('Ctrl Pts',(0.0644859284118255,-0.596387107977379,
-2.64545632841391));
#64244=CARTESIAN_POINT('Ctrl Pts',(0.159319227311396,-0.569874668047682,
-2.64081978509866));
#64245=CARTESIAN_POINT('Ctrl Pts',(0.254152526210965,-0.543362228117985,
-2.6361832417834));
#64246=CARTESIAN_POINT('Ctrl Pts',(0.342224415619212,-0.492664659660956,
-2.63154669846815));
#64247=CARTESIAN_POINT('Ctrl Pts',(0.412778251286195,-0.423973901011214,
-2.6269101551529));
#64248=CARTESIAN_POINT('Ctrl Pts',(0.483332086953178,-0.355283142361472,
-2.62227361183765));
#64249=CARTESIAN_POINT('Ctrl Pts',(0.536367868878897,-0.268599193519018,
-2.61763706852239));
#64250=CARTESIAN_POINT('Ctrl Pts',(0.565408081450532,-0.174509182864352,
-2.61300052520714));
#64251=CARTESIAN_POINT('Ctrl Pts',(0.594448294022167,-0.0804191722096898,
-2.60836398189189));
#64252=CARTESIAN_POINT('Ctrl Pts',(0.599492937239718,0.0210769002571867,
-2.60372743857663));
#64253=CARTESIAN_POINT('Ctrl Pts',(0.579925884518147,0.117582830121581,
-2.59909089526138));
#64254=CARTESIAN_POINT('Ctrl Pts',(0.560358831796575,0.214088759985979,
-2.59445435194613));
#64255=CARTESIAN_POINT('Ctrl Pts',(0.516180083135882,0.305604547247894,
-2.58981780863087));
#64256=CARTESIAN_POINT('Ctrl Pts',(0.452785401996388,0.380952927817237,
-2.58518126531562));
#64257=CARTESIAN_POINT('Ctrl Pts',(0.389390720856894,0.45630130838658,-2.58054472200037));
#64258=CARTESIAN_POINT('Ctrl Pts',(0.306780107238598,0.515482282263348,
-2.57590817868511));
#64259=CARTESIAN_POINT('Ctrl Pts',(0.215043193462692,0.551267791929587,
-2.57127163536986));
#64260=CARTESIAN_POINT('Ctrl Pts',(0.123306279686785,0.587053301595827,
-2.56663509205461));
#64261=CARTESIAN_POINT('Ctrl Pts',(0.0224430657532648,0.599443347051538,
-2.56199854873936));
#64262=CARTESIAN_POINT('Ctrl Pts',(-0.075227537985446,0.586924672340671,
-2.5573620054241));
#64263=CARTESIAN_POINT('Ctrl Pts',(-0.172898141724155,0.574405997629804,
-2.55272546210885));
#64264=CARTESIAN_POINT('Ctrl Pts',(-0.267376135268055,0.536978602752358,
-2.5480889187936));
#64265=CARTESIAN_POINT('Ctrl Pts',(-0.347122465999695,0.479213675798017,
-2.54345237547834));
#64266=CARTESIAN_POINT('Ctrl Pts',(-0.426868796731334,0.421448748843675,
-2.53881583216309));
#64267=CARTESIAN_POINT('Ctrl Pts',(-0.491883464650713,0.343346289812437,
-2.53417928884784));
#64268=CARTESIAN_POINT('Ctrl Pts',(-0.534225915075338,0.254445328382098,
-2.52954274553259));
#64269=CARTESIAN_POINT('Ctrl Pts',(-0.571912691855857,0.175319282170792,
-2.52541600342855));
#64270=CARTESIAN_POINT('Ctrl Pts',(-0.59163890281563,0.0876388361461731,
-2.52128926132452));
#64271=CARTESIAN_POINT('Ctrl Pts',(-0.591710646980237,-1.03961135234074E-5,
-2.51716251922049));
#64272=CARTESIAN_POINT('Origin',(0.,0.,-1.97));
#64273=CARTESIAN_POINT('',(-0.591628625190756,6.64897484074778E-6,-2.31698748077951));
#64274=CARTESIAN_POINT('',(-0.591624801665701,2.64146101175725E-6,-2.34216251922049));
#64275=CARTESIAN_POINT('',(-0.591675,-7.2459289488551E-17,-1.97));
#64276=CARTESIAN_POINT('Ctrl Pts',(-0.591628625190756,6.64897484074778E-6,
-2.31698748077951));
#64277=CARTESIAN_POINT('Ctrl Pts',(-0.591645139193398,0.041940739843989,
-2.31896105416692));
#64278=CARTESIAN_POINT('Ctrl Pts',(-0.58724964040398,0.083871419065752,
-2.32093462755434));
#64279=CARTESIAN_POINT('Ctrl Pts',(-0.57840659812157,0.124842149196146,
-2.32290820094175));
#64280=CARTESIAN_POINT('Ctrl Pts',(-0.557631516311841,0.22109525339722,
-2.327544744257));
#64281=CARTESIAN_POINT('Ctrl Pts',(-0.512309216138202,0.312050133983124,
-2.33218128757225));
#64282=CARTESIAN_POINT('Ctrl Pts',(-0.447975128517742,0.386598033098972,
-2.33681783088751));
#64283=CARTESIAN_POINT('Ctrl Pts',(-0.383641040897284,0.461145932214817,
-2.34145437420276));
#64284=CARTESIAN_POINT('Ctrl Pts',(-0.300295165830006,0.519286849860608,
-2.34609091751801));
#64285=CARTESIAN_POINT('Ctrl Pts',(-0.208116936660901,0.553919755597653,
-2.35072746083327));
#64286=CARTESIAN_POINT('Ctrl Pts',(-0.115938707491793,0.588552661334699,
-2.35536400414852));
#64287=CARTESIAN_POINT('Ctrl Pts',(-0.0149281242208578,0.599677555162998,
-2.36000054746377));
#64288=CARTESIAN_POINT('Ctrl Pts',(0.0825779038721678,0.585935700191207,
-2.36463709077902));
#64289=CARTESIAN_POINT('Ctrl Pts',(0.180083931965194,0.572193845219415,
-2.36927363409428));
#64290=CARTESIAN_POINT('Ctrl Pts',(0.27408540488031,0.533585241447532,-2.37391017740953));
#64291=CARTESIAN_POINT('Ctrl Pts',(0.353101469760693,0.47482534369947,-2.37854672072478));
#64292=CARTESIAN_POINT('Ctrl Pts',(0.432117534641076,0.416065445951407,
-2.38318326404004));
#64293=CARTESIAN_POINT('Ctrl Pts',(0.496148191486726,0.337154254227165,
-2.38781980735529));
#64294=CARTESIAN_POINT('Ctrl Pts',(0.537373067629286,0.247729572625416,
-2.39245635067054));
#64295=CARTESIAN_POINT('Ctrl Pts',(0.578597943771846,0.15830489102367,-2.39709289398579));
#64296=CARTESIAN_POINT('Ctrl Pts',(0.597017039211317,0.0583667195444171,
-2.40172943730105));
#64297=CARTESIAN_POINT('Ctrl Pts',(0.590380741064641,-0.0398790113524088,
-2.4063659806163));
#64298=CARTESIAN_POINT('Ctrl Pts',(0.583744442917966,-0.138124742249238,
-2.41100252393155));
#64299=CARTESIAN_POINT('Ctrl Pts',(0.552052751185142,-0.234678032563639,
-2.41563906724681));
#64300=CARTESIAN_POINT('Ctrl Pts',(0.499176324891873,-0.317746363683244,
-2.42027561056206));
#64301=CARTESIAN_POINT('Ctrl Pts',(0.446299898598605,-0.400814694802848,
-2.42491215387731));
#64302=CARTESIAN_POINT('Ctrl Pts',(0.372238737744891,-0.470398066727654,
-2.42954869719257));
#64303=CARTESIAN_POINT('Ctrl Pts',(0.286038288788097,-0.517997926939537,
-2.43418524050782));
#64304=CARTESIAN_POINT('Ctrl Pts',(0.199837839831306,-0.565597787151419,
-2.43882178382307));
#64305=CARTESIAN_POINT('Ctrl Pts',(0.101498102771434,-0.591214135650378,
-2.44345832713832));
#64306=CARTESIAN_POINT('Ctrl Pts',(0.00302978357031825,-0.59171832435543,
-2.44809487045358));
#64307=CARTESIAN_POINT('Ctrl Pts',(-0.0954385356308003,-0.592222513060482,
-2.45273141376883));
#64308=CARTESIAN_POINT('Ctrl Pts',(-0.194035436973163,-0.567614541971626,
-2.45736795708408));
#64309=CARTESIAN_POINT('Ctrl Pts',(-0.2807188057819,-0.520899901177631,
-2.46200450039934));
#64310=CARTESIAN_POINT('Ctrl Pts',(-0.367402174590638,-0.474185260383635,
-2.46664104371459));
#64311=CARTESIAN_POINT('Ctrl Pts',(-0.44217201086575,-0.4053639498845,-2.47127758702984));
#64312=CARTESIAN_POINT('Ctrl Pts',(-0.495896314205729,-0.32284144796425,
-2.4759141303451));
#64313=CARTESIAN_POINT('Ctrl Pts',(-0.549620617545708,-0.240318946044,-2.48055067366035));
#64314=CARTESIAN_POINT('Ctrl Pts',(-0.582299387950553,-0.144095252702636,
-2.4851872169756));
#64315=CARTESIAN_POINT('Ctrl Pts',(-0.589941409719859,-0.0459226312859645,
-2.48982376029085));
#64316=CARTESIAN_POINT('Ctrl Pts',(-0.591130168812766,-0.0306513326811538,
-2.49054500045374));
#64317=CARTESIAN_POINT('Ctrl Pts',(-0.591713100253902,-0.015332874817107,
-2.49126624061662));
#64318=CARTESIAN_POINT('Ctrl Pts',(-0.591698200799366,-1.32858733848662E-5,
-2.49198748077951));
#64319=CARTESIAN_POINT('Ctrl Pts',(-0.591710646980237,-1.03961135234074E-5,
-2.51716251922049));
#64320=CARTESIAN_POINT('Ctrl Pts',(-0.591719509967333,-0.0108382316414618,
-2.51665271800927));
#64321=CARTESIAN_POINT('Ctrl Pts',(-0.59142842332184,-0.0216655908116636,
-2.51614291679805));
#64322=CARTESIAN_POINT('Ctrl Pts',(-0.590834193531263,-0.0324762871618411,
-2.51563311558682));
#64323=CARTESIAN_POINT('Ctrl Pts',(-0.585429788632694,-0.130797477445996,
-2.51099657227157));
#64324=CARTESIAN_POINT('Ctrl Pts',(-0.554950745905688,-0.227740394184864,
-2.50636002895632));
#64325=CARTESIAN_POINT('Ctrl Pts',(-0.503119617709414,-0.311464931813341,
-2.50172348564107));
#64326=CARTESIAN_POINT('Ctrl Pts',(-0.451288489513141,-0.395189469441816,
-2.49708694232582));
#64327=CARTESIAN_POINT('Ctrl Pts',(-0.3781052758476,-0.4656956279599,-2.49245039901056));
#64328=CARTESIAN_POINT('Ctrl Pts',(-0.292508195249456,-0.514372150476152,
-2.48781385569531));
#64329=CARTESIAN_POINT('Ctrl Pts',(-0.206911114651311,-0.563048672992405,
-2.48317731238005));
#64330=CARTESIAN_POINT('Ctrl Pts',(-0.108900167120564,-0.589895559506825,
-2.4785407690648));
#64331=CARTESIAN_POINT('Ctrl Pts',(-0.0104459019694992,-0.591633870400943,
-2.47390422574955));
#64332=CARTESIAN_POINT('Ctrl Pts',(0.0880083631815653,-0.593372181295061,
-2.4692676824343));
#64333=CARTESIAN_POINT('Ctrl Pts',(0.186905945952945,-0.570001916568875,
-2.46463113911904));
#64334=CARTESIAN_POINT('Ctrl Pts',(0.274168007997934,-0.524377399268885,
-2.45999459580379));
#64335=CARTESIAN_POINT('Ctrl Pts',(0.361430070042924,-0.478752881968895,
-2.45535805248854));
#64336=CARTESIAN_POINT('Ctrl Pts',(0.437056611361525,-0.4108741120951,-2.45072150917328));
#64337=CARTESIAN_POINT('Ctrl Pts',(0.491810998037018,-0.329031450903083,
-2.44608496585803));
#64338=CARTESIAN_POINT('Ctrl Pts',(0.54656538471251,-0.247188789711066,
-2.44144842254278));
#64339=CARTESIAN_POINT('Ctrl Pts',(0.580447616744896,-0.151382237200826,
-2.43681187922752));
#64340=CARTESIAN_POINT('Ctrl Pts',(0.589319493866015,-0.053313109298369,
-2.43217533591227));
#64341=CARTESIAN_POINT('Ctrl Pts',(0.598191370987134,0.0447560186040879,
-2.42753879259702));
#64342=CARTESIAN_POINT('Ctrl Pts',(0.582052893196987,0.145087721898763,
-2.42290224928177));
#64343=CARTESIAN_POINT('Ctrl Pts',(0.542875130555393,0.235428006188772,
-2.41826570596651));
#64344=CARTESIAN_POINT('Ctrl Pts',(0.503697367913799,0.325768290478781,
-2.41362916265126));
#64345=CARTESIAN_POINT('Ctrl Pts',(0.441480320420757,0.406117155764124,
-2.40899261933601));
#64346=CARTESIAN_POINT('Ctrl Pts',(0.363822855895058,0.466661207946321,
-2.40435607602075));
#64347=CARTESIAN_POINT('Ctrl Pts',(0.286165391369361,0.527205260128516,
-2.3997195327055));
#64348=CARTESIAN_POINT('Ctrl Pts',(0.193067509811008,0.567944499207565,
-2.39508298939025));
#64349=CARTESIAN_POINT('Ctrl Pts',(0.0958997041102385,0.583903245602492,
-2.39044644607499));
#64350=CARTESIAN_POINT('Ctrl Pts',(-0.00126810159053549,0.59986199199742,
-2.38580990275974));
#64351=CARTESIAN_POINT('Ctrl Pts',(-0.102505831433723,0.591040245708224,
-2.38117335944449));
#64352=CARTESIAN_POINT('Ctrl Pts',(-0.195448833634162,0.558515449119003,
-2.37653681612924));
#64353=CARTESIAN_POINT('Ctrl Pts',(-0.288391835834599,0.525990652529782,
-2.37190027281398));
#64354=CARTESIAN_POINT('Ctrl Pts',(-0.373040110392285,0.469762805640536,
-2.36726372949873));
#64355=CARTESIAN_POINT('Ctrl Pts',(-0.439055155636522,0.396699286339848,
-2.36262718618348));
#64356=CARTESIAN_POINT('Ctrl Pts',(-0.505070200880759,0.32363576703916,
-2.35799064286822));
#64357=CARTESIAN_POINT('Ctrl Pts',(-0.552452016811549,0.233736575327029,
-2.35335409955297));
#64358=CARTESIAN_POINT('Ctrl Pts',(-0.575413633928087,0.137981532689086,
-2.34871755623772));
#64359=CARTESIAN_POINT('Ctrl Pts',(-0.586234500533539,0.092856115871717,
-2.34653254389864));
#64360=CARTESIAN_POINT('Ctrl Pts',(-0.591632008304765,0.0464302026459444,
-2.34434753155957));
#64361=CARTESIAN_POINT('Ctrl Pts',(-0.591624801665701,2.64146101175725E-6,
-2.34216251922049));
#64362=CARTESIAN_POINT('Origin',(0.,0.,-1.97));
#64363=CARTESIAN_POINT('',(-0.591726041258602,7.22680221576831E-7,-2.14198748077951));
#64364=CARTESIAN_POINT('',(-0.591722112168784,5.38077801797166E-6,-2.16716251922049));
#64365=CARTESIAN_POINT('',(-0.591675,-7.2459289488551E-17,-1.97));
#64366=CARTESIAN_POINT('Ctrl Pts',(-0.591726006610465,7.22189647403126E-7,
-2.14198748077951));
#64367=CARTESIAN_POINT('Ctrl Pts',(-0.591726055065786,0.000677008384288284,
-2.14201932440197));
#64368=CARTESIAN_POINT('Ctrl Pts',(-0.591724919978352,0.00135329441552927,
-2.14205116802442));
#64369=CARTESIAN_POINT('Ctrl Pts',(-0.591722600367928,0.00202957638392072,
-2.14208301164688));
#64370=CARTESIAN_POINT('Ctrl Pts',(-0.591384856940035,0.100498607159696,
-2.14671955496213));
#64371=CARTESIAN_POINT('Ctrl Pts',(-0.565934772246907,0.198881503968735,
-2.15135609827739));
#64372=CARTESIAN_POINT('Ctrl Pts',(-0.518480687769739,0.28516228954106,
-2.15599264159264));
#64373=CARTESIAN_POINT('Ctrl Pts',(-0.471026603292572,0.371443075113383,
-2.16062918490789));
#64374=CARTESIAN_POINT('Ctrl Pts',(-0.401568519031367,0.44562174944899,
-2.16526572822314));
#64375=CARTESIAN_POINT('Ctrl Pts',(-0.318589685518163,0.498638513602709,
-2.1699022715384));
#64376=CARTESIAN_POINT('Ctrl Pts',(-0.235610852004958,0.551655277756428,
-2.17453881485365));
#64377=CARTESIAN_POINT('Ctrl Pts',(-0.139111269239756,0.583510131728257,
-2.17917535816891));
#64378=CARTESIAN_POINT('Ctrl Pts',(-0.0408768962731364,0.590312488702006,
-2.18381190148416));
#64379=CARTESIAN_POINT('Ctrl Pts',(0.0573574766934885,0.597114845675755,
-2.18844844479941));
#64380=CARTESIAN_POINT('Ctrl Pts',(0.157326639861528,0.578864705651421,
-2.19308498811466));
#64381=CARTESIAN_POINT('Ctrl Pts',(0.246820877606758,0.537791046173057,
-2.19772153142992));
#64382=CARTESIAN_POINT('Ctrl Pts',(0.336315115351985,0.496717386694694,
-2.20235807474517));
#64383=CARTESIAN_POINT('Ctrl Pts',(0.4153344276744,0.432820207762303,-2.20699461806042));
#64384=CARTESIAN_POINT('Ctrl Pts',(0.474227805185672,0.353903579743497,
-2.21163116137568));
#64385=CARTESIAN_POINT('Ctrl Pts',(0.533121182696942,0.274986951724692,
-2.21626770469093));
#64386=CARTESIAN_POINT('Ctrl Pts',(0.57188862539707,0.18105087461947,-2.22090424800618));
#64387=CARTESIAN_POINT('Ctrl Pts',(0.585795278698428,0.0835682141792701,
-2.22554079132143));
#64388=CARTESIAN_POINT('Ctrl Pts',(0.599701931999787,-0.0139144462609336,
-2.23017733463669));
#64389=CARTESIAN_POINT('Ctrl Pts',(0.588747795902376,-0.114943690036117,
-2.23481387795194));
#64390=CARTESIAN_POINT('Ctrl Pts',(0.554270751833028,-0.207180328769239,
-2.23945042126719));
#64391=CARTESIAN_POINT('Ctrl Pts',(0.519793707763683,-0.299416967502356,
-2.24408696458245));
#64392=CARTESIAN_POINT('Ctrl Pts',(0.461793755722403,-0.382861001193412,
-2.2487235078977));
#64393=CARTESIAN_POINT('Ctrl Pts',(0.387354709339321,-0.447321007911691,
-2.25336005121295));
#64394=CARTESIAN_POINT('Ctrl Pts',(0.31291566295624,-0.51178101462997,-2.25799659452821));
#64395=CARTESIAN_POINT('Ctrl Pts',(0.222037522231357,-0.557256994375471,
-2.26263313784346));
#64396=CARTESIAN_POINT('Ctrl Pts',(0.125819672410541,-0.57819474660445,
-2.26726968115871));
#64397=CARTESIAN_POINT('Ctrl Pts',(0.0296018225897245,-0.599132498833431,
-2.27190622447397));
#64398=CARTESIAN_POINT('Ctrl Pts',(-0.0719557363270286,-0.595532023545888,
-2.27654276778922));
#64399=CARTESIAN_POINT('Ctrl Pts',(-0.166449290288611,-0.567833064138483,
-2.28117931110447));
#64400=CARTESIAN_POINT('Ctrl Pts',(-0.260942844250194,-0.540134104731079,
-2.28581585441972));
#64401=CARTESIAN_POINT('Ctrl Pts',(-0.348372393256609,-0.488336661203813,
-2.29045239773498));
#64402=CARTESIAN_POINT('Ctrl Pts',(-0.418059745186469,-0.418767004933657,
-2.29508894105023));
#64403=CARTESIAN_POINT('Ctrl Pts',(-0.487747097116328,-0.349197348663502,
-2.29972548436548));
#64404=CARTESIAN_POINT('Ctrl Pts',(-0.539692251969632,-0.261855479650458,
-2.30436202768074));
#64405=CARTESIAN_POINT('Ctrl Pts',(-0.567550897673375,-0.167408881235814,
-2.30899857099599));
#64406=CARTESIAN_POINT('Ctrl Pts',(-0.583551338237656,-0.113164062571531,
-2.31166154092383));
#64407=CARTESIAN_POINT('Ctrl Pts',(-0.591606342618086,-0.0565756010940282,
-2.31432451085167));
#64408=CARTESIAN_POINT('Ctrl Pts',(-0.591628625190756,6.64897484074778E-6,
-2.31698748077951));
#64409=CARTESIAN_POINT('Ctrl Pts',(-0.591624801665701,2.64146101175725E-6,
-2.34216251922049));
#64410=CARTESIAN_POINT('Ctrl Pts',(-0.591616715991041,-0.052087958833455,
-2.33971098824431));
#64411=CARTESIAN_POINT('Ctrl Pts',(-0.584805015269325,-0.104180633627865,
-2.33725945726814));
#64412=CARTESIAN_POINT('Ctrl Pts',(-0.571216032446229,-0.154440919933626,
-2.33480792629196));
#64413=CARTESIAN_POINT('Ctrl Pts',(-0.545515395545548,-0.249497436354648,
-2.33017138297671));
#64414=CARTESIAN_POINT('Ctrl Pts',(-0.495572703441898,-0.337999575632937,
-2.32553483966145));
#64415=CARTESIAN_POINT('Ctrl Pts',(-0.4274876977833,-0.409138145028656,
-2.3208982963462));
#64416=CARTESIAN_POINT('Ctrl Pts',(-0.359402692124703,-0.480276714424375,
-2.31626175303095));
#64417=CARTESIAN_POINT('Ctrl Pts',(-0.273175372911158,-0.534051713937523,
-2.31162520971569));
#64418=CARTESIAN_POINT('Ctrl Pts',(-0.179337098146204,-0.563895343749223,
-2.30698866640044));
#64419=CARTESIAN_POINT('Ctrl Pts',(-0.0854988233812528,-0.593738973560922,
-2.30235212308519));
#64420=CARTESIAN_POINT('Ctrl Pts',(0.0159504069351066,-0.599651233671174,
-2.29771557976993));
#64421=CARTESIAN_POINT('Ctrl Pts',(0.11262010944575,-0.580910031263003,
-2.29307903645468));
#64422=CARTESIAN_POINT('Ctrl Pts',(0.209289811956395,-0.562168828854832,
-2.28844249313943));
#64423=CARTESIAN_POINT('Ctrl Pts',(0.301179986661323,-0.518774163928237,
-2.28380594982418));
#64424=CARTESIAN_POINT('Ctrl Pts',(0.377067643727942,-0.456026036018793,
-2.27916940650892));
#64425=CARTESIAN_POINT('Ctrl Pts',(0.452955300794561,-0.393277908109348,
-2.27453286319367));
#64426=CARTESIAN_POINT('Ctrl Pts',(0.51284044022287,-0.311176317217054,
-2.26989631987842));
#64427=CARTESIAN_POINT('Ctrl Pts',(0.54940900136291,-0.219748726264717,
-2.26525977656316));
#64428=CARTESIAN_POINT('Ctrl Pts',(0.58597756250295,-0.128321135312378,
-2.26062323324791));
#64429=CARTESIAN_POINT('Ctrl Pts',(0.59922954535472,-0.0275675442999919,
-2.25598668993266));
#64430=CARTESIAN_POINT('Ctrl Pts',(0.587546421394525,0.0702065251956151,
-2.2513501466174));
#64431=CARTESIAN_POINT('Ctrl Pts',(0.575863297434331,0.167980594691218,
-2.24671360330215));
#64432=CARTESIAN_POINT('Ctrl Pts',(0.539245066662175,0.262775142670045,
-2.2420770599869));
#64433=CARTESIAN_POINT('Ctrl Pts',(0.4821640900564,0.343012454196112,-2.23744051667165));
#64434=CARTESIAN_POINT('Ctrl Pts',(0.425083113450623,0.423249765722182,
-2.23280397335639));
#64435=CARTESIAN_POINT('Ctrl Pts',(0.347539391011226,0.48892984079549,-2.22816743004114));
#64436=CARTESIAN_POINT('Ctrl Pts',(0.259003711223628,0.532030855351401,
-2.22353088672589));
#64437=CARTESIAN_POINT('Ctrl Pts',(0.170468031436031,0.575131869907311,
-2.21889434341063));
#64438=CARTESIAN_POINT('Ctrl Pts',(0.0709403943002352,0.595653823945825,
-2.21425780009538));
#64439=CARTESIAN_POINT('Ctrl Pts',(-0.0274234102614568,0.591090272330029,
-2.20962125678013));
#64440=CARTESIAN_POINT('Ctrl Pts',(-0.125787214823146,0.586526720714233,
-2.20498471346488));
#64441=CARTESIAN_POINT('Ctrl Pts',(-0.22298718681073,0.556877663444129,
-2.20034817014962));
#64442=CARTESIAN_POINT('Ctrl Pts',(-0.307151825262896,0.505764282755542,
-2.19571162683437));
#64443=CARTESIAN_POINT('Ctrl Pts',(-0.391316463715064,0.454650902066953,
-2.19107508351912));
#64444=CARTESIAN_POINT('Ctrl Pts',(-0.462445768631812,0.382073197959879,
-2.18643854020386));
#64445=CARTESIAN_POINT('Ctrl Pts',(-0.511852375249243,0.296895435170809,
-2.18180199688861));
#64446=CARTESIAN_POINT('Ctrl Pts',(-0.561258981866674,0.211717672381738,
-2.17716545357336));
#64447=CARTESIAN_POINT('Ctrl Pts',(-0.588942890184788,0.11393985091067,
-2.17252891025811));
#64448=CARTESIAN_POINT('Ctrl Pts',(-0.591522931078829,0.0155040472608508,
-2.16789236694285));
#64449=CARTESIAN_POINT('Ctrl Pts',(-0.591658307575361,0.0103390538445895,
-2.16764908436873));
#64450=CARTESIAN_POINT('Ctrl Pts',(-0.591724568804173,0.0051722488901429,
-2.16740580179461));
#64451=CARTESIAN_POINT('Ctrl Pts',(-0.591722112168784,5.38077801797166E-6,
-2.16716251922049));
#64452=CARTESIAN_POINT('Origin',(0.,0.,-1.97));
#64453=CARTESIAN_POINT('',(-0.591630412993812,-7.77508703958541E-6,-1.96698748077951));
#64454=CARTESIAN_POINT('',(-0.591638304234624,-1.11070860510166E-5,-1.99216251922049));
#64455=CARTESIAN_POINT('',(-0.591675,-7.2459289488551E-17,-1.97));
#64456=CARTESIAN_POINT('Ctrl Pts',(-0.591630412993812,-7.77508703958541E-6,
-1.96698748077951));
#64457=CARTESIAN_POINT('Ctrl Pts',(-0.591603633133982,0.0579271878064958,
-1.96971413795226));
#64458=CARTESIAN_POINT('Ctrl Pts',(-0.583152878724501,0.115869795114227,
-1.97244079512502));
#64459=CARTESIAN_POINT('Ctrl Pts',(-0.566389150662593,0.171298234019464,
-1.97516745229777));
#64460=CARTESIAN_POINT('Ctrl Pts',(-0.537883274654121,0.265551505185685,
-1.97980399561303));
#64461=CARTESIAN_POINT('Ctrl Pts',(-0.485340193320855,0.352534985223169,
-1.98444053892828));
#64462=CARTESIAN_POINT('Ctrl Pts',(-0.415177246378055,0.421624962563196,
-1.98907708224353));
#64463=CARTESIAN_POINT('Ctrl Pts',(-0.345014299435256,0.490714939903223,
-1.99371362555878));
#64464=CARTESIAN_POINT('Ctrl Pts',(-0.257231486882922,0.541911414545796,
-1.99835016887404));
#64465=CARTESIAN_POINT('Ctrl Pts',(-0.162550146621597,0.568961514339747,
-2.00298671218929));
#64466=CARTESIAN_POINT('Ctrl Pts',(-0.0678688063602742,0.596011614133698,
-2.00762325550455));
#64467=CARTESIAN_POINT('Ctrl Pts',(0.033711061610042,0.598915339079029,
-2.0122597988198));
#64468=CARTESIAN_POINT('Ctrl Pts',(0.129783018526036,0.57731804325584,-2.01689634213505));
#64469=CARTESIAN_POINT('Ctrl Pts',(0.225854975442031,0.555720747432651,
-2.0215328854503));
#64470=CARTESIAN_POINT('Ctrl Pts',(0.316419021303705,0.509622430840941,
-2.02616942876556));
#64471=CARTESIAN_POINT('Ctrl Pts',(0.390414132784378,0.444653303022369,
-2.03080597208081));
#64472=CARTESIAN_POINT('Ctrl Pts',(0.464409244265055,0.379684175203794,
-2.03544251539606));
#64473=CARTESIAN_POINT('Ctrl Pts',(0.52183542136473,0.295844236158354,-2.04007905871132));
#64474=CARTESIAN_POINT('Ctrl Pts',(0.555678928351764,0.203373261645469,
-2.04471560202657));
#64475=CARTESIAN_POINT('Ctrl Pts',(0.589522435338797,0.110902287132586,
-2.04935214534182));
#64476=CARTESIAN_POINT('Ctrl Pts',(0.599783272213191,0.0098002771522647,
-2.05398868865707));
#64477=CARTESIAN_POINT('Ctrl Pts',(0.58520823352306,-0.0875846926311919,
-2.05862523197233));
#64478=CARTESIAN_POINT('Ctrl Pts',(0.570633194832929,-0.184969662414646,
-2.06326177528758));
#64479=CARTESIAN_POINT('Ctrl Pts',(0.531222280578273,-0.278637592001229,
-2.06789831860283));
#64480=CARTESIAN_POINT('Ctrl Pts',(0.471788935628397,-0.357148365788093,
-2.07253486191809));
#64481=CARTESIAN_POINT('Ctrl Pts',(0.412355590678518,-0.435659139574962,
-2.07717140523334));
#64482=CARTESIAN_POINT('Ctrl Pts',(0.332899815033417,-0.499012757562111,
-2.08180794854859));
#64483=CARTESIAN_POINT('Ctrl Pts',(0.243125925450237,-0.539471537099453,
-2.08644449186384));
#64484=CARTESIAN_POINT('Ctrl Pts',(0.15335203586706,-0.579930316636794,
-2.0910810351791));
#64485=CARTESIAN_POINT('Ctrl Pts',(0.0532600323458043,-0.59749425772433,
-2.09571757849435));
#64486=CARTESIAN_POINT('Ctrl Pts',(-0.0449253664050277,-0.59001819160078,
-2.10035412180961));
#64487=CARTESIAN_POINT('Ctrl Pts',(-0.14311076515586,-0.58254212547723,
-2.10499066512486));
#64488=CARTESIAN_POINT('Ctrl Pts',(-0.23938955913627,-0.550026052142593,
-2.10962720844011));
#64489=CARTESIAN_POINT('Ctrl Pts',(-0.322002755293884,-0.496441316320094,
-2.11426375175536));
#64490=CARTESIAN_POINT('Ctrl Pts',(-0.404615951451499,-0.442856580497594,
-2.11890029507062));
#64491=CARTESIAN_POINT('Ctrl Pts',(-0.473563549786321,-0.368203182187231,
-2.12353683838587));
#64492=CARTESIAN_POINT('Ctrl Pts',(-0.520424647872401,-0.281598900660794,
-2.12817338170112));
#64493=CARTESIAN_POINT('Ctrl Pts',(-0.56696390552393,-0.195589414406746,
-2.13277808139392));
#64494=CARTESIAN_POINT('Ctrl Pts',(-0.591718999800854,-0.0977926377482492,
-2.13738278108671));
#64495=CARTESIAN_POINT('Ctrl Pts',(-0.591726006610465,7.22189647403126E-7,
-2.14198748077951));
#64496=CARTESIAN_POINT('Ctrl Pts',(-0.591722112168784,5.38077801797166E-6,
-2.16716251922049));
#64497=CARTESIAN_POINT('Ctrl Pts',(-0.5916777496005,-0.0932992832067527,
-2.16276925847936));
#64498=CARTESIAN_POINT('Ctrl Pts',(-0.569224431891521,-0.186624542965204,
-2.15837599773822));
#64499=CARTESIAN_POINT('Ctrl Pts',(-0.526702394959567,-0.269674508653324,
-2.15398273699709));
#64500=CARTESIAN_POINT('Ctrl Pts',(-0.481825644476292,-0.357323475089116,
-2.14934619368184));
#64501=CARTESIAN_POINT('Ctrl Pts',(-0.414595970039771,-0.433527622132128,
-2.14470965036659));
#64502=CARTESIAN_POINT('Ctrl Pts',(-0.333224455752003,-0.488979770095182,
-2.14007310705133));
#64503=CARTESIAN_POINT('Ctrl Pts',(-0.251852941464236,-0.544431918058235,
-2.13543656373608));
#64504=CARTESIAN_POINT('Ctrl Pts',(-0.156339587325221,-0.579132066941329,
-2.13080002042083));
#64505=CARTESIAN_POINT('Ctrl Pts',(-0.0583498995310369,-0.588842120349991,
-2.12616347710557));
#64506=CARTESIAN_POINT('Ctrl Pts',(0.0396397882631472,-0.598552173758654,
-2.12152693379032));
#64507=CARTESIAN_POINT('Ctrl Pts',(0.140105809712501,-0.583272131692884,
-2.11689039047507));
#64508=CARTESIAN_POINT('Ctrl Pts',(0.230777765496664,-0.544868219320894,
-2.11225384715982));
#64509=CARTESIAN_POINT('Ctrl Pts',(0.321449721280828,-0.506464306948905,
-2.10761730384456));
#64510=CARTESIAN_POINT('Ctrl Pts',(0.402327611399801,-0.444936524270695,
-2.10298076052931));
#64511=CARTESIAN_POINT('Ctrl Pts',(0.463533429402933,-0.367799555871825,
-2.09834421721406));
#64512=CARTESIAN_POINT('Ctrl Pts',(0.524739247406063,-0.290662587472958,
-2.0937076738988));
#64513=CARTESIAN_POINT('Ctrl Pts',(0.566272993293352,-0.19791643335343,
-2.08907113058355));
#64514=CARTESIAN_POINT('Ctrl Pts',(0.583061950538804,-0.100888628236492,
-2.0844345872683));
#64515=CARTESIAN_POINT('Ctrl Pts',(0.599850907784255,-0.00386082311955339,
-2.07979804395305));
#64516=CARTESIAN_POINT('Ctrl Pts',(0.591895076387869,0.0974486329947963,
-2.07516150063779));
#64517=CARTESIAN_POINT('Ctrl Pts',(0.560166140375257,0.19066632804626,-2.07052495732254));
#64518=CARTESIAN_POINT('Ctrl Pts',(0.528437204362642,0.28388402309773,-2.06588841400729));
#64519=CARTESIAN_POINT('Ctrl Pts',(0.472935163733799,0.369009957086312,
-2.06125187069203));
#64520=CARTESIAN_POINT('Ctrl Pts',(0.400438750161246,0.435647289493295,
-2.05661532737678));
#64521=CARTESIAN_POINT('Ctrl Pts',(0.327942336588698,0.502284621900274,
-2.05197878406153));
#64522=CARTESIAN_POINT('Ctrl Pts',(0.238451550072442,0.550433352725655,
-2.04734224074627));
#64523=CARTESIAN_POINT('Ctrl Pts',(0.142896331603534,0.574212845456986,
-2.04270569743102));
#64524=CARTESIAN_POINT('Ctrl Pts',(0.0473411131346229,0.597992338188318,
-2.03806915411577));
#64525=CARTESIAN_POINT('Ctrl Pts',(-0.0542785372869409,0.597402592825597,
-2.03343261080051));
#64526=CARTESIAN_POINT('Ctrl Pts',(-0.149551322075371,0.57251563781181,
-2.02879606748526));
#64527=CARTESIAN_POINT('Ctrl Pts',(-0.244824106863801,0.547628682798024,
-2.02415952417001));
#64528=CARTESIAN_POINT('Ctrl Pts',(-0.333750026019097,0.498444518133171,
-2.01952298085476));
#64529=CARTESIAN_POINT('Ctrl Pts',(-0.405468128522953,0.430970242854016,
-2.0148864375395));
#64530=CARTESIAN_POINT('Ctrl Pts',(-0.477186231026809,0.363495967574862,
-2.01024989422425));
#64531=CARTESIAN_POINT('Ctrl Pts',(-0.531696516879226,0.277731581681406,
-2.005613350909));
#64532=CARTESIAN_POINT('Ctrl Pts',(-0.562341382197547,0.184151902900045,
-2.00097680759374));
#64533=CARTESIAN_POINT('Ctrl Pts',(-0.581760495511739,0.124852102842694,
-1.99803871146933));
#64534=CARTESIAN_POINT('Ctrl Pts',(-0.591596366956281,0.0624140449901387,
-1.99510061534491));
#64535=CARTESIAN_POINT('Ctrl Pts',(-0.591638304234624,-1.11070860510166E-5,
-1.99216251922049));
#64536=CARTESIAN_POINT('Origin',(0.,0.,-1.97));
#64537=CARTESIAN_POINT('',(-0.591694101178176,1.39310560667294E-5,-1.79198748077951));
#64538=CARTESIAN_POINT('',(-0.591679947997511,1.52687619238092E-5,-1.81716251922049));
#64539=CARTESIAN_POINT('',(-0.591675,-7.2459289488551E-17,-1.97));
#64540=CARTESIAN_POINT('Ctrl Pts',(-0.591694101178176,1.39310560667294E-5,
-1.79198748077951));
#64541=CARTESIAN_POINT('Ctrl Pts',(-0.59171078017241,0.0166866101387685,
-1.79277240818731));
#64542=CARTESIAN_POINT('Ctrl Pts',(-0.591020216129536,0.033357911865641,
-1.79355733559511));
#64543=CARTESIAN_POINT('Ctrl Pts',(-0.589612508562732,0.049968437166311,
-1.79434226300291));
#64544=CARTESIAN_POINT('Ctrl Pts',(-0.581297221003853,0.148086325878601,
-1.79897880631816));
#64545=CARTESIAN_POINT('Ctrl Pts',(-0.547959143171164,0.244083585015765,
-1.80361534963341));
#64546=CARTESIAN_POINT('Ctrl Pts',(-0.493670015158273,0.326235606732483,
-1.80825189294867));
#64547=CARTESIAN_POINT('Ctrl Pts',(-0.439380887145383,0.408387628449198,
-1.81288843626392));
#64548=CARTESIAN_POINT('Ctrl Pts',(-0.364140708952291,0.476694412745469,
-1.81752497957917));
#64549=CARTESIAN_POINT('Ctrl Pts',(-0.27713892610541,0.5228133229018,-1.82216152289442));
#64550=CARTESIAN_POINT('Ctrl Pts',(-0.190137143258528,0.56893223305813,
-1.82679806620968));
#64551=CARTESIAN_POINT('Ctrl Pts',(-0.0913737557578566,0.592863269074521,
-1.83143460952493));
#64552=CARTESIAN_POINT('Ctrl Pts',(0.00708878796496597,0.591683618204585,
-1.83607115284018));
#64553=CARTESIAN_POINT('Ctrl Pts',(0.105551331687789,0.590503967334648,
-1.84070769615544));
#64554=CARTESIAN_POINT('Ctrl Pts',(0.203713031632762,0.564213629578384,
-1.84534423947069));
#64555=CARTESIAN_POINT('Ctrl Pts',(0.289584926368809,0.516023570572558,
-1.84998078278594));
#64556=CARTESIAN_POINT('Ctrl Pts',(0.375456821104856,0.467833511566733,
-1.8546173261012));
#64557=CARTESIAN_POINT('Ctrl Pts',(0.449038910631976,0.397743731311347,
-1.85925386941645));
#64558=CARTESIAN_POINT('Ctrl Pts',(0.501344259782448,0.314314632414194,
-1.8638904127317));
#64559=CARTESIAN_POINT('Ctrl Pts',(0.553649608932919,0.230885533517044,
-1.86852695604696));
#64560=CARTESIAN_POINT('Ctrl Pts',(0.584678217706743,0.134117115978128,
-1.87316349936221));
#64561=CARTESIAN_POINT('Ctrl Pts',(0.590640412595231,0.0358281729343923,
-1.87780004267746));
#64562=CARTESIAN_POINT('Ctrl Pts',(0.596602607483719,-0.0624607701093437,
-1.88243658599271));
#64563=CARTESIAN_POINT('Ctrl Pts',(0.57749838848687,-0.1622702386579,-1.88707312930797));
#64564=CARTESIAN_POINT('Ctrl Pts',(0.535661045929247,-0.251410021360458,
-1.89170967262322));
#64565=CARTESIAN_POINT('Ctrl Pts',(0.493823703371622,-0.340549804063018,
-1.89634621593847));
#64566=CARTESIAN_POINT('Ctrl Pts',(0.429253237253222,-0.419019900919579,
-1.90098275925373));
#64567=CARTESIAN_POINT('Ctrl Pts',(0.34983594975009,-0.477236380873183,
-1.90561930256898));
#64568=CARTESIAN_POINT('Ctrl Pts',(0.270418662246957,-0.535452860826788,
-1.91025584588423));
#64569=CARTESIAN_POINT('Ctrl Pts',(0.176154553359092,-0.573415723877436,
-1.91489238919948));
#64570=CARTESIAN_POINT('Ctrl Pts',(0.0785565529402472,-0.586488382627164,
-1.91952893251474));
#64571=CARTESIAN_POINT('Ctrl Pts',(-0.0190414474785949,-0.599561041376893,
-1.92416547582999));
#64572=CARTESIAN_POINT('Ctrl Pts',(-0.119973339428416,-0.587743495825703,
-1.92880201914524));
#64573=CARTESIAN_POINT('Ctrl Pts',(-0.211911824579722,-0.552479079757573,
-1.9334385624605));
#64574=CARTESIAN_POINT('Ctrl Pts',(-0.303850309731033,-0.51721466368944,
-1.93807510577575));
#64575=CARTESIAN_POINT('Ctrl Pts',(-0.386795388083827,-0.458503377104364,
-1.942711649091));
#64576=CARTESIAN_POINT('Ctrl Pts',(-0.450616577527191,-0.383515912348056,
-1.94734819240626));
#64577=CARTESIAN_POINT('Ctrl Pts',(-0.514437766970553,-0.30852844759175,
-1.95198473572151));
#64578=CARTESIAN_POINT('Ctrl Pts',(-0.559135067504486,-0.217264804664214,
-1.95662127903676));
#64579=CARTESIAN_POINT('Ctrl Pts',(-0.579249382429614,-0.120871452052966,
-1.96125782235201));
#64580=CARTESIAN_POINT('Ctrl Pts',(-0.587534876326536,-0.0811650768799965,
-1.96316770849451));
#64581=CARTESIAN_POINT('Ctrl Pts',(-0.591649170938044,-0.0405883012720437,
-1.96507759463701));
#64582=CARTESIAN_POINT('Ctrl Pts',(-0.591630412993812,-7.77508703958541E-6,
-1.96698748077951));
#64583=CARTESIAN_POINT('Ctrl Pts',(-0.591638304234624,-1.11070860510166E-5,
-1.99216251922049));
#64584=CARTESIAN_POINT('Ctrl Pts',(-0.591662547230624,-0.0360976814156448,
-1.99046407202966));
#64585=CARTESIAN_POINT('Ctrl Pts',(-0.588413916302922,-0.0721799429759043,
-1.98876562483882));
#64586=CARTESIAN_POINT('Ctrl Pts',(-0.581851710290273,-0.107649155620656,
-1.98706717764798));
#64587=CARTESIAN_POINT('Ctrl Pts',(-0.56393772828045,-0.204475563690727,
-1.98243063433273));
#64588=CARTESIAN_POINT('Ctrl Pts',(-0.521330319476581,-0.296733408161606,
-1.97779409101748));
#64589=CARTESIAN_POINT('Ctrl Pts',(-0.459233332030376,-0.373154793920477,
-1.97315754770223));
#64590=CARTESIAN_POINT('Ctrl Pts',(-0.39713634458417,-0.449576179679351,
-1.96852100438697));
#64591=CARTESIAN_POINT('Ctrl Pts',(-0.315549778495629,-0.510161106726214,
-1.96388446107172));
#64592=CARTESIAN_POINT('Ctrl Pts',(-0.224438194226501,-0.547510045977152,
-1.95924791775647));
#64593=CARTESIAN_POINT('Ctrl Pts',(-0.133326609957372,-0.58485898522809,
-1.95461137444121));
#64594=CARTESIAN_POINT('Ctrl Pts',(-0.032690007507657,-0.598971936683102,
-1.94997483112596));
#64595=CARTESIAN_POINT('Ctrl Pts',(0.0651803799227252,-0.588125217574187,
-1.94533828781071));
#64596=CARTESIAN_POINT('Ctrl Pts',(0.163050767353107,-0.577278498465272,
-1.94070174449545));
#64597=CARTESIAN_POINT('Ctrl Pts',(0.258154939764155,-0.541472108792431,
-1.9360652011802));
#64598=CARTESIAN_POINT('Ctrl Pts',(0.338877366295973,-0.485079255468486,
-1.93142865786495));
#64599=CARTESIAN_POINT('Ctrl Pts',(0.419599792827792,-0.42868640214454,
-1.9267921145497));
#64600=CARTESIAN_POINT('Ctrl Pts',(0.485940473480379,-0.351707085169493,
-1.92215557123444));
#64601=CARTESIAN_POINT('Ctrl Pts',(0.52979690124641,-0.263543159469671,
-1.91751902791919));
#64602=CARTESIAN_POINT('Ctrl Pts',(0.573653329012439,-0.175379233769854,
-1.91288248460394));
#64603=CARTESIAN_POINT('Ctrl Pts',(0.595025503891914,-0.0760306993452581,
-1.90824594128868));
#64604=CARTESIAN_POINT('Ctrl Pts',(0.591303139179611,0.0223685285589705,
-1.90360939797343));
#64605=CARTESIAN_POINT('Ctrl Pts',(0.587580774467307,0.120767756463208,
-1.89897285465818));
#64606=CARTESIAN_POINT('Ctrl Pts',(0.558763870163224,0.218217677847083,
-1.89433631134293));
#64607=CARTESIAN_POINT('Ctrl Pts',(0.508371973651507,0.30281626422507,-1.88969976802767));
#64608=CARTESIAN_POINT('Ctrl Pts',(0.457980077139792,0.387414850603052,
-1.88506322471242));
#64609=CARTESIAN_POINT('Ctrl Pts',(0.386013188420449,0.459162101975147,
-1.88042668139717));
#64610=CARTESIAN_POINT('Ctrl Pts',(0.30126097040329,0.509295180799135,-1.87579013808191));
#64611=CARTESIAN_POINT('Ctrl Pts',(0.216508752386129,0.559428259623125,
-1.87115359476666));
#64612=CARTESIAN_POINT('Ctrl Pts',(0.118971205071153,0.587947165899007,
-1.86651705145141));
#64613=CARTESIAN_POINT('Ctrl Pts',(0.0205610591211027,0.591368748177796,
-1.86188050813615));
#64614=CARTESIAN_POINT('Ctrl Pts',(-0.0778490868289508,0.594790330456586,
-1.8572439648209));
#64615=CARTESIAN_POINT('Ctrl Pts',(-0.177131831414078,0.573114588738283,
-1.85260742150565));
#64616=CARTESIAN_POINT('Ctrl Pts',(-0.265161294619265,0.528988885808947,
-1.84797087819039));
#64617=CARTESIAN_POINT('Ctrl Pts',(-0.353190757824444,0.484863182879615,
-1.84333433487514));
#64618=CARTESIAN_POINT('Ctrl Pts',(-0.429966939649683,0.418287518739253,
-1.83869779155989));
#64619=CARTESIAN_POINT('Ctrl Pts',(-0.486112795043358,0.337393100060878,
-1.83406124824464));
#64620=CARTESIAN_POINT('Ctrl Pts',(-0.542258650437036,0.256498681382499,
-1.82942470492938));
#64621=CARTESIAN_POINT('Ctrl Pts',(-0.577774179399147,0.161285508166105,
-1.82478816161413));
#64622=CARTESIAN_POINT('Ctrl Pts',(-0.588321699237055,0.0633824240651956,
-1.82015161829888));
#64623=CARTESIAN_POINT('Ctrl Pts',(-0.59058830028609,0.0423436171667834,
-1.81915525193941));
#64624=CARTESIAN_POINT('Ctrl Pts',(-0.591701890513321,0.0211805914592501,
-1.81815888557995));
#64625=CARTESIAN_POINT('Ctrl Pts',(-0.591679947997511,1.52687619238092E-5,
-1.81716251922049));
#64626=CARTESIAN_POINT('Origin',(0.,0.,-1.97));
#64627=CARTESIAN_POINT('',(-0.591669172308873,-1.54438390886913E-5,-1.61698748077951));
#64628=CARTESIAN_POINT('',(-0.591683400125346,-1.50610791253661E-5,-1.64216251922049));
#64629=CARTESIAN_POINT('',(-0.591675,-7.2459289488551E-17,-1.97));
#64630=CARTESIAN_POINT('Ctrl Pts',(-0.591669172308873,-1.54438390886913E-5,
-1.61698748077951));
#64631=CARTESIAN_POINT('Ctrl Pts',(-0.591594341966499,0.0739068633259733,
-1.62046722173761));
#64632=CARTESIAN_POINT('Ctrl Pts',(-0.577702068741859,0.147856503492052,
-1.6239469626957));
#64633=CARTESIAN_POINT('Ctrl Pts',(-0.550647018423414,0.216627828470594,
-1.6274267036538));
#64634=CARTESIAN_POINT('Ctrl Pts',(-0.51459780837922,0.308261438831276,
-1.63206324696905));
#64635=CARTESIAN_POINT('Ctrl Pts',(-0.455179479368241,0.390701498104475,
-1.6366997902843));
#64636=CARTESIAN_POINT('Ctrl Pts',(-0.379649078234728,0.453879204593031,
-1.64133633359956));
#64637=CARTESIAN_POINT('Ctrl Pts',(-0.304118677101214,0.517056911081587,
-1.64597287691481));
#64638=CARTESIAN_POINT('Ctrl Pts',(-0.212476203845164,0.5609722647855,-1.65060942023006));
#64639=CARTESIAN_POINT('Ctrl Pts',(-0.115914395327608,0.580261671939752,
-1.65524596354532));
#64640=CARTESIAN_POINT('Ctrl Pts',(-0.0193525868100518,0.599551079094004,
-1.65988250686057));
#64641=CARTESIAN_POINT('Ctrl Pts',(0.0821285569690107,0.594214539698594,
-1.66451905017582));
#64642=CARTESIAN_POINT('Ctrl Pts',(0.176134654907471,0.564903831025341,
-1.66915559349108));
#64643=CARTESIAN_POINT('Ctrl Pts',(0.270140752845928,0.535593122352088,
-1.67379213680633));
#64644=CARTESIAN_POINT('Ctrl Pts',(0.356671804943783,0.482308244400993,
-1.67842868012158));
#64645=CARTESIAN_POINT('Ctrl Pts',(0.425159356836724,0.411557136082785,
-1.68306522343683));
#64646=CARTESIAN_POINT('Ctrl Pts',(0.493646908729669,0.340806027764573,
-1.68770176675209));
#64647=CARTESIAN_POINT('Ctrl Pts',(0.544090960417698,0.252588689079246,
-1.69233831006734));
#64648=CARTESIAN_POINT('Ctrl Pts',(0.570330536790822,0.157679528697842,
-1.69697485338259));
#64649=CARTESIAN_POINT('Ctrl Pts',(0.596570113163946,0.062770368316437,
-1.70161139669785));
#64650=CARTESIAN_POINT('Ctrl Pts',(0.598605214222167,-0.0388306137610455,
-1.7062479400131));
#64651=CARTESIAN_POINT('Ctrl Pts',(0.576187283266596,-0.13471440000364,
-1.71088448332835));
#64652=CARTESIAN_POINT('Ctrl Pts',(0.553769352311027,-0.230598186246228,
-1.71552102664361));
#64653=CARTESIAN_POINT('Ctrl Pts',(0.50689838934167,-0.32076477665393,-1.72015756995886));
#64654=CARTESIAN_POINT('Ctrl Pts',(0.441298970925477,-0.394201691049895,
-1.72479411327411));
#64655=CARTESIAN_POINT('Ctrl Pts',(0.375699552509279,-0.467638605445864,
-1.72943065658937));
#64656=CARTESIAN_POINT('Ctrl Pts',(0.291371678646244,-0.524345843830095,
-1.73406719990462));
#64657=CARTESIAN_POINT('Ctrl Pts',(0.198614718926297,-0.557397477920656,
-1.73870374321987));
#64658=CARTESIAN_POINT('Ctrl Pts',(0.105857759206355,-0.590449112011215,
-1.74334028653512));
#64659=CARTESIAN_POINT('Ctrl Pts',(0.00467171362950315,-0.599845141808107,
-1.74797682985038));
#64660=CARTESIAN_POINT('Ctrl Pts',(-0.092585078467592,-0.584437984915107,
-1.75261337316563));
#64661=CARTESIAN_POINT('Ctrl Pts',(-0.189841870564687,-0.569030828022107,
-1.75724991648088));
#64662=CARTESIAN_POINT('Ctrl Pts',(-0.283169409182025,-0.528820484439216,
-1.76188645979614));
#64663=CARTESIAN_POINT('Ctrl Pts',(-0.361169152306093,-0.468718037191848,
-1.76652300311139));
#64664=CARTESIAN_POINT('Ctrl Pts',(-0.439168895430163,-0.408615589944479,
-1.77115954642664));
#64665=CARTESIAN_POINT('Ctrl Pts',(-0.501840843060962,-0.328621039032634,
-1.7757960897419));
#64666=CARTESIAN_POINT('Ctrl Pts',(-0.541530568233824,-0.238504504433004,
-1.78043263305715));
#64667=CARTESIAN_POINT('Ctrl Pts',(-0.574501159996734,-0.163643933833635,
-1.7842842489646));
#64668=CARTESIAN_POINT('Ctrl Pts',(-0.591612257839709,-0.0817984191520354,
-1.78813586487205));
#64669=CARTESIAN_POINT('Ctrl Pts',(-0.591694101178176,1.39310560667294E-5,
-1.79198748077951));
#64670=CARTESIAN_POINT('Ctrl Pts',(-0.591679947997511,1.52687619238092E-5,
-1.81716251922049));
#64671=CARTESIAN_POINT('Ctrl Pts',(-0.591599782062918,-0.0773112278756028,
-1.8135223422647));
#64672=CARTESIAN_POINT('Ctrl Pts',(-0.576362850266228,-0.154668384075078,
-1.80988216530891));
#64673=CARTESIAN_POINT('Ctrl Pts',(-0.546821475223447,-0.22611065368091,
-1.80624198835312));
#64674=CARTESIAN_POINT('Ctrl Pts',(-0.509194220658233,-0.317107652340668,
-1.80160544503786));
#64675=CARTESIAN_POINT('Ctrl Pts',(-0.4483602008141,-0.398508654674769,
-1.79696890172261));
#64676=CARTESIAN_POINT('Ctrl Pts',(-0.371749367678615,-0.46037176401698,
-1.79233235840736));
#64677=CARTESIAN_POINT('Ctrl Pts',(-0.295138534543124,-0.522234873359194,
-1.78769581509211));
#64678=CARTESIAN_POINT('Ctrl Pts',(-0.202750888116276,-0.564560089709517,
-1.78305927177685));
#64679=CARTESIAN_POINT('Ctrl Pts',(-0.105870176849256,-0.5821780304404,
-1.7784227284616));
#64680=CARTESIAN_POINT('Ctrl Pts',(-0.00898946558223347,-0.599795971171284,
-1.77378618514635));
#64681=CARTESIAN_POINT('Ctrl Pts',(0.0923843105249564,-0.592706636282727,
-1.76914964183109));
#64682=CARTESIAN_POINT('Ctrl Pts',(0.185869883701361,-0.561775880406411,
-1.76451309851584));
#64683=CARTESIAN_POINT('Ctrl Pts',(0.279355456877761,-0.530845124530096,
-1.75987655520059));
#64684=CARTESIAN_POINT('Ctrl Pts',(0.36495282712337,-0.476072947666023,
-1.75524001188534));
#64685=CARTESIAN_POINT('Ctrl Pts',(0.43220757513767,-0.404148939708088,
-1.75060346857008));
#64686=CARTESIAN_POINT('Ctrl Pts',(0.499462323151974,-0.332224931750148,
-1.74596692525483));
#64687=CARTESIAN_POINT('Ctrl Pts',(0.548374448934968,-0.243149092698343,
-1.74133038193958));
#64688=CARTESIAN_POINT('Ctrl Pts',(0.572970078869414,-0.147800684010369,
-1.73669383862432));
#64689=CARTESIAN_POINT('Ctrl Pts',(0.59756570880386,-0.0524522753223972,
-1.73205729530907));
#64690=CARTESIAN_POINT('Ctrl Pts',(0.59784484288976,0.0491687030017455,
-1.72742075199382));
#64691=CARTESIAN_POINT('Ctrl Pts',(0.573773389136127,0.14465079119313,-1.72278420867856));
#64692=CARTESIAN_POINT('Ctrl Pts',(0.549701935382493,0.240132879384514,
-1.71814766536331));
#64693=CARTESIAN_POINT('Ctrl Pts',(0.501279893789324,0.329476077443143,
-1.71351112204806));
#64694=CARTESIAN_POINT('Ctrl Pts',(0.434421281630162,0.40176847006748,-1.7088745787328));
#64695=CARTESIAN_POINT('Ctrl Pts',(0.367562669471001,0.474060862691815,
-1.70423803541755));
#64696=CARTESIAN_POINT('Ctrl Pts',(0.282267486745845,0.529302449881861,
-1.6996014921023));
#64697=CARTESIAN_POINT('Ctrl Pts',(0.188953245137173,0.560746310398639,
-1.69496494878705));
#64698=CARTESIAN_POINT('Ctrl Pts',(0.0956390035284988,0.592190170915418,
-1.69032840547179));
#64699=CARTESIAN_POINT('Ctrl Pts',(-0.00569429696368506,0.599836304758928,
-1.68569186215654));
#64700=CARTESIAN_POINT('Ctrl Pts',(-0.10267033205033,0.582750852758047,
-1.68105531884129));
#64701=CARTESIAN_POINT('Ctrl Pts',(-0.199646367136978,0.565665400757165,
-1.67641877552603));
#64702=CARTESIAN_POINT('Ctrl Pts',(-0.292265136818081,0.523848362911888,
-1.67178223221078));
#64703=CARTESIAN_POINT('Ctrl Pts',(-0.369214664445686,0.462407055560158,
-1.66714568889553));
#64704=CARTESIAN_POINT('Ctrl Pts',(-0.446164192073286,0.400965748208432,
-1.66250914558028));
#64705=CARTESIAN_POINT('Ctrl Pts',(-0.507444477647392,0.319900171350254,
-1.65787260226502));
#64706=CARTESIAN_POINT('Ctrl Pts',(-0.545571064596393,0.22911125452215,
-1.65323605894977));
#64707=CARTESIAN_POINT('Ctrl Pts',(-0.575923868874289,0.156833653939345,
-1.64954487904001));
#64708=CARTESIAN_POINT('Ctrl Pts',(-0.59160221209113,0.0783935487786571,
-1.64585369913025));
#64709=CARTESIAN_POINT('Ctrl Pts',(-0.591683400125346,-1.50610791253661E-5,
-1.64216251922049));
#64710=CARTESIAN_POINT('Origin',(0.,0.,-1.97));
#64711=CARTESIAN_POINT('',(-0.591646097050001,1.31033435099431E-5,-1.44198748077951));
#64712=CARTESIAN_POINT('',(-0.591636138149344,1.03689755184515E-5,-1.46716251922049));
#64713=CARTESIAN_POINT('',(-0.591675,-7.2459289488551E-17,-1.97));
#64714=CARTESIAN_POINT('Ctrl Pts',(-0.591646097050001,1.31033435099431E-5,
-1.44198748077951));
#64715=CARTESIAN_POINT('Ctrl Pts',(-0.59167246821368,0.0326896924703124,
-1.44352549197265));
#64716=CARTESIAN_POINT('Ctrl Pts',(-0.589011448984827,0.0653620312304001,
-1.44506350316579));
#64717=CARTESIAN_POINT('Ctrl Pts',(-0.583625010676761,0.0975786958256344,
-1.44660151435893));
#64718=CARTESIAN_POINT('Ctrl Pts',(-0.567386861928784,0.194700200230078,
-1.45123805767419));
#64719=CARTESIAN_POINT('Ctrl Pts',(-0.526380028614879,0.287680525121921,
-1.45587460098944));
#64720=CARTESIAN_POINT('Ctrl Pts',(-0.465612872889403,0.365163535373068,
-1.46051114430469));
#64721=CARTESIAN_POINT('Ctrl Pts',(-0.404845717163926,0.442646545624216,
-1.46514768761995));
#64722=CARTESIAN_POINT('Ctrl Pts',(-0.324318239026884,0.50463224123467,
-1.4697842309352));
#64723=CARTESIAN_POINT('Ctrl Pts',(-0.233865647425011,0.543550010505898,
-1.47442077425045));
#64724=CARTESIAN_POINT('Ctrl Pts',(-0.143413055823141,0.582467779777125,
-1.4790573175657));
#64725=CARTESIAN_POINT('Ctrl Pts',(-0.0430353507564487,0.598317622709121,
-1.48369386088096));
#64726=CARTESIAN_POINT('Ctrl Pts',(0.0550078549600969,0.589163721608154,
-1.48833040419621));
#64727=CARTESIAN_POINT('Ctrl Pts',(0.153051060676642,0.580009820507187,
-1.49296694751146));
#64728=CARTESIAN_POINT('Ctrl Pts',(0.24875976704304,0.545852175373257,-1.49760349082671));
#64729=CARTESIAN_POINT('Ctrl Pts',(0.33044460855433,0.49086262400376,-1.50224003414197));
#64730=CARTESIAN_POINT('Ctrl Pts',(0.412129450065623,0.435873072634261,
-1.50687657745722));
#64731=CARTESIAN_POINT('Ctrl Pts',(0.479790426721806,0.360051615029195,
-1.51151312077248));
#64732=CARTESIAN_POINT('Ctrl Pts',(0.525163777402457,0.272658691170599,
-1.51614966408773));
#64733=CARTESIAN_POINT('Ctrl Pts',(0.570537128083106,0.185265767312005,
-1.52078620740298));
#64734=CARTESIAN_POINT('Ctrl Pts',(0.593622852788224,0.0863013771998743,
-1.52542275071823));
#64735=CARTESIAN_POINT('Ctrl Pts',(0.59160138071521,-0.0121474813166226,
-1.53005929403348));
#64736=CARTESIAN_POINT('Ctrl Pts',(0.589579908642197,-0.110596339833122,
-1.53469583734874));
#64737=CARTESIAN_POINT('Ctrl Pts',(0.562451239791054,-0.208529666753994,
-1.53933238066399));
#64738=CARTESIAN_POINT('Ctrl Pts',(0.513528729214872,-0.293986392946068,
-1.54396892397925));
#64739=CARTESIAN_POINT('Ctrl Pts',(0.46460621863869,-0.379443119138142,
-1.5486054672945));
#64740=CARTESIAN_POINT('Ctrl Pts',(0.393889866337471,-0.452423244601417,
-1.55324201060975));
#64741=CARTESIAN_POINT('Ctrl Pts',(0.310016601182262,-0.504013354940005,
-1.557878553925));
#64742=CARTESIAN_POINT('Ctrl Pts',(0.226143336027052,-0.555603465278593,
-1.56251509724026));
#64743=CARTESIAN_POINT('Ctrl Pts',(0.129113158017854,-0.585803560492493,
-1.56715164055551));
#64744=CARTESIAN_POINT('Ctrl Pts',(0.0307768303592042,-0.59092515742649,
-1.57178818387076));
#64745=CARTESIAN_POINT('Ctrl Pts',(-0.0675594972994458,-0.596046754360487,
-1.57642472718602));
#64746=CARTESIAN_POINT('Ctrl Pts',(-0.167201974607546,-0.576089853014582,
-1.58106127050127));
#64747=CARTESIAN_POINT('Ctrl Pts',(-0.255980785659163,-0.533491885917489,
-1.58569781381652));
#64748=CARTESIAN_POINT('Ctrl Pts',(-0.34475959671078,-0.490893918820396,
-1.59033435713178));
#64749=CARTESIAN_POINT('Ctrl Pts',(-0.422674741505912,-0.425654885972116,
-1.59497090044703));
#64750=CARTESIAN_POINT('Ctrl Pts',(-0.480210067957043,-0.345742744825069,
-1.59960744376228));
#64751=CARTESIAN_POINT('Ctrl Pts',(-0.537745394408174,-0.265830603678023,
-1.60424398707753));
#64752=CARTESIAN_POINT('Ctrl Pts',(-0.574900902515302,-0.171245354232211,
-1.60888053039279));
#64753=CARTESIAN_POINT('Ctrl Pts',(-0.58713861103016,-0.0735391487852222,
-1.61351707370804));
#64754=CARTESIAN_POINT('Ctrl Pts',(-0.590191879185685,-0.0491617708368692,
-1.6146738760652));
#64755=CARTESIAN_POINT('Ctrl Pts',(-0.59169404884925,-0.0245901177026608,
-1.61583067842235));
#64756=CARTESIAN_POINT('Ctrl Pts',(-0.591669172308873,-1.54438390886913E-5,
-1.61698748077951));
#64757=CARTESIAN_POINT('Ctrl Pts',(-0.591683400125346,-1.50610791253661E-5,
-1.64216251922049));
#64758=CARTESIAN_POINT('Ctrl Pts',(-0.591704193529728,-0.0200966155542075,
-1.641217155815));
#64759=CARTESIAN_POINT('Ctrl Pts',(-0.590701899995329,-0.0401761041119696,
-1.6402717924095));
#64760=CARTESIAN_POINT('Ctrl Pts',(-0.58866101856647,-0.0601494696056588,
-1.63932642900401));
#64761=CARTESIAN_POINT('Ctrl Pts',(-0.578651497263644,-0.158109020107328,
-1.63468988568876));
#64762=CARTESIAN_POINT('Ctrl Pts',(-0.543659566334094,-0.253515864312632,
-1.63005334237351));
#64763=CARTESIAN_POINT('Ctrl Pts',(-0.487958958919651,-0.334717504596945,
-1.62541679905825));
#64764=CARTESIAN_POINT('Ctrl Pts',(-0.43225835150521,-0.415919144881255,
-1.620780255743));
#64765=CARTESIAN_POINT('Ctrl Pts',(-0.355849067605877,-0.482915581244573,
-1.61614371242774));
#64766=CARTESIAN_POINT('Ctrl Pts',(-0.268063341261597,-0.527524216074698,
-1.61150716911249));
#64767=CARTESIAN_POINT('Ctrl Pts',(-0.180277614917312,-0.572132850904825,
-1.60687062579724));
#64768=CARTESIAN_POINT('Ctrl Pts',(-0.0811154461280793,-0.594353684201755,
-1.60223408248199));
#64769=CARTESIAN_POINT('Ctrl Pts',(0.0173120115940635,-0.59147277851827,
-1.59759753916673));
#64770=CARTESIAN_POINT('Ctrl Pts',(0.115739469316201,-0.588591872834785,
-1.59296099585148));
#64771=CARTESIAN_POINT('Ctrl Pts',(0.213432215971247,-0.560609228170888,
-1.58832445253623));
#64772=CARTESIAN_POINT('Ctrl Pts',(0.298458565653194,-0.510942499760779,
-1.58368790922097));
#64773=CARTESIAN_POINT('Ctrl Pts',(0.383484915335141,-0.46127577135067,
-1.57905136590572));
#64774=CARTESIAN_POINT('Ctrl Pts',(0.455844868043987,-0.389924959194351,
-1.57441482259047));
#64775=CARTESIAN_POINT('Ctrl Pts',(0.506700754070803,-0.305604481802273,
-1.56977827927522));
#64776=CARTESIAN_POINT('Ctrl Pts',(0.557556640097621,-0.221284004410191,
-1.56514173595996));
#64777=CARTESIAN_POINT('Ctrl Pts',(0.586908459442404,-0.123993861782351,
-1.56050519264471));
#64778=CARTESIAN_POINT('Ctrl Pts',(0.591171332969464,-0.0256165678548721,
-1.55586864932946));
#64779=CARTESIAN_POINT('Ctrl Pts',(0.595434206496523,0.0727607260726045,
-1.5512321060142));
#64780=CARTESIAN_POINT('Ctrl Pts',(0.574608134205857,0.172225171299727,
-1.54659556269895));
#64781=CARTESIAN_POINT('Ctrl Pts',(0.531236704661987,0.260628695836489,
-1.5419590193837));
#64782=CARTESIAN_POINT('Ctrl Pts',(0.487865275118117,0.349032220373248,
-1.53732247606844));
#64783=CARTESIAN_POINT('Ctrl Pts',(0.421948488321044,0.426374824219655,
-1.53268593275319));
#64784=CARTESIAN_POINT('Ctrl Pts',(0.341537079078881,0.483210282473192,
-1.52804938943794));
#64785=CARTESIAN_POINT('Ctrl Pts',(0.261125669836717,0.540045740726729,
-1.52341284612269));
#64786=CARTESIAN_POINT('Ctrl Pts',(0.166219638149465,0.576374053387396,
-1.51877630280743));
#64787=CARTESIAN_POINT('Ctrl Pts',(0.0684103149956289,0.58775826857285,
-1.51413975949218));
#64788=CARTESIAN_POINT('Ctrl Pts',(-0.02939900815821,0.599142483758304,
-1.50950321617693));
#64789=CARTESIAN_POINT('Ctrl Pts',(-0.130111622778631,0.585582601468544,
-1.50486667286167));
#64790=CARTESIAN_POINT('Ctrl Pts',(-0.221427011933022,0.548734755469315,
-1.50023012954642));
#64791=CARTESIAN_POINT('Ctrl Pts',(-0.312742401087413,0.511886909470086,
-1.49559358623117));
#64792=CARTESIAN_POINT('Ctrl Pts',(-0.394660564775773,0.451751099761389,
-1.49095704291591));
#64793=CARTESIAN_POINT('Ctrl Pts',(-0.457176442923603,0.375672002562444,
-1.48632049960066));
#64794=CARTESIAN_POINT('Ctrl Pts',(-0.519692321071433,0.2995929053635,-1.48168395628541));
#64795=CARTESIAN_POINT('Ctrl Pts',(-0.562805913678733,0.207570520674309,
-1.47704741297016));
#64796=CARTESIAN_POINT('Ctrl Pts',(-0.581251549926701,0.110843985769928,
-1.4724108696549));
#64797=CARTESIAN_POINT('Ctrl Pts',(-0.588211416105208,0.0743473461422587,
-1.4706614195101));
#64798=CARTESIAN_POINT('Ctrl Pts',(-0.591659337574339,0.0371809827961072,
-1.46891196936529));
#64799=CARTESIAN_POINT('Ctrl Pts',(-0.591636138149344,1.03689755184515E-5,
-1.46716251922049));
#64800=CARTESIAN_POINT('Origin',(0.,0.,-1.97));
#64801=CARTESIAN_POINT('',(-0.591715913879701,-8.55716902248283E-6,-1.26698748077951));
#64802=CARTESIAN_POINT('',(-0.591723545535282,-4.29287131388572E-6,-1.29216251922049));
#64803=CARTESIAN_POINT('',(-0.591675,-7.2459289488551E-17,-1.97));
#64804=CARTESIAN_POINT('Ctrl Pts',(-0.591715913879701,-8.55716902248283E-6,
-1.26698748077951));
#64805=CARTESIAN_POINT('Ctrl Pts',(-0.591652719613147,0.0898914806554165,
-1.27122030552295));
#64806=CARTESIAN_POINT('Ctrl Pts',(-0.570864102899966,0.17981974451662,
-1.27545313026639));
#64807=CARTESIAN_POINT('Ctrl Pts',(-0.53128372471532,0.260532836354837,
-1.27968595500982));
#64808=CARTESIAN_POINT('Ctrl Pts',(-0.487928247224393,0.348944185536248,
-1.28432249832508));
#64809=CARTESIAN_POINT('Ctrl Pts',(-0.422025416978272,0.426298682244433,
-1.28895904164033));
#64810=CARTESIAN_POINT('Ctrl Pts',(-0.341624264204252,0.483148649044355,
-1.29359558495558));
#64811=CARTESIAN_POINT('Ctrl Pts',(-0.261223111430231,0.539998615844276,
-1.29823212827084));
#64812=CARTESIAN_POINT('Ctrl Pts',(-0.166323636128309,0.576344052735935,
-1.30286867158609));
#64813=CARTESIAN_POINT('Ctrl Pts',(-0.0685163685140617,0.58774591637214,
-1.30750521490134));
#64814=CARTESIAN_POINT('Ctrl Pts',(0.0292908991001856,0.599147780008344,
-1.3121417582166));
#64815=CARTESIAN_POINT('Ctrl Pts',(0.13000595902676,0.585606070389094,-1.31677830153185));
#64816=CARTESIAN_POINT('Ctrl Pts',(0.221327995676024,0.548774701764317,
-1.3214148448471));
#64817=CARTESIAN_POINT('Ctrl Pts',(0.312650032325287,0.51194333313954,-1.32605138816235));
#64818=CARTESIAN_POINT('Ctrl Pts',(0.39457904569724,0.451822305509234,-1.33068793147761));
#64819=CARTESIAN_POINT('Ctrl Pts',(0.457108650593243,0.375754489686159,
-1.33532447479286));
#64820=CARTESIAN_POINT('Ctrl Pts',(0.519638255489244,0.299686673863085,
-1.33996101810811));
#64821=CARTESIAN_POINT('Ctrl Pts',(0.562768451909297,0.207672069847241,
-1.34459756142337));
#64822=CARTESIAN_POINT('Ctrl Pts',(0.58123154113094,0.110948864622555,-1.34923410473862));
#64823=CARTESIAN_POINT('Ctrl Pts',(0.599694630352582,0.0142256593978662,
-1.35387064805387));
#64824=CARTESIAN_POINT('Ctrl Pts',(0.593490612375815,-0.0872061470356578,
-1.35850719136912));
#64825=CARTESIAN_POINT('Ctrl Pts',(0.563377213811757,-0.180958199383677,
-1.36314373468438));
#64826=CARTESIAN_POINT('Ctrl Pts',(0.533263815247699,-0.274710251731697,
-1.36778027799963));
#64827=CARTESIAN_POINT('Ctrl Pts',(0.479241036096351,-0.360782549994205,
-1.37241682131488));
#64828=CARTESIAN_POINT('Ctrl Pts',(0.407906938697792,-0.42866266962342,
-1.37705336463014));
#64829=CARTESIAN_POINT('Ctrl Pts',(0.336572841299233,-0.496542789252635,
-1.38168990794539));
#64830=CARTESIAN_POINT('Ctrl Pts',(0.247927425653462,-0.546230730248557,
-1.38632645126064));
#64831=CARTESIAN_POINT('Ctrl Pts',(0.152797383533493,-0.571657864943534,
-1.3909629945759));
#64832=CARTESIAN_POINT('Ctrl Pts',(0.0576673414135263,-0.59708499963851,
-1.39559953789115));
#64833=CARTESIAN_POINT('Ctrl Pts',(-0.043947327180648,-0.598251328032543,
-1.4002360812064));
#64834=CARTESIAN_POINT('Ctrl Pts',(-0.139635933117813,-0.575014400818622,
-1.40487262452166));
#64835=CARTESIAN_POINT('Ctrl Pts',(-0.235324539054983,-0.551777473604699,
-1.40950916783691));
#64836=CARTESIAN_POINT('Ctrl Pts',(-0.325087082335145,-0.504137290782826,
-1.41414571115216));
#64837=CARTESIAN_POINT('Ctrl Pts',(-0.397960431004153,-0.437912377447213,
-1.41878225446741));
#64838=CARTESIAN_POINT('Ctrl Pts',(-0.47083377967316,-0.3716874641116,-1.42341879778267));
#64839=CARTESIAN_POINT('Ctrl Pts',(-0.526817933731005,-0.286877820262249,
-1.42805534109792));
#64840=CARTESIAN_POINT('Ctrl Pts',(-0.5590752786689,-0.193841656379048,
-1.43269188441317));
#64841=CARTESIAN_POINT('Ctrl Pts',(-0.580632376849192,-0.131666988159784,
-1.43579041653529));
#64842=CARTESIAN_POINT('Ctrl Pts',(-0.591592968764511,-0.065818316806051,
-1.4388889486574));
#64843=CARTESIAN_POINT('Ctrl Pts',(-0.591646097050001,1.31033435099431E-5,
-1.44198748077951));
#64844=CARTESIAN_POINT('Ctrl Pts',(-0.591636138149344,1.03689755184515E-5,
-1.46716251922049));
#64845=CARTESIAN_POINT('Ctrl Pts',(-0.59159785246189,-0.0613317765103333,
-1.46427542605004));
#64846=CARTESIAN_POINT('Ctrl Pts',(-0.582106163230953,-0.122685497925498,
-1.46138833287959));
#64847=CARTESIAN_POINT('Ctrl Pts',(-0.563344551531624,-0.181059851245905,
-1.45850123970914));
#64848=CARTESIAN_POINT('Ctrl Pts',(-0.533214236999943,-0.274806468237785,
-1.45386469639389));
#64849=CARTESIAN_POINT('Ctrl Pts',(-0.479175928047944,-0.360869017101977,
-1.44922815307864));
#64850=CARTESIAN_POINT('Ctrl Pts',(-0.407829583745096,-0.428736264031698,
-1.44459160976339));
#64851=CARTESIAN_POINT('Ctrl Pts',(-0.336483239442246,-0.49660351096142,
-1.43995506644813));
#64852=CARTESIAN_POINT('Ctrl Pts',(-0.247828859788544,-0.546275455956669,
-1.43531852313288));
#64853=CARTESIAN_POINT('Ctrl Pts',(-0.152694231374487,-0.571685425018436,
-1.43068197981763));
#64854=CARTESIAN_POINT('Ctrl Pts',(-0.0575596029604325,-0.597095394080203,
-1.42604543650237));
#64855=CARTESIAN_POINT('Ctrl Pts',(0.0440552742139777,-0.59824338720849,
-1.42140889318712));
#64856=CARTESIAN_POINT('Ctrl Pts',(0.139739685542633,-0.574989194470645,
-1.41677234987187));
#64857=CARTESIAN_POINT('Ctrl Pts',(0.235424096871292,-0.5517350017328,-1.41213580655661));
#64858=CARTESIAN_POINT('Ctrl Pts',(0.325178042354196,-0.504078623128823,
-1.40749926324136));
#64859=CARTESIAN_POINT('Ctrl Pts',(0.398039440127595,-0.437840561821843,
-1.40286271992611));
#64860=CARTESIAN_POINT('Ctrl Pts',(0.470900837900994,-0.371602500514862,
-1.39822617661086));
#64861=CARTESIAN_POINT('Ctrl Pts',(0.526869687964888,-0.28678275650488,
-1.3935896332956));
#64862=CARTESIAN_POINT('Ctrl Pts',(0.559110244961018,-0.193740773853068,
-1.38895308998035));
#64863=CARTESIAN_POINT('Ctrl Pts',(0.591350801957148,-0.100698791201256,
-1.3843165466651));
#64864=CARTESIAN_POINT('Ctrl Pts',(0.599863065885513,0.000565430092384633,
-1.37968000334984));
#64865=CARTESIAN_POINT('Ctrl Pts',(0.58360739293406,0.0976840027141863,
-1.37504346003459));
#64866=CARTESIAN_POINT('Ctrl Pts',(0.567351719982608,0.194802575335988,
-1.37040691671934));
#64867=CARTESIAN_POINT('Ctrl Pts',(0.526328110151338,0.28777549928595,-1.36577037340408));
#64868=CARTESIAN_POINT('Ctrl Pts',(0.465546974591508,0.365247543348685,
-1.36113383008883));
#64869=CARTESIAN_POINT('Ctrl Pts',(0.404765839031678,0.44271958741142,-1.35649728677358));
#64870=CARTESIAN_POINT('Ctrl Pts',(0.324227177743289,0.504690751586928,
-1.35186074345833));
#64871=CARTESIAN_POINT('Ctrl Pts',(0.233767565525252,0.543592198970839,
-1.34722420014307));
#64872=CARTESIAN_POINT('Ctrl Pts',(0.143307953307216,0.58249364635475,-1.34258765682782));
#64873=CARTESIAN_POINT('Ctrl Pts',(0.0429273901595324,0.598325376947065,
-1.33795111351257));
#64874=CARTESIAN_POINT('Ctrl Pts',(-0.0551141620316234,0.589153785201375,
-1.33331457019731));
#64875=CARTESIAN_POINT('Ctrl Pts',(-0.153155714222779,0.579982193455684,
-1.32867802688206));
#64876=CARTESIAN_POINT('Ctrl Pts',(-0.248858255457407,0.545807279371989,
-1.32404148356681));
#64877=CARTESIAN_POINT('Ctrl Pts',(-0.330533173207798,0.490802989887734,
-1.31940494025155));
#64878=CARTESIAN_POINT('Ctrl Pts',(-0.412208090958186,0.435798700403481,
-1.3147683969363));
#64879=CARTESIAN_POINT('Ctrl Pts',(-0.479855385224338,0.359965035518671,
-1.31013185362105));
#64880=CARTESIAN_POINT('Ctrl Pts',(-0.525212965982056,0.272563926149239,
-1.3054953103058));
#64881=CARTESIAN_POINT('Ctrl Pts',(-0.568689546648524,0.188787381669575,
-1.30105104661069));
#64882=CARTESIAN_POINT('Ctrl Pts',(-0.591686809655619,0.0943829136852825,
-1.29660678291559));
#64883=CARTESIAN_POINT('Ctrl Pts',(-0.591723545535282,-4.29287131388572E-6,
-1.29216251922049));
#64884=CARTESIAN_POINT('Origin',(0.,0.,-1.97));
#64885=CARTESIAN_POINT('',(-0.591624151837836,5.41149558302978E-7,-1.09198748077951));
#64886=CARTESIAN_POINT('',(-0.591625419221713,-3.63663382748259E-6,-1.11716251922049));
#64887=CARTESIAN_POINT('',(-0.591675,-7.2459289488551E-17,-1.97));
#64888=CARTESIAN_POINT('Ctrl Pts',(-0.591624151837836,5.41149558302978E-7,
-1.09198748077951));
#64889=CARTESIAN_POINT('Ctrl Pts',(-0.591625697888236,0.0486823199268314,
-1.09427857575799));
#64890=CARTESIAN_POINT('Ctrl Pts',(-0.585685602356747,0.0973637280149376,
-1.09656967073648));
#64891=CARTESIAN_POINT('Ctrl Pts',(-0.573799481656066,0.144547258077456,
-1.09886076571496));
#64892=CARTESIAN_POINT('Ctrl Pts',(-0.549745256930946,0.240033688345932,
-1.10349730903021));
#64893=CARTESIAN_POINT('Ctrl Pts',(-0.501339337015882,0.32938562236306,
-1.10813385234546));
#64894=CARTESIAN_POINT('Ctrl Pts',(-0.434493770166178,0.4016900778626,-1.11277039566072));
#64895=CARTESIAN_POINT('Ctrl Pts',(-0.367648203316469,0.473994533362146,
-1.11740693897597));
#64896=CARTESIAN_POINT('Ctrl Pts',(-0.282362989532117,0.5292515103441,-1.12204348229122));
#64897=CARTESIAN_POINT('Ctrl Pts',(-0.189054422940825,0.560712207940038,
-1.12668002560648));
#64898=CARTESIAN_POINT('Ctrl Pts',(-0.0957458563495401,0.592172905535974,
-1.13131656892173));
#64899=CARTESIAN_POINT('Ctrl Pts',(0.00558606304868453,0.599837323745897,
-1.13595311223698));
#64900=CARTESIAN_POINT('Ctrl Pts',(0.102565179644448,0.582769370240907,
-1.14058965555223));
#64901=CARTESIAN_POINT('Ctrl Pts',(0.199544296240211,0.565701416735917,
-1.14522619886749));
#64902=CARTESIAN_POINT('Ctrl Pts',(0.292170610033512,0.523901091516013,
-1.14986274218274));
#64903=CARTESIAN_POINT('Ctrl Pts',(0.369131222977626,0.462473669725665,
-1.15449928549799));
#64904=CARTESIAN_POINT('Ctrl Pts',(0.446091835921745,0.401046247935313,
-1.15913582881325));
#64905=CARTESIAN_POINT('Ctrl Pts',(0.507386748016674,0.319991729574514,
-1.1637723721285));
#64906=CARTESIAN_POINT('Ctrl Pts',(0.545529716283336,0.229209693552223,
-1.16840891544375));
#64907=CARTESIAN_POINT('Ctrl Pts',(0.583672684549996,0.138427657529934,
-1.17304545875901));
#64908=CARTESIAN_POINT('Ctrl Pts',(0.598663708988391,0.0379181038461522,
-1.17768200207426));
#64909=CARTESIAN_POINT('Ctrl Pts',(0.588671863545843,-0.0600432513772004,
-1.18231854538951));
#64910=CARTESIAN_POINT('Ctrl Pts',(0.578680018103295,-0.158004606600553,
-1.18695508870476));
#64911=CARTESIAN_POINT('Ctrl Pts',(0.543705302779803,-0.253417763363477,
-1.19159163202002));
#64912=CARTESIAN_POINT('Ctrl Pts',(0.488019348092275,-0.334629453058263,
-1.19622817533527));
#64913=CARTESIAN_POINT('Ctrl Pts',(0.432333393404748,-0.415841142753046,
-1.20086471865052));
#64914=CARTESIAN_POINT('Ctrl Pts',(0.355936199353185,-0.482851365379693,
-1.20550126196578));
#64915=CARTESIAN_POINT('Ctrl Pts',(0.268158523386165,-0.527475839543227,
-1.21013780528103));
#64916=CARTESIAN_POINT('Ctrl Pts',(0.180380847419145,-0.572100313706762,
-1.21477434859628));
#64917=CARTESIAN_POINT('Ctrl Pts',(0.0812226895366682,-0.594339039407184,
-1.21941089191153));
#64918=CARTESIAN_POINT('Ctrl Pts',(-0.0172052866205986,-0.591475893911818,
-1.22404743522679));
#64919=CARTESIAN_POINT('Ctrl Pts',(-0.115633262777868,-0.588612748416452,
-1.22868397854204));
#64920=CARTESIAN_POINT('Ctrl Pts',(-0.213331057209928,-0.560647731725296,
-1.2333205218573));
#64921=CARTESIAN_POINT('Ctrl Pts',(-0.298366367501436,-0.510996346083296,
-1.23795706517255));
#64922=CARTESIAN_POINT('Ctrl Pts',(-0.383401677792944,-0.461344960441296,
-1.2425936084878));
#64923=CARTESIAN_POINT('Ctrl Pts',(-0.4557745039439,-0.390007205848451,
-1.24723015180305));
#64924=CARTESIAN_POINT('Ctrl Pts',(-0.506645603949854,-0.30569590603207,
-1.25186669511831));
#64925=CARTESIAN_POINT('Ctrl Pts',(-0.557516703955809,-0.221384606215688,
-1.25650323843356));
#64926=CARTESIAN_POINT('Ctrl Pts',(-0.586886077816762,-0.124099761175768,
-1.26113978174881));
#64927=CARTESIAN_POINT('Ctrl Pts',(-0.591166702379371,-0.0257232378284896,
-1.26577632506407));
#64928=CARTESIAN_POINT('Ctrl Pts',(-0.591539429973483,-0.0171572810789546,
-1.26618004363588));
#64929=CARTESIAN_POINT('Ctrl Pts',(-0.591721941225643,-0.00858304750972869,
-1.26658376220769));
#64930=CARTESIAN_POINT('Ctrl Pts',(-0.591715913879701,-8.55716902248283E-6,
-1.26698748077951));
#64931=CARTESIAN_POINT('Ctrl Pts',(-0.591723545535282,-4.29287131388572E-6,
-1.29216251922049));
#64932=CARTESIAN_POINT('Ctrl Pts',(-0.591725134901142,-0.00408792459727398,
-1.29197023960034));
#64933=CARTESIAN_POINT('Ctrl Pts',(-0.591683746017117,-0.00817152401274099,
-1.29177795998019));
#64934=CARTESIAN_POINT('Ctrl Pts',(-0.59159917794444,-0.0122542290259055,
-1.29158568036004));
#64935=CARTESIAN_POINT('Ctrl Pts',(-0.589559941899822,-0.11070272097756,
-1.28694913704478));
#64936=CARTESIAN_POINT('Ctrl Pts',(-0.562413602561303,-0.208631151026815,
-1.28231259372953));
#64937=CARTESIAN_POINT('Ctrl Pts',(-0.513475673163749,-0.294079048119024,
-1.27767605041428));
#64938=CARTESIAN_POINT('Ctrl Pts',(-0.464537743766196,-0.37952694521123,
-1.27303950709902));
#64939=CARTESIAN_POINT('Ctrl Pts',(-0.393808224309609,-0.452494309346392,
-1.26840296378377));
#64940=CARTESIAN_POINT('Ctrl Pts',(-0.309925651833169,-0.504069284731118,
-1.26376642046852));
#64941=CARTESIAN_POINT('Ctrl Pts',(-0.226043079356727,-0.555644260115845,
-1.25912987715326));
#64942=CARTESIAN_POINT('Ctrl Pts',(-0.129007453860431,-0.585826846750134,
-1.25449333383801));
#64943=CARTESIAN_POINT('Ctrl Pts',(-0.0306702038766711,-0.590930699885967,
-1.24985679052276));
#64944=CARTESIAN_POINT('Ctrl Pts',(0.0676670461070893,-0.596034553021801,
-1.24522024720751));
#64945=CARTESIAN_POINT('Ctrl Pts',(0.167305920578315,-0.576059672659178,
-1.24058370389225));
#64946=CARTESIAN_POINT('Ctrl Pts',(0.256077043662899,-0.533445687190763,
-1.235947160577));
#64947=CARTESIAN_POINT('Ctrl Pts',(0.344848166747481,-0.490831701722349,
-1.23131061726175));
#64948=CARTESIAN_POINT('Ctrl Pts',(0.422751538445423,-0.425578611148145,
-1.22667407394649));
#64949=CARTESIAN_POINT('Ctrl Pts',(0.480272444574299,-0.345656089858378,
-1.22203753063124));
#64950=CARTESIAN_POINT('Ctrl Pts',(0.537793350703178,-0.265733568568606,
-1.21740098731599));
#64951=CARTESIAN_POINT('Ctrl Pts',(0.574931791262988,-0.17114161656327,
-1.21276444400074));
#64952=CARTESIAN_POINT('Ctrl Pts',(0.587151869547258,-0.073433204755854,
-1.20812790068548));
#64953=CARTESIAN_POINT('Ctrl Pts',(0.599371947831528,0.0242752070515565,
-1.20349135737023));
#64954=CARTESIAN_POINT('Ctrl Pts',(0.586673663840261,0.125100078661047,
-1.19885481405498));
#64955=CARTESIAN_POINT('Ctrl Pts',(0.550607920187181,0.216727182652991,
-1.19421827073972));
#64956=CARTESIAN_POINT('Ctrl Pts',(0.514542176534101,0.308354286644934,
-1.18958172742447));
#64957=CARTESIAN_POINT('Ctrl Pts',(0.455108973219207,0.390783623019332,
-1.18494518410922));
#64958=CARTESIAN_POINT('Ctrl Pts',(0.37956717375716,0.453947699718324,-1.18030864079397));
#64959=CARTESIAN_POINT('Ctrl Pts',(0.304025374295109,0.517111776417319,
-1.17567209747871));
#64960=CARTESIAN_POINT('Ctrl Pts',(0.212374978685904,0.561010593440907,
-1.17103555416346));
#64961=CARTESIAN_POINT('Ctrl Pts',(0.11580969138574,0.580282576728524,-1.1663990108482));
#64962=CARTESIAN_POINT('Ctrl Pts',(0.0192444040855797,0.59955456001614,
-1.16176246753295));
#64963=CARTESIAN_POINT('Ctrl Pts',(-0.082235774905539,0.594199709567786,
-1.1571259242177));
#64964=CARTESIAN_POINT('Ctrl Pts',(-0.176236582319707,0.564872039072412,
-1.15248938090245));
#64965=CARTESIAN_POINT('Ctrl Pts',(-0.270237389733872,0.535544368577038,
-1.14785283758719));
#64966=CARTESIAN_POINT('Ctrl Pts',(-0.356758825571087,0.482243878034646,
-1.14321629427194));
#64967=CARTESIAN_POINT('Ctrl Pts',(-0.425233609947291,0.411480413196972,
-1.13857975095669));
#64968=CARTESIAN_POINT('Ctrl Pts',(-0.493708394323496,0.340716948359297,
-1.13394320764143));
#64969=CARTESIAN_POINT('Ctrl Pts',(-0.544136527238688,0.25249050922634,
-1.12930666432618));
#64970=CARTESIAN_POINT('Ctrl Pts',(-0.570358977819315,0.157576615950659,
-1.12467012101093));
#64971=CARTESIAN_POINT('Ctrl Pts',(-0.584512317462174,0.106347667526243,
-1.12216758708078));
#64972=CARTESIAN_POINT('Ctrl Pts',(-0.591614041410101,0.0531705254529068,
-1.11966505315064));
#64973=CARTESIAN_POINT('Ctrl Pts',(-0.591625419221713,-3.63663382748259E-6,
-1.11716251922049));
#64974=CARTESIAN_POINT('Origin',(0.,0.,-1.97));
#64975=CARTESIAN_POINT('',(-0.591718276663101,7.52894403206403E-6,-0.916987480779508));
#64976=CARTESIAN_POINT('',(-0.591707850850199,1.11928198428649E-5,-0.942162519220489));
#64977=CARTESIAN_POINT('',(-0.591675,-7.2459289488551E-17,-1.97));
#64978=CARTESIAN_POINT('Ctrl Pts',(-0.591718276663101,7.52894403206403E-6,
-0.916987480779508));
#64979=CARTESIAN_POINT('Ctrl Pts',(-0.591722974652918,0.0074275342378391,
-0.917336845993036));
#64980=CARTESIAN_POINT('Ctrl Pts',(-0.591586310640105,0.0148473662541653,
-0.917686211206564));
#64981=CARTESIAN_POINT('Ctrl Pts',(-0.591307166968182,0.02226183412354,
-0.918035576420092));
#64982=CARTESIAN_POINT('Ctrl Pts',(-0.587602557362138,0.120661732295286,
-0.922672119735345));
#64983=CARTESIAN_POINT('Ctrl Pts',(-0.558803237227458,0.218116851992544,
-0.927308663050598));
#64984=CARTESIAN_POINT('Ctrl Pts',(-0.50842660630895,0.302724529834708,
-0.931945206365852));
#64985=CARTESIAN_POINT('Ctrl Pts',(-0.45804997539044,0.387332207676875,
-0.936581749681105));
#64986=CARTESIAN_POINT('Ctrl Pts',(-0.386096033688106,0.459092443663951,
-0.941218292996357));
#64987=CARTESIAN_POINT('Ctrl Pts',(-0.301352862830176,0.50924081438013,
-0.94585483631161));
#64988=CARTESIAN_POINT('Ctrl Pts',(-0.216609691972246,0.55938918509631,
-0.950491379626863));
#64989=CARTESIAN_POINT('Ctrl Pts',(-0.119077291958735,0.587925690541584,
-0.955127922942115));
#64990=CARTESIAN_POINT('Ctrl Pts',(-0.020667764787635,0.591365029795611,
-0.959764466257368));
#64991=CARTESIAN_POINT('Ctrl Pts',(0.0777417623834591,0.594804369049637,
-0.964401009572621));
#64992=CARTESIAN_POINT('Ctrl Pts',(0.177028416712141,0.573146542112413,
-0.969037552887874));
#64993=CARTESIAN_POINT('Ctrl Pts',(0.265065840667561,0.529036723751461,
-0.973674096203127));
#64994=CARTESIAN_POINT('Ctrl Pts',(0.353103264622989,0.484926905390506,
-0.97831063951838));
#64995=CARTESIAN_POINT('Ctrl Pts',(0.429891458205161,0.418365095605818,
-0.982947182833634));
#64996=CARTESIAN_POINT('Ctrl Pts',(0.486051909308696,0.337480808971196,
-0.987583726148887));
#64997=CARTESIAN_POINT('Ctrl Pts',(0.542212360412227,0.256596522336578,
-0.99222026946414));
#64998=CARTESIAN_POINT('Ctrl Pts',(0.577745069037122,0.161389758852027,
-0.996856812779392));
#64999=CARTESIAN_POINT('Ctrl Pts',(0.588310254255745,0.0634885793196063,
-1.00149335609465));
#65000=CARTESIAN_POINT('Ctrl Pts',(0.598875439474368,-0.0344126002128146,
-1.0061298994099));
#65001=CARTESIAN_POINT('Ctrl Pts',(0.584473101286718,-0.135008195793106,
-1.01076644272515));
#65002=CARTESIAN_POINT('Ctrl Pts',(0.546862266656937,-0.226011982587911,
-1.0154029860404));
#65003=CARTESIAN_POINT('Ctrl Pts',(0.509251432027154,-0.317015769382721,
-1.02003952935566));
#65004=CARTESIAN_POINT('Ctrl Pts',(0.448432100955235,-0.398427747392044,
-1.02467607267091));
#65005=CARTESIAN_POINT('Ctrl Pts',(0.371832431418214,-0.460304679437544,
-1.02931261598616));
#65006=CARTESIAN_POINT('Ctrl Pts',(0.295232761881193,-0.522181611483043,
-1.03394915930142));
#65007=CARTESIAN_POINT('Ctrl Pts',(0.202852753879069,-0.564523497564719,
-1.03858570261667));
#65008=CARTESIAN_POINT('Ctrl Pts',(0.105975222945406,-0.582158919100406,
-1.04322224593192));
#65009=CARTESIAN_POINT('Ctrl Pts',(0.00909769201174822,-0.599794340636091,
-1.04785878924718));
#65010=CARTESIAN_POINT('Ctrl Pts',(-0.0922773618534477,-0.592723297625791,
-1.05249533256243));
#65011=CARTESIAN_POINT('Ctrl Pts',(-0.185768514820475,-0.561809410625949,
-1.05713187587768));
#65012=CARTESIAN_POINT('Ctrl Pts',(-0.279259667787502,-0.530895523626107,
-1.06176841919293));
#65013=CARTESIAN_POINT('Ctrl Pts',(-0.364866919856361,-0.476138792636723,
-1.06640496250819));
#65014=CARTESIAN_POINT('Ctrl Pts',(-0.432134644811843,-0.404226921072587,
-1.07104150582344));
#65015=CARTESIAN_POINT('Ctrl Pts',(-0.499402369767325,-0.332315049508451,
-1.07567804913869));
#65016=CARTESIAN_POINT('Ctrl Pts',(-0.54833056760943,-0.243248037369564,
-1.08031459245395));
#65017=CARTESIAN_POINT('Ctrl Pts',(-0.572943401762895,-0.147904068040208,
-1.0849511357692));
#65018=CARTESIAN_POINT('Ctrl Pts',(-0.585394084740131,-0.0996732333257132,
-1.08729658410597));
#65019=CARTESIAN_POINT('Ctrl Pts',(-0.591622569109328,-0.049836151845043,
-1.08964203244274));
#65020=CARTESIAN_POINT('Ctrl Pts',(-0.591624151837836,5.41149558302978E-7,
-1.09198748077951));
#65021=CARTESIAN_POINT('Ctrl Pts',(-0.591625419221713,-3.63663382748259E-6,
-1.11716251922049));
#65022=CARTESIAN_POINT('Ctrl Pts',(-0.591635121530429,-0.0453473418964572,
-1.11502850983538));
#65023=CARTESIAN_POINT('Ctrl Pts',(-0.586488975449466,-0.0906888802184572,
-1.11289450045028));
#65024=CARTESIAN_POINT('Ctrl Pts',(-0.576162964933303,-0.134818364152742,
-1.11076049106517));
#65025=CARTESIAN_POINT('Ctrl Pts',(-0.553727733220603,-0.230698103562057,
-1.10612394774992));
#65026=CARTESIAN_POINT('Ctrl Pts',(-0.506840501549141,-0.320856234962282,
-1.10148740443466));
#65027=CARTESIAN_POINT('Ctrl Pts',(-0.441227833460853,-0.394281311315915,
-1.09685086111941));
#65028=CARTESIAN_POINT('Ctrl Pts',(-0.375615165372566,-0.467706387669546,
-1.09221431780416));
#65029=CARTESIAN_POINT('Ctrl Pts',(-0.291277060867453,-0.524398408976585,
-1.0875777744889));
#65030=CARTESIAN_POINT('Ctrl Pts',(-0.198514139053056,-0.557433305490064,
-1.08294123117365));
#65031=CARTESIAN_POINT('Ctrl Pts',(-0.105751217238654,-0.590468202003546,
-1.0783046878584));
#65032=CARTESIAN_POINT('Ctrl Pts',(-0.00456347811496688,-0.599845973723464,
-1.07366814454314));
#65033=CARTESIAN_POINT('Ctrl Pts',(0.0926905321403009,-0.584421268200519,
-1.06903160122789));
#65034=CARTESIAN_POINT('Ctrl Pts',(0.189944542395563,-0.568996562677575,
-1.06439505791264));
#65035=CARTESIAN_POINT('Ctrl Pts',(0.283264823782407,-0.52876937991177,
-1.05975851459739));
#65036=CARTESIAN_POINT('Ctrl Pts',(0.361253720647849,-0.468652859579073,
-1.05512197128213));
#65037=CARTESIAN_POINT('Ctrl Pts',(0.43924261751329,-0.408536339246375,
-1.05048542796688));
#65038=CARTESIAN_POINT('Ctrl Pts',(0.501900129857331,-0.328530481346785,
-1.04584888465163));
#65039=CARTESIAN_POINT('Ctrl Pts',(0.541573593766437,-0.238406786833893,
-1.04121234133637));
#65040=CARTESIAN_POINT('Ctrl Pts',(0.581247057675546,-0.148283092320996,
-1.03657579802112));
#65041=CARTESIAN_POINT('Ctrl Pts',(0.597936473149718,-0.048041561194797,
-1.03193925470587));
#65042=CARTESIAN_POINT('Ctrl Pts',(0.589603481454953,0.0500748253092742,
-1.02730271139062));
#65043=CARTESIAN_POINT('Ctrl Pts',(0.581270489760189,0.14819121181334,-1.02266616807536));
#65044=CARTESIAN_POINT('Ctrl Pts',(0.54791509089649,0.244182453695277,-1.01802962476011));
#65045=CARTESIAN_POINT('Ctrl Pts',(0.493611140458446,0.326324678026145,
-1.01339308144486));
#65046=CARTESIAN_POINT('Ctrl Pts',(0.439307190020401,0.408466902357016,
-1.0087565381296));
#65047=CARTESIAN_POINT('Ctrl Pts',(0.364054688008008,0.476760109136816,
-1.00411999481435));
#65048=CARTESIAN_POINT('Ctrl Pts',(0.277044585115118,0.522863319933563,
-0.999483451499097));
#65049=CARTESIAN_POINT('Ctrl Pts',(0.190034482222228,0.568966530730311,
-0.994846908183844));
#65050=CARTESIAN_POINT('Ctrl Pts',(0.0912667784488393,0.592879745544007,
-0.990210364868592));
#65051=CARTESIAN_POINT('Ctrl Pts',(-0.00719555060622232,0.591682328217624,
-0.985573821553339));
#65052=CARTESIAN_POINT('Ctrl Pts',(-0.105657879661281,0.590484910891242,
-0.980937278238086));
#65053=CARTESIAN_POINT('Ctrl Pts',(-0.203814833998013,0.564176861424783,
-0.976300734922833));
#65054=CARTESIAN_POINT('Ctrl Pts',(-0.289678031789344,0.515971308671526,
-0.97166419160758));
#65055=CARTESIAN_POINT('Ctrl Pts',(-0.37554122958068,0.467765755918267,
-0.967027648292327));
#65056=CARTESIAN_POINT('Ctrl Pts',(-0.449110670826613,0.397662699878209,
-0.962391104977074));
#65057=CARTESIAN_POINT('Ctrl Pts',(-0.501400965154952,0.314224164594702,
-0.95775456166182));
#65058=CARTESIAN_POINT('Ctrl Pts',(-0.553691259483289,0.230785629311198,
-0.953118018346567));
#65059=CARTESIAN_POINT('Ctrl Pts',(-0.584702406894033,0.134011614784245,
-0.948481475031314));
#65060=CARTESIAN_POINT('Ctrl Pts',(-0.590646866518909,0.0357215977379096,
-0.943844931716061));
#65061=CARTESIAN_POINT('Ctrl Pts',(-0.591365867181854,0.0238331180649364,
-0.94328412755087));
#65062=CARTESIAN_POINT('Ctrl Pts',(-0.591718151075332,0.0119224598117231,
-0.94272332338568));
#65063=CARTESIAN_POINT('Ctrl Pts',(-0.591707850850199,1.11928198428649E-5,
-0.942162519220489));
#65064=CARTESIAN_POINT('Origin',(0.,0.,-1.97));
#65065=CARTESIAN_POINT('',(-0.591643300061755,-1.24859503531638E-5,-0.741987480779508));
#65066=CARTESIAN_POINT('',(-0.591654968200026,-1.45109499015529E-5,-0.76716251922049));
#65067=CARTESIAN_POINT('',(-0.591675,-7.2459289488551E-17,-1.97));
#65068=CARTESIAN_POINT('Ctrl Pts',(-0.591643300061755,-1.24859503531638E-5,
-0.741987480779508));
#65069=CARTESIAN_POINT('Ctrl Pts',(-0.591593891768562,0.0646650190051903,
-0.745031659543333));
#65070=CARTESIAN_POINT('Ctrl Pts',(-0.581021510217558,0.129358282919564,
-0.748075838307159));
#65071=CARTESIAN_POINT('Ctrl Pts',(-0.560200536082961,0.190565249557322,
-0.751120017070985));
#65072=CARTESIAN_POINT('Ctrl Pts',(-0.528488420622464,0.283788668425994,
-0.755756560386238));
#65073=CARTESIAN_POINT('Ctrl Pts',(-0.473001740813173,0.368924615940348,
-0.76039310370149));
#65074=CARTESIAN_POINT('Ctrl Pts',(-0.400517352236696,0.435575028581515,
-0.765029647016743));
#65075=CARTESIAN_POINT('Ctrl Pts',(-0.328032963660219,0.502225441222683,
-0.769666190331996));
#65076=CARTESIAN_POINT('Ctrl Pts',(-0.238550866316555,0.550390318990665,
-0.77430273364725));
#65077=CARTESIAN_POINT('Ctrl Pts',(-0.142999939946241,0.5741870532691,-0.778939276962502));
#65078=CARTESIAN_POINT('Ctrl Pts',(-0.0474490135759239,0.597983787547536,
-0.783575820277755));
#65079=CARTESIAN_POINT('Ctrl Pts',(0.054170741821044,0.597412378336424,
-0.788212363593008));
#65080=CARTESIAN_POINT('Ctrl Pts',(0.149448015837724,0.572542614596196,
-0.792848906908261));
#65081=CARTESIAN_POINT('Ctrl Pts',(0.244725289854398,0.547672850855969,
-0.797485450223514));
#65082=CARTESIAN_POINT('Ctrl Pts',(0.333660082490784,0.49850473258663,-0.802121993538768));
#65083=CARTESIAN_POINT('Ctrl Pts',(0.405390358967573,0.431043399001334,
-0.806758536854021));
#65084=CARTESIAN_POINT('Ctrl Pts',(0.477120635444364,0.363582065416036,
-0.811395080169274));
#65085=CARTESIAN_POINT('Ctrl Pts',(0.531646395761552,0.27782751651479,-0.816031623484526));
#65086=CARTESIAN_POINT('Ctrl Pts',(0.562308146065541,0.184253368584715,
-0.820668166799779));
#65087=CARTESIAN_POINT('Ctrl Pts',(0.592969896369529,0.0906792206546452,
-0.825304710115031));
#65088=CARTESIAN_POINT('Ctrl Pts',(0.599767636660314,-0.0107145263042522,
-0.829941253430284));
#65089=CARTESIAN_POINT('Ctrl Pts',(0.581871126159565,-0.107544165384645,
-0.834577796745537));
#65090=CARTESIAN_POINT('Ctrl Pts',(0.563974615658815,-0.204373804465043,
-0.839214340060791));
#65091=CARTESIAN_POINT('Ctrl Pts',(0.52138385436653,-0.296639335666945,
-0.843850883376044));
#65092=CARTESIAN_POINT('Ctrl Pts',(0.459300657193611,-0.373071925060032,
-0.848487426691297));
#65093=CARTESIAN_POINT('Ctrl Pts',(0.397217460020693,-0.449504514453119,
-0.85312397000655));
#65094=CARTESIAN_POINT('Ctrl Pts',(0.315641826967143,-0.510104162037391,
-0.857760513321803));
#65095=CARTESIAN_POINT('Ctrl Pts',(0.224536983190461,-0.547469540838764,
-0.862397056637056));
#65096=CARTESIAN_POINT('Ctrl Pts',(0.13343213941378,-0.584834919640138,
-0.867033599952309));
#65097=CARTESIAN_POINT('Ctrl Pts',(0.032798084913967,-0.598966029658612,
-0.871670143267562));
#65098=CARTESIAN_POINT('Ctrl Pts',(-0.0650742583024552,-0.588136970333329,
-0.876306686582815));
#65099=CARTESIAN_POINT('Ctrl Pts',(-0.162946601518877,-0.577307911008045,
-0.880943229898068));
#65100=CARTESIAN_POINT('Ctrl Pts',(-0.258057233451909,-0.541518682339004,
-0.885579773213321));
#65101=CARTESIAN_POINT('Ctrl Pts',(-0.338789834309108,-0.485140395282941,
-0.890216316528574));
#65102=CARTESIAN_POINT('Ctrl Pts',(-0.419522435166307,-0.428762108226878,
-0.894852859843827));
#65103=CARTESIAN_POINT('Ctrl Pts',(-0.485877004947672,-0.351794762783792,
-0.89948940315908));
#65104=CARTESIAN_POINT('Ctrl Pts',(-0.529749340299652,-0.263638751739126,
-0.904125946474333));
#65105=CARTESIAN_POINT('Ctrl Pts',(-0.570315879336133,-0.182125327968706,
-0.908413124576058));
#65106=CARTESIAN_POINT('Ctrl Pts',(-0.591660626049118,-0.0910458529569786,
-0.912700302677783));
#65107=CARTESIAN_POINT('Ctrl Pts',(-0.591718276663101,7.52894403206403E-6,
-0.916987480779508));
#65108=CARTESIAN_POINT('Ctrl Pts',(-0.591707850850199,1.11928198428649E-5,
-0.942162519220489));
#65109=CARTESIAN_POINT('Ctrl Pts',(-0.591632992221397,-0.0865559552489433,
-0.938086780070427));
#65110=CARTESIAN_POINT('Ctrl Pts',(-0.572406797455186,-0.173155256294739,
-0.934011040920365));
#65111=CARTESIAN_POINT('Ctrl Pts',(-0.535615671906496,-0.25150667084932,
-0.929935301770302));
#65112=CARTESIAN_POINT('Ctrl Pts',(-0.493762245830199,-0.340638902824493,
-0.92529875845505));
#65113=CARTESIAN_POINT('Ctrl Pts',(-0.429177621838593,-0.419097347209124,
-0.920662215139797));
#65114=CARTESIAN_POINT('Ctrl Pts',(-0.349749831277004,-0.477299496118803,
-0.916025671824544));
#65115=CARTESIAN_POINT('Ctrl Pts',(-0.270322040715412,-0.535501645028483,
-0.911389128509291));
#65116=CARTESIAN_POINT('Ctrl Pts',(-0.176051083583834,-0.573447498463211,
-0.906752585194038));
#65117=CARTESIAN_POINT('Ctrl Pts',(-0.0784507261450266,-0.58650254649138,
-0.902116041878785));
#65118=CARTESIAN_POINT('Ctrl Pts',(0.0191496312937804,-0.599557594519549,
-0.897479498563532));
#65119=CARTESIAN_POINT('Ctrl Pts',(0.120079389039817,-0.587721837141161,
-0.892842955248279));
#65120=CARTESIAN_POINT('Ctrl Pts',(0.212011509424179,-0.552440832438404,
-0.888206411933026));
#65121=CARTESIAN_POINT('Ctrl Pts',(0.303943629808538,-0.517159827735649,
-0.883569868617773));
#65122=CARTESIAN_POINT('Ctrl Pts',(0.386878112831224,-0.458433575708527,
-0.87893332530252));
#65123=CARTESIAN_POINT('Ctrl Pts',(0.450685770440045,-0.383434596504304,
-0.874296781987267));
#65124=CARTESIAN_POINT('Ctrl Pts',(0.514493428048868,-0.308435617300078,
-0.869660238672014));
#65125=CARTESIAN_POINT('Ctrl Pts',(0.559174260243827,-0.217163910918747,
-0.865023695356761));
#65126=CARTESIAN_POINT('Ctrl Pts',(0.57927118168314,-0.1207669306763,-0.860387152041508));
#65127=CARTESIAN_POINT('Ctrl Pts',(0.599368103122454,-0.0243699504338505,
-0.855750608726255));
#65128=CARTESIAN_POINT('Ctrl Pts',(0.594881113806123,0.07715230366971,-0.851114065411002));
#65129=CARTESIAN_POINT('Ctrl Pts',(0.566358231361036,0.171400429530254,
-0.846477522095749));
#65130=CARTESIAN_POINT('Ctrl Pts',(0.537835348915949,0.265648555390792,
-0.841840978780496));
#65131=CARTESIAN_POINT('Ctrl Pts',(0.485276573342108,0.352622553008308,
-0.837204435465243));
#65132=CARTESIAN_POINT('Ctrl Pts',(0.415101161168002,0.421699868947729,
-0.83256789214999));
#65133=CARTESIAN_POINT('Ctrl Pts',(0.344925748993893,0.490777184887153,
-0.827931348834737));
#65134=CARTESIAN_POINT('Ctrl Pts',(0.257133700219515,0.541957819148481,
-0.823294805519484));
#65135=CARTESIAN_POINT('Ctrl Pts',(0.162447480809717,0.568990834242638,
-0.818658262204231));
#65136=CARTESIAN_POINT('Ctrl Pts',(0.0677612613999249,0.596023849336792,
-0.814021718888978));
#65137=CARTESIAN_POINT('Ctrl Pts',(-0.0338191286452886,0.598909245263779,
-0.809385175573725));
#65138=CARTESIAN_POINT('Ctrl Pts',(-0.129887186799085,0.57729461471503,
-0.804748632258472));
#65139=CARTESIAN_POINT('Ctrl Pts',(-0.225955244952882,0.555679984166281,
-0.80011208894322));
#65140=CARTESIAN_POINT('Ctrl Pts',(-0.316510971215263,0.509565327141797,
-0.795475545627967));
#65141=CARTESIAN_POINT('Ctrl Pts',(-0.390494358372299,0.444582848919031,
-0.790839002312714));
#65142=CARTESIAN_POINT('Ctrl Pts',(-0.464477745529339,0.379600370696262,
-0.78620245899746));
#65143=CARTESIAN_POINT('Ctrl Pts',(-0.521888793581034,0.295750071275207,
-0.781565915682207));
#65144=CARTESIAN_POINT('Ctrl Pts',(-0.555715614579277,0.203272991777885,
-0.776929372366954));
#65145=CARTESIAN_POINT('Ctrl Pts',(-0.579467619081906,0.13833883764249,
-0.773673754651466));
#65146=CARTESIAN_POINT('Ctrl Pts',(-0.59159176314519,0.0691513749487757,
-0.770418136935978));
#65147=CARTESIAN_POINT('Ctrl Pts',(-0.591654968200026,-1.45109499015529E-5,
-0.76716251922049));
#65148=CARTESIAN_POINT('Origin',(0.,0.,-1.97));
#65149=CARTESIAN_POINT('',(-0.59167279304111,1.54653535696381E-5,-0.566987480779507));
#65150=CARTESIAN_POINT('',(-0.591659059186468,1.49283821118909E-5,-0.59216251922049));
#65151=CARTESIAN_POINT('',(-0.591675,-7.2459289488551E-17,-1.97));
#65152=CARTESIAN_POINT('Ctrl Pts',(-0.59167279304111,1.54653535696381E-5,
-0.566987480779507));
#65153=CARTESIAN_POINT('Ctrl Pts',(-0.591696802954663,0.0234350648064659,
-0.568089929778377));
#65154=CARTESIAN_POINT('Ctrl Pts',(-0.590332828147301,0.0468518849396706,
-0.569192378777246));
#65155=CARTESIAN_POINT('Ctrl Pts',(-0.587559081074247,0.0701005079415737,
-0.570294827776116));
#65156=CARTESIAN_POINT('Ctrl Pts',(-0.575893599530016,0.167876684144606,
-0.574931371091369));
#65157=CARTESIAN_POINT('Ctrl Pts',(-0.539292473904837,0.262677838137568,
-0.579567914406623));
#65158=CARTESIAN_POINT('Ctrl Pts',(-0.48222597604303,0.342925448160133,
-0.584204457721876));
#65159=CARTESIAN_POINT('Ctrl Pts',(-0.425159478181225,0.423173058182693,
-0.588841001037129));
#65160=CARTESIAN_POINT('Ctrl Pts',(-0.347627608082795,0.488867124234858,
-0.593477544352382));
#65161=CARTESIAN_POINT('Ctrl Pts',(-0.259099706649643,0.531984113466323,
-0.598114087667635));
#65162=CARTESIAN_POINT('Ctrl Pts',(-0.170571805216496,0.575101102697786,
-0.602750630982888));
#65163=CARTESIAN_POINT('Ctrl Pts',(-0.0710478724486285,0.595641015108553,
-0.607387174298142));
#65164=CARTESIAN_POINT('Ctrl Pts',(0.0273167541639602,0.591095212219171,
-0.612023717613394));
#65165=CARTESIAN_POINT('Ctrl Pts',(0.125681380776549,0.586549409329789,
-0.616660260928647));
#65166=CARTESIAN_POINT('Ctrl Pts',(0.222886701233859,0.556917891140258,
-0.6212968042439));
#65167=CARTESIAN_POINT('Ctrl Pts',(0.307060561340197,0.505819697753977,
-0.625933347559153));
#65168=CARTESIAN_POINT('Ctrl Pts',(0.391234421446539,0.454721504367692,
-0.630569890874406));
#65169=CARTESIAN_POINT('Ctrl Pts',(0.462376821201907,0.382156635784654,
-0.635206434189659));
#65170=CARTESIAN_POINT('Ctrl Pts',(0.511798796506661,0.29698778907695,-0.639842977504912));
#65171=CARTESIAN_POINT('Ctrl Pts',(0.561220771811414,0.211818942369245,
-0.644479520820166));
#65172=CARTESIAN_POINT('Ctrl Pts',(0.588922322665554,0.114046117536873,
-0.649116064135418));
#65173=CARTESIAN_POINT('Ctrl Pts',(0.591520125176384,0.0156107808195186,
-0.653752607450672));
#65174=CARTESIAN_POINT('Ctrl Pts',(0.594117927687215,-0.0828245558978302,
-0.658389150765925));
#65175=CARTESIAN_POINT('Ctrl Pts',(0.57161198185474,-0.181922404500161,
-0.663025694081178));
#65176=CARTESIAN_POINT('Ctrl Pts',(0.52675104729403,-0.269579467209807,
-0.667662237396431));
#65177=CARTESIAN_POINT('Ctrl Pts',(0.48189011273332,-0.357236529919453,
-0.672298780711684));
#65178=CARTESIAN_POINT('Ctrl Pts',(0.414674189444375,-0.433452806736414,
-0.676935324026936));
#65179=CARTESIAN_POINT('Ctrl Pts',(0.333312682035277,-0.488919636505767,
-0.681571867342189));
#65180=CARTESIAN_POINT('Ctrl Pts',(0.251951174626179,-0.54438646627512,
-0.686208410657442));
#65181=CARTESIAN_POINT('Ctrl Pts',(0.156444083096928,-0.579103848996866,
-0.690844953972695));
#65182=CARTESIAN_POINT('Ctrl Pts',(0.0584561487608926,-0.588831583424772,
-0.695481497287948));
#65183=CARTESIAN_POINT('Ctrl Pts',(-0.039531785575143,-0.598559317852679,
-0.700118040603201));
#65184=CARTESIAN_POINT('Ctrl Pts',(-0.140000562717963,-0.583297403986747,
-0.704754583918453));
#65185=CARTESIAN_POINT('Ctrl Pts',(-0.230679446781087,-0.544909852910784,
-0.709391127233706));
#65186=CARTESIAN_POINT('Ctrl Pts',(-0.321358330844217,-0.50652230183482,
-0.71402767054896));
#65187=CARTESIAN_POINT('Ctrl Pts',(-0.402247321827649,-0.445009113548823,
-0.718664213864213));
#65188=CARTESIAN_POINT('Ctrl Pts',(-0.463467057478662,-0.367883190154907,
-0.723300757179466));
#65189=CARTESIAN_POINT('Ctrl Pts',(-0.524686793129676,-0.290757266760991,
-0.727937300494719));
#65190=CARTESIAN_POINT('Ctrl Pts',(-0.566237273448271,-0.198018608259155,
-0.732573843809972));
#65191=CARTESIAN_POINT('Ctrl Pts',(-0.583043738051716,-0.100993833896741,
-0.737210387125225));
#65192=CARTESIAN_POINT('Ctrl Pts',(-0.588815714425,-0.0676718522392664,
-0.738802751676653));
#65193=CARTESIAN_POINT('Ctrl Pts',(-0.591669144803714,-0.0338443250623759,
-0.74039511622808));
#65194=CARTESIAN_POINT('Ctrl Pts',(-0.591643300061755,-1.24859503531638E-5,
-0.741987480779508));
#65195=CARTESIAN_POINT('Ctrl Pts',(-0.591654968200026,-1.45109499015529E-5,
-0.76716251922049));
#65196=CARTESIAN_POINT('Ctrl Pts',(-0.591681777698525,-0.0293523972789734,
-0.765781593620725));
#65197=CARTESIAN_POINT('Ctrl Pts',(-0.589538611466783,-0.0586864015619183,
-0.76440066802096));
#65198=CARTESIAN_POINT('Ctrl Pts',(-0.585192419058669,-0.0876902853788226,
-0.763019742421195));
#65199=CARTESIAN_POINT('Ctrl Pts',(-0.570599808595024,-0.185072623464623,
-0.758383199105942));
#65200=CARTESIAN_POINT('Ctrl Pts',(-0.531171993722942,-0.278733440062635,
-0.753746655790689));
#65201=CARTESIAN_POINT('Ctrl Pts',(-0.471724483465576,-0.357233488313583,
-0.749110112475436));
#65202=CARTESIAN_POINT('Ctrl Pts',(-0.412276973208212,-0.435733536564528,
-0.744473569160183));
#65203=CARTESIAN_POINT('Ctrl Pts',(-0.332809767565565,-0.49907281646841,
-0.73983702584493));
#65204=CARTESIAN_POINT('Ctrl Pts',(-0.243028579295454,-0.539515396554342,
-0.735200482529677));
#65205=CARTESIAN_POINT('Ctrl Pts',(-0.15324739102534,-0.579957976640276,
-0.730563939214424));
#65206=CARTESIAN_POINT('Ctrl Pts',(-0.0531522201277623,-0.59750385690826,
-0.725927395899172));
#65207=CARTESIAN_POINT('Ctrl Pts',(0.0450318278418444,-0.590010074451935,
-0.721290852583919));
#65208=CARTESIAN_POINT('Ctrl Pts',(0.143215875811451,-0.582516291995611,
-0.716654309268665));
#65209=CARTESIAN_POINT('Ctrl Pts',(0.239488800853087,-0.549982846814977,
-0.712017765953412));
#65210=CARTESIAN_POINT('Ctrl Pts',(0.322092326716154,-0.496383205340521,
-0.707381222638159));
#65211=CARTESIAN_POINT('Ctrl Pts',(0.404695852579222,-0.442783563866064,
-0.702744679322906));
#65212=CARTESIAN_POINT('Ctrl Pts',(0.473629979263721,-0.368117726097785,
-0.698108136007653));
#65213=CARTESIAN_POINT('Ctrl Pts',(0.520475449701276,-0.281504990598408,
-0.6934715926924));
#65214=CARTESIAN_POINT('Ctrl Pts',(0.567320920138831,-0.194892255099032,
-0.688835049377147));
#65215=CARTESIAN_POINT('Ctrl Pts',(0.592077734329442,-0.0963326218685597,
-0.684198506061894));
#65216=CARTESIAN_POINT('Ctrl Pts',(0.591722223259084,0.0021363461522315,
-0.679561962746641));
#65217=CARTESIAN_POINT('Ctrl Pts',(0.591366712188726,0.100605314173023,
-0.674925419431388));
#65218=CARTESIAN_POINT('Ctrl Pts',(0.565898875857402,0.198983616984125,
-0.670288876116135));
#65219=CARTESIAN_POINT('Ctrl Pts',(0.518429223839417,0.285255838402679,
-0.665652332800882));
#65220=CARTESIAN_POINT('Ctrl Pts',(0.470959571821432,0.371528059821234,
-0.661015789485629));
#65221=CARTESIAN_POINT('Ctrl Pts',(0.40148810411678,0.445694199847239,-0.656379246170376));
#65222=CARTESIAN_POINT('Ctrl Pts',(0.318499705841953,0.498695990411137,
-0.651742702855123));
#65223=CARTESIAN_POINT('Ctrl Pts',(0.235511307567128,0.551697780975035,
-0.64710615953987));
#65224=CARTESIAN_POINT('Ctrl Pts',(0.139005978722123,0.583535222076834,
-0.642469616224617));
#65225=CARTESIAN_POINT('Ctrl Pts',(0.0407703801539367,0.590319853618069,
-0.637833072909364));
#65226=CARTESIAN_POINT('Ctrl Pts',(-0.0574652184142526,0.597104485159305,
-0.633196529594111));
#65227=CARTESIAN_POINT('Ctrl Pts',(-0.157431086705624,0.578836307139974,
-0.628559986278858));
#65228=CARTESIAN_POINT('Ctrl Pts',(-0.246917911515115,0.537746500171382,
-0.623923442963605));
#65229=CARTESIAN_POINT('Ctrl Pts',(-0.336404736324606,0.496656693202789,
-0.619286899648352));
#65230=CARTESIAN_POINT('Ctrl Pts',(-0.415412517652216,0.432745257284934,
-0.614650356333099));
#65231=CARTESIAN_POINT('Ctrl Pts',(-0.474291654445574,0.353818004059765,
-0.610013813017846));
#65232=CARTESIAN_POINT('Ctrl Pts',(-0.533170791238929,0.274890750834599,
-0.605377269702594));
#65233=CARTESIAN_POINT('Ctrl Pts',(-0.571921283498033,0.180947680302121,
-0.60074072638734));
#65234=CARTESIAN_POINT('Ctrl Pts',(-0.585810346874303,0.0834625123547343,
-0.596104183072088));
#65235=CARTESIAN_POINT('Ctrl Pts',(-0.589746182641055,0.0558374954374221,
-0.594790295121555));
#65236=CARTESIAN_POINT('Ctrl Pts',(-0.591685588338141,0.0279280399296278,
-0.593476407171022));
#65237=CARTESIAN_POINT('Ctrl Pts',(-0.591659059186468,1.49283821118909E-5,
-0.59216251922049));
#65238=CARTESIAN_POINT('Origin',(0.,0.,-1.97));
#65239=CARTESIAN_POINT('',(-0.591690521605803,-1.43942328892088E-5,-0.391987480779507));
#65240=CARTESIAN_POINT('',(-0.591703958414771,-1.21461586050568E-5,-0.417162519220489));
#65241=CARTESIAN_POINT('',(-0.591675,-7.2459289488551E-17,-1.97));
#65242=CARTESIAN_POINT('Ctrl Pts',(-0.591690521605803,-1.43942328892088E-5,
-0.391987480779507));
#65243=CARTESIAN_POINT('Ctrl Pts',(-0.591608432467092,0.0806448416080524,
-0.395784743328675));
#65244=CARTESIAN_POINT('Ctrl Pts',(-0.5749902789137,0.161336859953991,-0.399582005877842));
#65245=CARTESIAN_POINT('Ctrl Pts',(-0.542917603258004,0.235330047038208,
-0.40337926842701));
#65246=CARTESIAN_POINT('Ctrl Pts',(-0.503756142076895,0.325677399244553,
-0.408015811742263));
#65247=CARTESIAN_POINT('Ctrl Pts',(-0.441553593529191,0.40603748977217,
-0.412652355057516));
#65248=CARTESIAN_POINT('Ctrl Pts',(-0.363907054607492,0.466595553529413,
-0.417288898372769));
#65249=CARTESIAN_POINT('Ctrl Pts',(-0.286260515685798,0.527153617286652,
-0.421925441688022));
#65250=CARTESIAN_POINT('Ctrl Pts',(-0.19316998639011,0.567909654273519,
-0.426561985003275));
#65251=CARTESIAN_POINT('Ctrl Pts',(-0.0960050616434672,0.58388593329973,
-0.431198528318528));
#65252=CARTESIAN_POINT('Ctrl Pts',(0.00115986310317598,0.599862212325941,
-0.435835071633781));
#65253=CARTESIAN_POINT('Ctrl Pts',(0.102399183300774,0.591058733391496,
-0.440471614949033));
#65254=CARTESIAN_POINT('Ctrl Pts',(0.195348052926546,0.558550707800371,
-0.445108158264286));
#65255=CARTESIAN_POINT('Ctrl Pts',(0.288296922552323,0.526042682209244,
-0.449744701579539));
#65256=CARTESIAN_POINT('Ctrl Pts',(0.372955341606272,0.469830109961435,
-0.454381244894793));
#65257=CARTESIAN_POINT('Ctrl Pts',(0.438983569421467,0.396778503379994,
-0.459017788210046));
#65258=CARTESIAN_POINT('Ctrl Pts',(0.505011797236659,0.323726896798557,
-0.463654331525299));
#65259=CARTESIAN_POINT('Ctrl Pts',(0.552409833813099,0.233836255883489,
-0.468290874840552));
#65260=CARTESIAN_POINT('Ctrl Pts',(0.575388728544376,0.138085357770356,
-0.472927418155804));
#65261=CARTESIAN_POINT('Ctrl Pts',(0.598367623275652,0.0423344596572228,
-0.477563961471057));
#65262=CARTESIAN_POINT('Ctrl Pts',(0.596927376161766,-0.0592766956539763,
-0.48220050478631));
#65263=CARTESIAN_POINT('Ctrl Pts',(0.571243891522922,-0.154337848126212,
-0.486837048101563));
#65264=CARTESIAN_POINT('Ctrl Pts',(0.545560406884078,-0.249399000598452,
-0.491473591416816));
#65265=CARTESIAN_POINT('Ctrl Pts',(0.495633684720274,-0.337910150231728,
-0.496110134732069));
#65266=CARTESIAN_POINT('Ctrl Pts',(0.427561516193825,-0.409061003808133,
-0.500746678047323));
#65267=CARTESIAN_POINT('Ctrl Pts',(0.359489347667377,-0.480211857384537,
-0.505383221362576));
#65268=CARTESIAN_POINT('Ctrl Pts',(0.273271732778284,-0.534002414904071,
-0.510019764677829));
#65269=CARTESIAN_POINT('Ctrl Pts',(0.179438844294176,-0.563862976373561,
-0.514656307993082));
#65270=CARTESIAN_POINT('Ctrl Pts',(0.0856059558100742,-0.593723537843051,
-0.519292851308335));
#65271=CARTESIAN_POINT('Ctrl Pts',(-0.0158422062690415,-0.5996541032625,
-0.523929394623587));
#65272=CARTESIAN_POINT('Ctrl Pts',(-0.112515289055007,-0.580930344099315,
-0.52856593793884));
#65273=CARTESIAN_POINT('Ctrl Pts',(-0.209188371840973,-0.562206584936131,
-0.533202481254093));
#65274=CARTESIAN_POINT('Ctrl Pts',(-0.301086375333789,-0.518828501190311,
-0.537839024569346));
#65275=CARTESIAN_POINT('Ctrl Pts',(-0.376985353533273,-0.456094067257922,
-0.542475567884599));
#65276=CARTESIAN_POINT('Ctrl Pts',(-0.452884331732758,-0.393359633325533,
-0.547112111199852));
#65277=CARTESIAN_POINT('Ctrl Pts',(-0.51278428463891,-0.311268849206574,
-0.551748654515105));
#65278=CARTESIAN_POINT('Ctrl Pts',(-0.54936934236034,-0.219847857940548,
-0.556385197830358));
#65279=CARTESIAN_POINT('Ctrl Pts',(-0.5772554281287,-0.150164392551905,
-0.559919292146741));
#65280=CARTESIAN_POINT('Ctrl Pts',(-0.591595825037046,-0.0750601829560788,
-0.563453386463124));
#65281=CARTESIAN_POINT('Ctrl Pts',(-0.59167279304111,1.54653535696381E-5,
-0.566987480779507));
#65282=CARTESIAN_POINT('Ctrl Pts',(-0.591659059186468,1.49283821118909E-5,
-0.59216251922049));
#65283=CARTESIAN_POINT('Ctrl Pts',(-0.591591970339134,-0.0705737772923772,
-0.588839863855769));
#65284=CARTESIAN_POINT('Ctrl Pts',(-0.578952340615824,-0.141185864061551,
-0.585517208491049));
#65285=CARTESIAN_POINT('Ctrl Pts',(-0.554233358227024,-0.207280336988223,
-0.582194553126328));
#65286=CARTESIAN_POINT('Ctrl Pts',(-0.519739671710038,-0.299510753021489,
-0.577558009811075));
#65287=CARTESIAN_POINT('Ctrl Pts',(-0.461724664182631,-0.382944319725719,
-0.572921466495822));
#65288=CARTESIAN_POINT('Ctrl Pts',(-0.387273988074007,-0.447390893553736,
-0.568284923180568));
#65289=CARTESIAN_POINT('Ctrl Pts',(-0.312823311965386,-0.511837467381749,
-0.563648379865316));
#65290=CARTESIAN_POINT('Ctrl Pts',(-0.221936967275551,-0.55729704833355,
-0.559011836550063));
#65291=CARTESIAN_POINT('Ctrl Pts',(-0.12571534124014,-0.578217438729092,
-0.55437529323481));
#65292=CARTESIAN_POINT('Ctrl Pts',(-0.0294937152047297,-0.599137829124633,
-0.549738749919557));
#65293=CARTESIAN_POINT('Ctrl Pts',(0.072063192176254,-0.595519028963915,
-0.545102206604304));
#65294=CARTESIAN_POINT('Ctrl Pts',(0.166551746426916,-0.567803019748663,
-0.540465663289051));
#65295=CARTESIAN_POINT('Ctrl Pts',(0.261040300677573,-0.540087010533411,
-0.535829119973799));
#65296=CARTESIAN_POINT('Ctrl Pts',(0.348460501797907,-0.488273792263629,
-0.531192576658546));
#65297=CARTESIAN_POINT('Ctrl Pts',(0.418135299368905,-0.418691562961605,
-0.526556033343293));
#65298=CARTESIAN_POINT('Ctrl Pts',(0.487810096939912,-0.349109333659573,
-0.52191949002804));
#65299=CARTESIAN_POINT('Ctrl Pts',(0.539739490961578,-0.261758093325295,
-0.517282946712787));
#65300=CARTESIAN_POINT('Ctrl Pts',(0.567581094307214,-0.167306469864681,
-0.512646403397534));
#65301=CARTESIAN_POINT('Ctrl Pts',(0.595422697652849,-0.0728548464040694,
-0.508009860082281));
#65302=CARTESIAN_POINT('Ctrl Pts',(0.599176510322455,0.0286971601828845,
-0.503373316767028));
#65303=CARTESIAN_POINT('Ctrl Pts',(0.578384061086002,0.12494651397786,-0.498736773451775));
#65304=CARTESIAN_POINT('Ctrl Pts',(0.557591611849549,0.221195867772839,
-0.494100230136521));
#65305=CARTESIAN_POINT('Ctrl Pts',(0.512252900707038,0.312142568775845,
-0.489463686821268));
#65306=CARTESIAN_POINT('Ctrl Pts',(0.447905362926267,0.386678858143867,
-0.484827143506015));
#65307=CARTESIAN_POINT('Ctrl Pts',(0.3835578251455,0.461215147511885,-0.480190600190762));
#65308=CARTESIAN_POINT('Ctrl Pts',(0.300201460726476,0.519341025244921,
-0.475554056875509));
#65309=CARTESIAN_POINT('Ctrl Pts',(0.208016984129261,0.553957297801303,
-0.470917513560257));
#65310=CARTESIAN_POINT('Ctrl Pts',(0.115832507532046,0.588573570357686,
-0.466280970245004));
#65311=CARTESIAN_POINT('Ctrl Pts',(0.0148199187566409,0.599680237737416,
-0.461644426929751));
#65312=CARTESIAN_POINT('Ctrl Pts',(-0.0826836279752934,0.585920789133139,
-0.457007883614498));
#65313=CARTESIAN_POINT('Ctrl Pts',(-0.180187174707233,0.57216134052886,
-0.452371340299245));
#65314=CARTESIAN_POINT('Ctrl Pts',(-0.2741816793957,0.533535775940572,-0.447734796983991));
#65315=CARTESIAN_POINT('Ctrl Pts',(-0.353187140246972,0.474761621698427,
-0.443098253668738));
#65316=CARTESIAN_POINT('Ctrl Pts',(-0.432192601098239,0.415987467456285,
-0.438461710353485));
#65317=CARTESIAN_POINT('Ctrl Pts',(-0.496209018112312,0.337064723560289,
-0.433825167038233));
#65318=CARTESIAN_POINT('Ctrl Pts',(-0.537417757800081,0.247632605031507,
-0.42918862372298));
#65319=CARTESIAN_POINT('Ctrl Pts',(-0.573046355529395,0.170310634030099,
-0.42517992222215));
#65320=CARTESIAN_POINT('Ctrl Pts',(-0.591625916202752,0.0851327680602624,
-0.421171220721319));
#65321=CARTESIAN_POINT('Ctrl Pts',(-0.591703958414771,-1.21461586050568E-5,
-0.417162519220489));
#65322=CARTESIAN_POINT('Origin',(0.,0.,-1.97));
#65323=CARTESIAN_POINT('',(-0.591632161208708,8.69568651094832E-6,-0.216987480779508));
#65324=CARTESIAN_POINT('',(-0.591626527824809,4.92094362445281E-6,-0.24216251922049));
#65325=CARTESIAN_POINT('',(-0.591675,-7.2459289488551E-17,-1.97));
#65326=CARTESIAN_POINT('Ctrl Pts',(-0.591632161208708,8.69568651094832E-6,
-0.216987480779508));
#65327=CARTESIAN_POINT('Ctrl Pts',(-0.591652619919161,0.0394340094205286,
-0.21884301356372));
#65328=CARTESIAN_POINT('Ctrl Pts',(-0.587770808522292,0.0788553485646517,
-0.220698546347931));
#65329=CARTESIAN_POINT('Ctrl Pts',(-0.57994709302668,0.117478187578517,
-0.222554079132143));
#65330=CARTESIAN_POINT('Ctrl Pts',(-0.560397454189643,0.213987647055358,
-0.227190622447396));
#65331=CARTESIAN_POINT('Ctrl Pts',(-0.516235218791925,0.305511403920623,
-0.23182716576265));
#65332=CARTESIAN_POINT('Ctrl Pts',(-0.452854134240634,0.380871222130496,
-0.236463709077903));
#65333=CARTESIAN_POINT('Ctrl Pts',(-0.389473049689346,0.456231040340365,
-0.241100252393156));
#65334=CARTESIAN_POINT('Ctrl Pts',(-0.306873115984487,0.515426919894844,
-0.245736795708408));
#65335=CARTESIAN_POINT('Ctrl Pts',(-0.215142660653105,0.551228982051028,
-0.250373339023661));
#65336=CARTESIAN_POINT('Ctrl Pts',(-0.123412205321724,0.587031044207212,
-0.255009882338914));
#65337=CARTESIAN_POINT('Ctrl Pts',(-0.0225512283638192,0.5994392889651,
-0.259646425654167));
#65338=CARTESIAN_POINT('Ctrl Pts',(0.0751216328736339,0.586938237969985,
-0.26428296896942));
#65339=CARTESIAN_POINT('Ctrl Pts',(0.172794494111093,0.57443718697487,-0.268919512284673));
#65340=CARTESIAN_POINT('Ctrl Pts',(0.2672792396281,0.537026840226748,-0.273556055599926));
#65341=CARTESIAN_POINT('Ctrl Pts',(0.347035992262199,0.47927630345588,-0.278192598915179));
#65342=CARTESIAN_POINT('Ctrl Pts',(0.426792744896299,0.421525766685012,
-0.282829142230433));
#65343=CARTESIAN_POINT('Ctrl Pts',(0.491821504647491,0.343435039891398,
-0.287465685545686));
#65344=CARTESIAN_POINT('Ctrl Pts',(0.534179995675711,0.254541719934951,
-0.292102228860939));
#65345=CARTESIAN_POINT('Ctrl Pts',(0.576538486703928,0.16564839997851,-0.296738772176192));
#65346=CARTESIAN_POINT('Ctrl Pts',(0.596226709009175,0.0659524868592369,
-0.301375315491445));
#65347=CARTESIAN_POINT('Ctrl Pts',(0.590840045156427,-0.0323696771933723,
-0.306011858806698));
#65348=CARTESIAN_POINT('Ctrl Pts',(0.585453381303679,-0.130691841245981,
-0.31064840212195));
#65349=CARTESIAN_POINT('Ctrl Pts',(0.554991831292937,-0.227640256231927,
-0.315284945437203));
#65350=CARTESIAN_POINT('Ctrl Pts',(0.503175810999434,-0.31137414503334,
-0.319921488752456));
#65351=CARTESIAN_POINT('Ctrl Pts',(0.451359790705932,-0.395108033834752,
-0.324558032067709));
#65352=CARTESIAN_POINT('Ctrl Pts',(0.37818930012967,-0.465627396451632,
-0.329194575382962));
#65353=CARTESIAN_POINT('Ctrl Pts',(0.292601003882376,-0.5143193633253,-0.333831118698215));
#65354=CARTESIAN_POINT('Ctrl Pts',(0.207012707635082,-0.563011330198967,
-0.338467662013468));
#65355=CARTESIAN_POINT('Ctrl Pts',(0.109006605716757,-0.589875901329423,
-0.343104205328721));
#65356=CARTESIAN_POINT('Ctrl Pts',(0.010552655617975,-0.591631977184183,
-0.347740748643974));
#65357=CARTESIAN_POINT('Ctrl Pts',(-0.0879012944808124,-0.593388053038943,
-0.352377291959227));
#65358=CARTESIAN_POINT('Ctrl Pts',(-0.186803092760056,-0.570035633618004,
-0.35701383527448));
#65359=CARTESIAN_POINT('Ctrl Pts',(-0.27407338601086,-0.524426862438141,
-0.361650378589733));
#65360=CARTESIAN_POINT('Ctrl Pts',(-0.361343679261664,-0.478818091258278,
-0.366286921904986));
#65361=CARTESIAN_POINT('Ctrl Pts',(-0.436982467484029,-0.41095296831949,
-0.370923465220239));
#65362=CARTESIAN_POINT('Ctrl Pts',(-0.491751620988836,-0.329120188109687,
-0.375560008535492));
#65363=CARTESIAN_POINT('Ctrl Pts',(-0.546520774493641,-0.24728740789989,
-0.380196551850745));
#65364=CARTESIAN_POINT('Ctrl Pts',(-0.580420293280891,-0.15148697041908,
-0.384833095165998));
#65365=CARTESIAN_POINT('Ctrl Pts',(-0.589309865767258,-0.0534194447361406,
-0.389469638481251));
#65366=CARTESIAN_POINT('Ctrl Pts',(-0.590919005744876,-0.0356678176107098,
-0.390308919247336));
#65367=CARTESIAN_POINT('Ctrl Pts',(-0.591708665159043,-0.0178419066505627,
-0.391148200013422));
#65368=CARTESIAN_POINT('Ctrl Pts',(-0.591690521605803,-1.43942328892088E-5,
-0.391987480779507));
#65369=CARTESIAN_POINT('Ctrl Pts',(-0.591703958414771,-1.21461586050568E-5,
-0.417162519220489));
#65370=CARTESIAN_POINT('Ctrl Pts',(-0.591716181366265,-0.0133475210726419,
-0.416534677406066));
#65371=CARTESIAN_POINT('Ctrl Pts',(-0.591274566785637,-0.0266820876886264,
-0.415906835591644));
#65372=CARTESIAN_POINT('Ctrl Pts',(-0.590373534468136,-0.0399855383001813,
-0.415278993777221));
#65373=CARTESIAN_POINT('Ctrl Pts',(-0.583719509086956,-0.138230069941527,
-0.410642450461968));
#65374=CARTESIAN_POINT('Ctrl Pts',(-0.552010395963128,-0.234777640062649,
-0.406005907146715));
#65375=CARTESIAN_POINT('Ctrl Pts',(-0.499118981880783,-0.31783642868596,
-0.401369363831461));
#65376=CARTESIAN_POINT('Ctrl Pts',(-0.44622756779844,-0.400895217309266,
-0.396732820516209));
#65377=CARTESIAN_POINT('Ctrl Pts',(-0.372153852757582,-0.470465224434766,
-0.392096277200956));
#65378=CARTESIAN_POINT('Ctrl Pts',(-0.285944816518956,-0.518049529851638,
-0.387459733885703));
#65379=CARTESIAN_POINT('Ctrl Pts',(-0.199735780280327,-0.565633835268512,
-0.38282319057045));
#65380=CARTESIAN_POINT('Ctrl Pts',(-0.101391422843937,-0.591232438976756,
-0.378186647255197));
#65381=CARTESIAN_POINT('Ctrl Pts',(-0.00292301448043288,-0.591718860152255,
-0.373550103939944));
#65382=CARTESIAN_POINT('Ctrl Pts',(0.0955453938830743,-0.592205281327754,
-0.368913560624691));
#65383=CARTESIAN_POINT('Ctrl Pts',(0.194137853173688,-0.567579519970502,
-0.364277017309438));
#65384=CARTESIAN_POINT('Ctrl Pts',(0.280812791245678,-0.520849238980347,
-0.359640473994185));
#65385=CARTESIAN_POINT('Ctrl Pts',(0.367487729317668,-0.474118957990191,
-0.355003930678932));
#65386=CARTESIAN_POINT('Ctrl Pts',(0.442245146171034,-0.40528415736713,
-0.350367387363679));
#65387=CARTESIAN_POINT('Ctrl Pts',(0.495954558248181,-0.322751963009284,
-0.345730844048426));
#65388=CARTESIAN_POINT('Ctrl Pts',(0.549663970325325,-0.240219768651443,
-0.341094300733173));
#65389=CARTESIAN_POINT('Ctrl Pts',(0.582325377626253,-0.143990180558819,
-0.33645775741792));
#65390=CARTESIAN_POINT('Ctrl Pts',(0.589949685089932,-0.045816182031098,
-0.331821214102667));
#65391=CARTESIAN_POINT('Ctrl Pts',(0.597573992553612,0.0523578164966226,
-0.327184670787414));
#65392=CARTESIAN_POINT('Ctrl Pts',(0.580161200180044,0.15247622545944,-0.322548127472161));
#65393=CARTESIAN_POINT('Ctrl Pts',(0.53983801621007,0.242311101124062,-0.317911584156908));
#65394=CARTESIAN_POINT('Ctrl Pts',(0.499514832240094,0.332145976788689,
-0.313275040841655));
#65395=CARTESIAN_POINT('Ctrl Pts',(0.436281256673708,0.411697319155121,
-0.308638497526402));
#65396=CARTESIAN_POINT('Ctrl Pts',(0.357860310801024,0.471249139443922,
-0.304001954211149));
#65397=CARTESIAN_POINT('Ctrl Pts',(0.279439364928339,0.530800959732723,
-0.299365410895896));
#65398=CARTESIAN_POINT('Ctrl Pts',(0.185831048749355,0.570353257943894,
-0.294728867580642));
#65399=CARTESIAN_POINT('Ctrl Pts',(0.0884681969955049,0.58507532130052,
-0.290092324265389));
#65400=CARTESIAN_POINT('Ctrl Pts',(-0.00889465475833943,0.599797384657145,
-0.285455780950136));
#65401=CARTESIAN_POINT('Ctrl Pts',(-0.110012042087051,0.589689213159228,
-0.280819237634883));
#65402=CARTESIAN_POINT('Ctrl Pts',(-0.202534011219225,0.555985366507808,
-0.276182694319631));
#65403=CARTESIAN_POINT('Ctrl Pts',(-0.2950559803514,0.522281519856387,-0.271546151004378));
#65404=CARTESIAN_POINT('Ctrl Pts',(-0.37898253128704,0.464981998051463,
-0.266909607689125));
#65405=CARTESIAN_POINT('Ctrl Pts',(-0.444063309934188,0.391085067789069,
-0.262273064373872));
#65406=CARTESIAN_POINT('Ctrl Pts',(-0.509144088581336,0.317188137526676,
-0.257636521058619));
#65407=CARTESIAN_POINT('Ctrl Pts',(-0.555379094939994,0.226693798806812,
-0.252999977743366));
#65408=CARTESIAN_POINT('Ctrl Pts',(-0.577121424898413,0.13065456131464,
-0.248363434428113));
#65409=CARTESIAN_POINT('Ctrl Pts',(-0.586814158998031,0.0878402542039476,
-0.246296462692239));
#65410=CARTESIAN_POINT('Ctrl Pts',(-0.591639272973499,0.0439239662231613,
-0.244229490956364));
#65411=CARTESIAN_POINT('Ctrl Pts',(-0.591626527824809,4.92094362445281E-6,
-0.24216251922049));
#65412=CARTESIAN_POINT('Origin',(0.,0.,-1.97));
#65413=CARTESIAN_POINT('',(-0.591724346791278,-4.07989592221547E-6,-0.0419874807795086));
#65414=CARTESIAN_POINT('',(-0.591724986204225,2.85874560315911E-6,-0.0671625192204902));
#65415=CARTESIAN_POINT('',(-0.591675,-7.2459289488551E-17,-1.97));
#65416=CARTESIAN_POINT('Ctrl Pts',(-0.591724346791278,-4.07989592221547E-6,
-0.0419874807795086));
#65417=CARTESIAN_POINT('Ctrl Pts',(-0.591705292818391,0.0966334251737516,
-0.0465378271140176));
#65418=CARTESIAN_POINT('Ctrl Pts',(-0.567555912119278,0.193285312577123,
-0.0510881734485265));
#65419=CARTESIAN_POINT('Ctrl Pts',(-0.522064928224495,0.278548318802823,
-0.0556385197830354));
#65420=CARTESIAN_POINT('Ctrl Pts',(-0.475712210919869,0.365426457848211,
-0.0602750630982883));
#65421=CARTESIAN_POINT('Ctrl Pts',(-0.407201686475803,0.440480150981304,
-0.0649116064135412));
#65422=CARTESIAN_POINT('Ctrl Pts',(-0.324903331847967,0.494547117028557,
-0.069548149728794));
#65423=CARTESIAN_POINT('Ctrl Pts',(-0.242604977220127,0.548614083075814,
-0.0741846930440472));
#65424=CARTESIAN_POINT('Ctrl Pts',(-0.146518792408516,0.581694322037228,
-0.0788212363593003));
#65425=CARTESIAN_POINT('Ctrl Pts',(-0.0483789899463179,0.589745342092519,
-0.0834577796745535));
#65426=CARTESIAN_POINT('Ctrl Pts',(0.04976081251588,0.59779636214781,-0.0880943229898067));
#65427=CARTESIAN_POINT('Ctrl Pts',(0.149954232628665,0.580818163296978,
-0.0927308663050599));
#65428=CARTESIAN_POINT('Ctrl Pts',(0.239963522432172,0.540885522215563,
-0.0973674096203131));
#65429=CARTESIAN_POINT('Ctrl Pts',(0.329972812235668,0.500952881134153,
-0.102003952935566));
#65430=CARTESIAN_POINT('Ctrl Pts',(0.409797971729889,0.438065797822166,
-0.106640496250818));
#65431=CARTESIAN_POINT('Ctrl Pts',(0.469689898424806,0.359904387670641,
-0.111277039566071));
#65432=CARTESIAN_POINT('Ctrl Pts',(0.52958182511973,0.281742977519106,-0.115913582881324));
#65433=CARTESIAN_POINT('Ctrl Pts',(0.569540519015346,0.188307240528029,
-0.120550126196577));
#65434=CARTESIAN_POINT('Ctrl Pts',(0.58468546397641,0.091009233937934,-0.12518666951183));
#65435=CARTESIAN_POINT('Ctrl Pts',(0.599830408937475,-0.00628877265216127,
-0.129823212827083));
#65436=CARTESIAN_POINT('Ctrl Pts',(0.590161604963988,-0.107449048841275,
-0.134459756142337));
#65437=CARTESIAN_POINT('Ctrl Pts',(0.556860035796763,-0.200116556369054,
-0.13909629945759));
#65438=CARTESIAN_POINT('Ctrl Pts',(0.523558466629538,-0.292784063896833,
-0.143732842772843));
#65439=CARTESIAN_POINT('Ctrl Pts',(0.466624132268574,-0.376958802763277,
-0.148369386088096));
#65440=CARTESIAN_POINT('Ctrl Pts',(0.393010653253385,-0.442360027824988,
-0.153005929403349));
#65441=CARTESIAN_POINT('Ctrl Pts',(0.319397174238201,-0.507761252886696,
-0.157642472718602));
#65442=CARTESIAN_POINT('Ctrl Pts',(0.229104550568795,-0.554388964143672,
-0.162279016033855));
#65443=CARTESIAN_POINT('Ctrl Pts',(0.133160678021782,-0.576548334788175,
-0.166915559349108));
#65444=CARTESIAN_POINT('Ctrl Pts',(0.0372168054747698,-0.598707705432679,
-0.171552102664361));
#65445=CARTESIAN_POINT('Ctrl Pts',(-0.0643783159498496,-0.596398735464708,
-0.176188645979614));
#65446=CARTESIAN_POINT('Ctrl Pts',(-0.159216396050027,-0.569903409913743,
-0.180825189294867));
#65447=CARTESIAN_POINT('Ctrl Pts',(-0.254054476150203,-0.543408084362778,
-0.185461732610119));
#65448=CARTESIAN_POINT('Ctrl Pts',(-0.342135514925938,-0.492726403228817,
-0.190098275925372));
#65449=CARTESIAN_POINT('Ctrl Pts',(-0.412701744766264,-0.424048374991887,
-0.194734819240625));
#65450=CARTESIAN_POINT('Ctrl Pts',(-0.483267974606591,-0.355370346754957,
-0.199371362555878));
#65451=CARTESIAN_POINT('Ctrl Pts',(-0.536319395511509,-0.268695971415057,
-0.204007905871131));
#65452=CARTESIAN_POINT('Ctrl Pts',(-0.56537658482579,-0.174611202700902,
-0.208644449186384));
#65453=CARTESIAN_POINT('Ctrl Pts',(-0.582805161243839,-0.118178917954655,
-0.211425459717425));
#65454=CARTESIAN_POINT('Ctrl Pts',(-0.591601498377145,-0.0590806470709061,
-0.214206470248466));
#65455=CARTESIAN_POINT('Ctrl Pts',(-0.591632161208708,8.69568651094832E-6,
-0.216987480779508));
#65456=CARTESIAN_POINT('Ctrl Pts',(-0.591626527824809,4.92094362445281E-6,
-0.24216251922049));
#65457=CARTESIAN_POINT('Ctrl Pts',(-0.591610683596618,-0.0545933730654515,
-0.239592947641111));
#65458=CARTESIAN_POINT('Ctrl Pts',(-0.58411821465468,-0.109195928316423,
-0.237023376061733));
#65459=CARTESIAN_POINT('Ctrl Pts',(-0.569206298617938,-0.161690887462097,
-0.234453804482355));
#65460=CARTESIAN_POINT('Ctrl Pts',(-0.542299188820864,-0.256412962482184,
-0.229817261167102));
#65461=CARTESIAN_POINT('Ctrl Pts',(-0.491235315668536,-0.344272976257873,
-0.225180717851848));
#65462=CARTESIAN_POINT('Ctrl Pts',(-0.422251356090625,-0.414540161825823,
-0.220544174536595));
#65463=CARTESIAN_POINT('Ctrl Pts',(-0.353267396512714,-0.484807347393774,
-0.215907631221342));
#65464=CARTESIAN_POINT('Ctrl Pts',(-0.26636335050922,-0.537481704753986,
-0.211271087906089));
#65465=CARTESIAN_POINT('Ctrl Pts',(-0.172153227914291,-0.566129861023301,
-0.206634544590836));
#65466=CARTESIAN_POINT('Ctrl Pts',(-0.0779431053193665,-0.594778017292615,
-0.201998001275583));
#65467=CARTESIAN_POINT('Ctrl Pts',(0.0235730938669932,-0.599399972471034,
-0.19736145796033));
#65468=CARTESIAN_POINT('Ctrl Pts',(0.119996706913808,-0.5794312244984,-0.192724914645077));
#65469=CARTESIAN_POINT('Ctrl Pts',(0.216420319960622,-0.559462476525766,
-0.188088371329824));
#65470=CARTESIAN_POINT('Ctrl Pts',(0.307751346867891,-0.51490302540208,
-0.183451828014571));
#65471=CARTESIAN_POINT('Ctrl Pts',(0.382835089497417,-0.451195132399647,
-0.178815284699319));
#65472=CARTESIAN_POINT('Ctrl Pts',(0.457918832126947,-0.38748723939721,
-0.174178741384065));
#65473=CARTESIAN_POINT('Ctrl Pts',(0.516755290478732,-0.304630904516024,
-0.169542198068812));
#65474=CARTESIAN_POINT('Ctrl Pts',(0.552158483830049,-0.212745769664315,
-0.164905654753559));
#65475=CARTESIAN_POINT('Ctrl Pts',(0.587561677181366,-0.120860634812606,
-0.160269111438306));
#65476=CARTESIAN_POINT('Ctrl Pts',(0.599531605532214,-0.0199466999903742,
-0.155632568123053));
#65477=CARTESIAN_POINT('Ctrl Pts',(0.586606324919602,0.0776709266649116,
-0.150996024807799));
#65478=CARTESIAN_POINT('Ctrl Pts',(0.573681044306991,0.175288553320192,
-0.146359481492547));
#65479=CARTESIAN_POINT('Ctrl Pts',(0.535860554730924,0.269609871808526,
-0.141722938177294));
#65480=CARTESIAN_POINT('Ctrl Pts',(0.477764052747148,0.349114970849799,
-0.137086394862041));
#65481=CARTESIAN_POINT('Ctrl Pts',(0.419667550763372,0.428620069891072,
-0.132449851546788));
#65482=CARTESIAN_POINT('Ctrl Pts',(0.341295036371886,0.493308949485282,
-0.127813308231535));
#65483=CARTESIAN_POINT('Ctrl Pts',(0.252218526483655,0.535280833604227,
-0.123176764916282));
#65484=CARTESIAN_POINT('Ctrl Pts',(0.163142016595425,0.577252717723171,
-0.118540221601029));
#65485=CARTESIAN_POINT('Ctrl Pts',(0.0633615112104499,0.596507606366848,
-0.113903678285777));
#65486=CARTESIAN_POINT('Ctrl Pts',(-0.0349363236836362,0.590693829557053,
-0.109267134970524));
#65487=CARTESIAN_POINT('Ctrl Pts',(-0.133234158577722,0.584880052747258,
-0.104630591655271));
#65488=CARTESIAN_POINT('Ctrl Pts',(-0.23004932298092,0.553997610483989,
-0.0999940483400178));
#65489=CARTESIAN_POINT('Ctrl Pts',(-0.313557298800687,0.501818280580585,
-0.0953575050247649));
#65490=CARTESIAN_POINT('Ctrl Pts',(-0.397065274620459,0.449638950677177,
-0.0907209617095118));
#65491=CARTESIAN_POINT('Ctrl Pts',(-0.4672660618568,0.37616273313363,-0.0860844183942587));
#65492=CARTESIAN_POINT('Ctrl Pts',(-0.51558573043494,0.290363717785175,
-0.0814478750790056));
#65493=CARTESIAN_POINT('Ctrl Pts',(-0.563905399013081,0.20456470243672,
-0.0768113317637524));
#65494=CARTESIAN_POINT('Ctrl Pts',(-0.59034394893302,0.106442889283356,
-0.0721747884484991));
#65495=CARTESIAN_POINT('Ctrl Pts',(-0.591672253399873,0.00798220150416167,
-0.067538245133246));
#65496=CARTESIAN_POINT('Ctrl Pts',(-0.591708133463553,0.00532258856473375,
-0.0674130031623274));
#65497=CARTESIAN_POINT('Ctrl Pts',(-0.591725691981876,0.00266272836739514,
-0.0672877611914088));
#65498=CARTESIAN_POINT('Ctrl Pts',(-0.591724986204225,2.85874560315911E-6,
-0.0671625192204902));
#65499=CARTESIAN_POINT('Origin',(0.,0.,-4.27183905640093));
#65500=CARTESIAN_POINT('',(-0.491789390605438,7.22821825122446E-6,-0.159339056400925));
#65501=CARTESIAN_POINT('',(-0.491866550623049,2.37630884976706E-6,-0.124810943599073));
#65502=CARTESIAN_POINT('',(-0.491825,-1.07154090996976E-14,-4.27183905640093));
#65503=CARTESIAN_POINT('',(-0.416126897194384,0.262207742448202,-3.33066907387547E-16));
#65504=CARTESIAN_POINT('Ctrl Pts',(-0.491789390605438,7.22821825123801E-6,
-0.159339056400925));
#65505=CARTESIAN_POINT('Ctrl Pts',(-0.491763902377726,-0.0491103042136956,
-0.156558045869883));
#65506=CARTESIAN_POINT('Ctrl Pts',(-0.472261535530513,-0.180137132920269,
-0.149140492023589));
#65507=CARTESIAN_POINT('Ctrl Pts',(-0.357613988294798,-0.367446056440282,
-0.137086394862041));
#65508=CARTESIAN_POINT('Ctrl Pts',(-0.137964061075247,-0.493832254050675,
-0.123176764916282));
#65509=CARTESIAN_POINT('Ctrl Pts',(0.115386277850666,-0.499590191201122,
-0.109267134970524));
#65510=CARTESIAN_POINT('Ctrl Pts',(0.340551290583365,-0.383313481407925,
-0.0953575050247649));
#65511=CARTESIAN_POINT('Ctrl Pts',(0.482529888616476,-0.173404793650348,
-0.0814478750790055));
#65512=CARTESIAN_POINT('Ctrl Pts',(0.506641231064238,0.0788611606491063,
-0.0675382451332463));
#65513=CARTESIAN_POINT('Ctrl Pts',(0.406995219528124,0.311864235034375,
-0.0536286151874873));
#65514=CARTESIAN_POINT('Ctrl Pts',(0.207933188506461,0.468687354567501,
-0.0397189852417286));
#65515=CARTESIAN_POINT('Ctrl Pts',(-0.0419216921981646,0.511026320975463,
-0.0258093552959692));
#65516=CARTESIAN_POINT('Ctrl Pts',(-0.269993129330808,0.432506628936349,
-0.0125696935487264));
#65517=CARTESIAN_POINT('Ctrl Pts',(-0.3787346762928,0.321423241660421,-0.00396657511673683));
#65518=CARTESIAN_POINT('Ctrl Pts',(-0.416126897194384,0.262207742448202,
-3.5377516888202E-16));
#65519=CARTESIAN_POINT('',(0.112693552167563,0.478740006605732,0.));
#65520=CARTESIAN_POINT('Origin',(0.,0.,0.));
#65521=CARTESIAN_POINT('Ctrl Pts',(-0.491866550623049,2.37630884974928E-6,
-0.124810943599073));
#65522=CARTESIAN_POINT('Ctrl Pts',(-0.491845418300655,-0.0796391684329172,
-0.120299642254739));
#65523=CARTESIAN_POINT('Ctrl Pts',(-0.451858604081596,-0.241153864017004,
-0.111151797595152));
#65524=CARTESIAN_POINT('Ctrl Pts',(-0.283335167309922,-0.427346729913706,
-0.0973674096203128));
#65525=CARTESIAN_POINT('Ctrl Pts',(-0.0440696378965106,-0.510845571762323,
-0.0834577796745537));
#65526=CARTESIAN_POINT('Ctrl Pts',(0.205959307621291,-0.469556250960448,
-0.0695481497287949));
#65527=CARTESIAN_POINT('Ctrl Pts',(0.405681497053104,-0.313576606935647,
-0.0556385197830361));
#65528=CARTESIAN_POINT('Ctrl Pts',(0.506302444914719,-0.0809840427845483,
-0.0417288898372769));
#65529=CARTESIAN_POINT('Ctrl Pts',(0.48325998950616,0.171359585523517,-0.0278192598915182));
#65530=CARTESIAN_POINT('Ctrl Pts',(0.342150143078732,0.381908292889331,
-0.0139096299457593));
#65531=CARTESIAN_POINT('Ctrl Pts',(0.192389430706698,0.459979903999379,
-0.00463654331525315));
#65532=CARTESIAN_POINT('Ctrl Pts',(0.112693552167563,0.478740006605732,
0.));
#65533=CARTESIAN_POINT('Origin',(0.,0.,-4.27183905640093));
#65534=CARTESIAN_POINT('',(-0.491837902207756,-1.19650882245787E-5,-0.334339056400925));
#65535=CARTESIAN_POINT('',(-0.49178470790119,4.0904940728087E-6,-0.299810943599072));
#65536=CARTESIAN_POINT('',(-0.491825,-1.07154090996976E-14,-4.27183905640093));
#65537=CARTESIAN_POINT('Ctrl Pts',(-0.491837902207756,-1.19650882245553E-5,
-0.334339056400925));
#65538=CARTESIAN_POINT('Ctrl Pts',(-0.491852983887855,-0.0148309388404159,
-0.333499775634839));
#65539=CARTESIAN_POINT('Ctrl Pts',(-0.4875703651248,-0.111507530516403,
-0.3280239515535));
#65540=CARTESIAN_POINT('Ctrl Pts',(-0.426112222229761,-0.285188962782551,
-0.317911584156906));
#65541=CARTESIAN_POINT('Ctrl Pts',(-0.237489851752064,-0.454425946376765,
-0.304001954211149));
#65542=CARTESIAN_POINT('Ctrl Pts',(0.00914407872677023,-0.512660468783674,
-0.290092324265389));
#65543=CARTESIAN_POINT('Ctrl Pts',(0.253544388403441,-0.445667604307889,
-0.27618269431963));
#65544=CARTESIAN_POINT('Ctrl Pts',(0.436011502246361,-0.269811675703265,
-0.262273064373872));
#65545=CARTESIAN_POINT('Ctrl Pts',(0.511974244464808,-0.0280489468379449,
-0.248363434428113));
#65546=CARTESIAN_POINT('Ctrl Pts',(0.462877223624254,0.220565288020147,
-0.234453804482355));
#65547=CARTESIAN_POINT('Ctrl Pts',(0.300713351069406,0.41530212009148,-0.220544174536595));
#65548=CARTESIAN_POINT('Ctrl Pts',(0.0650943374357338,0.508593253514698,
-0.206634544590836));
#65549=CARTESIAN_POINT('Ctrl Pts',(-0.186425246756546,0.477650497890165,
-0.192724914645077));
#65550=CARTESIAN_POINT('Ctrl Pts',(-0.392406802818875,0.330032227073166,
-0.178815284699318));
#65551=CARTESIAN_POINT('Ctrl Pts',(-0.480516842828346,0.147429109124288,
-0.167686665284601));
#65552=CARTESIAN_POINT('Ctrl Pts',(-0.491806396741015,0.0327791975041391,
-0.161194589185136));
#65553=CARTESIAN_POINT('Ctrl Pts',(-0.491789390605438,7.22821825123801E-6,
-0.159339056400925));
#65554=CARTESIAN_POINT('Ctrl Pts',(-0.49178470790119,4.0904940727983E-6,
-0.299810943599072));
#65555=CARTESIAN_POINT('Ctrl Pts',(-0.491771537516212,-0.0453802944317873,
-0.297241372019695));
#65556=CARTESIAN_POINT('Ctrl Pts',(-0.474305564106061,-0.172666344668371,
-0.290035257125064));
#65557=CARTESIAN_POINT('Ctrl Pts',(-0.365888908126138,-0.359207010306768,
-0.278192598915179));
#65558=CARTESIAN_POINT('Ctrl Pts',(-0.149174077725999,-0.490562395317217,
-0.26428296896942));
#65559=CARTESIAN_POINT('Ctrl Pts',(0.103979450806552,-0.502088282530429,
-0.250373339023661));
#65560=CARTESIAN_POINT('Ctrl Pts',(0.331733956110991,-0.390969245649164,
-0.236463709077902));
#65561=CARTESIAN_POINT('Ctrl Pts',(0.478455929130976,-0.184348295450463,
-0.222554079132143));
#65562=CARTESIAN_POINT('Ctrl Pts',(0.508305643980286,0.067303351115353,
-0.208644449186384));
#65563=CARTESIAN_POINT('Ctrl Pts',(0.413991726952782,0.302514822609971,
-0.194734819240625));
#65564=CARTESIAN_POINT('Ctrl Pts',(0.218552193979818,0.463831127370637,
-0.180825189294866));
#65565=CARTESIAN_POINT('Ctrl Pts',(-0.0302729907633189,0.511847533035115,
-0.166915559349108));
#65566=CARTESIAN_POINT('Ctrl Pts',(-0.271703429260484,0.434835201098837,
-0.153005929403349));
#65567=CARTESIAN_POINT('Ctrl Pts',(-0.446764918333941,0.251605688139759,
-0.13909629945759));
#65568=CARTESIAN_POINT('Ctrl Pts',(-0.491312211182185,0.0862766077408699,
-0.129697970856164));
#65569=CARTESIAN_POINT('Ctrl Pts',(-0.491867137294944,0.00221337115693925,
-0.124936185569992));
#65570=CARTESIAN_POINT('Ctrl Pts',(-0.491866550623049,2.37630884974928E-6,
-0.124810943599073));
#65571=CARTESIAN_POINT('Origin',(0.,0.,-4.27183905640093));
#65572=CARTESIAN_POINT('',(-0.49182316548349,1.28554485876743E-5,-0.509339056400925));
#65573=CARTESIAN_POINT('',(-0.49184907144521,-1.00963949215827E-5,-0.474810943599073));
#65574=CARTESIAN_POINT('',(-0.491825,-1.07154090996976E-14,-4.27183905640093));
#65575=CARTESIAN_POINT('Ctrl Pts',(-0.49182316548349,1.28554485876817E-5,
-0.509339056400925));
#65576=CARTESIAN_POINT('Ctrl Pts',(-0.491759186460215,-0.0623931626016951,
-0.505804962084542));
#65577=CARTESIAN_POINT('Ctrl Pts',(-0.46420000164389,-0.206727437724254,
-0.497634324452905));
#65578=CARTESIAN_POINT('Ctrl Pts',(-0.326665047731261,-0.395214267223794,
-0.484827143506015));
#65579=CARTESIAN_POINT('Ctrl Pts',(-0.0974966584912855,-0.503387298220306,
-0.470917513560256));
#65580=CARTESIAN_POINT('Ctrl Pts',(0.155487204176033,-0.488598096357353,
-0.457007883614497));
#65581=CARTESIAN_POINT('Ctrl Pts',(0.37049026384305,-0.354459214612929,
-0.443098253668739));
#65582=CARTESIAN_POINT('Ctrl Pts',(0.494993801063038,-0.133736709005703,
-0.429188623722979));
#65583=CARTESIAN_POINT('Ctrl Pts',(0.498585381931524,0.11965361403109,-0.41527899377722));
#65584=CARTESIAN_POINT('Ctrl Pts',(0.380387692291731,0.343816192142657,
-0.401369363831462));
#65585=CARTESIAN_POINT('Ctrl Pts',(0.169272838945517,0.483994913632211,
-0.387459733885702));
#65586=CARTESIAN_POINT('Ctrl Pts',(-0.0831902294088231,0.505948373015826,
-0.373550103939943));
#65587=CARTESIAN_POINT('Ctrl Pts',(-0.315332450581861,0.404314006728254,
-0.359640473994185));
#65588=CARTESIAN_POINT('Ctrl Pts',(-0.461089117569146,0.216009520375589,
-0.346570124814512));
#65589=CARTESIAN_POINT('Ctrl Pts',(-0.491769666283222,0.0670353643873584,
-0.338136318950092));
#65590=CARTESIAN_POINT('Ctrl Pts',(-0.491837902207756,-1.19650882245553E-5,
-0.334339056400925));
#65591=CARTESIAN_POINT('Ctrl Pts',(-0.49184907144521,-1.00963949215896E-5,
-0.474810943599073));
#65592=CARTESIAN_POINT('Ctrl Pts',(-0.491859231673575,-0.0110950176221044,
-0.47418310178465));
#65593=CARTESIAN_POINT('Ctrl Pts',(-0.488781234601853,-0.104035239247785,
-0.468918716654975));
#65594=CARTESIAN_POINT('Ctrl Pts',(-0.432496181911419,-0.275411368569959,
-0.459017788210046));
#65595=CARTESIAN_POINT('Ctrl Pts',(-0.247776674242662,-0.448899865233663,
-0.445108158264288));
#65596=CARTESIAN_POINT('Ctrl Pts',(-0.0025328481751963,-0.512735754541854,
-0.431198528318528));
#65597=CARTESIAN_POINT('Ctrl Pts',(0.243329675797957,-0.451325866953922,
-0.41728889837277));
#65598=CARTESIAN_POINT('Ctrl Pts',(0.429754148070265,-0.279670773449364,
-0.40337926842701));
#65599=CARTESIAN_POINT('Ctrl Pts',(0.511202730378688,-0.0397006014952209,
-0.389469638481251));
#65600=CARTESIAN_POINT('Ctrl Pts',(0.467780007046806,0.209967221996417,
-0.375560008535492));
#65601=CARTESIAN_POINT('Ctrl Pts',(0.310092830963972,0.408346428280455,
-0.361650378589733));
#65602=CARTESIAN_POINT('Ctrl Pts',(0.0766593914673165,0.506979000559367,
-0.347740748643974));
#65603=CARTESIAN_POINT('Ctrl Pts',(-0.175499609789847,0.481771996138208,
-0.333831118698215));
#65604=CARTESIAN_POINT('Ctrl Pts',(-0.384789384990357,0.338882720885541,
-0.319921488752456));
#65605=CARTESIAN_POINT('Ctrl Pts',(-0.478787527436172,0.154903082696593,
-0.308581430386075));
#65606=CARTESIAN_POINT('Ctrl Pts',(-0.491795302201702,0.0365114373392391,
-0.301877915334947));
#65607=CARTESIAN_POINT('Ctrl Pts',(-0.49178470790119,4.0904940727983E-6,
-0.299810943599072));
#65608=CARTESIAN_POINT('Origin',(0.,0.,-4.27183905640093));
#65609=CARTESIAN_POINT('',(-0.491798649685846,-1.03788440164814E-5,-0.684339056400923));
#65610=CARTESIAN_POINT('',(-0.491811749329251,1.24090953615708E-5,-0.649810943599071));
#65611=CARTESIAN_POINT('',(-0.491825,-1.07154090996976E-14,-4.27183905640093));
#65612=CARTESIAN_POINT('Ctrl Pts',(-0.491798649685846,-1.03788440165044E-5,
-0.684339056400923));
#65613=CARTESIAN_POINT('Ctrl Pts',(-0.491820132916021,-0.0281328181413851,
-0.682746691849496));
#65614=CARTESIAN_POINT('Ctrl Pts',(-0.48254192569275,-0.138126322570039,
-0.676517783982815));
#65615=CARTESIAN_POINT('Ctrl Pts',(-0.401603104826651,-0.318777848383641,
-0.665652332800882));
#65616=CARTESIAN_POINT('Ctrl Pts',(-0.199888170155967,-0.472174850937878,
-0.651742702855122));
#65617=CARTESIAN_POINT('Ctrl Pts',(0.0506533753796834,-0.510233873815872,
-0.637833072909363));
#65618=CARTESIAN_POINT('Ctrl Pts',(0.288821839273072,-0.423658253295539,
-0.623923442963605));
#65619=CARTESIAN_POINT('Ctrl Pts',(0.45643989718452,-0.233595784817902,
-0.610013813017846));
#65620=CARTESIAN_POINT('Ctrl Pts',(0.512563546869181,0.0135270413392405,
-0.596104183072087));
#65621=CARTESIAN_POINT('Ctrl Pts',(0.443483484763275,0.257345622011976,
-0.582194553126329));
#65622=CARTESIAN_POINT('Ctrl Pts',(0.266073872596039,0.438302480883072,
-0.568284923180568));
#65623=CARTESIAN_POINT('Ctrl Pts',(0.0236704920209714,0.51219535163255,
-0.55437529323481));
#65624=CARTESIAN_POINT('Ctrl Pts',(-0.224514871059556,0.460974449508451,
-0.540465663289051));
#65625=CARTESIAN_POINT('Ctrl Pts',(-0.417858067972524,0.297151485705153,
-0.526556033343292));
#65626=CARTESIAN_POINT('Ctrl Pts',(-0.485940965058413,0.120808897856263,
-0.516180497713917));
#65627=CARTESIAN_POINT('Ctrl Pts',(-0.491843123527572,0.019480205769144,
-0.510441505399794));
#65628=CARTESIAN_POINT('Ctrl Pts',(-0.49182316548349,1.28554485876817E-5,
-0.509339056400925));
#65629=CARTESIAN_POINT('Ctrl Pts',(-0.491811749329251,1.24090953615708E-5,
-0.649810943599071));
#65630=CARTESIAN_POINT('Ctrl Pts',(-0.491755982274121,-0.058663874621788,
-0.646488288234352));
#65631=CARTESIAN_POINT('Ctrl Pts',(-0.466588151730041,-0.199265543584639,
-0.638529089554379));
#65632=CARTESIAN_POINT('Ctrl Pts',(-0.33558034712377,-0.387672800090266,
-0.625933347559152));
#65633=CARTESIAN_POINT('Ctrl Pts',(-0.108934757177873,-0.501036513623642,
-0.612023717613395));
#65634=CARTESIAN_POINT('Ctrl Pts',(0.144320286415244,-0.49201221959882,
-0.598114087667635));
#65635=CARTESIAN_POINT('Ctrl Pts',(0.362322265961503,-0.362804279045959,
-0.584204457721877));
#65636=CARTESIAN_POINT('Ctrl Pts',(0.491819916942383,-0.144974268766304,
-0.570294827776118));
#65637=CARTESIAN_POINT('Ctrl Pts',(0.501180895095398,0.108268553592046,
-0.55638519783036));
#65638=CARTESIAN_POINT('Ctrl Pts',(0.388118597680438,0.33506465561158,-0.542475567884599));
#65639=CARTESIAN_POINT('Ctrl Pts',(0.180250711102229,0.480014635665076,
-0.528565937938842));
#65640=CARTESIAN_POINT('Ctrl Pts',(-0.0716469513364315,0.507711614668931,
-0.514656307993081));
#65641=CARTESIAN_POINT('Ctrl Pts',(-0.306043438944004,0.411390061601957,
-0.500746678047323));
#65642=CARTESIAN_POINT('Ctrl Pts',(-0.45847713183902,0.223461935246029,
-0.487464889915986));
#65643=CARTESIAN_POINT('Ctrl Pts',(-0.491784199495365,0.0707659165103001,
-0.478819645099903));
#65644=CARTESIAN_POINT('Ctrl Pts',(-0.49184907144521,-1.00963949215896E-5,
-0.474810943599073));
#65645=CARTESIAN_POINT('Origin',(0.,0.,-4.27183905640093));
#65646=CARTESIAN_POINT('',(-0.491860973371918,6.25837308208287E-6,-0.859339056400924));
#65647=CARTESIAN_POINT('',(-0.491808348730261,-1.20621083624095E-5,-0.824810943599071));
#65648=CARTESIAN_POINT('',(-0.491825,-1.07154090996976E-14,-4.27183905640093));
#65649=CARTESIAN_POINT('Ctrl Pts',(-0.491860973371918,6.25837308207075E-6,
-0.859339056400924));
#65650=CARTESIAN_POINT('Ctrl Pts',(-0.491813051771,-0.0756811199232177,
-0.855051878299199));
#65651=CARTESIAN_POINT('Ctrl Pts',(-0.454881898913209,-0.233268842049668,
-0.846128156882221));
#65652=CARTESIAN_POINT('Ctrl Pts',(-0.293567896890941,-0.420383468206752,
-0.832567892149989));
#65653=CARTESIAN_POINT('Ctrl Pts',(-0.0563880943787678,-0.509631978234137,
-0.818658262204231));
#65654=CARTESIAN_POINT('Ctrl Pts',(0.194565607506746,-0.474392869678749,
-0.804748632258471));
#65655=CARTESIAN_POINT('Ctrl Pts',(0.397992838976195,-0.323273986813317,
-0.790839002312714));
#65656=CARTESIAN_POINT('Ctrl Pts',(0.504202503940466,-0.0931890843751128,
-0.776929372366952));
#65657=CARTESIAN_POINT('Ctrl Pts',(0.487250806039511,0.159659081922555,
-0.763019742421195));
#65658=CARTESIAN_POINT('Ctrl Pts',(0.351278530374647,0.373507382155073,
-0.749110112475436));
#65659=CARTESIAN_POINT('Ctrl Pts',(0.12949957543287,0.496119169544188,-0.735200482529676));
#65660=CARTESIAN_POINT('Ctrl Pts',(-0.123912193856582,0.497544107230863,
-0.721290852583919));
#65661=CARTESIAN_POINT('Ctrl Pts',(-0.347055976470588,0.377434126202911,
-0.707381222638158));
#65662=CARTESIAN_POINT('Ctrl Pts',(-0.469584188812454,0.18943305115538,
-0.695063957243828));
#65663=CARTESIAN_POINT('Ctrl Pts',(-0.49175757944661,0.0537522676675991,
-0.687383235164749));
#65664=CARTESIAN_POINT('Ctrl Pts',(-0.491798649685846,-1.03788440165044E-5,
-0.684339056400923));
#65665=CARTESIAN_POINT('Ctrl Pts',(-0.491808348730261,-1.20621083624407E-5,
-0.824810943599071));
#65666=CARTESIAN_POINT('Ctrl Pts',(-0.49183063390641,-0.0243989399446512,
-0.823430017999307));
#65667=CARTESIAN_POINT('Ctrl Pts',(-0.484067683462823,-0.130652210543813,
-0.81741254908429));
#65668=CARTESIAN_POINT('Ctrl Pts',(-0.408758323003886,-0.309549677241936,
-0.80675853685402));
#65669=CARTESIAN_POINT('Ctrl Pts',(-0.210588930608419,-0.467500450920358,
-0.792848906908262));
#65670=CARTESIAN_POINT('Ctrl Pts',(0.0390209435287369,-0.511255058920363,
-0.778939276962502));
#65671=CARTESIAN_POINT('Ctrl Pts',(0.279099185935138,-0.430125579006736,
-0.765029647016744));
#65672=CARTESIAN_POINT('Ctrl Pts',(0.45100197136601,-0.243929479828719,
-0.751120017070984));
#65673=CARTESIAN_POINT('Ctrl Pts',(0.512738668738538,0.00185118496315108,
-0.737210387125225));
#65674=CARTESIAN_POINT('Ctrl Pts',(0.449228877364958,0.247179661475123,
-0.723300757179467));
#65675=CARTESIAN_POINT('Ctrl Pts',(0.27598611096193,0.432129651680657,-0.709391127233707));
#65676=CARTESIAN_POINT('Ctrl Pts',(0.0353283172785953,0.511523488516217,
-0.695481497287949));
#65677=CARTESIAN_POINT('Ctrl Pts',(-0.213959111659945,0.46596766823807,
-0.681571867342189));
#65678=CARTESIAN_POINT('Ctrl Pts',(-0.41098282595302,0.306590094551677,
-0.667662237396431));
#65679=CARTESIAN_POINT('Ctrl Pts',(-0.484532737369335,0.128282565717192,
-0.657075262815391));
#65680=CARTESIAN_POINT('Ctrl Pts',(-0.4918338014694,0.0232149545584419,
-0.651124831549605));
#65681=CARTESIAN_POINT('Ctrl Pts',(-0.491811749329251,1.24090953615708E-5,
-0.649810943599071));
#65682=CARTESIAN_POINT('Origin',(0.,0.,-4.27183905640093));
#65683=CARTESIAN_POINT('',(-0.49178273288147,4.4982614547824E-7,-1.03433905640092));
#65684=CARTESIAN_POINT('',(-0.491852307000294,9.3039398275617E-6,-0.999810943599072));
#65685=CARTESIAN_POINT('',(-0.491825,-1.07154090996976E-14,-4.27183905640093));
#65686=CARTESIAN_POINT('Ctrl Pts',(-0.49178273288147,4.49826145484944E-7,
-1.03433905640092));
#65687=CARTESIAN_POINT('Ctrl Pts',(-0.491781417251355,-0.0414258932373119,
-1.03199360806415));
#65688=CARTESIAN_POINT('Ctrl Pts',(-0.476369267714836,-0.164745870733351,
-1.02501161641213));
#65689=CARTESIAN_POINT('Ctrl Pts',(-0.37445296760404,-0.350270389098243,
-1.01339308144486));
#65690=CARTESIAN_POINT('Ctrl Pts',(-0.160971985229762,-0.48681864220436,
-0.999483451499097));
#65691=CARTESIAN_POINT('Ctrl Pts',(0.091829565624597,-0.50445188204992,
-0.985573821553339));
#65692=CARTESIAN_POINT('Ctrl Pts',(0.322199941771856,-0.398862843529854,
-0.971664191607578));
#65693=CARTESIAN_POINT('Ctrl Pts',(0.473866654939281,-0.195843722807663,
-0.957754561661822));
#65694=CARTESIAN_POINT('Ctrl Pts',(0.509782132080318,0.0550140730918329,
-0.94384493171606));
#65695=CARTESIAN_POINT('Ctrl Pts',(0.421173312613008,0.292433601299668,
-0.929935301770304));
#65696=CARTESIAN_POINT('Ctrl Pts',(0.229684640748129,0.458420479724576,
-0.916025671824541));
#65697=CARTESIAN_POINT('Ctrl Pts',(-0.017909015052109,0.512429153743588,
-0.902116041878785));
#65698=CARTESIAN_POINT('Ctrl Pts',(-0.261128042237548,0.441266944132112,
-0.888206411933025));
#65699=CARTESIAN_POINT('Ctrl Pts',(-0.440561417203972,0.262316618035793,
-0.874296781987266));
#65700=CARTESIAN_POINT('Ctrl Pts',(-0.490243642695107,0.0941950370601843,
-0.864674330143233));
#65701=CARTESIAN_POINT('Ctrl Pts',(-0.491864878537493,0.00617407702965306,
-0.859688421614452));
#65702=CARTESIAN_POINT('Ctrl Pts',(-0.491860973371918,6.25837308207075E-6,
-0.859339056400924));
#65703=CARTESIAN_POINT('Ctrl Pts',(-0.491852307000294,9.30393982757037E-6,
-0.999810943599072));
#65704=CARTESIAN_POINT('Ctrl Pts',(-0.491790081377928,-0.0719489292099996,
-0.99573520444901));
#65705=CARTESIAN_POINT('Ctrl Pts',(-0.457627845654389,-0.225823669989117,
-0.987022921983695));
#65706=CARTESIAN_POINT('Ctrl Pts',(-0.30306494471812,-0.413589178519626,
-0.973674096203129));
#65707=CARTESIAN_POINT('Ctrl Pts',(-0.0679790606200691,-0.508215718590787,
-0.959764466257369));
#65708=CARTESIAN_POINT('Ctrl Pts',(0.183712043973384,-0.478700589308868,
-0.94585483631161));
#65709=CARTESIAN_POINT('Ctrl Pts',(0.390527874180675,-0.332253440604396,
-0.931945206365851));
#65710=CARTESIAN_POINT('Ctrl Pts',(0.501949602127359,-0.104646864404638,
-0.918035576420092));
#65711=CARTESIAN_POINT('Ctrl Pts',(0.490760282718032,0.148521763428982,
-0.904125946474333));
#65712=CARTESIAN_POINT('Ctrl Pts',(0.359693126948704,0.365411033948621,
-0.890216316528574));
#65713=CARTESIAN_POINT('Ctrl Pts',(0.140763861447594,0.493041483666333,
-0.876306686582815));
#65714=CARTESIAN_POINT('Ctrl Pts',(-0.112549741462726,0.500236868895336,
-0.862397056637057));
#65715=CARTESIAN_POINT('Ctrl Pts',(-0.338370859824982,0.385239575494054,
-0.848487426691298));
#65716=CARTESIAN_POINT('Ctrl Pts',(-0.467324823515431,0.196899023737536,
-0.835958722345302));
#65717=CARTESIAN_POINT('Ctrl Pts',(-0.491755810045864,0.0574815143180991,
-0.82806656131456));
#65718=CARTESIAN_POINT('Ctrl Pts',(-0.491808348730261,-1.20621083624407E-5,
-0.824810943599071));
#65719=CARTESIAN_POINT('Origin',(0.,0.,-4.27183905640093));
#65720=CARTESIAN_POINT('',(-0.49185900932756,-7.11307669150856E-6,-1.20933905640092));
#65721=CARTESIAN_POINT('',(-0.491783786383942,-3.02292213444355E-6,-1.17481094359907));
#65722=CARTESIAN_POINT('',(-0.491825,-1.07154090996976E-14,-4.27183905640093));
#65723=CARTESIAN_POINT('Ctrl Pts',(-0.49185900932756,-7.11307669150688E-6,
-1.20933905640092));
#65724=CARTESIAN_POINT('Ctrl Pts',(-0.491864019509531,-0.00713458797730284,
-1.20893533782911));
#65725=CARTESIAN_POINT('Ctrl Pts',(-0.489969969681151,-0.0961155435516917,
-1.20389507594204));
#65726=CARTESIAN_POINT('Ctrl Pts',(-0.439018144460899,-0.264891372567355,
-1.19421827073972));
#65727=CARTESIAN_POINT('Ctrl Pts',(-0.258540186688332,-0.442788146062732,
-1.18030864079396));
#65728=CARTESIAN_POINT('Ctrl Pts',(-0.0149087112336633,-0.512525219629101,
-1.1663990108482));
#65729=CARTESIAN_POINT('Ctrl Pts',(0.232364509709674,-0.45706794358595,
-1.15248938090245));
#65730=CARTESIAN_POINT('Ctrl Pts',(0.422878136097861,-0.289962846649199,
-1.13857975095669));
#65731=CARTESIAN_POINT('Ctrl Pts',(0.51009547347383,-0.052028630272347,
-1.12467012101093));
#65732=CARTESIAN_POINT('Ctrl Pts',(0.472711974452847,0.198614600760868,
-1.11076049106517));
#65733=CARTESIAN_POINT('Ctrl Pts',(0.319859292789327,0.400742315263586,
-1.09685086111941));
#65734=CARTESIAN_POINT('Ctrl Pts',(0.0888746976244564,0.504980849685084,
-1.08294123117365));
#65735=CARTESIAN_POINT('Ctrl Pts',(-0.163819287712257,0.485867895008465,
-1.06903160122789));
#65736=CARTESIAN_POINT('Ctrl Pts',(-0.376497195023632,0.348072165744182,
-1.05512197128213));
#65737=CARTESIAN_POINT('Ctrl Pts',(-0.476853910979439,0.16282485140757,
-1.04355778967314));
#65738=CARTESIAN_POINT('Ctrl Pts',(-0.491784018023207,0.0404667799011544,
-1.03663015137941));
#65739=CARTESIAN_POINT('Ctrl Pts',(-0.49178273288147,4.49826145484944E-7,
-1.03433905640092));
#65740=CARTESIAN_POINT('Ctrl Pts',(-0.491783786383942,-3.02292213442967E-6,
-1.17481094359907));
#65741=CARTESIAN_POINT('Ctrl Pts',(-0.491791851348631,-0.0376946067152404,
-1.17267693421397));
#65742=CARTESIAN_POINT('Ctrl Pts',(-0.478220056409159,-0.157272646410343,
-1.16590638151361));
#65743=CARTESIAN_POINT('Ctrl Pts',(-0.382332390176345,-0.341652327267911,
-1.15449928549799));
#65744=CARTESIAN_POINT('Ctrl Pts',(-0.172016313369507,-0.483026663073893,
-1.14058965555223));
#65745=CARTESIAN_POINT('Ctrl Pts',(0.0803181259485588,-0.506412250986929,
-1.12668002560648));
#65746=CARTESIAN_POINT('Ctrl Pts',(0.313033285756316,-0.406096701924727,
-1.11277039566072));
#65747=CARTESIAN_POINT('Ctrl Pts',(0.469283918326265,-0.206584058692545,
-1.09886076571496));
#65748=CARTESIAN_POINT('Ctrl Pts',(0.510902738281055,0.0433907976701933,
-1.0849511357692));
#65749=CARTESIAN_POINT('Ctrl Pts',(0.427723531557066,0.282766599615103,
-1.07104150582344));
#65750=CARTESIAN_POINT('Ctrl Pts',(0.240064452828482,0.45307110677431,-1.05713187587768));
#65751=CARTESIAN_POINT('Ctrl Pts',(-0.0062350827696745,0.512704098919047,
-1.04322224593192));
#65752=CARTESIAN_POINT('Ctrl Pts',(-0.251011576959888,0.447099046674948,
-1.02931261598616));
#65753=CARTESIAN_POINT('Ctrl Pts',(-0.434473564237258,0.27228127237199,
-1.0154029860404));
#65754=CARTESIAN_POINT('Ctrl Pts',(-0.489146988657971,0.101666277091445,
-1.00556909524471));
#65755=CARTESIAN_POINT('Ctrl Pts',(-0.491860868978114,0.00991044711519981,
-1.00037174776426));
#65756=CARTESIAN_POINT('Ctrl Pts',(-0.491852307000294,9.30393982757037E-6,
-0.999810943599072));
#65757=CARTESIAN_POINT('Origin',(0.,0.,-4.27183905640093));
#65758=CARTESIAN_POINT('',(-0.491800974659427,1.08920470272003E-5,-1.38433905640092));
#65759=CARTESIAN_POINT('',(-0.491865353078785,-3.56841417972764E-6,-1.34981094359907));
#65760=CARTESIAN_POINT('',(-0.491825,-1.07154090996976E-14,-4.27183905640093));
#65761=CARTESIAN_POINT('Ctrl Pts',(-0.491800974659428,1.08920470272104E-5,
-1.38433905640092));
#65762=CARTESIAN_POINT('Ctrl Pts',(-0.491756812207049,-0.0547109370230884,
-1.38124052427881));
#65763=CARTESIAN_POINT('Ctrl Pts',(-0.469012650190695,-0.191352540086311,
-1.37350544884145));
#65764=CARTESIAN_POINT('Ctrl Pts',(-0.344840355124436,-0.379459483876949,
-1.36113383008883));
#65765=CARTESIAN_POINT('Ctrl Pts',(-0.120997217343892,-0.498261019769301,
-1.34722420014307));
#65766=CARTESIAN_POINT('Ctrl Pts',(0.132401866856018,-0.495352516981138,
-1.33331457019731));
#65767=CARTESIAN_POINT('Ctrl Pts',(0.353459195034396,-0.371444434434203,
-1.31940494025155));
#65768=CARTESIAN_POINT('Ctrl Pts',(0.488177173769909,-0.156803754535824,
-1.30549531030579));
#65769=CARTESIAN_POINT('Ctrl Pts',(0.503648291231812,0.0961393216419958,
-1.29158568036004));
#65770=CARTESIAN_POINT('Ctrl Pts',(0.396093423165933,0.325598480572622,
-1.27767605041428));
#65771=CARTESIAN_POINT('Ctrl Pts',(0.191784958206317,0.475523816682518,
-1.26376642046852));
#65772=CARTESIAN_POINT('Ctrl Pts',(-0.0593707489727289,0.509293122467725,
-1.24985679052276));
#65773=CARTESIAN_POINT('Ctrl Pts',(-0.296023984821974,0.418657581845388,
-1.235947160577));
#65774=CARTESIAN_POINT('Ctrl Pts',(-0.45559757693874,0.231355536394371,
-1.22244124920305));
#65775=CARTESIAN_POINT('Ctrl Pts',(-0.491806479610826,0.0747215573978147,
-1.21357188114436));
#65776=CARTESIAN_POINT('Ctrl Pts',(-0.49185900932756,-7.11307669150688E-6,
-1.20933905640092));
#65777=CARTESIAN_POINT('Ctrl Pts',(-0.491865353078785,-3.56841417971767E-6,
-1.34981094359907));
#65778=CARTESIAN_POINT('Ctrl Pts',(-0.491866674226144,-0.00339805385570091,
-1.34961866397892));
#65779=CARTESIAN_POINT('Ctrl Pts',(-0.491002663521623,-0.0886449429922445,
-1.34478984104352));
#65780=CARTESIAN_POINT('Ctrl Pts',(-0.444936530586125,-0.254825142118117,
-1.33532447479286));
#65781=CARTESIAN_POINT('Ctrl Pts',(-0.268556528523827,-0.436785714387234,
-1.3214148448471));
#65782=CARTESIAN_POINT('Ctrl Pts',(-0.0265763205901719,-0.512052798536855,
-1.30750521490134));
#65783=CARTESIAN_POINT('Ctrl Pts',(0.221895675540188,-0.462240931205903,
-1.29359558495558));
#65784=CARTESIAN_POINT('Ctrl Pts',(0.416165295443046,-0.299517639170616,
-1.27968595500983));
#65785=CARTESIAN_POINT('Ctrl Pts',(0.508778369487043,-0.063631281989616,
-1.26577632506407));
#65786=CARTESIAN_POINT('Ctrl Pts',(0.477112335647494,0.187798265376785,
-1.25186669511831));
#65787=CARTESIAN_POINT('Ctrl Pts',(0.328902244531517,0.393354398536063,
-1.23795706517255));
#65788=CARTESIAN_POINT('Ctrl Pts',(0.100351321370171,0.502825995355051,
-1.22404743522679));
#65789=CARTESIAN_POINT('Ctrl Pts',(-0.15271238268513,0.489472468561989,
-1.21013780528103));
#65790=CARTESIAN_POINT('Ctrl Pts',(-0.368473088379839,0.356555679305995,
-1.19622817533527));
#65791=CARTESIAN_POINT('Ctrl Pts',(-0.474933894869138,0.170297388134082,
-1.18445255477462));
#65792=CARTESIAN_POINT('Ctrl Pts',(-0.491774328671187,0.0441975640019624,
-1.17731347752922));
#65793=CARTESIAN_POINT('Ctrl Pts',(-0.491783786383942,-3.02292213442967E-6,
-1.17481094359907));
#65794=CARTESIAN_POINT('Origin',(0.,0.,-4.27183905640093));
#65795=CARTESIAN_POINT('',(-0.491820155779459,-1.28375648062008E-5,-1.55933905640092));
#65796=CARTESIAN_POINT('',(-0.491792696404785,8.61912597031889E-6,-1.52481094359907));
#65797=CARTESIAN_POINT('',(-0.491825,-1.07154090996976E-14,-4.27183905640093));
#65798=CARTESIAN_POINT('Ctrl Pts',(-0.491820155779459,-1.28375648062243E-5,
-1.55933905640092));
#65799=CARTESIAN_POINT('Ctrl Pts',(-0.491840834199996,-0.0204403340332267,
-1.55818225404377));
#65800=CARTESIAN_POINT('Ctrl Pts',(-0.485587427915056,-0.122730064592817,
-1.55238890837136));
#65801=CARTESIAN_POINT('Ctrl Pts',(-0.416111244906428,-0.299592727363217,
-1.5419590193837));
#65802=CARTESIAN_POINT('Ctrl Pts',(-0.221812266131596,-0.462280963289723,
-1.52804938943794));
#65803=CARTESIAN_POINT('Ctrl Pts',(0.0266687144847388,-0.512047995889291,
-1.51413975949218));
#65804=CARTESIAN_POINT('Ctrl Pts',(0.268635337881236,-0.436737250149265,
-1.50023012954642));
#65805=CARTESIAN_POINT('Ctrl Pts',(0.44498250467321,-0.254744854631581,
-1.48632049960066));
#65806=CARTESIAN_POINT('Ctrl Pts',(0.512633956353846,-0.0105260258174941,
-1.4724108696549));
#65807=CARTESIAN_POINT('Ctrl Pts',(0.455064497344623,0.23626399150737,-1.45850123970914));
#65808=CARTESIAN_POINT('Ctrl Pts',(0.286336598528917,0.425341889271909,
-1.44459160976338));
#65809=CARTESIAN_POINT('Ctrl Pts',(0.047665362586952,0.510521677929509,
-1.43068197981763));
#65810=CARTESIAN_POINT('Ctrl Pts',(-0.202649074195538,0.47099652138227,
-1.41677234987187));
#65811=CARTESIAN_POINT('Ctrl Pts',(-0.403462495084136,0.316421215292198,
-1.40286271992611));
#65812=CARTESIAN_POINT('Ctrl Pts',(-0.482942720425566,0.136204978692006,
-1.39205162210246));
#65813=CARTESIAN_POINT('Ctrl Pts',(-0.491822895473348,0.0271730392516382,
-1.38587706759407));
#65814=CARTESIAN_POINT('Ctrl Pts',(-0.491800974659428,1.08920470272104E-5,
-1.38433905640092));
#65815=CARTESIAN_POINT('Ctrl Pts',(-0.491792696404785,8.61912597030848E-6,
-1.52481094359907));
#65816=CARTESIAN_POINT('Ctrl Pts',(-0.49176087174051,-0.0509815371313851,
-1.52192385042862));
#65817=CARTESIAN_POINT('Ctrl Pts',(-0.471200171751201,-0.183884693624623,
-1.51440021394292));
#65818=CARTESIAN_POINT('Ctrl Pts',(-0.353392165482507,-0.371508205402143,
-1.50224003414197));
#65819=CARTESIAN_POINT('Ctrl Pts',(-0.132312483529502,-0.495376398315253,
-1.48833040419621));
#65820=CARTESIAN_POINT('Ctrl Pts',(0.121087120812267,-0.498239177984762,
-1.47442077425045));
#65821=CARTESIAN_POINT('Ctrl Pts',(0.344908818047041,-0.379397254258554,
-1.46051114430469));
#65822=CARTESIAN_POINT('Ctrl Pts',(0.484479763326162,-0.167880100765288,
-1.44660151435893));
#65823=CARTESIAN_POINT('Ctrl Pts',(0.505707012440461,0.0846450640857451,
-1.43269188441317));
#65824=CARTESIAN_POINT('Ctrl Pts',(0.40340539294362,0.316494009816205,-1.41878225446742));
#65825=CARTESIAN_POINT('Ctrl Pts',(0.202564084346017,0.47103307849725,-1.40487262452166));
#65826=CARTESIAN_POINT('Ctrl Pts',(-0.0477574797057481,0.510513067842236,
-1.3909629945759));
#65827=CARTESIAN_POINT('Ctrl Pts',(-0.28641334150177,0.425290215165276,
-1.37705336463014));
#65828=CARTESIAN_POINT('Ctrl Pts',(-0.452775183555581,0.238796012894704,
-1.36333601430453));
#65829=CARTESIAN_POINT('Ctrl Pts',(-0.49183481667956,0.0784550243347217,
-1.35425520729417));
#65830=CARTESIAN_POINT('Ctrl Pts',(-0.491865353078785,-3.56841417971767E-6,
-1.34981094359907));
#65831=CARTESIAN_POINT('Origin',(0.,0.,-4.27183905640093));
#65832=CARTESIAN_POINT('',(-0.491840877697987,1.15800763210497E-5,-1.73433905640093));
#65833=CARTESIAN_POINT('',(-0.491831982535426,-1.2519398762012E-5,-1.69981094359907));
#65834=CARTESIAN_POINT('',(-0.491825,-1.07154090996976E-14,-4.27183905640093));
#65835=CARTESIAN_POINT('Ctrl Pts',(-0.491840877697987,1.1580076321056E-5,
-1.73433905640093));
#65836=CARTESIAN_POINT('Ctrl Pts',(-0.491772846092899,-0.0679942662770046,
-1.73048744049347));
#65837=CARTESIAN_POINT('Ctrl Pts',(-0.46042730279502,-0.217925740442619,
-1.72199928127076));
#65838=CARTESIAN_POINT('Ctrl Pts',(-0.312960005664294,-0.406153179577745,
-1.70887457873281));
#65839=CARTESIAN_POINT('Ctrl Pts',(-0.0802267483162252,-0.506426736341114,
-1.69496494878705));
#65840=CARTESIAN_POINT('Ctrl Pts',(0.172103467761028,-0.482995617797032,
-1.68105531884129));
#65841=CARTESIAN_POINT('Ctrl Pts',(0.38239403215543,-0.341583334778529,
-1.66714568889553));
#65842=CARTESIAN_POINT('Ctrl Pts',(0.499277344932229,-0.116732614396888,
-1.65323605894977));
#65843=CARTESIAN_POINT('Ctrl Pts',(0.494202361649382,0.136632339388161,
-1.63932642900401));
#65844=CARTESIAN_POINT('Ctrl Pts',(0.36840874663372,0.35662216115979,-1.62541679905825));
#65845=CARTESIAN_POINT('Ctrl Pts',(0.152624060625208,0.489500016899674,
-1.61150716911249));
#65846=CARTESIAN_POINT('Ctrl Pts',(-0.100442049346334,0.502807880954164,
-1.59759753916673));
#65847=CARTESIAN_POINT('Ctrl Pts',(-0.328973216334069,0.393295046194743,
-1.58368790922097));
#65848=CARTESIAN_POINT('Ctrl Pts',(-0.464823322547969,0.20480959069708,
-1.57093508163237));
#65849=CARTESIAN_POINT('Ctrl Pts',(-0.491757953669959,0.0614344751008574,
-1.56281879735902));
#65850=CARTESIAN_POINT('Ctrl Pts',(-0.491820155779459,-1.28375648062243E-5,
-1.55933905640092));
#65851=CARTESIAN_POINT('Ctrl Pts',(-0.491831982535426,-1.25193987619981E-5,
-1.69981094359907));
#65852=CARTESIAN_POINT('Ctrl Pts',(-0.491849266882592,-0.016705147158428,
-1.69886558019358));
#65853=CARTESIAN_POINT('Ctrl Pts',(-0.486929935288758,-0.115256778052977,
-1.69328367347283));
#65854=CARTESIAN_POINT('Ctrl Pts',(-0.422825807720183,-0.290039144998243,
-1.68306522343684));
#65855=CARTESIAN_POINT('Ctrl Pts',(-0.232282032571033,-0.457109862779405,
-1.66915559349108));
#65856=CARTESIAN_POINT('Ctrl Pts',(0.0150011904725086,-0.51252252008077,
-1.65524596354532));
#65857=CARTESIAN_POINT('Ctrl Pts',(0.25862007815723,-0.442741487190307,
-1.64133633359956));
#65858=CARTESIAN_POINT('Ctrl Pts',(0.439065933099701,-0.264812151716694,
-1.6274267036538));
#65859=CARTESIAN_POINT('Ctrl Pts',(0.512261311724355,-0.0221972479370705,
-1.61351707370804));
#65860=CARTESIAN_POINT('Ctrl Pts',(0.46032680542771,0.225839769549687,-1.59960744376228));
#65861=CARTESIAN_POINT('Ctrl Pts',(0.295948437236704,0.418710988394965,
-1.58569781381652));
#65862=CARTESIAN_POINT('Ctrl Pts',(0.0592788515625552,0.509303825886828,
-1.57178818387076));
#65863=CARTESIAN_POINT('Ctrl Pts',(-0.191870757694326,0.475489202450847,
-1.55787855392501));
#65864=CARTESIAN_POINT('Ctrl Pts',(-0.396152166521947,0.325527003895996,
-1.54396892397925));
#65865=CARTESIAN_POINT('Ctrl Pts',(-0.481350054693306,0.143679183617523,
-1.53294638720394));
#65866=CARTESIAN_POINT('Ctrl Pts',(-0.491811980736892,0.0309063875669545,
-1.52656039374388));
#65867=CARTESIAN_POINT('Ctrl Pts',(-0.491792696404785,8.61912597030848E-6,
-1.52481094359907));
#65868=CARTESIAN_POINT('Origin',(0.,0.,-4.27183905640093));
#65869=CARTESIAN_POINT('',(-0.491787937416117,-6.46297745255268E-6,-1.90933905640093));
#65870=CARTESIAN_POINT('',(-0.491829112982424,1.26920333077193E-5,-1.87481094359907));
#65871=CARTESIAN_POINT('',(-0.491825,-1.07154090996976E-14,-4.27183905640093));
#65872=CARTESIAN_POINT('Ctrl Pts',(-0.491787937416117,-6.46297745255861E-6,
-1.90933905640093));
#65873=CARTESIAN_POINT('Ctrl Pts',(-0.491803529803698,-0.0337386931560804,
-1.90742917025843));
#65874=CARTESIAN_POINT('Ctrl Pts',(-0.480081042180642,-0.149350430953692,
-1.90088274080068));
#65875=CARTESIAN_POINT('Ctrl Pts',(-0.390467917193037,-0.332323902344444,
-1.88969976802767));
#65876=CARTESIAN_POINT('Ctrl Pts',(-0.183625665141514,-0.478733731345353,
-1.87579013808191));
#65877=CARTESIAN_POINT('Ctrl Pts',(0.0680707615702241,-0.508203445330468,
-1.86188050813615));
#65878=CARTESIAN_POINT('Ctrl Pts',(0.303139568028706,-0.413534487947351,
-1.8479708781904));
#65879=CARTESIAN_POINT('Ctrl Pts',(0.464160582092247,-0.217851611098688,
-1.83406124824463));
#65880=CARTESIAN_POINT('Ctrl Pts',(0.511801259025317,0.0310457998223131,
-1.82015161829888));
#65881=CARTESIAN_POINT('Ctrl Pts',(0.43442442794312,0.272359664474753,-1.80624198835312));
#65882=CARTESIAN_POINT('Ctrl Pts',(0.250930899325168,0.447144332615734,
-1.79233235840736));
#65883=CARTESIAN_POINT('Ctrl Pts',(0.00614257089095992,0.512705216717518,
-1.7784227284616));
#65884=CARTESIAN_POINT('Ctrl Pts',(-0.240146201108115,0.453027783386239,
-1.76451309851584));
#65885=CARTESIAN_POINT('Ctrl Pts',(-0.427774547614985,0.282689417628787,
-1.75060346857008));
#65886=CARTESIAN_POINT('Ctrl Pts',(-0.487889963149149,0.109586602519485,
-1.74054545453178));
#65887=CARTESIAN_POINT('Ctrl Pts',(-0.4918547419754,0.0138706080728537,
-1.73512398380873));
#65888=CARTESIAN_POINT('Ctrl Pts',(-0.491840877697987,1.1580076321056E-5,
-1.73433905640093));
#65889=CARTESIAN_POINT('Ctrl Pts',(-0.491829112982424,1.26920333077315E-5,
-1.87481094359907));
#65890=CARTESIAN_POINT('Ctrl Pts',(-0.491762475705567,-0.064264325262914,
-1.87117076664328));
#65891=CARTESIAN_POINT('Ctrl Pts',(-0.462964584526037,-0.210469807830858,
-1.86289404637224));
#65892=CARTESIAN_POINT('Ctrl Pts',(-0.322127965446493,-0.398920973606101,
-1.84998078278594));
#65893=CARTESIAN_POINT('Ctrl Pts',(-0.0917385411651713,-0.504468442393003,
-1.83607115284018));
#65894=CARTESIAN_POINT('Ctrl Pts',(0.161059823311547,-0.48678958762528,
-1.82216152289443));
#65895=CARTESIAN_POINT('Ctrl Pts',(0.37451616313179,-0.350202816748494,
-1.80825189294867));
#65896=CARTESIAN_POINT('Ctrl Pts',(0.496489575545123,-0.128072130772313,
-1.79434226300291));
#65897=CARTESIAN_POINT('Ctrl Pts',(0.497185659316439,0.125342688161754,
-1.78043263305715));
#65898=CARTESIAN_POINT('Ctrl Pts',(0.376434382315248,0.348140094094997,
-1.76652300311139));
#65899=CARTESIAN_POINT('Ctrl Pts',(0.163731615202558,0.485897445443685,
-1.75261337316563));
#65900=CARTESIAN_POINT('Ctrl Pts',(-0.088965814203307,0.504964803930609,
-1.73870374321987));
#65901=CARTESIAN_POINT('Ctrl Pts',(-0.319931596423644,0.40068459281005,
-1.72479411327411));
#65902=CARTESIAN_POINT('Ctrl Pts',(-0.462361700510878,0.212268719064823,
-1.71182984673385));
#65903=CARTESIAN_POINT('Ctrl Pts',(-0.491764495646635,0.0651639956531007,
-1.70350212350883));
#65904=CARTESIAN_POINT('Ctrl Pts',(-0.491831982535426,-1.25193987619981E-5,
-1.69981094359907));
#65905=CARTESIAN_POINT('Origin',(0.,0.,-4.27183905640093));
#65906=CARTESIAN_POINT('',(-0.491867427628364,6.00722023146672E-7,-2.08433905640092));
#65907=CARTESIAN_POINT('',(-0.491794496945441,-9.2326743954263E-6,-2.04981094359907));
#65908=CARTESIAN_POINT('',(-0.491825,-1.07154090996976E-14,-4.27183905640093));
#65909=CARTESIAN_POINT('Ctrl Pts',(-0.491867398827384,6.00314237376911E-7,
-2.08433905640092));
#65910=CARTESIAN_POINT('Ctrl Pts',(-0.491861574474256,-0.0812893295483687,
-2.07973435670813));
#65911=CARTESIAN_POINT('Ctrl Pts',(-0.45056433286084,-0.244437046519258,
-2.07049311370008));
#65912=CARTESIAN_POINT('Ctrl Pts',(-0.279021570577783,-0.430175933286389,
-2.05661532737678));
#65913=CARTESIAN_POINT('Ctrl Pts',(-0.0389286926494526,-0.511262092585704,
-2.04270569743102));
#65914=CARTESIAN_POINT('Ctrl Pts',(0.210673282920791,-0.467462445860503,
-2.02879606748526));
#65915=CARTESIAN_POINT('Ctrl Pts',(0.408814172040582,-0.309475916939077,
-2.0148864375395));
#65916=CARTESIAN_POINT('Ctrl Pts',(0.507094171550263,-0.0758938179712873,
-2.00097680759374));
#65917=CARTESIAN_POINT('Ctrl Pts',(0.481506461595899,0.176226836401005,
-1.98706717764799));
#65918=CARTESIAN_POINT('Ctrl Pts',(0.338301342812545,0.385300625327465,
-1.97315754770222));
#65919=CARTESIAN_POINT('Ctrl Pts',(0.112459477653878,0.500257170175825,
-1.95924791775647));
#65920=CARTESIAN_POINT('Ctrl Pts',(-0.140852823344986,0.493016077407475,
-1.94533828781071));
#65921=CARTESIAN_POINT('Ctrl Pts',(-0.359759056244216,0.365346126128058,
-1.93142865786495));
#65922=CARTESIAN_POINT('Ctrl Pts',(-0.472796042913746,0.178216817683005,
-1.91942891406169));
#65923=CARTESIAN_POINT('Ctrl Pts',(-0.491765676876868,0.0481515006429693,
-1.91206571357368));
#65924=CARTESIAN_POINT('Ctrl Pts',(-0.491787937416117,-6.46297745255861E-6,
-1.90933905640093));
#65925=CARTESIAN_POINT('Ctrl Pts',(-0.491794496945441,-9.23267439544018E-6,
-2.04981094359907));
#65926=CARTESIAN_POINT('Ctrl Pts',(-0.491814648737398,-0.0300059021629562,
-2.04811249640824));
#65927=CARTESIAN_POINT('Ctrl Pts',(-0.481742510538666,-0.141876266339579,
-2.04177750590215));
#65928=CARTESIAN_POINT('Ctrl Pts',(-0.397934500429466,-0.32334579427215,
-2.03080597208081));
#65929=CARTESIAN_POINT('Ctrl Pts',(-0.194480004972519,-0.474427968158946,
-2.01689634213505));
#65930=CARTESIAN_POINT('Ctrl Pts',(0.0564800508004891,-0.509621794242663,
-2.00298671218929));
#65931=CARTESIAN_POINT('Ctrl Pts',(0.293643745038357,-0.420330489383515,
-1.98907708224353));
#65932=CARTESIAN_POINT('Ctrl Pts',(0.459079188120922,-0.228365208251544,
-1.97516745229777));
#65933=CARTESIAN_POINT('Ctrl Pts',(0.512375524336397,0.0193827595181383,
-1.96125782235201));
#65934=CARTESIAN_POINT('Ctrl Pts',(0.440514076957236,0.262396107646534,
-1.94734819240626));
#65935=CARTESIAN_POINT('Ctrl Pts',(0.261048415685123,0.441314053678131,
-1.9334385624605));
#65936=CARTESIAN_POINT('Ctrl Pts',(0.0178165525430863,0.512432375793154,
-1.91952893251474));
#65937=CARTESIAN_POINT('Ctrl Pts',(-0.229767353430185,0.458379027228804,
-1.90561930256898));
#65938=CARTESIAN_POINT('Ctrl Pts',(-0.421226071271232,0.292357599844676,
-1.89170967262322));
#65939=CARTESIAN_POINT('Ctrl Pts',(-0.486614162270651,0.117059418554486,
-1.88144021963325));
#65940=CARTESIAN_POINT('Ctrl Pts',(-0.49184735251906,0.0176061932554664,
-1.87580730995854));
#65941=CARTESIAN_POINT('Ctrl Pts',(-0.491829112982424,1.26920333077315E-5,
-1.87481094359907));
#65942=CARTESIAN_POINT('Origin',(0.,0.,-4.27183905640093));
#65943=CARTESIAN_POINT('',(-0.491786451319463,5.52690589573186E-6,-2.25933905640092));
#65944=CARTESIAN_POINT('',(-0.491864161604618,4.47272762704037E-6,-2.22481094359907));
#65945=CARTESIAN_POINT('',(-0.491825,-1.07154090996976E-14,-4.27183905640093));
#65946=CARTESIAN_POINT('Ctrl Pts',(-0.491786451319463,5.52690589572871E-6,
-2.25933905640092));
#65947=CARTESIAN_POINT('Ctrl Pts',(-0.491767929113347,-0.0470280052530091,
-2.25667608647308));
#65948=CARTESIAN_POINT('Ctrl Pts',(-0.473414348620751,-0.175966592201857,
-2.24937657322999));
#65949=CARTESIAN_POINT('Ctrl Pts',(-0.362256796811613,-0.362869650963398,
-2.23744051667165));
#65950=CARTESIAN_POINT('Ctrl Pts',(-0.144231506204031,-0.492038253639516,
-2.22353088672589));
#65951=CARTESIAN_POINT('Ctrl Pts',(0.1090251621404,-0.501016850461905,-2.20962125678013));
#65952=CARTESIAN_POINT('Ctrl Pts',(0.33565029365018,-0.387612242839485,
-2.19571162683437));
#65953=CARTESIAN_POINT('Ctrl Pts',(0.480286249602533,-0.179525733167259,
-2.18180199688861));
#65954=CARTESIAN_POINT('Ctrl Pts',(0.507602857467195,0.0724134622680479,
-2.16789236694285));
#65955=CARTESIAN_POINT('Ctrl Pts',(0.410927499343277,0.306664247524861,
-2.15398273699709));
#65956=CARTESIAN_POINT('Ctrl Pts',(0.213875029915099,0.466006268203898,
-2.14007310705133));
#65957=CARTESIAN_POINT('Ctrl Pts',(-0.0354206155412066,0.511517106675026,
-2.12616347710558));
#65958=CARTESIAN_POINT('Ctrl Pts',(-0.276064080079156,0.432079846922483,
-2.11225384715981));
#65959=CARTESIAN_POINT('Ctrl Pts',(-0.449273471848797,0.247098599590194,
-2.09834421721406));
#65960=CARTESIAN_POINT('Ctrl Pts',(-0.491729113979008,0.0829769823530704,
-2.08903928696109));
#65961=CARTESIAN_POINT('Ctrl Pts',(-0.491867439105472,0.000562757677112689,
-2.08437090002338));
#65962=CARTESIAN_POINT('Ctrl Pts',(-0.491867398827384,6.00314237376911E-7,
-2.08433905640092));
#65963=CARTESIAN_POINT('Ctrl Pts',(-0.491864161604618,4.47272762705338E-6,
-2.22481094359907));
#65964=CARTESIAN_POINT('Ctrl Pts',(-0.491827285582898,-0.0775542653706536,
-2.22041768285794));
#65965=CARTESIAN_POINT('Ctrl Pts',(-0.453465461486664,-0.237001846569603,
-2.21138787880155));
#65966=CARTESIAN_POINT('Ctrl Pts',(-0.288745389504487,-0.423710360205458,
-2.19772153142992));
#65967=CARTESIAN_POINT('Ctrl Pts',(-0.0505613083818057,-0.510243004263906,
-2.18381190148416));
#65968=CARTESIAN_POINT('Ctrl Pts',(0.199973365210935,-0.472138774632788,
-2.1699022715384));
#65969=CARTESIAN_POINT('Ctrl Pts',(0.401660617373509,-0.318705377671398,
-2.15599264159264));
#65970=CARTESIAN_POINT('Ctrl Pts',(0.505234376131355,-0.0874219336362221,
-2.14208301164688));
#65971=CARTESIAN_POINT('Ctrl Pts',(0.485394716977961,0.165216034438012,
-2.12817338170112));
#65972=CARTESIAN_POINT('Ctrl Pts',(0.346987866262887,0.377496741670528,
-2.11426375175536));
#65973=CARTESIAN_POINT('Ctrl Pts',(0.123822415238128,0.49756645665693,-2.10035412180961));
#65974=CARTESIAN_POINT('Ctrl Pts',(-0.129589092271495,0.496095793642505,
-2.08644449186384));
#65975=CARTESIAN_POINT('Ctrl Pts',(-0.351345919187724,0.37344399094867,
-2.07253486191809));
#65976=CARTESIAN_POINT('Ctrl Pts',(-0.470681307409857,0.185686283826414,
-2.06032367916316));
#65977=CARTESIAN_POINT('Ctrl Pts',(-0.491759636926143,0.0518811639451681,
-2.05274903972349));
#65978=CARTESIAN_POINT('Ctrl Pts',(-0.491794496945441,-9.23267439544018E-6,
-2.04981094359907));
#65979=CARTESIAN_POINT('Origin',(0.,0.,-4.27183905640093));
#65980=CARTESIAN_POINT('',(-0.49184428547454,-1.10437734740307E-5,-2.43433905640093));
#65981=CARTESIAN_POINT('',(-0.491783273045562,2.19569279796827E-6,-2.39981094359907));
#65982=CARTESIAN_POINT('',(-0.491825,-1.07154090996976E-14,-4.27183905640093));
#65983=CARTESIAN_POINT('Ctrl Pts',(-0.49184428547454,-1.1043773474018E-5,
-2.43433905640093));
#65984=CARTESIAN_POINT('Ctrl Pts',(-0.491856670524148,-0.0127453266690652,
-2.43361781623804));
#65985=CARTESIAN_POINT('Ctrl Pts',(-0.488257104721263,-0.1073358620036,
-2.4282600327599));
#65986=CARTESIAN_POINT('Ctrl Pts',(-0.429703678489127,-0.279748313881283,
-2.41826570596651));
#65987=CARTESIAN_POINT('Ctrl Pts',(-0.243248235588849,-0.451369766720613,
-2.40435607602075));
#65988=CARTESIAN_POINT('Ctrl Pts',(0.00262536564176082,-0.512735290263655,
-2.39044644607499));
#65989=CARTESIAN_POINT('Ctrl Pts',(0.247857669758745,-0.448855150319423,
-2.37653681612923));
#65990=CARTESIAN_POINT('Ctrl Pts',(0.432545870731629,-0.275333325515683,
-2.36262718618348));
#65991=CARTESIAN_POINT('Ctrl Pts',(0.511576248657834,-0.0345559290959576,
-2.34871755623772));
#65992=CARTESIAN_POINT('Ctrl Pts',(0.46564408176967,0.214662431597587,-2.33480792629196));
#65993=CARTESIAN_POINT('Ctrl Pts',(0.305969203822596,0.411445277939455,
-2.3208982963462));
#65994=CARTESIAN_POINT('Ctrl Pts',(0.0715553393709438,0.507724535387071,
-2.30698866640044));
#65995=CARTESIAN_POINT('Ctrl Pts',(-0.180337321890193,0.479982104624726,
-2.29307903645468));
#65996=CARTESIAN_POINT('Ctrl Pts',(-0.388179050905097,0.334994619158167,
-2.27916940650892));
#65997=CARTESIAN_POINT('Ctrl Pts',(-0.479562715419935,0.151601669956443,
-2.267922746491));
#65998=CARTESIAN_POINT('Ctrl Pts',(-0.491800178448968,0.0348628966472575,
-2.26131262978834));
#65999=CARTESIAN_POINT('Ctrl Pts',(-0.491786451319463,5.52690589572871E-6,
-2.25933905640092));
#66000=CARTESIAN_POINT('Ctrl Pts',(-0.491783273045562,2.19569279793705E-6,
-2.39981094359907));
#66001=CARTESIAN_POINT('Ctrl Pts',(-0.491776551894691,-0.0432976893620342,
-2.3973594126229));
#66002=CARTESIAN_POINT('Ctrl Pts',(-0.475405604406094,-0.168494975390873,
-2.39027133833147));
#66003=CARTESIAN_POINT('Ctrl Pts',(-0.370426298772862,-0.354526058961786,
-2.37854672072478));
#66004=CARTESIAN_POINT('Ctrl Pts',(-0.155399039185073,-0.488626143309885,
-2.36463709077902));
#66005=CARTESIAN_POINT('Ctrl Pts',(0.0975874873726366,-0.503369696757594,
-2.35072746083327));
#66006=CARTESIAN_POINT('Ctrl Pts',(0.326736353765087,-0.395155316848746,
-2.3368178308875));
#66007=CARTESIAN_POINT('Ctrl Pts',(0.476073449464557,-0.190416490936197,
-2.32290820094175));
#66008=CARTESIAN_POINT('Ctrl Pts',(0.509120256238909,0.060835302191775,
-2.30899857099599));
#66009=CARTESIAN_POINT('Ctrl Pts',(0.417804442576766,0.297226878106026,
-2.29508894105023));
#66010=CARTESIAN_POINT('Ctrl Pts',(0.224431689179598,0.461014952249414,
-2.28117931110447));
#66011=CARTESIAN_POINT('Ctrl Pts',(-0.0237629115774706,0.512191071123753,
-2.26726968115871));
#66012=CARTESIAN_POINT('Ctrl Pts',(-0.266152954537513,0.438254462722844,
-2.25336005121295));
#66013=CARTESIAN_POINT('Ctrl Pts',(-0.443529911772546,0.257265595578916,
-2.23945042126719));
#66014=CARTESIAN_POINT('Ctrl Pts',(-0.49076141250102,0.0904469082399701,
-2.22993405206257));
#66015=CARTESIAN_POINT('Ctrl Pts',(-0.491866203662674,0.00429938954725858,
-2.22505422617319));
#66016=CARTESIAN_POINT('Ctrl Pts',(-0.491864161604618,4.47272762705338E-6,
-2.22481094359907));
#66017=CARTESIAN_POINT('Origin',(0.,0.,-4.27183905640093));
#66018=CARTESIAN_POINT('',(-0.49181668614067,1.27304208609013E-5,-2.60933905640093));
#66019=CARTESIAN_POINT('',(-0.491854631260498,-8.64168429531853E-6,-2.57481094359907));
#66020=CARTESIAN_POINT('',(-0.491825,-1.07154090996976E-14,-4.27183905640093));
#66021=CARTESIAN_POINT('Ctrl Pts',(-0.49181668614067,1.27304208609111E-5,
-2.60933905640093));
#66022=CARTESIAN_POINT('Ctrl Pts',(-0.491756878388132,-0.0603111785225525,
-2.60592300268774));
#66023=CARTESIAN_POINT('Ctrl Pts',(-0.46554538245605,-0.202562094355018,
-2.59787040565931));
#66024=CARTESIAN_POINT('Ctrl Pts',(-0.331663405555064,-0.391029098459597,
-2.58518126531562));
#66025=CARTESIAN_POINT('Ctrl Pts',(-0.103888852940067,-0.502107037056149,
-2.57127163536986));
#66026=CARTESIAN_POINT('Ctrl Pts',(0.149262592123117,-0.490535471723703,
-2.5573620054241));
#66027=CARTESIAN_POINT('Ctrl Pts',(0.365953717915752,-0.359140984531349,
-2.54345237547834));
#66028=CARTESIAN_POINT('Ctrl Pts',(0.49325346169053,-0.140019259235349,
-2.52954274553259));
#66029=CARTESIAN_POINT('Ctrl Pts',(0.500066361181473,0.113304919757393,
-2.51563311558682));
#66030=CARTESIAN_POINT('Ctrl Pts',(0.384728231899584,0.338952147073784,
-2.50172348564107));
#66031=CARTESIAN_POINT('Ctrl Pts',(0.175412676874732,0.481803656293877,
-2.48781385569531));
#66032=CARTESIAN_POINT('Ctrl Pts',(-0.0767508691435963,0.506965161043843,
-2.47390422574955));
#66033=CARTESIAN_POINT('Ctrl Pts',(-0.310166508178242,0.4082904696794,-2.45999459580379));
#66034=CARTESIAN_POINT('Ctrl Pts',(-0.459643369733334,0.220170619003029,
-2.44680620602092));
#66035=CARTESIAN_POINT('Ctrl Pts',(-0.491777052358209,0.0691179101173199,
-2.43825435955329));
#66036=CARTESIAN_POINT('Ctrl Pts',(-0.49184428547454,-1.1043773474018E-5,
-2.43433905640093));
#66037=CARTESIAN_POINT('Ctrl Pts',(-0.491854631260498,-8.64168429529598E-6,
-2.57481094359907));
#66038=CARTESIAN_POINT('Ctrl Pts',(-0.491861998545963,-0.00900919132475913,
-2.57430114238785));
#66039=CARTESIAN_POINT('Ctrl Pts',(-0.489419424958644,-0.0998640001557114,
-2.56915479786138));
#66040=CARTESIAN_POINT('Ctrl Pts',(-0.435962809677364,-0.269890344183994,
-2.55937191001965));
#66041=CARTESIAN_POINT('Ctrl Pts',(-0.253463967943028,-0.445713345391533,
-2.54546228007389));
#66042=CARTESIAN_POINT('Ctrl Pts',(-0.00905157463938524,-0.512662109290402,
-2.53155265012813));
#66043=CARTESIAN_POINT('Ctrl Pts',(0.237571843520245,-0.454383085591805,
-2.51764302018238));
#66044=CARTESIAN_POINT('Ctrl Pts',(0.426163673582462,-0.285112070288575,
-2.50373339023661));
#66045=CARTESIAN_POINT('Ctrl Pts',(0.510656657582095,-0.0461968329284603,
-2.48982376029085));
#66046=CARTESIAN_POINT('Ctrl Pts',(0.470411724946076,0.204002888064838,
-2.4759141303451));
#66047=CARTESIAN_POINT('Ctrl Pts',(0.315259490780706,0.404370897541139,
-2.46200450039934));
#66048=CARTESIAN_POINT('Ctrl Pts',(0.083098935083214,0.505963374458638,
-2.44809487045358));
#66049=CARTESIAN_POINT('Ctrl Pts',(-0.169360167363873,0.48396436130775,
-2.43418524050782));
#66050=CARTESIAN_POINT('Ctrl Pts',(-0.380449723121679,0.343747549056243,
-2.42027561056206));
#66051=CARTESIAN_POINT('Ctrl Pts',(-0.477782100252891,0.159075394567747,
-2.40881751159248));
#66052=CARTESIAN_POINT('Ctrl Pts',(-0.491789263505291,0.0385947258483526,
-2.40199595593815));
#66053=CARTESIAN_POINT('Ctrl Pts',(-0.491783273045562,2.19569279793705E-6,
-2.39981094359907));
#66054=CARTESIAN_POINT('Origin',(0.,0.,-4.27183905640093));
#66055=CARTESIAN_POINT('',(-0.491803854275335,-1.14244199510044E-5,-2.78433905640093));
#66056=CARTESIAN_POINT('',(-0.491805856046874,1.17355489448745E-5,-2.74981094359907));
#66057=CARTESIAN_POINT('',(-0.491825,-1.07154090996976E-14,-4.27183905640093));
#66058=CARTESIAN_POINT('Ctrl Pts',(-0.491803854275335,-1.14244199509762E-5,
-2.78433905640093));
#66059=CARTESIAN_POINT('Ctrl Pts',(-0.491826081341972,-0.02604838175069,
-2.7828647324527));
#66060=CARTESIAN_POINT('Ctrl Pts',(-0.483404780242388,-0.133953703491761,
-2.77675386518922));
#66061=CARTESIAN_POINT('Ctrl Pts',(-0.405623591737084,-0.313646093954341,
-2.76600645461048));
#66062=CARTESIAN_POINT('Ctrl Pts',(-0.205875253078692,-0.469595305125906,
-2.75209682466473));
#66063=CARTESIAN_POINT('Ctrl Pts',(0.0441621590199009,-0.510836641341642,
-2.73818719471897));
#66064=CARTESIAN_POINT('Ctrl Pts',(0.283412096543389,-0.427296096354025,
-2.72427756477321));
#66065=CARTESIAN_POINT('Ctrl Pts',(0.453433063980492,-0.239380088803917,
-2.71036793482745));
#66066=CARTESIAN_POINT('Ctrl Pts',(0.512694101247579,0.00700920626356338,
-2.69645830488169));
#66067=CARTESIAN_POINT('Ctrl Pts',(0.446719536253416,0.251686365057864,
-2.68254867493593));
#66068=CARTESIAN_POINT('Ctrl Pts',(0.271624952073492,0.434884186695241,
-2.66863904499017));
#66069=CARTESIAN_POINT('Ctrl Pts',(0.0301806393140316,0.511853005693142,
-2.65472941504441));
#66070=CARTESIAN_POINT('Ctrl Pts',(-0.218635887270253,0.463791676535983,
-2.64081978509866));
#66071=CARTESIAN_POINT('Ctrl Pts',(-0.414046304926066,0.302440122674851,
-2.6269101551529));
#66072=CARTESIAN_POINT('Ctrl Pts',(-0.485165733168298,0.124981187180373,
-2.61641657892032));
#66073=CARTESIAN_POINT('Ctrl Pts',(-0.491838054288311,0.0215652907150948,
-2.610559546003));
#66074=CARTESIAN_POINT('Ctrl Pts',(-0.49181668614067,1.27304208609111E-5,
-2.60933905640093));
#66075=CARTESIAN_POINT('Ctrl Pts',(-0.491805856046874,1.1735548944871E-5,
-2.74981094359907));
#66076=CARTESIAN_POINT('Ctrl Pts',(-0.491755926810843,-0.05658196160197,
-2.74660632883756));
#66077=CARTESIAN_POINT('Ctrl Pts',(-0.467878716857623,-0.195098347367542,
-2.73876517076078));
#66078=CARTESIAN_POINT('Ctrl Pts',(-0.340482102013575,-0.383374891606055,
-2.72628746936876));
#66079=CARTESIAN_POINT('Ctrl Pts',(-0.115296139210803,-0.499611018281843,
-2.712377839423));
#66080=CARTESIAN_POINT('Ctrl Pts',(0.138053169722395,-0.493807342629832,
-2.69846820947724));
#66081=CARTESIAN_POINT('Ctrl Pts',(0.357680280931475,-0.367381526397719,
-2.68455857953148));
#66082=CARTESIAN_POINT('Ctrl Pts',(0.489936959575747,-0.151215557887439,
-2.67064894958572));
#66083=CARTESIAN_POINT('Ctrl Pts',(0.502516914705533,0.101887780132694,
-2.65673931963996));
#66084=CARTESIAN_POINT('Ctrl Pts',(0.392347245241488,0.330103027033912,
-2.64282968969421));
#66085=CARTESIAN_POINT('Ctrl Pts',(0.186339056407328,0.477684127183188,
-2.62892005974845));
#66086=CARTESIAN_POINT('Ctrl Pts',(-0.0651861061879488,0.508581498744882,
-2.61501042980269));
#66087=CARTESIAN_POINT('Ctrl Pts',(-0.300788282254515,0.415247851967851,
-2.60110079985693));
#66088=CARTESIAN_POINT('Ctrl Pts',(-0.456974840927703,0.227620125942558,
-2.58770097112239));
#66089=CARTESIAN_POINT('Ctrl Pts',(-0.491794994511007,0.0728490650907621,
-2.57893768570311));
#66090=CARTESIAN_POINT('Ctrl Pts',(-0.491854631260498,-8.64168429529598E-6,
-2.57481094359907));
#66091=CARTESIAN_POINT('Origin',(0.,0.,-4.27183905640093));
#66092=CARTESIAN_POINT('',(-0.491856460957234,8.05430276504716E-6,-2.95933905640093));
#66093=CARTESIAN_POINT('',(-0.491814419211658,-1.26084172522301E-5,-2.92481094359907));
#66094=CARTESIAN_POINT('',(-0.491825,-1.07154090996976E-14,-4.27183905640093));
#66095=CARTESIAN_POINT('Ctrl Pts',(-0.491856460957234,8.0543027650452E-6,
-2.95933905640093));
#66096=CARTESIAN_POINT('Ctrl Pts',(-0.491799376571172,-0.0735973513096081,
-2.9551699189024));
#66097=CARTESIAN_POINT('Ctrl Pts',(-0.456427518232039,-0.229113145239056,
-2.94636423808863));
#66098=CARTESIAN_POINT('Ctrl Pts',(-0.29888893149109,-0.416617062851034,
-2.93292201395959));
#66099=CARTESIAN_POINT('Ctrl Pts',(-0.0628630064529875,-0.5088738673249,
-2.91901238401384));
#66100=CARTESIAN_POINT('Ctrl Pts',(0.188518442383684,-0.476828236692982,
-2.90510275406808));
#66101=CARTESIAN_POINT('Ctrl Pts',(0.393850559636817,-0.328307945533265,
-2.89119312412232));
#66102=CARTESIAN_POINT('Ctrl Pts',(0.502976943457436,-0.0995919915290553,
-2.87728349417656));
#66103=CARTESIAN_POINT('Ctrl Pts',(0.489241331627754,0.153451262144076,
-2.8633738642308));
#66104=CARTESIAN_POINT('Ctrl Pts',(0.35599891707028,0.369011031639022,-2.84946423428504));
#66105=CARTESIAN_POINT('Ctrl Pts',(0.135796776088882,0.494432610201203,
-2.83555460433928));
#66106=CARTESIAN_POINT('Ctrl Pts',(-0.117576394161712,0.499079314300279,
-2.82164497439352));
#66107=CARTESIAN_POINT('Ctrl Pts',(-0.342229221231611,0.381816095210394,
-2.80773534444777));
#66108=CARTESIAN_POINT('Ctrl Pts',(-0.468334820753547,0.193601437055532,
-2.79530003845023));
#66109=CARTESIAN_POINT('Ctrl Pts',(-0.491756180315567,0.0558342198353221,
-2.78750127576795));
#66110=CARTESIAN_POINT('Ctrl Pts',(-0.491803854275335,-1.14244199509762E-5,
-2.78433905640093));
#66111=CARTESIAN_POINT('Ctrl Pts',(-0.491814419211658,-1.26084172522266E-5,
-2.92481094359907));
#66112=CARTESIAN_POINT('Ctrl Pts',(-0.491836147905159,-0.0223141218257271,
-2.92354805860251));
#66113=CARTESIAN_POINT('Ctrl Pts',(-0.48488055383623,-0.126479739420017,
-2.91764863029069));
#66114=CARTESIAN_POINT('Ctrl Pts',(-0.412660904457599,-0.304327697125603,
-2.90711265866362));
#66115=CARTESIAN_POINT('Ctrl Pts',(-0.216515718225303,-0.464785233271151,
-2.89320302871787));
#66116=CARTESIAN_POINT('Ctrl Pts',(0.0325176840114124,-0.511709848969189,
-2.87929339877211));
#66117=CARTESIAN_POINT('Ctrl Pts',(0.273608003362249,-0.43363928535323,
-2.86538376882635));
#66118=CARTESIAN_POINT('Ctrl Pts',(0.447864194914093,-0.249643810697336,
-2.85147413888059));
#66119=CARTESIAN_POINT('Ctrl Pts',(0.51272076192407,-0.00466793289774274,
-2.83756450893483));
#66120=CARTESIAN_POINT('Ctrl Pts',(0.452335214279015,0.241448179178668,
-2.82365487898907));
#66121=CARTESIAN_POINT('Ctrl Pts',(0.281457907812556,0.428585832051545,
-2.80974524904331));
#66122=CARTESIAN_POINT('Ctrl Pts',(0.0418289802326045,0.511032979090623,
-2.79583561909755));
#66123=CARTESIAN_POINT('Ctrl Pts',(-0.208017497185851,0.468650285575578,
-2.78192598915179));
#66124=CARTESIAN_POINT('Ctrl Pts',(-0.40705161597261,0.311790556687697,
-2.76801635920603));
#66125=CARTESIAN_POINT('Ctrl Pts',(-0.483707850118771,0.13245508266619,
-2.7573113440218));
#66126=CARTESIAN_POINT('Ctrl Pts',(-0.491828166091625,0.0252996833812049,
-2.75124287215281));
#66127=CARTESIAN_POINT('Ctrl Pts',(-0.491805856046874,1.1735548944871E-5,
-2.74981094359907));
#66128=CARTESIAN_POINT('Origin',(0.,0.,-4.27183905640093));
#66129=CARTESIAN_POINT('',(-0.491782972158755,-1.50095741644205E-6,-3.13433905640093));
#66130=CARTESIAN_POINT('',(-0.491846492690184,1.06369834088973E-5,-3.09981094359907));
#66131=CARTESIAN_POINT('',(-0.491825,-1.07154090996976E-14,-4.27183905640093));
#66132=CARTESIAN_POINT('Ctrl Pts',(-0.491782972158755,-1.50095741644624E-6,
-3.13433905640093));
#66133=CARTESIAN_POINT('Ctrl Pts',(-0.491787143576006,-0.0393429040773888,
-3.13211164866736));
#66134=CARTESIAN_POINT('Ctrl Pts',(-0.477413957249408,-0.160573869922756,
-3.12524769761854));
#66135=CARTESIAN_POINT('Ctrl Pts',(-0.378876045665121,-0.345481276551521,
-3.11374720325446));
#66136=CARTESIAN_POINT('Ctrl Pts',(-0.167148395020481,-0.484732693830926,
-3.0998375733087));
#66137=CARTESIAN_POINT('Ctrl Pts',(0.0854085334848828,-0.505578631702793,
-3.08592794336294));
#66138=CARTESIAN_POINT('Ctrl Pts',(0.317102750476299,-0.402927060479777,
-3.07201831341718));
#66139=CARTESIAN_POINT('Ctrl Pts',(0.47133839355793,-0.201852642253547,
-3.05810868347143));
#66140=CARTESIAN_POINT('Ctrl Pts',(0.510440378104306,0.0485282477248127,
-3.04419905352566));
#66141=CARTESIAN_POINT('Ctrl Pts',(0.424857276524671,0.287055160222818,
-3.03028942357991));
#66142=CARTESIAN_POINT('Ctrl Pts',(0.235494442018191,0.455463212790065,
-3.01637979363415));
#66143=CARTESIAN_POINT('Ctrl Pts',(-0.0113925344738468,0.512615431473507,
-3.00247016368839));
#66144=CARTESIAN_POINT('Ctrl Pts',(-0.255496660699727,0.444551264532895,
-2.98856053374263));
#66145=CARTESIAN_POINT('Ctrl Pts',(-0.437190710233471,0.267896721353699,
-2.97465090379687));
#66146=CARTESIAN_POINT('Ctrl Pts',(-0.489642054774299,0.0983659229714609,
-2.96491041134964));
#66147=CARTESIAN_POINT('Ctrl Pts',(-0.491862860739947,0.00826002362209832,
-2.95980646221765));
#66148=CARTESIAN_POINT('Ctrl Pts',(-0.491856460957234,8.0543027650452E-6,
-2.95933905640093));
#66149=CARTESIAN_POINT('Ctrl Pts',(-0.491846492690184,1.06369834089078E-5,
-3.09981094359907));
#66150=CARTESIAN_POINT('Ctrl Pts',(-0.4917801485058,-0.0698659474040416,
-3.09585324505221));
#66151=CARTESIAN_POINT('Ctrl Pts',(-0.459116439411713,-0.221664739361114,
-3.0872590031901));
#66152=CARTESIAN_POINT('Ctrl Pts',(-0.308298828990521,-0.409702576692666,
-3.07402821801273));
#66153=CARTESIAN_POINT('Ctrl Pts',(-0.0744350294889845,-0.507310354408927,
-3.06011858806697));
#66154=CARTESIAN_POINT('Ctrl Pts',(0.177610987683289,-0.480997615752618,
-3.04620895812121));
#66155=CARTESIAN_POINT('Ctrl Pts',(0.386272033277762,-0.337191763857008,
-3.03229932817546));
#66156=CARTESIAN_POINT('Ctrl Pts',(0.500578549326249,-0.111020202035327,
-3.0183896982297));
#66157=CARTESIAN_POINT('Ctrl Pts',(0.492608924589448,0.142270224292942,
-3.00448006828394));
#66158=CARTESIAN_POINT('Ctrl Pts',(0.364309896412847,0.360808354505819,
-2.99057043833818));
#66159=CARTESIAN_POINT('Ctrl Pts',(0.147021021901026,0.491211958755805,
-2.97666080839242));
#66160=CARTESIAN_POINT('Ctrl Pts',(-0.10618062433576,0.501627395903777,
-2.96275117844666));
#66161=CARTESIAN_POINT('Ctrl Pts',(-0.333445567956295,0.389510490893173,
-2.9488415485009));
#66162=CARTESIAN_POINT('Ctrl Pts',(-0.46602109057202,0.201065803521883,
-2.93619480355171));
#66163=CARTESIAN_POINT('Ctrl Pts',(-0.491756373397683,0.0595634309169782,
-2.92818460191776));
#66164=CARTESIAN_POINT('Ctrl Pts',(-0.491814419211658,-1.26084172522266E-5,
-2.92481094359907));
#66165=CARTESIAN_POINT('Origin',(0.,0.,-4.27183905640093));
#66166=CARTESIAN_POINT('',(-0.491862997454019,-5.20327585691352E-6,-3.30933905640093));
#66167=CARTESIAN_POINT('',(-0.491785594053212,-4.88331669762365E-6,-3.27481094359907));
#66168=CARTESIAN_POINT('',(-0.491825,-1.07154090996976E-14,-4.27183905640093));
#66169=CARTESIAN_POINT('Ctrl Pts',(-0.491862997454019,-5.20327585694629E-6,
-3.30933905640093));
#66170=CARTESIAN_POINT('Ctrl Pts',(-0.491865730726733,-0.00504860421699772,
-3.30905337843231));
#66171=CARTESIAN_POINT('Ctrl Pts',(-0.490557081626144,-0.0919448026840877,
-3.30413115714845));
#66172=CARTESIAN_POINT('Ctrl Pts',(-0.442350493670444,-0.259288278130775,
-3.29457239254933));
#66173=CARTESIAN_POINT('Ctrl Pts',(-0.264148905910468,-0.439465272726765,
-3.28066276260357));
#66174=CARTESIAN_POINT('Ctrl Pts',(-0.0214237606571462,-0.512294244458996,
-3.26675313265781));
#66175=CARTESIAN_POINT('Ctrl Pts',(0.226534558845831,-0.459985286802776,
-3.25284350271205));
#66176=CARTESIAN_POINT('Ctrl Pts',(0.419157363777824,-0.295315889882908,
-3.2389338727663));
#66177=CARTESIAN_POINT('Ctrl Pts',(0.509392751403437,-0.0585097875927088,
-3.22502424282053));
#66178=CARTESIAN_POINT('Ctrl Pts',(0.475198956297498,0.192588479303088,
-3.21111461287478));
#66179=CARTESIAN_POINT('Ctrl Pts',(0.324928484395358,0.396643228172426,
-3.19720498292901));
#66180=CARTESIAN_POINT('Ctrl Pts',(0.0952878493958325,0.503810079478394,
-3.18329535298326));
#66181=CARTESIAN_POINT('Ctrl Pts',(-0.157628714033977,0.487911425300231,
-3.1693857230375));
#66182=CARTESIAN_POINT('Ctrl Pts',(-0.372041368626771,0.35283082413081,
-3.15547609309174));
#66183=CARTESIAN_POINT('Ctrl Pts',(-0.475793553181783,0.166996697092384,
-3.14379387087955));
#66184=CARTESIAN_POINT('Ctrl Pts',(-0.49177846040746,0.042549655106789,
-3.13674819198261));
#66185=CARTESIAN_POINT('Ctrl Pts',(-0.491782972158755,-1.50095741644624E-6,
-3.13433905640093));
#66186=CARTESIAN_POINT('Ctrl Pts',(-0.491785594053212,-4.88331669762365E-6,
-3.27481094359907));
#66187=CARTESIAN_POINT('Ctrl Pts',(-0.49179795679528,-0.0356112203065527,
-3.27279497481717));
#66188=CARTESIAN_POINT('Ctrl Pts',(-0.479213063431929,-0.153100258346796,
-3.26614246272001));
#66189=CARTESIAN_POINT('Ctrl Pts',(-0.386645261186138,-0.336763732174116,
-3.2548534073076));
#66190=CARTESIAN_POINT('Ctrl Pts',(-0.178143619199366,-0.480800603414854,
-3.24094377736184));
#66191=CARTESIAN_POINT('Ctrl Pts',(0.0738731000725598,-0.507392485548619,
-3.22703414741608));
#66192=CARTESIAN_POINT('Ctrl Pts',(0.307844863968601,-0.410043789166097,
-3.21312451747032));
#66193=CARTESIAN_POINT('Ctrl Pts',(0.466619474536125,-0.212533845043952,
-3.19921488752456));
#66194=CARTESIAN_POINT('Ctrl Pts',(0.511413115207255,0.0368916643640206,
-3.18530525757881));
#66195=CARTESIAN_POINT('Ctrl Pts',(0.431284059612851,0.277305660290942,
-3.17139562763304));
#66196=CARTESIAN_POINT('Ctrl Pts',(0.245805403116349,0.449982303101295,
-3.15748599768729));
#66197=CARTESIAN_POINT('Ctrl Pts',(0.000283949904538727,0.5127419318507,
-3.14357636774152));
#66198=CARTESIAN_POINT('Ctrl Pts',(-0.24530686364752,0.450254274774769,
-3.12966673779577));
#66199=CARTESIAN_POINT('Ctrl Pts',(-0.430976658539604,0.277783169215801,
-3.11575710785));
#66200=CARTESIAN_POINT('Ctrl Pts',(-0.488497120387308,0.105837624003322,
-3.10580517645111));
#66201=CARTESIAN_POINT('Ctrl Pts',(-0.491857872385214,0.0119962273922986,
-3.10048978836747));
#66202=CARTESIAN_POINT('Ctrl Pts',(-0.491846492690184,1.06369834089078E-5,
-3.09981094359907));
#66203=CARTESIAN_POINT('Origin',(0.,0.,-4.27183905640093));
#66204=CARTESIAN_POINT('',(-0.49179609326986,9.71264568225073E-6,-3.48433905640093));
#66205=CARTESIAN_POINT('',(-0.491867129348278,-1.39672308571703E-6,-3.44981094359908));
#66206=CARTESIAN_POINT('',(-0.491825,-1.07154090996976E-14,-4.27183905640093));
#66207=CARTESIAN_POINT('Ctrl Pts',(-0.49179609326986,9.71264568224578E-6,
-3.48433905640093));
#66208=CARTESIAN_POINT('Ctrl Pts',(-0.491758729881948,-0.0526289498675229,
-3.48135856488202));
#66209=CARTESIAN_POINT('Ctrl Pts',(-0.470245757754536,-0.187183730626312,
-3.47374153004786));
#66210=CARTESIAN_POINT('Ctrl Pts',(-0.349636937317957,-0.3750445073447,
-3.46148795189843));
#66211=CARTESIAN_POINT('Ctrl Pts',(-0.127322336735289,-0.496682386435005,
-3.44757832195268));
#66212=CARTESIAN_POINT('Ctrl Pts',(0.12609324488764,-0.496995839037123,
-3.43366869200692));
#66213=CARTESIAN_POINT('Ctrl Pts',(0.348708075290391,-0.375908298197551,
-3.41975906206116));
#66214=CARTESIAN_POINT('Ctrl Pts',(0.486144110547877,-0.162997773623204,
-3.4058494321154));
#66215=CARTESIAN_POINT('Ctrl Pts',(0.504829900148016,0.0897281580277445,
-3.39193980216964));
#66216=CARTESIAN_POINT('Ctrl Pts',(0.40020107303874,0.320536225043519,-3.37803017222388));
#66217=CARTESIAN_POINT('Ctrl Pts',(0.197815274890308,0.473047024561597,
-3.36412054227812));
#66218=CARTESIAN_POINT('Ctrl Pts',(-0.0528907887479718,0.51000679886853,
-3.35021091233236));
#66219=CARTESIAN_POINT('Ctrl Pts',(-0.29067723859158,0.422387397292203,
-3.3363012823866));
#66220=CARTESIAN_POINT('Ctrl Pts',(-0.4540346552045,0.235510171083702,-3.32267733040946));
#66221=CARTESIAN_POINT('Ctrl Pts',(-0.491821369807362,0.0768056144799782,
-3.31368992174757));
#66222=CARTESIAN_POINT('Ctrl Pts',(-0.491862997454019,-5.20327585694629E-6,
-3.30933905640093));
#66223=CARTESIAN_POINT('Ctrl Pts',(-0.491867129348278,-1.39672308572809E-6,
-3.44981094359908));
#66224=CARTESIAN_POINT('Ctrl Pts',(-0.491867342373088,-0.00131199121913817,
-3.44973670458213));
#66225=CARTESIAN_POINT('Ctrl Pts',(-0.491541924711959,-0.0844746968207473,
-3.44502592224992));
#66226=CARTESIAN_POINT('Ctrl Pts',(-0.448140419207187,-0.24914761483575,
-3.43567859660246));
#66227=CARTESIAN_POINT('Ctrl Pts',(-0.274088123141906,-0.433335978264076,
-3.42176896665671));
#66228=CARTESIAN_POINT('Ctrl Pts',(-0.0330844205931006,-0.511673519365186,
-3.40785933671095));
#66229=CARTESIAN_POINT('Ctrl Pts',(0.216000801380951,-0.4650247553715,-3.39394970676519));
#66230=CARTESIAN_POINT('Ctrl Pts',(0.412323585901499,-0.304784562953681,
-3.38004007681943));
#66231=CARTESIAN_POINT('Ctrl Pts',(0.50792823756029,-0.0700947558269063,
-3.36613044687367));
#66232=CARTESIAN_POINT('Ctrl Pts',(0.479461442753112,0.18171707189651,-3.35222081692791));
#66233=CARTESIAN_POINT('Ctrl Pts',(0.33387677512836,0.38914093633981,-3.33831118698215));
#66234=CARTESIAN_POINT('Ctrl Pts',(0.106736148672607,0.501509485326126,
-3.3244015570364));
#66235=CARTESIAN_POINT('Ctrl Pts',(-0.146476878127779,0.491374494127927,
-3.31049192709063));
#66236=CARTESIAN_POINT('Ctrl Pts',(-0.363910051005443,0.361211633371286,
-3.29658229714488));
#66237=CARTESIAN_POINT('Ctrl Pts',(-0.473821174853051,0.174468579041008,
-3.28468863598102));
#66238=CARTESIAN_POINT('Ctrl Pts',(-0.491769523622302,0.0462800893370987,
-3.27743151813242));
#66239=CARTESIAN_POINT('Ctrl Pts',(-0.491785594053212,-4.88331669762365E-6,
-3.27481094359907));
#66240=CARTESIAN_POINT('Origin',(0.,0.,-4.27183905640093));
#66241=CARTESIAN_POINT('',(-0.491826729621748,-1.27889840308831E-5,-3.65933905640093));
#66242=CARTESIAN_POINT('',(-0.491789055620677,7.06292780691675E-6,-3.62481094359907));
#66243=CARTESIAN_POINT('',(-0.491825,-1.07154090996976E-14,-4.27183905640093));
#66244=CARTESIAN_POINT('Ctrl Pts',(-0.491826729621748,-1.27889840308929E-5,
-3.65933905640093));
#66245=CARTESIAN_POINT('Ctrl Pts',(-0.491845702227525,-0.018355149817109,
-3.65830029464697));
#66246=CARTESIAN_POINT('Ctrl Pts',(-0.486347785408333,-0.11855786198984,
-3.65262498957776));
#66247=CARTESIAN_POINT('Ctrl Pts',(-0.419886639219421,-0.294278066833141,
-3.6423131411933));
#66248=CARTESIAN_POINT('Ctrl Pts',(-0.227671785951002,-0.459423473843918,
-3.62840351124754));
#66249=CARTESIAN_POINT('Ctrl Pts',(0.0201563719388868,-0.512345675389839,
-3.61449388130178));
#66250=CARTESIAN_POINT('Ctrl Pts',(0.263060940163059,-0.440117384557558,
-3.60058425135602));
#66251=CARTESIAN_POINT('Ctrl Pts',(0.441707707892028,-0.260381779728162,
-3.58667462141027));
#66252=CARTESIAN_POINT('Ctrl Pts',(0.512458693932598,-0.0170428119589638,
-3.57276499146451));
#66253=CARTESIAN_POINT('Ctrl Pts',(0.458031580571258,0.230459197312829,
-3.55885536151875));
#66254=CARTESIAN_POINT('Ctrl Pts',(0.291721259059309,0.421667021996254,
-3.54494573157299));
#66255=CARTESIAN_POINT('Ctrl Pts',(0.0541522913452231,0.509874396070913,
-3.53103610162723));
#66256=CARTESIAN_POINT('Ctrl Pts',(-0.196644436945652,0.473534936245239,
-3.51712647168147));
#66257=CARTESIAN_POINT('Ctrl Pts',(-0.399406899907004,0.321525269198555,
-3.50321684173571));
#66258=CARTESIAN_POINT('Ctrl Pts',(-0.482064722644773,0.140377619227812,
-3.49228770330886));
#66259=CARTESIAN_POINT('Ctrl Pts',(-0.491816853505303,0.0292573555458383,
-3.48599510819727));
#66260=CARTESIAN_POINT('Ctrl Pts',(-0.49179609326986,9.71264568224578E-6,
-3.48433905640093));
#66261=CARTESIAN_POINT('Ctrl Pts',(-0.491789055620677,7.06292780690287E-6,
-3.62481094359907));
#66262=CARTESIAN_POINT('Ctrl Pts',(-0.491764279731792,-0.0488993655234134,
-3.62204189103183));
#66263=CARTESIAN_POINT('Ctrl Pts',(-0.472379668665207,-0.179714664337686,
-3.61463629514933));
#66264=CARTESIAN_POINT('Ctrl Pts',(-0.358086963773074,-0.366985143679068,
-3.60259415595158));
#66265=CARTESIAN_POINT('Ctrl Pts',(-0.13860001322218,-0.493654135646059,
-3.58868452600581));
#66266=CARTESIAN_POINT('Ctrl Pts',(0.114742712316349,-0.499738410846886,
-3.57477489606006));
#66267=CARTESIAN_POINT('Ctrl Pts',(0.340057277111318,-0.383751765584462,
-3.5608652661143));
#66268=CARTESIAN_POINT('Ctrl Pts',(0.482306174096344,-0.174026215651783,
-3.54695563616854));
#66269=CARTESIAN_POINT('Ctrl Pts',(0.506742316769786,0.0782086548939713,
-3.53304600622278));
#66270=CARTESIAN_POINT('Ctrl Pts',(0.407396697418865,0.311339525659273,
-3.51913637627702));
#66271=CARTESIAN_POINT('Ctrl Pts',(0.208536434469852,0.46841960335167,-3.50522674633126));
#66272=CARTESIAN_POINT('Ctrl Pts',(-0.041262947733106,0.511078994334449,
-3.4913171163855));
#66273=CARTESIAN_POINT('Ctrl Pts',(-0.280983044651029,0.428897304636174,
-3.47740748643975));
#66274=CARTESIAN_POINT('Ctrl Pts',(-0.451154396430177,0.242946813420274,
-3.46357209551093));
#66275=CARTESIAN_POINT('Ctrl Pts',(-0.491854038064979,0.0805402261099205,
-3.45437324789738));
#66276=CARTESIAN_POINT('Ctrl Pts',(-0.491867129348278,-1.39672308572809E-6,
-3.44981094359908));
#66277=CARTESIAN_POINT('Origin',(0.,0.,-4.27183905640093));
#66278=CARTESIAN_POINT('',(-0.491834365111822,1.2415361585749E-5,-3.83433905640093));
#66279=CARTESIAN_POINT('',(-0.491838560105423,-1.18860308867263E-5,-3.79981094359907));
#66280=CARTESIAN_POINT('',(-0.491825,-1.07154090996976E-14,-4.27183905640093));
#66281=CARTESIAN_POINT('Ctrl Pts',(-0.491834365111822,1.24153615857388E-5,
-3.83433905640092));
#66282=CARTESIAN_POINT('Ctrl Pts',(-0.491766406376123,-0.0659117740156114,
-3.83060548109667));
#66283=CARTESIAN_POINT('Ctrl Pts',(-0.461856136979431,-0.213763970312948,
-3.82223536247717));
#66284=CARTESIAN_POINT('Ctrl Pts',(-0.318098551972822,-0.402141302407426,
-3.80922870054241));
#66285=CARTESIAN_POINT('Ctrl Pts',(-0.086658980441776,-0.505365835465607,
-3.79531907059665));
#66286=CARTESIAN_POINT('Ctrl Pts',(0.165948741836808,-0.485144687019642,
-3.7814094406509));
#66287=CARTESIAN_POINT('Ctrl Pts',(0.378020228680476,-0.346417499554377,
-3.76749981070513));
#66288=CARTESIAN_POINT('Ctrl Pts',(0.497752849465234,-0.123070995229855,
-3.75359018075938));
#66289=CARTESIAN_POINT('Ctrl Pts',(0.495899563082201,0.130337996110901,
-3.73968055081361));
#66290=CARTESIAN_POINT('Ctrl Pts',(0.372913069708243,0.351909382815266,
-3.72577092086785));
#66291=CARTESIAN_POINT('Ctrl Pts',(0.158835236222117,0.487519986810459,
-3.7118612909221));
#66292=CARTESIAN_POINT('Ctrl Pts',(-0.0940412229640735,0.504044263082503,
-3.69795166097634));
#66293=CARTESIAN_POINT('Ctrl Pts',(-0.323946266642341,0.397445828529313,
-3.68404203103058));
#66294=CARTESIAN_POINT('Ctrl Pts',(-0.463461312679454,0.208974308740659,
-3.67117116283877));
#66295=CARTESIAN_POINT('Ctrl Pts',(-0.49176101744956,0.0635165114976635,
-3.66293683796222));
#66296=CARTESIAN_POINT('Ctrl Pts',(-0.491826729621748,-1.27889840308929E-5,
-3.65933905640093));
#66297=CARTESIAN_POINT('Ctrl Pts',(-0.491838560105423,-1.18860308867142E-5,
-3.79981094359907));
#66298=CARTESIAN_POINT('Ctrl Pts',(-0.491853378270322,-0.0146196642867341,
-3.79898362079678));
#66299=CARTESIAN_POINT('Ctrl Pts',(-0.48764117239995,-0.111084912717674,
-3.79351975467924));
#66300=CARTESIAN_POINT('Ctrl Pts',(-0.426479195061789,-0.284639888869293,
-3.78341934524644));
#66301=CARTESIAN_POINT('Ctrl Pts',(-0.238074960618299,-0.454119677846183,
-3.76950971530068));
#66302=CARTESIAN_POINT('Ctrl Pts',(0.00848375782171881,-0.512671820463746,
-3.75560008535492));
#66303=CARTESIAN_POINT('Ctrl Pts',(0.252970151983937,-0.445993801941228,
-3.74169045540916));
#66304=CARTESIAN_POINT('Ctrl Pts',(0.435663618735166,-0.270373039805825,
-3.72778082546341));
#66305=CARTESIAN_POINT('Ctrl Pts',(0.511937691309605,-0.0287083528804346,
-3.71387119551764));
#66306=CARTESIAN_POINT('Ctrl Pts',(0.46316092958135,0.219968912808865,-3.69996156557189));
#66307=CARTESIAN_POINT('Ctrl Pts',(0.301248015490757,0.414914452000562,
-3.68605193562613));
#66308=CARTESIAN_POINT('Ctrl Pts',(0.0657493578520152,0.508508988358545,
-3.67214230568037));
#66309=CARTESIAN_POINT('Ctrl Pts',(-0.185809871592183,0.477890218488734,
-3.65823267573461));
#66310=CARTESIAN_POINT('Ctrl Pts',(-0.391981391059797,0.330537378169973,
-3.64432304578885));
#66311=CARTESIAN_POINT('Ctrl Pts',(-0.480421481164107,0.147851808358191,
-3.63318246841034));
#66312=CARTESIAN_POINT('Ctrl Pts',(-0.491805764853219,0.0329902947129077,
-3.62667843434708));
#66313=CARTESIAN_POINT('Ctrl Pts',(-0.491789055620677,7.06292780690287E-6,
-3.62481094359907));
#66314=CARTESIAN_POINT('Ctrl Pts',(-0.214786219406509,0.442446279878201,
-4.00597342437858));
#66315=CARTESIAN_POINT('Ctrl Pts',(-0.288440279010312,0.406690804635878,
-4.00133688106333));
#66316=CARTESIAN_POINT('Ctrl Pts',(-0.417471723369089,0.297721387833798,
-3.99206379443282));
#66317=CARTESIAN_POINT('Ctrl Pts',(-0.509054350485474,0.0613839821133976,
-3.97815416448707));
#66318=CARTESIAN_POINT('Ctrl Pts',(-0.476283132556506,-0.189881432885139,
-3.9642445345413));
#66319=CARTESIAN_POINT('Ctrl Pts',(-0.327174291768812,-0.394797097600903,
-3.95033490459555));
#66320=CARTESIAN_POINT('Ctrl Pts',(-0.0981447036446028,-0.503259303300383,
-3.93642527464979));
#66321=CARTESIAN_POINT('Ctrl Pts',(0.154857629827177,-0.488798982873136,
-3.92251564470403));
#66322=CARTESIAN_POINT('Ctrl Pts',(0.37003347141403,-0.354935592235777,
-3.90860601475827));
#66323=CARTESIAN_POINT('Ctrl Pts',(0.494821102216335,-0.134374424279909,
-3.89469638481251));
#66324=CARTESIAN_POINT('Ctrl Pts',(0.498739099375933,0.119011467407269,
-3.88078675486675));
#66325=CARTESIAN_POINT('Ctrl Pts',(0.380830207075808,0.343325891736714,
-3.86687712492099));
#66326=CARTESIAN_POINT('Ctrl Pts',(0.169896094203756,0.483776521506451,
-3.85296749497524));
#66327=CARTESIAN_POINT('Ctrl Pts',(-0.0825384944710284,0.506055083932911,
-3.83905786502947));
#66328=CARTESIAN_POINT('Ctrl Pts',(-0.314811425572855,0.404719832155649,
-3.82514823508372));
#66329=CARTESIAN_POINT('Ctrl Pts',(-0.47018548870497,0.204523773912369,
-3.81123860513796));
#66330=CARTESIAN_POINT('Ctrl Pts',(-0.510707510476629,-0.0456312120848563,
-3.7973289751922));
#66331=CARTESIAN_POINT('Ctrl Pts',(-0.426479195061789,-0.284639888869293,
-3.78341934524644));
#66332=CARTESIAN_POINT('Ctrl Pts',(-0.238074960618299,-0.454119677846183,
-3.76950971530068));
#66333=CARTESIAN_POINT('Ctrl Pts',(0.00848375782171881,-0.512671820463746,
-3.75560008535492));
#66334=CARTESIAN_POINT('Ctrl Pts',(0.252970151983937,-0.445993801941228,
-3.74169045540916));
#66335=CARTESIAN_POINT('Ctrl Pts',(0.435663618735166,-0.270373039805825,
-3.72778082546341));
#66336=CARTESIAN_POINT('Ctrl Pts',(0.511937691309605,-0.0287083528804346,
-3.71387119551764));
#66337=CARTESIAN_POINT('Ctrl Pts',(0.46316092958135,0.219968912808865,-3.69996156557189));
#66338=CARTESIAN_POINT('Ctrl Pts',(0.301248015490757,0.414914452000562,
-3.68605193562613));
#66339=CARTESIAN_POINT('Ctrl Pts',(0.0657493578520152,0.508508988358545,
-3.67214230568037));
#66340=CARTESIAN_POINT('Ctrl Pts',(-0.185809871592183,0.477890218488734,
-3.65823267573461));
#66341=CARTESIAN_POINT('Ctrl Pts',(-0.391981391059797,0.330537378169973,
-3.64432304578885));
#66342=CARTESIAN_POINT('Ctrl Pts',(-0.502403758224836,0.102444292311302,
-3.63041341584309));
#66343=CARTESIAN_POINT('Ctrl Pts',(-0.490104141488973,-0.15067282369779,
-3.61650378589733));
#66344=CARTESIAN_POINT('Ctrl Pts',(-0.358086963773074,-0.366985143679068,
-3.60259415595158));
#66345=CARTESIAN_POINT('Ctrl Pts',(-0.13860001322218,-0.493654135646059,
-3.58868452600581));
#66346=CARTESIAN_POINT('Ctrl Pts',(0.114742712316349,-0.499738410846886,
-3.57477489606006));
#66347=CARTESIAN_POINT('Ctrl Pts',(0.340057277111318,-0.383751765584462,
-3.5608652661143));
#66348=CARTESIAN_POINT('Ctrl Pts',(0.482306174096344,-0.174026215651783,
-3.54695563616854));
#66349=CARTESIAN_POINT('Ctrl Pts',(0.506742316769786,0.0782086548939713,
-3.53304600622278));
#66350=CARTESIAN_POINT('Ctrl Pts',(0.407396697418865,0.311339525659273,
-3.51913637627702));
#66351=CARTESIAN_POINT('Ctrl Pts',(0.208536434469852,0.46841960335167,-3.50522674633126));
#66352=CARTESIAN_POINT('Ctrl Pts',(-0.041262947733106,0.511078994334449,
-3.4913171163855));
#66353=CARTESIAN_POINT('Ctrl Pts',(-0.280983044651029,0.428897304636174,
-3.47740748643975));
#66354=CARTESIAN_POINT('Ctrl Pts',(-0.452067515107786,0.24194902580876,
-3.46349785649398));
#66355=CARTESIAN_POINT('Ctrl Pts',(-0.512725617522656,-0.00410005384696384,
-3.44958822654823));
#66356=CARTESIAN_POINT('Ctrl Pts',(-0.448140419207187,-0.24914761483575,
-3.43567859660246));
#66357=CARTESIAN_POINT('Ctrl Pts',(-0.274088123141906,-0.433335978264076,
-3.42176896665671));
#66358=CARTESIAN_POINT('Ctrl Pts',(-0.0330844205931006,-0.511673519365186,
-3.40785933671095));
#66359=CARTESIAN_POINT('Ctrl Pts',(0.216000801380951,-0.4650247553715,-3.39394970676519));
#66360=CARTESIAN_POINT('Ctrl Pts',(0.412323585901499,-0.304784562953681,
-3.38004007681943));
#66361=CARTESIAN_POINT('Ctrl Pts',(0.50792823756029,-0.0700947558269063,
-3.36613044687367));
#66362=CARTESIAN_POINT('Ctrl Pts',(0.479461442753112,0.18171707189651,-3.35222081692791));
#66363=CARTESIAN_POINT('Ctrl Pts',(0.33387677512836,0.38914093633981,-3.33831118698215));
#66364=CARTESIAN_POINT('Ctrl Pts',(0.106736148672607,0.501509485326126,
-3.3244015570364));
#66365=CARTESIAN_POINT('Ctrl Pts',(-0.146476878127779,0.491374494127927,
-3.31049192709063));
#66366=CARTESIAN_POINT('Ctrl Pts',(-0.363910051005443,0.361211633371286,
-3.29658229714488));
#66367=CARTESIAN_POINT('Ctrl Pts',(-0.492451047640611,0.142815737869471,
-3.28267266719911));
#66368=CARTESIAN_POINT('Ctrl Pts',(-0.500701205381039,-0.110465706151326,
-3.26876303725336));
#66369=CARTESIAN_POINT('Ctrl Pts',(-0.386645261186138,-0.336763732174116,
-3.2548534073076));
#66370=CARTESIAN_POINT('Ctrl Pts',(-0.178143619199366,-0.480800603414854,
-3.24094377736184));
#66371=CARTESIAN_POINT('Ctrl Pts',(0.0738731000725598,-0.507392485548619,
-3.22703414741608));
#66372=CARTESIAN_POINT('Ctrl Pts',(0.307844863968601,-0.410043789166097,
-3.21312451747032));
#66373=CARTESIAN_POINT('Ctrl Pts',(0.466619474536125,-0.212533845043952,
-3.19921488752456));
#66374=CARTESIAN_POINT('Ctrl Pts',(0.511413115207255,0.0368916643640206,
-3.18530525757881));
#66375=CARTESIAN_POINT('Ctrl Pts',(0.431284059612851,0.277305660290942,
-3.17139562763304));
#66376=CARTESIAN_POINT('Ctrl Pts',(0.245805403116349,0.449982303101295,
-3.15748599768729));
#66377=CARTESIAN_POINT('Ctrl Pts',(0.000283949904538727,0.5127419318507,
-3.14357636774152));
#66378=CARTESIAN_POINT('Ctrl Pts',(-0.24530686364752,0.450254274774769,
-3.12966673779577));
#66379=CARTESIAN_POINT('Ctrl Pts',(-0.430976658539604,0.277783169215801,
-3.11575710785));
#66380=CARTESIAN_POINT('Ctrl Pts',(-0.51137194127832,0.0374580696082845,
-3.10184747790425));
#66381=CARTESIAN_POINT('Ctrl Pts',(-0.466854585292198,-0.212016899083981,
-3.08793784795849));
#66382=CARTESIAN_POINT('Ctrl Pts',(-0.308298828990521,-0.409702576692666,
-3.07402821801273));
#66383=CARTESIAN_POINT('Ctrl Pts',(-0.0744350294889845,-0.507310354408927,
-3.06011858806697));
#66384=CARTESIAN_POINT('Ctrl Pts',(0.177610987683289,-0.480997615752618,
-3.04620895812121));
#66385=CARTESIAN_POINT('Ctrl Pts',(0.386272033277762,-0.337191763857008,
-3.03229932817546));
#66386=CARTESIAN_POINT('Ctrl Pts',(0.500578549326249,-0.111020202035327,
-3.0183896982297));
#66387=CARTESIAN_POINT('Ctrl Pts',(0.492608924589448,0.142270224292942,
-3.00448006828394));
#66388=CARTESIAN_POINT('Ctrl Pts',(0.364309896412847,0.360808354505819,
-2.99057043833818));
#66389=CARTESIAN_POINT('Ctrl Pts',(0.147021021901026,0.491211958755805,
-2.97666080839242));
#66390=CARTESIAN_POINT('Ctrl Pts',(-0.10618062433576,0.501627395903777,
-2.96275117844666));
#66391=CARTESIAN_POINT('Ctrl Pts',(-0.333445567956295,0.389510490893173,
-2.9488415485009));
#66392=CARTESIAN_POINT('Ctrl Pts',(-0.479259883565437,0.1822479994688,-2.93493191855514));
#66393=CARTESIAN_POINT('Ctrl Pts',(-0.508005561146717,-0.0695321447213124,
-2.92102228860938));
#66394=CARTESIAN_POINT('Ctrl Pts',(-0.412660904457599,-0.304327697125603,
-2.90711265866362));
#66395=CARTESIAN_POINT('Ctrl Pts',(-0.216515718225303,-0.464785233271151,
-2.89320302871787));
#66396=CARTESIAN_POINT('Ctrl Pts',(0.0325176840114124,-0.511709848969189,
-2.87929339877211));
#66397=CARTESIAN_POINT('Ctrl Pts',(0.273608003362249,-0.43363928535323,
-2.86538376882635));
#66398=CARTESIAN_POINT('Ctrl Pts',(0.447864194914093,-0.249643810697336,
-2.85147413888059));
#66399=CARTESIAN_POINT('Ctrl Pts',(0.51272076192407,-0.00466793289774274,
-2.83756450893483));
#66400=CARTESIAN_POINT('Ctrl Pts',(0.452335214279015,0.241448179178668,
-2.82365487898907));
#66401=CARTESIAN_POINT('Ctrl Pts',(0.281457907812556,0.428585832051545,
-2.80974524904331));
#66402=CARTESIAN_POINT('Ctrl Pts',(0.0418289802326045,0.511032979090623,
-2.79583561909755));
#66403=CARTESIAN_POINT('Ctrl Pts',(-0.208017497185851,0.468650285575578,
-2.78192598915179));
#66404=CARTESIAN_POINT('Ctrl Pts',(-0.40705161597261,0.311790556687697,
-2.76801635920603));
#66405=CARTESIAN_POINT('Ctrl Pts',(-0.506655384081065,0.0787698615411085,
-2.75410672926028));
#66406=CARTESIAN_POINT('Ctrl Pts',(-0.482498625181512,-0.17349191913022,
-2.74019709931452));
#66407=CARTESIAN_POINT('Ctrl Pts',(-0.340482102013575,-0.383374891606055,
-2.72628746936876));
#66408=CARTESIAN_POINT('Ctrl Pts',(-0.115296139210803,-0.499611018281843,
-2.712377839423));
#66409=CARTESIAN_POINT('Ctrl Pts',(0.138053169722395,-0.493807342629832,
-2.69846820947724));
#66410=CARTESIAN_POINT('Ctrl Pts',(0.357680280931475,-0.367381526397719,
-2.68455857953148));
#66411=CARTESIAN_POINT('Ctrl Pts',(0.489936959575747,-0.151215557887439,
-2.67064894958572));
#66412=CARTESIAN_POINT('Ctrl Pts',(0.502516914705533,0.101887780132694,
-2.65673931963996));
#66413=CARTESIAN_POINT('Ctrl Pts',(0.392347245241488,0.330103027033912,
-2.64282968969421));
#66414=CARTESIAN_POINT('Ctrl Pts',(0.186339056407328,0.477684127183188,
-2.62892005974845));
#66415=CARTESIAN_POINT('Ctrl Pts',(-0.0651861061879488,0.508581498744882,
-2.61501042980269));
#66416=CARTESIAN_POINT('Ctrl Pts',(-0.300788282254515,0.415247851967851,
-2.60110079985693));
#66417=CARTESIAN_POINT('Ctrl Pts',(-0.46291701364987,0.220481762917078,
-2.58719116991117));
#66418=CARTESIAN_POINT('Ctrl Pts',(-0.511969173927383,-0.028141326437292,
-2.57328153996541));
#66419=CARTESIAN_POINT('Ctrl Pts',(-0.435962809677364,-0.269890344183994,
-2.55937191001965));
#66420=CARTESIAN_POINT('Ctrl Pts',(-0.253463967943028,-0.445713345391533,
-2.54546228007389));
#66421=CARTESIAN_POINT('Ctrl Pts',(-0.00905157463938524,-0.512662109290402,
-2.53155265012813));
#66422=CARTESIAN_POINT('Ctrl Pts',(0.237571843520245,-0.454383085591805,
-2.51764302018238));
#66423=CARTESIAN_POINT('Ctrl Pts',(0.426163673582462,-0.285112070288575,
-2.50373339023661));
#66424=CARTESIAN_POINT('Ctrl Pts',(0.510656657582095,-0.0461968329284603,
-2.48982376029085));
#66425=CARTESIAN_POINT('Ctrl Pts',(0.470411724946076,0.204002888064838,
-2.4759141303451));
#66426=CARTESIAN_POINT('Ctrl Pts',(0.315259490780706,0.404370897541139,
-2.46200450039934));
#66427=CARTESIAN_POINT('Ctrl Pts',(0.083098935083214,0.505963374458638,
-2.44809487045358));
#66428=CARTESIAN_POINT('Ctrl Pts',(-0.169360167363873,0.48396436130775,
-2.43418524050782));
#66429=CARTESIAN_POINT('Ctrl Pts',(-0.380449723121679,0.343747549056243,
-2.42027561056206));
#66430=CARTESIAN_POINT('Ctrl Pts',(-0.498606962924748,0.119563647604509,
-2.4063659806163));
#66431=CARTESIAN_POINT('Ctrl Pts',(-0.494969660638129,-0.133826022706017,
-2.39245635067054));
#66432=CARTESIAN_POINT('Ctrl Pts',(-0.370426298772862,-0.354526058961786,
-2.37854672072478));
#66433=CARTESIAN_POINT('Ctrl Pts',(-0.155399039185073,-0.488626143309885,
-2.36463709077902));
#66434=CARTESIAN_POINT('Ctrl Pts',(0.0975874873726366,-0.503369696757594,
-2.35072746083327));
#66435=CARTESIAN_POINT('Ctrl Pts',(0.326736353765087,-0.395155316848746,
-2.3368178308875));
#66436=CARTESIAN_POINT('Ctrl Pts',(0.476073449464557,-0.190416490936197,
-2.32290820094175));
#66437=CARTESIAN_POINT('Ctrl Pts',(0.509120256238909,0.060835302191775,
-2.30899857099599));
#66438=CARTESIAN_POINT('Ctrl Pts',(0.417804442576766,0.297226878106026,
-2.29508894105023));
#66439=CARTESIAN_POINT('Ctrl Pts',(0.224431689179598,0.461014952249414,
-2.28117931110447));
#66440=CARTESIAN_POINT('Ctrl Pts',(-0.0237629115774706,0.512191071123753,
-2.26726968115871));
#66441=CARTESIAN_POINT('Ctrl Pts',(-0.266152954537513,0.438254462722844,
-2.25336005121295));
#66442=CARTESIAN_POINT('Ctrl Pts',(-0.443529911772546,0.257265595578916,
-2.23945042126719));
#66443=CARTESIAN_POINT('Ctrl Pts',(-0.512565978237527,0.013434554661145,
-2.22554079132144));
#66444=CARTESIAN_POINT('Ctrl Pts',(-0.456397739002481,-0.233678140053707,
-2.21163116137568));
#66445=CARTESIAN_POINT('Ctrl Pts',(-0.288745389504487,-0.423710360205458,
-2.19772153142992));
#66446=CARTESIAN_POINT('Ctrl Pts',(-0.0505613083818057,-0.510243004263906,
-2.18381190148416));
#66447=CARTESIAN_POINT('Ctrl Pts',(0.199973365210935,-0.472138774632788,
-2.1699022715384));
#66448=CARTESIAN_POINT('Ctrl Pts',(0.401660617373509,-0.318705377671398,
-2.15599264159264));
#66449=CARTESIAN_POINT('Ctrl Pts',(0.505234376131355,-0.0874219336362221,
-2.14208301164688));
#66450=CARTESIAN_POINT('Ctrl Pts',(0.485394716977961,0.165216034438012,
-2.12817338170112));
#66451=CARTESIAN_POINT('Ctrl Pts',(0.346987866262887,0.377496741670528,
-2.11426375175536));
#66452=CARTESIAN_POINT('Ctrl Pts',(0.123822415238128,0.49756645665693,-2.10035412180961));
#66453=CARTESIAN_POINT('Ctrl Pts',(-0.129589092271495,0.496095793642505,
-2.08644449186384));
#66454=CARTESIAN_POINT('Ctrl Pts',(-0.351345919187724,0.37344399094867,
-2.07253486191809));
#66455=CARTESIAN_POINT('Ctrl Pts',(-0.487279605786099,0.159571159958436,
-2.05862523197233));
#66456=CARTESIAN_POINT('Ctrl Pts',(-0.504185679716899,-0.0932800604306441,
-2.04471560202657));
#66457=CARTESIAN_POINT('Ctrl Pts',(-0.397934500429466,-0.32334579427215,
-2.03080597208081));
#66458=CARTESIAN_POINT('Ctrl Pts',(-0.194480004972519,-0.474427968158946,
-2.01689634213505));
#66459=CARTESIAN_POINT('Ctrl Pts',(0.0564800508004891,-0.509621794242663,
-2.00298671218929));
#66460=CARTESIAN_POINT('Ctrl Pts',(0.293643745038357,-0.420330489383515,
-1.98907708224353));
#66461=CARTESIAN_POINT('Ctrl Pts',(0.459079188120922,-0.228365208251544,
-1.97516745229777));
#66462=CARTESIAN_POINT('Ctrl Pts',(0.512375524336397,0.0193827595181383,
-1.96125782235201));
#66463=CARTESIAN_POINT('Ctrl Pts',(0.440514076957236,0.262396107646534,
-1.94734819240626));
#66464=CARTESIAN_POINT('Ctrl Pts',(0.261048415685123,0.441314053678131,
-1.9334385624605));
#66465=CARTESIAN_POINT('Ctrl Pts',(0.0178165525430863,0.512432375793154,
-1.91952893251474));
#66466=CARTESIAN_POINT('Ctrl Pts',(-0.229767353430185,0.458379027228804,
-1.90561930256898));
#66467=CARTESIAN_POINT('Ctrl Pts',(-0.421226071271232,0.292357599844676,
-1.89170967262322));
#66468=CARTESIAN_POINT('Ctrl Pts',(-0.50979204937639,0.0549220875254831,
-1.87780004267746));
#66469=CARTESIAN_POINT('Ctrl Pts',(-0.473831308378887,-0.195929223204422,
-1.8638904127317));
#66470=CARTESIAN_POINT('Ctrl Pts',(-0.322127965446493,-0.398920973606101,
-1.84998078278594));
#66471=CARTESIAN_POINT('Ctrl Pts',(-0.0917385411651713,-0.504468442393003,
-1.83607115284018));
#66472=CARTESIAN_POINT('Ctrl Pts',(0.161059823311547,-0.48678958762528,
-1.82216152289443));
#66473=CARTESIAN_POINT('Ctrl Pts',(0.37451616313179,-0.350202816748494,
-1.80825189294867));
#66474=CARTESIAN_POINT('Ctrl Pts',(0.496489575545123,-0.128072130772313,
-1.79434226300291));
#66475=CARTESIAN_POINT('Ctrl Pts',(0.497185659316439,0.125342688161754,
-1.78043263305715));
#66476=CARTESIAN_POINT('Ctrl Pts',(0.376434382315248,0.348140094094997,
-1.76652300311139));
#66477=CARTESIAN_POINT('Ctrl Pts',(0.163731615202558,0.485897445443685,
-1.75261337316563));
#66478=CARTESIAN_POINT('Ctrl Pts',(-0.088965814203307,0.504964803930609,
-1.73870374321987));
#66479=CARTESIAN_POINT('Ctrl Pts',(-0.319931596423644,0.40068459281005,
-1.72479411327411));
#66480=CARTESIAN_POINT('Ctrl Pts',(-0.472747803560086,0.198529301451072,
-1.71088448332836));
#66481=CARTESIAN_POINT('Ctrl Pts',(-0.510086076090958,-0.0521206704069183,
-1.69697485338259));
#66482=CARTESIAN_POINT('Ctrl Pts',(-0.422825807720183,-0.290039144998243,
-1.68306522343684));
#66483=CARTESIAN_POINT('Ctrl Pts',(-0.232282032571033,-0.457109862779405,
-1.66915559349108));
#66484=CARTESIAN_POINT('Ctrl Pts',(0.0150011904725086,-0.51252252008077,
-1.65524596354532));
#66485=CARTESIAN_POINT('Ctrl Pts',(0.25862007815723,-0.442741487190307,
-1.64133633359956));
#66486=CARTESIAN_POINT('Ctrl Pts',(0.439065933099701,-0.264812151716694,
-1.6274267036538));
#66487=CARTESIAN_POINT('Ctrl Pts',(0.512261311724355,-0.0221972479370705,
-1.61351707370804));
#66488=CARTESIAN_POINT('Ctrl Pts',(0.46032680542771,0.225839769549687,-1.59960744376228));
#66489=CARTESIAN_POINT('Ctrl Pts',(0.295948437236704,0.418710988394965,
-1.58569781381652));
#66490=CARTESIAN_POINT('Ctrl Pts',(0.0592788515625552,0.509303825886828,
-1.57178818387076));
#66491=CARTESIAN_POINT('Ctrl Pts',(-0.191870757694326,0.475489202450847,
-1.55787855392501));
#66492=CARTESIAN_POINT('Ctrl Pts',(-0.396152166521947,0.325527003895996,
-1.54396892397925));
#66493=CARTESIAN_POINT('Ctrl Pts',(-0.503665629237551,0.0960484421023013,
-1.53005929403349));
#66494=CARTESIAN_POINT('Ctrl Pts',(-0.488148871276991,-0.15689183782637,
-1.51614966408773));
#66495=CARTESIAN_POINT('Ctrl Pts',(-0.353392165482507,-0.371508205402143,
-1.50224003414197));
#66496=CARTESIAN_POINT('Ctrl Pts',(-0.132312483529502,-0.495376398315253,
-1.48833040419621));
#66497=CARTESIAN_POINT('Ctrl Pts',(0.121087120812267,-0.498239177984762,
-1.47442077425045));
#66498=CARTESIAN_POINT('Ctrl Pts',(0.344908818047041,-0.379397254258554,
-1.46051114430469));
#66499=CARTESIAN_POINT('Ctrl Pts',(0.484479763326162,-0.167880100765288,
-1.44660151435893));
#66500=CARTESIAN_POINT('Ctrl Pts',(0.505707012440461,0.0846450640857451,
-1.43269188441317));
#66501=CARTESIAN_POINT('Ctrl Pts',(0.40340539294362,0.316494009816205,-1.41878225446742));
#66502=CARTESIAN_POINT('Ctrl Pts',(0.202564084346017,0.47103307849725,-1.40487262452166));
#66503=CARTESIAN_POINT('Ctrl Pts',(-0.0477574797057481,0.510513067842236,
-1.3909629945759));
#66504=CARTESIAN_POINT('Ctrl Pts',(-0.28641334150177,0.425290215165276,
-1.37705336463014));
#66505=CARTESIAN_POINT('Ctrl Pts',(-0.455107120193369,0.236181875796673,
-1.36314373468438));
#66506=CARTESIAN_POINT('Ctrl Pts',(-0.512632047610675,-0.0106185247573672,
-1.34923410473862));
#66507=CARTESIAN_POINT('Ctrl Pts',(-0.444936530586125,-0.254825142118117,
-1.33532447479286));
#66508=CARTESIAN_POINT('Ctrl Pts',(-0.268556528523827,-0.436785714387234,
-1.3214148448471));
#66509=CARTESIAN_POINT('Ctrl Pts',(-0.0265763205901719,-0.512052798536855,
-1.30750521490134));
#66510=CARTESIAN_POINT('Ctrl Pts',(0.221895675540188,-0.462240931205903,
-1.29359558495558));
#66511=CARTESIAN_POINT('Ctrl Pts',(0.416165295443046,-0.299517639170616,
-1.27968595500983));
#66512=CARTESIAN_POINT('Ctrl Pts',(0.508778369487043,-0.063631281989616,
-1.26577632506407));
#66513=CARTESIAN_POINT('Ctrl Pts',(0.477112335647494,0.187798265376785,
-1.25186669511831));
#66514=CARTESIAN_POINT('Ctrl Pts',(0.328902244531517,0.393354398536063,
-1.23795706517255));
#66515=CARTESIAN_POINT('Ctrl Pts',(0.100351321370171,0.502825995355051,
-1.22404743522679));
#66516=CARTESIAN_POINT('Ctrl Pts',(-0.15271238268513,0.489472468561989,
-1.21013780528103));
#66517=CARTESIAN_POINT('Ctrl Pts',(-0.368473088379839,0.356555679305995,
-1.19622817533527));
#66518=CARTESIAN_POINT('Ctrl Pts',(-0.494227006346698,0.136543163516585,
-1.18231854538951));
#66519=CARTESIAN_POINT('Ctrl Pts',(-0.499256272629466,-0.116822701328421,
-1.16840891544375));
#66520=CARTESIAN_POINT('Ctrl Pts',(-0.382332390176345,-0.341652327267911,
-1.15449928549799));
#66521=CARTESIAN_POINT('Ctrl Pts',(-0.172016313369507,-0.483026663073893,
-1.14058965555223));
#66522=CARTESIAN_POINT('Ctrl Pts',(0.0803181259485588,-0.506412250986929,
-1.12668002560648));
#66523=CARTESIAN_POINT('Ctrl Pts',(0.313033285756316,-0.406096701924727,
-1.11277039566072));
#66524=CARTESIAN_POINT('Ctrl Pts',(0.469283918326265,-0.206584058692545,
-1.09886076571496));
#66525=CARTESIAN_POINT('Ctrl Pts',(0.510902738281055,0.0433907976701933,
-1.0849511357692));
#66526=CARTESIAN_POINT('Ctrl Pts',(0.427723531557066,0.282766599615103,
-1.07104150582344));
#66527=CARTESIAN_POINT('Ctrl Pts',(0.240064452828482,0.45307110677431,-1.05713187587768));
#66528=CARTESIAN_POINT('Ctrl Pts',(-0.0062350827696745,0.512704098919047,
-1.04322224593192));
#66529=CARTESIAN_POINT('Ctrl Pts',(-0.251011576959888,0.447099046674948,
-1.02931261598616));
#66530=CARTESIAN_POINT('Ctrl Pts',(-0.434473564237258,0.27228127237199,
-1.0154029860404));
#66531=CARTESIAN_POINT('Ctrl Pts',(-0.511806851474115,0.0309534503680939,
-1.00149335609465));
#66532=CARTESIAN_POINT('Ctrl Pts',(-0.464121264630259,-0.217935359736655,
-0.987583726148886));
#66533=CARTESIAN_POINT('Ctrl Pts',(-0.30306494471812,-0.413589178519626,
-0.973674096203129));
#66534=CARTESIAN_POINT('Ctrl Pts',(-0.0679790606200691,-0.508215718590787,
-0.959764466257369));
#66535=CARTESIAN_POINT('Ctrl Pts',(0.183712043973384,-0.478700589308868,
-0.94585483631161));
#66536=CARTESIAN_POINT('Ctrl Pts',(0.390527874180675,-0.332253440604396,
-0.931945206365851));
#66537=CARTESIAN_POINT('Ctrl Pts',(0.501949602127359,-0.104646864404638,
-0.918035576420092));
#66538=CARTESIAN_POINT('Ctrl Pts',(0.490760282718032,0.148521763428982,
-0.904125946474333));
#66539=CARTESIAN_POINT('Ctrl Pts',(0.359693126948704,0.365411033948621,
-0.890216316528574));
#66540=CARTESIAN_POINT('Ctrl Pts',(0.140763861447594,0.493041483666333,
-0.876306686582815));
#66541=CARTESIAN_POINT('Ctrl Pts',(-0.112549741462726,0.500236868895336,
-0.862397056637057));
#66542=CARTESIAN_POINT('Ctrl Pts',(-0.338370859824982,0.385239575494054,
-0.848487426691298));
#66543=CARTESIAN_POINT('Ctrl Pts',(-0.481538250916493,0.176139950635345,
-0.834577796745538));
#66544=CARTESIAN_POINT('Ctrl Pts',(-0.507080468013198,-0.0759853161147112,
-0.820668166799779));
#66545=CARTESIAN_POINT('Ctrl Pts',(-0.408758323003886,-0.309549677241936,
-0.80675853685402));
#66546=CARTESIAN_POINT('Ctrl Pts',(-0.210588930608419,-0.467500450920358,
-0.792848906908262));
#66547=CARTESIAN_POINT('Ctrl Pts',(0.0390209435287369,-0.511255058920363,
-0.778939276962502));
#66548=CARTESIAN_POINT('Ctrl Pts',(0.279099185935138,-0.430125579006736,
-0.765029647016744));
#66549=CARTESIAN_POINT('Ctrl Pts',(0.45100197136601,-0.243929479828719,
-0.751120017070984));
#66550=CARTESIAN_POINT('Ctrl Pts',(0.512738668738538,0.00185118496315108,
-0.737210387125225));
#66551=CARTESIAN_POINT('Ctrl Pts',(0.449228877364958,0.247179661475123,
-0.723300757179467));
#66552=CARTESIAN_POINT('Ctrl Pts',(0.27598611096193,0.432129651680657,-0.709391127233707));
#66553=CARTESIAN_POINT('Ctrl Pts',(0.0353283172785953,0.511523488516217,
-0.695481497287949));
#66554=CARTESIAN_POINT('Ctrl Pts',(-0.213959111659945,0.46596766823807,
-0.681571867342189));
#66555=CARTESIAN_POINT('Ctrl Pts',(-0.41098282595302,0.306590094551677,
-0.667662237396431));
#66556=CARTESIAN_POINT('Ctrl Pts',(-0.507615914330933,0.0723218696073868,
-0.653752607450671));
#66557=CARTESIAN_POINT('Ctrl Pts',(-0.480253847324892,-0.179612392209383,
-0.639842977504913));
#66558=CARTESIAN_POINT('Ctrl Pts',(-0.33558034712377,-0.387672800090266,
-0.625933347559152));
#66559=CARTESIAN_POINT('Ctrl Pts',(-0.108934757177873,-0.501036513623642,
-0.612023717613395));
#66560=CARTESIAN_POINT('Ctrl Pts',(0.144320286415244,-0.49201221959882,
-0.598114087667635));
#66561=CARTESIAN_POINT('Ctrl Pts',(0.362322265961503,-0.362804279045959,
-0.584204457721877));
#66562=CARTESIAN_POINT('Ctrl Pts',(0.491819916942383,-0.144974268766304,
-0.570294827776118));
#66563=CARTESIAN_POINT('Ctrl Pts',(0.501180895095398,0.108268553592046,
-0.55638519783036));
#66564=CARTESIAN_POINT('Ctrl Pts',(0.388118597680438,0.33506465561158,-0.542475567884599));
#66565=CARTESIAN_POINT('Ctrl Pts',(0.180250711102229,0.480014635665076,
-0.528565937938842));
#66566=CARTESIAN_POINT('Ctrl Pts',(-0.0716469513364315,0.507711614668931,
-0.514656307993081));
#66567=CARTESIAN_POINT('Ctrl Pts',(-0.306043438944004,0.411390061601957,
-0.500746678047323));
#66568=CARTESIAN_POINT('Ctrl Pts',(-0.46568280666081,0.214578407315484,
-0.486837048101564));
#66569=CARTESIAN_POINT('Ctrl Pts',(-0.511570004003579,-0.0346482367417505,
-0.472927418155805));
#66570=CARTESIAN_POINT('Ctrl Pts',(-0.432496181911419,-0.275411368569959,
-0.459017788210046));
#66571=CARTESIAN_POINT('Ctrl Pts',(-0.247776674242662,-0.448899865233663,
-0.445108158264288));
#66572=CARTESIAN_POINT('Ctrl Pts',(-0.0025328481751963,-0.512735754541854,
-0.431198528318528));
#66573=CARTESIAN_POINT('Ctrl Pts',(0.243329675797957,-0.451325866953922,
-0.41728889837277));
#66574=CARTESIAN_POINT('Ctrl Pts',(0.429754148070265,-0.279670773449364,
-0.40337926842701));
#66575=CARTESIAN_POINT('Ctrl Pts',(0.511202730378688,-0.0397006014952209,
-0.389469638481251));
#66576=CARTESIAN_POINT('Ctrl Pts',(0.467780007046806,0.209967221996417,
-0.375560008535492));
#66577=CARTESIAN_POINT('Ctrl Pts',(0.310092830963972,0.408346428280455,
-0.361650378589733));
#66578=CARTESIAN_POINT('Ctrl Pts',(0.0766593914673165,0.506979000559367,
-0.347740748643974));
#66579=CARTESIAN_POINT('Ctrl Pts',(-0.175499609789847,0.481771996138208,
-0.333831118698215));
#66580=CARTESIAN_POINT('Ctrl Pts',(-0.384789384990357,0.338882720885541,
-0.319921488752456));
#66581=CARTESIAN_POINT('Ctrl Pts',(-0.500086796588008,0.113214686199793,
-0.306011858806698));
#66582=CARTESIAN_POINT('Ctrl Pts',(-0.493228187695886,-0.140108258752822,
-0.292102228860939));
#66583=CARTESIAN_POINT('Ctrl Pts',(-0.365888908126138,-0.359207010306768,
-0.278192598915179));
#66584=CARTESIAN_POINT('Ctrl Pts',(-0.149174077725999,-0.490562395317217,
-0.26428296896942));
#66585=CARTESIAN_POINT('Ctrl Pts',(0.103979450806552,-0.502088282530429,
-0.250373339023661));
#66586=CARTESIAN_POINT('Ctrl Pts',(0.331733956110991,-0.390969245649164,
-0.236463709077902));
#66587=CARTESIAN_POINT('Ctrl Pts',(0.478455929130976,-0.184348295450463,
-0.222554079132143));
#66588=CARTESIAN_POINT('Ctrl Pts',(0.508305643980286,0.067303351115353,
-0.208644449186384));
#66589=CARTESIAN_POINT('Ctrl Pts',(0.413991726952782,0.302514822609971,
-0.194734819240625));
#66590=CARTESIAN_POINT('Ctrl Pts',(0.218552193979818,0.463831127370637,
-0.180825189294866));
#66591=CARTESIAN_POINT('Ctrl Pts',(-0.0302729907633189,0.511847533035115,
-0.166915559349108));
#66592=CARTESIAN_POINT('Ctrl Pts',(-0.271703429260484,0.434835201098837,
-0.153005929403349));
#66593=CARTESIAN_POINT('Ctrl Pts',(-0.446764918333941,0.251605688139759,
-0.13909629945759));
#66594=CARTESIAN_POINT('Ctrl Pts',(-0.51269540287887,0.006916826412533,
-0.12518666951183));
#66595=CARTESIAN_POINT('Ctrl Pts',(-0.453389771617352,-0.23946215586583,
-0.111277039566072));
#66596=CARTESIAN_POINT('Ctrl Pts',(-0.283335167309922,-0.427346729913706,
-0.0973674096203128));
#66597=CARTESIAN_POINT('Ctrl Pts',(-0.0440696378965106,-0.510845571762323,
-0.0834577796745537));
#66598=CARTESIAN_POINT('Ctrl Pts',(0.205959307621291,-0.469556250960448,
-0.0695481497287949));
#66599=CARTESIAN_POINT('Ctrl Pts',(0.405681497053104,-0.313576606935647,
-0.0556385197830361));
#66600=CARTESIAN_POINT('Ctrl Pts',(0.506302444914719,-0.0809840427845483,
-0.0417288898372769));
#66601=CARTESIAN_POINT('Ctrl Pts',(0.48325998950616,0.171359585523517,-0.0278192598915182));
#66602=CARTESIAN_POINT('Ctrl Pts',(0.342150143078732,0.381908292889331,
-0.0139096299457593));
#66603=CARTESIAN_POINT('Ctrl Pts',(0.192389430706698,0.459979903999379,
-0.00463654331525315));
#66604=CARTESIAN_POINT('Ctrl Pts',(0.112693552167563,0.478740006605732,
0.));
#66605=CARTESIAN_POINT('Ctrl Pts',(-0.229321473482477,0.472388001049917,
-3.98675728291905));
#66606=CARTESIAN_POINT('Ctrl Pts',(-0.30795993326347,0.43421284116167,-3.9821207396038));
#66607=CARTESIAN_POINT('Ctrl Pts',(-0.445723338325901,0.317869123698659,
-3.9728476529733));
#66608=CARTESIAN_POINT('Ctrl Pts',(-0.543503647759894,0.0655380278369941,
-3.95893802302754));
#66609=CARTESIAN_POINT('Ctrl Pts',(-0.508514699194888,-0.202731302299111,
-3.94502839308177));
#66610=CARTESIAN_POINT('Ctrl Pts',(-0.34931519760125,-0.421514249836929,
-3.93111876313602));
#66611=CARTESIAN_POINT('Ctrl Pts',(-0.104786462169088,-0.537316431638404,
-3.91720913319026));
#66612=CARTESIAN_POINT('Ctrl Pts',(0.165337329136378,-0.52187753617962,
-3.9032995032445));
#66613=CARTESIAN_POINT('Ctrl Pts',(0.395074791748627,-0.37895519194756,
-3.88938987329874));
#66614=CARTESIAN_POINT('Ctrl Pts',(0.528307191141123,-0.143467961116758,
-3.87548024335298));
#66615=CARTESIAN_POINT('Ctrl Pts',(0.53249033140134,0.127065344986093,-3.86157061340723));
#66616=CARTESIAN_POINT('Ctrl Pts',(0.406602176222368,0.366559826767745,
-3.84766098346146));
#66617=CARTESIAN_POINT('Ctrl Pts',(0.181393493350638,0.516515189171047,
-3.83375135351571));
#66618=CARTESIAN_POINT('Ctrl Pts',(-0.0881241320947979,0.540301411475365,
-3.81984172356994));
#66619=CARTESIAN_POINT('Ctrl Pts',(-0.336115697650287,0.432108486819904,
-3.80593209362419));
#66620=CARTESIAN_POINT('Ctrl Pts',(-0.502004408745765,0.21836453626019,
-3.79202246367843));
#66621=CARTESIAN_POINT('Ctrl Pts',(-0.545268682249171,-0.0487192186770869,
-3.77811283373267));
#66622=CARTESIAN_POINT('Ctrl Pts',(-0.455340373751309,-0.303902358855974,
-3.76420320378691));
#66623=CARTESIAN_POINT('Ctrl Pts',(-0.254186236524524,-0.484851374305249,
-3.75029357384116));
#66624=CARTESIAN_POINT('Ctrl Pts',(0.00905788020162857,-0.547365923226114,
-3.73638394389539));
#66625=CARTESIAN_POINT('Ctrl Pts',(0.270089431995863,-0.476175595007076,
-3.72247431394964));
#66626=CARTESIAN_POINT('Ctrl Pts',(0.465146336050408,-0.288670027572214,
-3.70856468400387));
#66627=CARTESIAN_POINT('Ctrl Pts',(0.546582113260003,-0.030651136753501,
-3.69465505405812));
#66628=CARTESIAN_POINT('Ctrl Pts',(0.494504475774067,0.234854895928853,
-3.68074542411236));
#66629=CARTESIAN_POINT('Ctrl Pts',(0.321634409260054,0.442993008419515,
-3.6668357941666));
#66630=CARTESIAN_POINT('Ctrl Pts',(0.0701988221814853,0.542921379275098,
-3.65292616422084));
#66631=CARTESIAN_POINT('Ctrl Pts',(-0.198384205741171,0.510230541649818,
-3.63901653427508));
#66632=CARTESIAN_POINT('Ctrl Pts',(-0.418507995642945,0.352905874559456,
-3.62510690432932));
#66633=CARTESIAN_POINT('Ctrl Pts',(-0.536402989156401,0.109377017425102,
-3.61119727438356));
#66634=CARTESIAN_POINT('Ctrl Pts',(-0.523271018953975,-0.160869324110351,
-3.59728764443781));
#66635=CARTESIAN_POINT('Ctrl Pts',(-0.382319826636045,-0.391820174158306,
-3.58337801449204));
#66636=CARTESIAN_POINT('Ctrl Pts',(-0.147979508855949,-0.527061252299515,
-3.56946838454629));
#66637=CARTESIAN_POINT('Ctrl Pts',(0.122507709910199,-0.533557269399598,
-3.55555875460053));
#66638=CARTESIAN_POINT('Ctrl Pts',(0.363070014785332,-0.409721445717036,
-3.54164912465477));
#66639=CARTESIAN_POINT('Ctrl Pts',(0.514945338760956,-0.18580311301218,
-3.52773949470901));
#66640=CARTESIAN_POINT('Ctrl Pts',(0.541035151503999,0.0835012787548714,
-3.51382986476325));
#66641=CARTESIAN_POINT('Ctrl Pts',(0.43496650391323,0.332408843429535,-3.49992023481749));
#66642=CARTESIAN_POINT('Ctrl Pts',(0.222648746085987,0.500119020417133,
-3.48601060487173));
#66643=CARTESIAN_POINT('Ctrl Pts',(-0.0440553402379942,0.545665305579503,
-3.47210097492598));
#66644=CARTESIAN_POINT('Ctrl Pts',(-0.299998044572006,0.45792212435045,
-3.45819134498021));
#66645=CARTESIAN_POINT('Ctrl Pts',(-0.482660335307052,0.258322471802089,
-3.44428171503446));
#66646=CARTESIAN_POINT('Ctrl Pts',(-0.547423360899966,-0.00437751729203636,
-3.43037208508869));
#66647=CARTESIAN_POINT('Ctrl Pts',(-0.478467480565623,-0.266008211824075,
-3.41646245514294));
#66648=CARTESIAN_POINT('Ctrl Pts',(-0.292636522196936,-0.462661176881245,
-3.40255282519718));
#66649=CARTESIAN_POINT('Ctrl Pts',(-0.0353233466313068,-0.546300063975303,
-3.38864319525142));
#66650=CARTESIAN_POINT('Ctrl Pts',(0.230618250011315,-0.496494432474701,
-3.37473356530566));
#66651=CARTESIAN_POINT('Ctrl Pts',(0.440226810322289,-0.325410285931654,
-3.3608239353599));
#66652=CARTESIAN_POINT('Ctrl Pts',(0.542301327257096,-0.0748382868046036,
-3.34691430541414));
#66653=CARTESIAN_POINT('Ctrl Pts',(0.511908095565866,0.194014433511492,
-3.33300467546839));
#66654=CARTESIAN_POINT('Ctrl Pts',(0.356471258936331,0.415475318483546,
-3.31909504552262));
#66655=CARTESIAN_POINT('Ctrl Pts',(0.113959317106475,0.535448198018523,
-3.30518541557687));
#66656=CARTESIAN_POINT('Ctrl Pts',(-0.156389425802974,0.524627340322321,
-3.2912757856311));
#66657=CARTESIAN_POINT('Ctrl Pts',(-0.388536980362357,0.385655952381858,
-3.27736615568535));
#66658=CARTESIAN_POINT('Ctrl Pts',(-0.52577674757244,0.152480524752521,
-3.26345652573959));
#66659=CARTESIAN_POINT('Ctrl Pts',(-0.534585219245928,-0.117941265384257,
-3.24954689579383));
#66660=CARTESIAN_POINT('Ctrl Pts',(-0.412810753200192,-0.359553585379074,
-3.23563726584807));
#66661=CARTESIAN_POINT('Ctrl Pts',(-0.190199154113247,-0.513337881410735,
-3.22172763590231));
#66662=CARTESIAN_POINT('Ctrl Pts',(0.0788723234021615,-0.541729319234063,
-3.20781800595655));
#66663=CARTESIAN_POINT('Ctrl Pts',(0.328677687071171,-0.437792732623787,
-3.1939083760108));
#66664=CARTESIAN_POINT('Ctrl Pts',(0.498197071264252,-0.226916673914411,
-3.17999874606503));
#66665=CARTESIAN_POINT('Ctrl Pts',(0.546022037454967,0.0393882384752367,
-3.16608911611928));
#66666=CARTESIAN_POINT('Ctrl Pts',(0.460470398488362,0.296071800130688,
-3.15217948617351));
#66667=CARTESIAN_POINT('Ctrl Pts',(0.26243982220252,0.480434010493602,-3.13826985622776));
#66668=CARTESIAN_POINT('Ctrl Pts',(0.000303165681132534,0.547440779269527,
-3.124360226282));
#66669=CARTESIAN_POINT('Ctrl Pts',(-0.261907545011288,0.480724387339375,
-3.11045059633624));
#66670=CARTESIAN_POINT('Ctrl Pts',(-0.460142194624714,0.296581623575379,
-3.09654096639048));
#66671=CARTESIAN_POINT('Ctrl Pts',(-0.545978077157708,0.0399929741308204,
-3.08263133644472));
#66672=CARTESIAN_POINT('Ctrl Pts',(-0.498448092699254,-0.22636474460731,
-3.06872170649896));
#66673=CARTESIAN_POINT('Ctrl Pts',(-0.329162373323501,-0.43742842923694,
-3.0548120765532));
#66674=CARTESIAN_POINT('Ctrl Pts',(-0.0794722803366616,-0.541641630023716,
-3.04090244660745));
#66675=CARTESIAN_POINT('Ctrl Pts',(0.189630477759485,-0.513548226188511,
-3.02699281666168));
#66676=CARTESIAN_POINT('Ctrl Pts',(0.412412267793957,-0.360010583302355,
-3.01308318671593));
#66677=CARTESIAN_POINT('Ctrl Pts',(0.534454262672952,-0.118533285735985,
-2.99917355677017));
#66678=CARTESIAN_POINT('Ctrl Pts',(0.525945308547331,0.151898094569056,
-2.98526392682441));
#66679=CARTESIAN_POINT('Ctrl Pts',(0.388963884556884,0.385225382376441,
-2.97135429687865));
#66680=CARTESIAN_POINT('Ctrl Pts',(0.156970393484291,0.524453805674097,
-2.9574446669329));
#66681=CARTESIAN_POINT('Ctrl Pts',(-0.113366198703285,0.535574087973106,
-2.94353503698713));
#66682=CARTESIAN_POINT('Ctrl Pts',(-0.356010870628611,0.415869881947366,
-2.92962540704138));
#66683=CARTESIAN_POINT('Ctrl Pts',(-0.51169289623865,0.19458129061027,-2.91571577709561));
#66684=CARTESIAN_POINT('Ctrl Pts',(-0.542383883572038,-0.0742376020488999,
-2.90180614714986));
#66685=CARTESIAN_POINT('Ctrl Pts',(-0.440586956278262,-0.324922502566556,
-2.8878965172041));
#66686=CARTESIAN_POINT('Ctrl Pts',(-0.231168012886207,-0.496238701165981,
-2.87398688725834));
#66687=CARTESIAN_POINT('Ctrl Pts',(0.034718257215661,-0.54633885211704,
-2.86007725731258));
#66688=CARTESIAN_POINT('Ctrl Pts',(0.292123911212751,-0.462985009708113,
-2.84616762736682));
#66689=CARTESIAN_POINT('Ctrl Pts',(0.478172563312183,-0.266537986808846,
-2.83225799742106));
#66690=CARTESIAN_POINT('Ctrl Pts',(0.547418176707864,-0.00498382649122336,
-2.8183483674753));
#66691=CARTESIAN_POINT('Ctrl Pts',(0.482946150517014,0.257787731316786,
-2.80443873752954));
#66692=CARTESIAN_POINT('Ctrl Pts',(0.3005050432063,0.457589573443535,-2.79052910758379));
#66693=CARTESIAN_POINT('Ctrl Pts',(0.0446596779240103,0.545616176340457,
-2.77661947763802));
#66694=CARTESIAN_POINT('Ctrl Pts',(-0.222094690695742,0.500365313627373,
-2.76270984769227));
#66695=CARTESIAN_POINT('Ctrl Pts',(-0.434598069728088,0.332890397135869,
-2.7488002177465));
#66696=CARTESIAN_POINT('Ctrl Pts',(-0.54094233580881,0.0841004640080302,
-2.73489058780075));
#66697=CARTESIAN_POINT('Ctrl Pts',(-0.515150813611932,-0.185232658976813,
-2.72098095785499));
#66698=CARTESIAN_POINT('Ctrl Pts',(-0.36352358891512,-0.409319067499827,
-2.70707132790923));
#66699=CARTESIAN_POINT('Ctrl Pts',(-0.12309858893052,-0.533421255781931,
-2.69316169796347));
#66700=CARTESIAN_POINT('Ctrl Pts',(0.147395658749169,-0.527224827278226,
-2.67925206801771));
#66701=CARTESIAN_POINT('Ctrl Pts',(0.381885622296803,-0.392243381333121,
-2.66534243807195));
#66702=CARTESIAN_POINT('Ctrl Pts',(0.523092523318703,-0.161448786817147,
-2.6514328081262));
#66703=CARTESIAN_POINT('Ctrl Pts',(0.536523803289445,0.108782844329816,
-2.63752317818043));
#66704=CARTESIAN_POINT('Ctrl Pts',(0.418898608319388,0.35244212952588,-2.62361354823468));
#66705=CARTESIAN_POINT('Ctrl Pts',(0.198949202144987,0.510010503502163,
-2.60970391828892));
#66706=CARTESIAN_POINT('Ctrl Pts',(-0.0695974535187176,0.542998796665671,
-2.59579428834316));
#66707=CARTESIAN_POINT('Ctrl Pts',(-0.321143564440328,0.443348970603538,
-2.5818846583974));
#66708=CARTESIAN_POINT('Ctrl Pts',(-0.494244053289945,0.235402452205118,
-2.56797502845164));
#66709=CARTESIAN_POINT('Ctrl Pts',(-0.546615726404821,-0.0300457378605709,
-2.55406539850588));
#66710=CARTESIAN_POINT('Ctrl Pts',(-0.465465774177804,-0.288154666430573,
-2.54015576856012));
#66711=CARTESIAN_POINT('Ctrl Pts',(-0.270616666022705,-0.475876159087017,
-2.52624613861436));
#66712=CARTESIAN_POINT('Ctrl Pts',(-0.00966412295619432,-0.547355554867349,
-2.5123365086686));
#66713=CARTESIAN_POINT('Ctrl Pts',(0.253649071921605,-0.485132607675433,
-2.49842687872285));
#66714=CARTESIAN_POINT('Ctrl Pts',(0.45500349994835,-0.304406494266152,
-2.48451724877709));
#66715=CARTESIAN_POINT('Ctrl Pts',(0.54521438798049,-0.049323116849169,
-2.47060761883133));
#66716=CARTESIAN_POINT('Ctrl Pts',(0.502245955099664,0.217808400441037,
-2.45669798888557));
#66717=CARTESIAN_POINT('Ctrl Pts',(0.33659408482971,0.431735938710581,-2.44278835893981));
#66718=CARTESIAN_POINT('Ctrl Pts',(0.0887224994730275,0.54020349573463,
-2.42887872899405));
#66719=CARTESIAN_POINT('Ctrl Pts',(-0.18082129866822,0.516715740678176,
-2.41496909904829));
#66720=CARTESIAN_POINT('Ctrl Pts',(-0.40619594373111,0.367010018954592,
-2.40105946910253));
#66721=CARTESIAN_POINT('Ctrl Pts',(-0.532349252863944,0.127654892941306,
-2.38714983915677));
#66722=CARTESIAN_POINT('Ctrl Pts',(-0.528465802975152,-0.142882447496131,
-2.37324020921101));
#66723=CARTESIAN_POINT('Ctrl Pts',(-0.395494202961323,-0.378517944278266,
-2.35933057926526));
#66724=CARTESIAN_POINT('Ctrl Pts',(-0.165915377355921,-0.52169300002348,
-2.3454209493195));
#66725=CARTESIAN_POINT('Ctrl Pts',(0.104191537332248,-0.537434295765537,
-2.33151131937374));
#66726=CARTESIAN_POINT('Ctrl Pts',(0.348847622965475,-0.421896710899712,
-2.31760168942798));
#66727=CARTESIAN_POINT('Ctrl Pts',(0.508290826193431,-0.203302569399051,
-2.30369205948222));
#66728=CARTESIAN_POINT('Ctrl Pts',(0.543574013561436,0.064952217031977,
-2.28978242953646));
#66729=CARTESIAN_POINT('Ctrl Pts',(0.446078573681184,0.317341148953642,
-2.27587279959071));
#66730=CARTESIAN_POINT('Ctrl Pts',(0.239619682310341,0.492213273455875,
-2.26196316964494));
#66731=CARTESIAN_POINT('Ctrl Pts',(-0.0253710219968334,0.546852640077282,
-2.24805353969918));
#66732=CARTESIAN_POINT('Ctrl Pts',(-0.284164355957781,0.467912510539904,
-2.23414390975342));
#66733=CARTESIAN_POINT('Ctrl Pts',(-0.473544965697884,0.274675561670212,
-2.22023427980767));
#66734=CARTESIAN_POINT('Ctrl Pts',(-0.547252918325985,0.0143437129206318,
-2.20632464986191));
#66735=CARTESIAN_POINT('Ctrl Pts',(-0.487283598972591,-0.249491869384507,
-2.19241501991615));
#66736=CARTESIAN_POINT('Ctrl Pts',(-0.308285691537408,-0.452384163195352,
-2.17850538997039));
#66737=CARTESIAN_POINT('Ctrl Pts',(-0.0539829499832726,-0.544772741450746,
-2.16459576002463));
#66738=CARTESIAN_POINT('Ctrl Pts',(0.213506187194575,-0.504089879630896,
-2.15068613007887));
#66739=CARTESIAN_POINT('Ctrl Pts',(0.428842245421929,-0.340273165645094,
-2.13677650013311));
#66740=CARTESIAN_POINT('Ctrl Pts',(0.539425163814452,-0.0933380488354483,
-2.12286687018735));
#66741=CARTESIAN_POINT('Ctrl Pts',(0.518242892982467,0.176396719328393,
-2.10895724024159));
#66742=CARTESIAN_POINT('Ctrl Pts',(0.370469618543577,0.403043124805315,
-2.09504761029584));
#66743=CARTESIAN_POINT('Ctrl Pts',(0.13220186467748,0.531238332288299,-2.08113798035007));
#66744=CARTESIAN_POINT('Ctrl Pts',(-0.138358790750498,0.529668144915963,
-2.06722835040432));
#66745=CARTESIAN_POINT('Ctrl Pts',(-0.375122594516613,0.398716111788552,
-2.05331872045856));
#66746=CARTESIAN_POINT('Ctrl Pts',(-0.52025533810128,0.170369838568274,
-2.0394090905128));
#66747=CARTESIAN_POINT('Ctrl Pts',(-0.538305498839373,-0.0995926133603777,
-2.02549946056704));
#66748=CARTESIAN_POINT('Ctrl Pts',(-0.424863970510547,-0.345227613725596,
-2.01158983062128));
#66749=CARTESIAN_POINT('Ctrl Pts',(-0.207641074117375,-0.506533990030323,
-1.99768020067552));
#66750=CARTESIAN_POINT('Ctrl Pts',(0.0603022321810123,-0.544109492207814,
-1.98377057072976));
#66751=CARTESIAN_POINT('Ctrl Pts',(0.313515534083973,-0.448775565962206,
-1.969860940784));
#66752=CARTESIAN_POINT('Ctrl Pts',(0.490146510124936,-0.243819394899179,
-1.95595131083825));
#66753=CARTESIAN_POINT('Ctrl Pts',(0.547049575814728,0.0206944513718702,
-1.94204168089249));
#66754=CARTESIAN_POINT('Ctrl Pts',(0.470325039924538,0.280153271508007,
-1.92813205094673));
#66755=CARTESIAN_POINT('Ctrl Pts',(0.278714377023783,0.471179153567835,
-1.91422242100097));
#66756=CARTESIAN_POINT('Ctrl Pts',(0.0190222542807834,0.547110274587066,
-1.90031279105521));
#66757=CARTESIAN_POINT('Ctrl Pts',(-0.245316427619855,0.489398967159197,
-1.88640316110945));
#66758=CARTESIAN_POINT('Ctrl Pts',(-0.449731754672463,0.312142351429414,
-1.87249353116369));
#66759=CARTESIAN_POINT('Ctrl Pts',(-0.544291269038013,0.0586388366668922,
-1.85858390121793));
#66760=CARTESIAN_POINT('Ctrl Pts',(-0.505896952420048,-0.209188365471801,
-1.84467427127217));
#66761=CARTESIAN_POINT('Ctrl Pts',(-0.343927370620985,-0.425917201407025,
-1.83076464132642));
#66762=CARTESIAN_POINT('Ctrl Pts',(-0.0979467746732575,-0.538607396948615,
-1.81685501138066));
#66763=CARTESIAN_POINT('Ctrl Pts',(0.171959244418416,-0.519732158881576,
-1.8029453814349));
#66764=CARTESIAN_POINT('Ctrl Pts',(0.399860841210855,-0.373902134766311,
-1.78903575148914));
#66765=CARTESIAN_POINT('Ctrl Pts',(0.530088575269402,-0.136739171730388,
-1.77512612154338));
#66766=CARTESIAN_POINT('Ctrl Pts',(0.530831765202846,0.133825019216465,
-1.76121649159762));
#66767=CARTESIAN_POINT('Ctrl Pts',(0.401908872275551,0.371699821230588,
-1.74730686165186));
#66768=CARTESIAN_POINT('Ctrl Pts',(0.174811844808601,0.518779642653092,
-1.7333972317061));
#66769=CARTESIAN_POINT('Ctrl Pts',(-0.0949864086208329,0.539137348821219,
-1.71948760176035));
#66770=CARTESIAN_POINT('Ctrl Pts',(-0.341582366448823,0.427800170228903,
-1.70557797181458));
#66771=CARTESIAN_POINT('Ctrl Pts',(-0.504740123447223,0.211964399131406,
-1.69166834186883));
#66772=CARTESIAN_POINT('Ctrl Pts',(-0.54460519345837,-0.0556478389052866,
-1.67775871192307));
#66773=CARTESIAN_POINT('Ctrl Pts',(-0.451439750281636,-0.309666999504807,
-1.66384908197731));
#66774=CARTESIAN_POINT('Ctrl Pts',(-0.248001282949535,-0.488043914388902,
-1.64993945203155));
#66775=CARTESIAN_POINT('Ctrl Pts',(0.0160163678687228,-0.547206519220075,
-1.63602982208579));
#66776=CARTESIAN_POINT('Ctrl Pts',(0.276121706313586,-0.472703185962534,
-1.62212019214003));
#66777=CARTESIAN_POINT('Ctrl Pts',(0.468778895650747,-0.282732816823804,
-1.60821056219427));
#66778=CARTESIAN_POINT('Ctrl Pts',(0.546927634078633,-0.0236994050095503,
-1.59430093224851));
#66779=CARTESIAN_POINT('Ctrl Pts',(0.491478557590205,0.241123051875402,
-1.58039130230275));
#66780=CARTESIAN_POINT('Ctrl Pts',(0.315976191999128,0.44704646828533,-1.56648167235699));
#66781=CARTESIAN_POINT('Ctrl Pts',(0.0632904365291062,0.543770005940573,
-1.55257204241124));
#66782=CARTESIAN_POINT('Ctrl Pts',(-0.204855250929235,0.507667041360159,
-1.53866241246548));
#66783=CARTESIAN_POINT('Ctrl Pts',(-0.422961020502676,0.347556432614895,
-1.52475278251972));
#66784=CARTESIAN_POINT('Ctrl Pts',(-0.537750254920378,0.10254834006324,
-1.51084315257396));
#66785=CARTESIAN_POINT('Ctrl Pts',(-0.521183429501975,-0.16750919834211,
-1.4969335226282));
#66786=CARTESIAN_POINT('Ctrl Pts',(-0.377307316686986,-0.396649325590153,
-1.48302389268244));
#66787=CARTESIAN_POINT('Ctrl Pts',(-0.141266482397949,-0.528900065860808,
-1.46911426273668));
#66788=CARTESIAN_POINT('Ctrl Pts',(0.129281464337643,-0.531956578768767,
-1.45520463279092));
#66789=CARTESIAN_POINT('Ctrl Pts',(0.368249874643727,-0.405072251013983,
-1.44129500284516));
#66790=CARTESIAN_POINT('Ctrl Pts',(0.517266021560369,-0.179241071341825,
-1.4273853728994));
#66791=CARTESIAN_POINT('Ctrl Pts',(0.539929784898266,0.0903732598525054,
-1.41347574295365));
#66792=CARTESIAN_POINT('Ctrl Pts',(0.430705095402437,0.337912147622774,
-1.39956611300789));
#66793=CARTESIAN_POINT('Ctrl Pts',(0.216272228382311,0.502909357585645,
-1.38565648306213));
#66794=CARTESIAN_POINT('Ctrl Pts',(-0.0509893774665488,0.545061081074617,
-1.37174685311637));
#66795=CARTESIAN_POINT('Ctrl Pts',(-0.305795826565191,0.454070931872949,
-1.35783722317061));
#66796=CARTESIAN_POINT('Ctrl Pts',(-0.485905639959076,0.252165040742401,
-1.34392759322485));
#66797=CARTESIAN_POINT('Ctrl Pts',(-0.547323458819898,-0.0113371134810136,
-1.33001796327909));
#66798=CARTESIAN_POINT('Ctrl Pts',(-0.475046774798344,-0.2720699551041,
-1.31610833333333));
#66799=CARTESIAN_POINT('Ctrl Pts',(-0.286730587300225,-0.466344367418676,
-1.30219870338757));
#66800=CARTESIAN_POINT('Ctrl Pts',(-0.0283748231814932,-0.54670501015271,
-1.28828907344181));
#66801=CARTESIAN_POINT('Ctrl Pts',(0.236912048709972,-0.493522218236121,
-1.27437944349606));
#66802=CARTESIAN_POINT('Ctrl Pts',(0.444328500343154,-0.319786932971721,
-1.2604698135503));
#66803=CARTESIAN_POINT('Ctrl Pts',(0.543208990265627,-0.0679374095123898,
-1.24656018360454));
#66804=CARTESIAN_POINT('Ctrl Pts',(0.509400017047994,0.20050716034137,-1.23265055365878));
#66805=CARTESIAN_POINT('Ctrl Pts',(0.351160086322446,0.419973918821954,
-1.21874092371302));
#66806=CARTESIAN_POINT('Ctrl Pts',(0.10714240860568,0.536853800391532,-1.20483129376726));
#66807=CARTESIAN_POINT('Ctrl Pts',(-0.163046906422306,0.522596598747804,
-1.1909216638215));
#66808=CARTESIAN_POINT('Ctrl Pts',(-0.393408812722661,0.38068491536808,
-1.17701203387574));
#66809=CARTESIAN_POINT('Ctrl Pts',(-0.527672890949092,0.14578346570885,
-1.16310240392999));
#66810=CARTESIAN_POINT('Ctrl Pts',(-0.533042503383665,-0.124728458272891,
-1.14919277398422));
#66811=CARTESIAN_POINT('Ctrl Pts',(-0.408206016743456,-0.364773006966111,
-1.13528314403847));
#66812=CARTESIAN_POINT('Ctrl Pts',(-0.183657194367116,-0.515714585477138,
-1.12137351409271));
#66813=CARTESIAN_POINT('Ctrl Pts',(0.085753504301945,-0.540682749139079,
-1.10746388414695));
#66814=CARTESIAN_POINT('Ctrl Pts',(0.334217225560628,-0.43357853366514,
-1.09355425420119));
#66815=CARTESIAN_POINT('Ctrl Pts',(0.501041826284635,-0.220564246944092,
-1.07964462425543));
#66816=CARTESIAN_POINT('Ctrl Pts',(0.545477121728666,0.0463271884239284,
-1.06573499430967));
#66817=CARTESIAN_POINT('Ctrl Pts',(0.456668918382307,0.301902298269141,
-1.05182536436391));
#66818=CARTESIAN_POINT('Ctrl Pts',(0.256310363884194,0.483731843155078,
-1.03791573441815));
#66819=CARTESIAN_POINT('Ctrl Pts',(-0.00665703028796617,0.547400386065266,
-1.02400610447239));
#66820=CARTESIAN_POINT('Ctrl Pts',(-0.267998314084843,0.477355635102738,
-1.01009647452664));
#66821=CARTESIAN_POINT('Ctrl Pts',(-0.463875746849021,0.290707396194043,
-0.996186844580877));
#66822=CARTESIAN_POINT('Ctrl Pts',(-0.546442419084335,0.0330481669978269,
-0.982277214635117));
#66823=CARTESIAN_POINT('Ctrl Pts',(-0.495529799694107,-0.232683725971057,
-0.968367584689358));
#66824=CARTESIAN_POINT('Ctrl Pts',(-0.323574295761076,-0.441578049544336,
-0.9544579547436));
#66825=CARTESIAN_POINT('Ctrl Pts',(-0.0725794158974647,-0.542608263026504,
-0.940548324797841));
#66826=CARTESIAN_POINT('Ctrl Pts',(0.196144411577539,-0.511095752793503,
-0.926638694852082));
#66827=CARTESIAN_POINT('Ctrl Pts',(0.416956114738421,-0.354738068296732,
-0.912729064906324));
#66828=CARTESIAN_POINT('Ctrl Pts',(0.535918098897834,-0.111728644448898,
-0.898819434960564));
#66829=CARTESIAN_POINT('Ctrl Pts',(0.523971563308618,0.158572694877081,
-0.884909805014805));
#66830=CARTESIAN_POINT('Ctrl Pts',(0.384034683888557,0.390139539507691,
-0.871000175069045));
#66831=CARTESIAN_POINT('Ctrl Pts',(0.150289791446776,0.526407140247491,
-0.857090545123288));
#66832=CARTESIAN_POINT('Ctrl Pts',(-0.120166333871985,0.534089459660479,
-0.843180915177528));
#66833=CARTESIAN_POINT('Ctrl Pts',(-0.361269472375872,0.411309940368472,
-0.82927128523177));
#66834=CARTESIAN_POINT('Ctrl Pts',(-0.514125447821904,0.188059891041614,
-0.815361655286009));
#66835=CARTESIAN_POINT('Ctrl Pts',(-0.541396186497834,-0.0811274796986776,
-0.801452025340252));
#66836=CARTESIAN_POINT('Ctrl Pts',(-0.436420274952878,-0.330497870381506,
-0.787542395394492));
#66837=CARTESIAN_POINT('Ctrl Pts',(-0.224840141046584,-0.499137666071003,
-0.773632765448734));
#66838=CARTESIAN_POINT('Ctrl Pts',(0.0416616126090963,-0.545853285005657,
-0.759723135502974));
#66839=CARTESIAN_POINT('Ctrl Pts',(0.297986699255,-0.459233519882606,-0.745813505557216));
#66840=CARTESIAN_POINT('Ctrl Pts',(0.481522682893413,-0.260436949328981,
-0.731903875611456));
#66841=CARTESIAN_POINT('Ctrl Pts',(0.547437295332376,0.00197646042940402,
-0.717994245665697));
#66842=CARTESIAN_POINT('Ctrl Pts',(0.47962959808533,0.263907080915161,-0.704084615719938));
#66843=CARTESIAN_POINT('Ctrl Pts',(0.294662952778667,0.461373214411515,
-0.69017498577418));
#66844=CARTESIAN_POINT('Ctrl Pts',(0.0377190948114364,0.546139880070356,
-0.67626535582842));
#66845=CARTESIAN_POINT('Ctrl Pts',(-0.228438392772295,0.497501155198928,
-0.662355725882662));
#66846=CARTESIAN_POINT('Ctrl Pts',(-0.438795316961955,0.327338003490144,
-0.648446095936902));
#66847=CARTESIAN_POINT('Ctrl Pts',(-0.541967868139668,0.077216116328137,
-0.634536465991144));
#66848=CARTESIAN_POINT('Ctrl Pts',(-0.512754124629076,-0.191767323578675,
-0.620626836045384));
#66849=CARTESIAN_POINT('Ctrl Pts',(-0.358290116967589,-0.413907828870158,
-0.606717206099626));
#66850=CARTESIAN_POINT('Ctrl Pts',(-0.11630671231382,-0.534943218844212,
-0.592807576153866));
#66851=CARTESIAN_POINT('Ctrl Pts',(0.154086890795909,-0.525308222666945,
-0.578897946208108));
#66852=CARTESIAN_POINT('Ctrl Pts',(0.386841744947087,-0.387356377361918,
-0.564988316262349));
#66853=CARTESIAN_POINT('Ctrl Pts',(0.525102906289336,-0.154785130174539,
-0.55107868631659));
#66854=CARTESIAN_POINT('Ctrl Pts',(0.535097371060952,0.115595424651308,
-0.537169056370831));
#66855=CARTESIAN_POINT('Ctrl Pts',(0.414383794975135,0.357739527000668,
-0.523259426425071));
#66856=CARTESIAN_POINT('Ctrl Pts',(0.19244883950397,0.51249872476937,-0.509349796479313));
#66857=CARTESIAN_POINT('Ctrl Pts',(-0.0764955242305444,0.542070044818335,
-0.495440166533554));
#66858=CARTESIAN_POINT('Ctrl Pts',(-0.326754353990724,0.439230111518734,
-0.481530536587795));
#66859=CARTESIAN_POINT('Ctrl Pts',(-0.497197016149334,0.229099598098419,
-0.467620906642036));
#66860=CARTESIAN_POINT('Ctrl Pts',(-0.54618954340598,-0.0369929911013041,
-0.453711276696277));
#66861=CARTESIAN_POINT('Ctrl Pts',(-0.46176454888738,-0.294049315774561,
-0.439801646750518));
#66862=CARTESIAN_POINT('Ctrl Pts',(-0.264544495400683,-0.479278320675863,
-0.425892016804759));
#66863=CARTESIAN_POINT('Ctrl Pts',(-0.00270425391930869,-0.547434183922904,
-0.411982386859));
#66864=CARTESIAN_POINT('Ctrl Pts',(0.259796554686738,-0.481868497507032,
-0.398072756913241));
#66865=CARTESIAN_POINT('Ctrl Pts',(0.458836953054976,-0.298596967880934,
-0.384163126967482));
#66866=CARTESIAN_POINT('Ctrl Pts',(0.545797415228185,-0.0423872651522121,
-0.370253497021723));
#66867=CARTESIAN_POINT('Ctrl Pts',(0.499436140633363,0.224176359471699,
-0.356343867075964));
#66868=CARTESIAN_POINT('Ctrl Pts',(0.331077781011755,0.435980506027487,
-0.342434237130205));
#66869=CARTESIAN_POINT('Ctrl Pts',(0.0818471718350033,0.541287852424598,
-0.328524607184445));
#66870=CARTESIAN_POINT('Ctrl Pts',(-0.187376216331818,0.514375011312576,
-0.314614977238687));
#66871=CARTESIAN_POINT('Ctrl Pts',(-0.410829284067798,0.36181597267254,
-0.300705347292928));
#66872=CARTESIAN_POINT('Ctrl Pts',(-0.533929231491555,0.120876277495512,
-0.28679571734717));
#66873=CARTESIAN_POINT('Ctrl Pts',(-0.526606479121654,-0.149589822070715,
-0.27288608740141));
#66874=CARTESIAN_POINT('Ctrl Pts',(-0.390649752922828,-0.383515670215699,
-0.258976457455652));
#66875=CARTESIAN_POINT('Ctrl Pts',(-0.159269153319243,-0.523760284249544,
-0.245066827509892));
#66876=CARTESIAN_POINT('Ctrl Pts',(0.111016064888819,-0.53606616423677,
-0.231157197564133));
#66877=CARTESIAN_POINT('Ctrl Pts',(0.354183428665716,-0.41742735519224,
-0.217247567618374));
#66878=CARTESIAN_POINT('Ctrl Pts',(0.51083453569749,-0.196823720178588,
-0.203337937672615));
#66879=CARTESIAN_POINT('Ctrl Pts',(0.542704273947877,0.0718579790208525,
-0.189428307726856));
#66880=CARTESIAN_POINT('Ctrl Pts',(0.442007839686807,0.322986945172268,
-0.175518677781097));
#66881=CARTESIAN_POINT('Ctrl Pts',(0.233342303313345,0.495220027940256,
-0.161609047835339));
#66882=CARTESIAN_POINT('Ctrl Pts',(-0.0323216585670542,0.546485853693586,
-0.14769941788958));
#66883=CARTESIAN_POINT('Ctrl Pts',(-0.290090448635031,0.464261856806131,
-0.133789787943821));
#66884=CARTESIAN_POINT('Ctrl Pts',(-0.476998895253674,0.2686326306232,-0.119880157998062));
#66885=CARTESIAN_POINT('Ctrl Pts',(-0.5473911015369,0.00738490965168814,
-0.105970528052302));
#66886=CARTESIAN_POINT('Ctrl Pts',(-0.484072073042989,-0.255667307605576,
-0.0920608981065435));
#66887=CARTESIAN_POINT('Ctrl Pts',(-0.302509342715061,-0.456266617395285,
-0.0781512681607847));
#66888=CARTESIAN_POINT('Ctrl Pts',(-0.0470519678878475,-0.545416086573125,
-0.0642416382150256));
#66889=CARTESIAN_POINT('Ctrl Pts',(0.219897217017238,-0.501332588518456,
-0.0503320082692668));
#66890=CARTESIAN_POINT('Ctrl Pts',(0.433135230583494,-0.334797314980531,
-0.0364223783235079));
#66891=CARTESIAN_POINT('Ctrl Pts',(0.540565512147126,-0.0864644858093628,
-0.0225127483777489));
#66892=CARTESIAN_POINT('Ctrl Pts',(0.515963701837572,0.18295602369734,-0.00860311843199006));
#66893=CARTESIAN_POINT('Ctrl Pts',(0.365304511527139,0.407753219468906,
0.00530651151376877));
#66894=CARTESIAN_POINT('Ctrl Pts',(0.205409024163764,0.491108180259118,
0.0145795981442749));
#66895=CARTESIAN_POINT('Ctrl Pts',(0.120319876696228,0.511137837581914,
0.0192161414595281));
#66896=CARTESIAN_POINT('Ctrl Pts',(-0.243856727558445,0.502329722221634,
-3.96754114145953));
#66897=CARTESIAN_POINT('Ctrl Pts',(-0.327479587516629,0.461734877687463,
-3.96290459814427));
#66898=CARTESIAN_POINT('Ctrl Pts',(-0.473974953282714,0.33801685956352,
-3.95363151151377));
#66899=CARTESIAN_POINT('Ctrl Pts',(-0.577952945034314,0.0696920735605909,
-3.93972188156801));
#66900=CARTESIAN_POINT('Ctrl Pts',(-0.540746265833271,-0.215581171713082,
-3.92581225162225));
#66901=CARTESIAN_POINT('Ctrl Pts',(-0.371456103433689,-0.448231402072954,
-3.9119026216765));
#66902=CARTESIAN_POINT('Ctrl Pts',(-0.111428220693573,-0.571373559976427,
-3.89799299173073));
#66903=CARTESIAN_POINT('Ctrl Pts',(0.175817028445578,-0.554956089486103,
-3.88408336178498));
#66904=CARTESIAN_POINT('Ctrl Pts',(0.420116112083225,-0.402974791659343,
-3.87017373183921));
#66905=CARTESIAN_POINT('Ctrl Pts',(0.56179328006591,-0.152561497953608,
-3.85626410189346));
#66906=CARTESIAN_POINT('Ctrl Pts',(0.566241563426747,0.135119222564917,
-3.8423544719477));
#66907=CARTESIAN_POINT('Ctrl Pts',(0.432374145368927,0.389793761798776,
-3.82844484200194));
#66908=CARTESIAN_POINT('Ctrl Pts',(0.192890892497521,0.549253856835642,
-3.81453521205618));
#66909=CARTESIAN_POINT('Ctrl Pts',(-0.0937097697185672,0.574547739017817,
-3.80062558211042));
#66910=CARTESIAN_POINT('Ctrl Pts',(-0.357419969727719,0.45949714148416,
-3.78671595216466));
#66911=CARTESIAN_POINT('Ctrl Pts',(-0.533823328786559,0.232205298608011,
-3.7728063222189));
#66912=CARTESIAN_POINT('Ctrl Pts',(-0.579829854021713,-0.0518072252693176,
-3.75889669227314));
#66913=CARTESIAN_POINT('Ctrl Pts',(-0.48420155244083,-0.323164828842655,
-3.74498706232738));
#66914=CARTESIAN_POINT('Ctrl Pts',(-0.27029751243075,-0.515583070764315,
-3.73107743238163));
#66915=CARTESIAN_POINT('Ctrl Pts',(0.00963200258153823,-0.582060025988483,
-3.71716780243587));
#66916=CARTESIAN_POINT('Ctrl Pts',(0.287208712007788,-0.506357388072924,
-3.70325817249011));
#66917=CARTESIAN_POINT('Ctrl Pts',(0.494629053365649,-0.306967015338603,
-3.68934854254435));
#66918=CARTESIAN_POINT('Ctrl Pts',(0.581226535210402,-0.0325939206265673,
-3.67543891259859));
#66919=CARTESIAN_POINT('Ctrl Pts',(0.525848021966783,0.249740879048841,
-3.66152928265284));
#66920=CARTESIAN_POINT('Ctrl Pts',(0.342020803029351,0.471071564838469,
-3.64761965270707));
#66921=CARTESIAN_POINT('Ctrl Pts',(0.0746482865109549,0.577333770191651,
-3.63371002276131));
#66922=CARTESIAN_POINT('Ctrl Pts',(-0.210958539890159,0.542570864810902,
-3.61980039281555));
#66923=CARTESIAN_POINT('Ctrl Pts',(-0.445034600226093,0.37527437094894,
-3.6058907628698));
#66924=CARTESIAN_POINT('Ctrl Pts',(-0.570402220087964,0.116309742538902,
-3.59198113292404));
#66925=CARTESIAN_POINT('Ctrl Pts',(-0.556437896418977,-0.171065824522912,
-3.57807150297827));
#66926=CARTESIAN_POINT('Ctrl Pts',(-0.406552689499017,-0.416655204637545,
-3.56416187303252));
#66927=CARTESIAN_POINT('Ctrl Pts',(-0.157359004489718,-0.560468368952972,
-3.55025224308676));
#66928=CARTESIAN_POINT('Ctrl Pts',(0.13027270750405,-0.567376127952309,
-3.536342613141));
#66929=CARTESIAN_POINT('Ctrl Pts',(0.386082752459345,-0.435691125849609,
-3.52243298319524));
#66930=CARTESIAN_POINT('Ctrl Pts',(0.547584503425569,-0.197580010372577,
-3.50852335324949));
#66931=CARTESIAN_POINT('Ctrl Pts',(0.575327986238213,0.0887939026157717,
-3.49461372330372));
#66932=CARTESIAN_POINT('Ctrl Pts',(0.462536310407596,0.353478161199798,
-3.48070409335796));
#66933=CARTESIAN_POINT('Ctrl Pts',(0.236761057702121,0.531818437482596,
-3.46679446341221));
#66934=CARTESIAN_POINT('Ctrl Pts',(-0.046847732742882,0.580251616824556,
-3.45288483346644));
#66935=CARTESIAN_POINT('Ctrl Pts',(-0.319013044492984,0.486946944064727,
-3.43897520352069));
#66936=CARTESIAN_POINT('Ctrl Pts',(-0.513253155506318,0.274695917795417,
-3.42506557357493));
#66937=CARTESIAN_POINT('Ctrl Pts',(-0.582121104277277,-0.00465498073710868,
-3.41115594362916));
#66938=CARTESIAN_POINT('Ctrl Pts',(-0.508794541924058,-0.2828688088124,
-3.39724631368342));
#66939=CARTESIAN_POINT('Ctrl Pts',(-0.311184921251967,-0.491986375498414,
-3.38333668373764));
#66940=CARTESIAN_POINT('Ctrl Pts',(-0.0375622726695128,-0.580926608585422,
-3.3694270537919));
#66941=CARTESIAN_POINT('Ctrl Pts',(0.24523569864168,-0.527964109577901,
-3.35551742384613));
#66942=CARTESIAN_POINT('Ctrl Pts',(0.468130034743078,-0.346036008909629,
-3.34160779390038));
#66943=CARTESIAN_POINT('Ctrl Pts',(0.576674416953902,-0.0795818177823006,
-3.32769816395461));
#66944=CARTESIAN_POINT('Ctrl Pts',(0.544354748378621,0.206311795126474,
-3.31378853400886));
#66945=CARTESIAN_POINT('Ctrl Pts',(0.379065742744303,0.441809700627282,
-3.2998789040631));
#66946=CARTESIAN_POINT('Ctrl Pts',(0.121182485540343,0.569386910710919,
-3.28596927411734));
#66947=CARTESIAN_POINT('Ctrl Pts',(-0.166301973478169,0.557880186516715,
-3.27205964417158));
#66948=CARTESIAN_POINT('Ctrl Pts',(-0.413163909719271,0.41010027139243,
-3.25815001422582));
#66949=CARTESIAN_POINT('Ctrl Pts',(-0.559102447504268,0.162145311635571,
-3.24424038428006));
#66950=CARTESIAN_POINT('Ctrl Pts',(-0.568469233110817,-0.125416824617188,
-3.2303307543343));
#66951=CARTESIAN_POINT('Ctrl Pts',(-0.438976245214247,-0.382343438584031,
-3.21642112438855));
#66952=CARTESIAN_POINT('Ctrl Pts',(-0.202254689027127,-0.545875159406616,
-3.20251149444278));
#66953=CARTESIAN_POINT('Ctrl Pts',(0.0838715467317631,-0.576066152919507,
-3.18860186449702));
#66954=CARTESIAN_POINT('Ctrl Pts',(0.349510510173741,-0.465541676081477,
-3.17469223455127));
#66955=CARTESIAN_POINT('Ctrl Pts',(0.529774667992378,-0.241299502784869,
-3.16078260460551));
#66956=CARTESIAN_POINT('Ctrl Pts',(0.580630959702681,0.0418848125864526,
-3.14687297465975));
#66957=CARTESIAN_POINT('Ctrl Pts',(0.489656737363871,0.314837939970435,
-3.13296334471399));
#66958=CARTESIAN_POINT('Ctrl Pts',(0.279074241288692,0.51088571788591,-3.11905371476823));
#66959=CARTESIAN_POINT('Ctrl Pts',(0.000322381457725726,0.582139626688352,
-3.10514408482247));
#66960=CARTESIAN_POINT('Ctrl Pts',(-0.278508226375054,0.511194499903981,
-3.09123445487671));
#66961=CARTESIAN_POINT('Ctrl Pts',(-0.489307730709825,0.315380077934957,
-3.07732482493096));
#66962=CARTESIAN_POINT('Ctrl Pts',(-0.580584213037096,0.0425278786533559,
-3.06341519498519));
#66963=CARTESIAN_POINT('Ctrl Pts',(-0.530041600106311,-0.240712590130639,
-3.04950556503944));
#66964=CARTESIAN_POINT('Ctrl Pts',(-0.350025917656482,-0.465154281781214,
-3.03559593509368));
#66965=CARTESIAN_POINT('Ctrl Pts',(-0.0845095311843385,-0.575972905638505,
-3.02168630514792));
#66966=CARTESIAN_POINT('Ctrl Pts',(0.20164996783568,-0.546098836624404,
-3.00777667520216));
#66967=CARTESIAN_POINT('Ctrl Pts',(0.438552502310153,-0.382829402747702,
-2.9938670452564));
#66968=CARTESIAN_POINT('Ctrl Pts',(0.568329976019654,-0.126046369436643,
-2.97995741531064));
#66969=CARTESIAN_POINT('Ctrl Pts',(0.559281692505214,0.161525964845169,
-2.96604778536488));
#66970=CARTESIAN_POINT('Ctrl Pts',(0.413617872700921,0.409642410247063,
-2.95213815541912));
#66971=CARTESIAN_POINT('Ctrl Pts',(0.166919765067557,0.557695652592388,
-2.93822852547337));
#66972=CARTESIAN_POINT('Ctrl Pts',(-0.120551773070811,0.569520780042436,
-2.9243188955276));
#66973=CARTESIAN_POINT('Ctrl Pts',(-0.378576173300926,0.442229273001557,
-2.91040926558185));
#66974=CARTESIAN_POINT('Ctrl Pts',(-0.544125908911863,0.206914581751741,
-2.89649963563609));
#66975=CARTESIAN_POINT('Ctrl Pts',(-0.576762205997358,-0.0789430593764874,
-2.88259000569033));
#66976=CARTESIAN_POINT('Ctrl Pts',(-0.468513008098925,-0.34551730800751,
-2.86868037574457));
#66977=CARTESIAN_POINT('Ctrl Pts',(-0.245820307547111,-0.527692169060811,
-2.85477074579881));
#66978=CARTESIAN_POINT('Ctrl Pts',(0.0369188304199093,-0.580967855264889,
-2.84086111585305));
#66979=CARTESIAN_POINT('Ctrl Pts',(0.310639819063253,-0.492330734062996,
-2.82695148590729));
#66980=CARTESIAN_POINT('Ctrl Pts',(0.508480931710273,-0.283432162920356,
-2.81304185596153));
#66981=CARTESIAN_POINT('Ctrl Pts',(0.582115591491657,-0.00529972008470409,
-2.79913222601578));
#66982=CARTESIAN_POINT('Ctrl Pts',(0.513557086755012,0.274127283454903,
-2.78522259607001));
#66983=CARTESIAN_POINT('Ctrl Pts',(0.319552178600044,0.486593314835525,
-2.77131296612426));
#66984=CARTESIAN_POINT('Ctrl Pts',(0.047490375615416,0.58019937359029,-2.75740333617849));
#66985=CARTESIAN_POINT('Ctrl Pts',(-0.236171884205633,0.532080341679168,
-2.74349370623274));
#66986=CARTESIAN_POINT('Ctrl Pts',(-0.462144523483567,0.353990237584042,
-2.72958407628697));
#66987=CARTESIAN_POINT('Ctrl Pts',(-0.575229287536554,0.0894310664749516,
-2.71567444634122));
#66988=CARTESIAN_POINT('Ctrl Pts',(-0.547803002042353,-0.196973398823406,
-2.70176481639546));
#66989=CARTESIAN_POINT('Ctrl Pts',(-0.386565075816664,-0.435263243393599,
-2.6878551864497));
#66990=CARTESIAN_POINT('Ctrl Pts',(-0.130901038650237,-0.567231493282018,
-2.67394555650394));
#66991=CARTESIAN_POINT('Ctrl Pts',(0.156738147775943,-0.560642311926621,
-2.66003592655819));
#66992=CARTESIAN_POINT('Ctrl Pts',(0.406090963662131,-0.417105236268524,
-2.64612629661242));
#66993=CARTESIAN_POINT('Ctrl Pts',(0.55624808706166,-0.171682015746856,
-2.63221666666667));
#66994=CARTESIAN_POINT('Ctrl Pts',(0.570530691873357,0.115677908526938,
-2.61830703672091));
#66995=CARTESIAN_POINT('Ctrl Pts',(0.445449971397287,0.374781232017847,
-2.60439740677515));
#66996=CARTESIAN_POINT('Ctrl Pts',(0.211559347882646,0.54233687982114,-2.59048777682939));
#66997=CARTESIAN_POINT('Ctrl Pts',(-0.0740088008494859,0.57741609458646,
-2.57657814688363));
#66998=CARTESIAN_POINT('Ctrl Pts',(-0.341498846626141,0.471450089239226,
-2.56266851693787));
#66999=CARTESIAN_POINT('Ctrl Pts',(-0.52557109293002,0.250323141493158,
-2.54875888699211));
#67000=CARTESIAN_POINT('Ctrl Pts',(-0.58126227888226,-0.0319501492838499,
-2.53484925704635));
#67001=CARTESIAN_POINT('Ctrl Pts',(-0.494968738678243,-0.306418988677151,
-2.5209396271006));
#67002=CARTESIAN_POINT('Ctrl Pts',(-0.287769364102383,-0.506038972782501,
-2.50702999715484));
#67003=CARTESIAN_POINT('Ctrl Pts',(-0.0102766712730032,-0.582049000444297,
-2.49312036720908));
#67004=CARTESIAN_POINT('Ctrl Pts',(0.269726300322964,-0.515882129759062,
-2.47921073726332));
#67005=CARTESIAN_POINT('Ctrl Pts',(0.483843326314238,-0.323700918243729,
-2.46530110731756));
#67006=CARTESIAN_POINT('Ctrl Pts',(0.579772118378885,-0.0524494007698775,
-2.4513914773718));
#67007=CARTESIAN_POINT('Ctrl Pts',(0.534080185253253,0.231613912817236,
-2.43748184742604));
#67008=CARTESIAN_POINT('Ctrl Pts',(0.357928678878714,0.459100979880023,
-2.42357221748028));
#67009=CARTESIAN_POINT('Ctrl Pts',(0.0943460638628411,0.574443617010623,
-2.40966258753452));
#67010=CARTESIAN_POINT('Ctrl Pts',(-0.192282429972567,0.549467120048602,
-2.39575295758877));
#67011=CARTESIAN_POINT('Ctrl Pts',(-0.431942164340539,0.390272488852942,
-2.381843327643));
#67012=CARTESIAN_POINT('Ctrl Pts',(-0.566091542803142,0.135746138278104,
-2.36793369769725));
#67013=CARTESIAN_POINT('Ctrl Pts',(-0.561961945312173,-0.151938872286246,
-2.35402406775148));
#67014=CARTESIAN_POINT('Ctrl Pts',(-0.420562107149786,-0.402509829594746,
-2.34011443780573));
#67015=CARTESIAN_POINT('Ctrl Pts',(-0.176431715526768,-0.554759856737075,
-2.32620480785997));
#67016=CARTESIAN_POINT('Ctrl Pts',(0.110795587291858,-0.571498894773481,
-2.31229517791421));
#67017=CARTESIAN_POINT('Ctrl Pts',(0.370958892165863,-0.448638104950677,
-2.29838554796845));
#67018=CARTESIAN_POINT('Ctrl Pts',(0.540508202922305,-0.216188647861906,
-2.28447591802269));
#67019=CARTESIAN_POINT('Ctrl Pts',(0.578027770883962,0.0690691318721798,
-2.27056628807693));
#67020=CARTESIAN_POINT('Ctrl Pts',(0.474352704785602,0.337455419801257,
-2.25665665813117));
#67021=CARTESIAN_POINT('Ctrl Pts',(0.254807675441085,0.523411594662337,
-2.24274702818541));
#67022=CARTESIAN_POINT('Ctrl Pts',(-0.0269791324161961,0.581514209030809,
-2.22883739823966));
#67023=CARTESIAN_POINT('Ctrl Pts',(-0.302175757378049,0.497570558356965,
-2.2149277682939));
#67024=CARTESIAN_POINT('Ctrl Pts',(-0.503560019623222,0.292085527761509,
-2.20101813834814));
#67025=CARTESIAN_POINT('Ctrl Pts',(-0.581939858414442,0.0152528711801189,
-2.18710850840238));
#67026=CARTESIAN_POINT('Ctrl Pts',(-0.518169458942701,-0.265305598715306,
-2.17319887845662));
#67027=CARTESIAN_POINT('Ctrl Pts',(-0.327825993570329,-0.481057966185246,
-2.15928924851086));
#67028=CARTESIAN_POINT('Ctrl Pts',(-0.0574045915847395,-0.579302478637584,
-2.1453796185651));
#67029=CARTESIAN_POINT('Ctrl Pts',(0.227039009178215,-0.536040984629006,
-2.13146998861935));
#67030=CARTESIAN_POINT('Ctrl Pts',(0.456023873470351,-0.361840953618791,
-2.11756035867358));
#67031=CARTESIAN_POINT('Ctrl Pts',(0.573615951497547,-0.0992541640346744,
-2.10365072872783));
#67032=CARTESIAN_POINT('Ctrl Pts',(0.551091068986974,0.187577404218774,
-2.08974109878207));
#67033=CARTESIAN_POINT('Ctrl Pts',(0.393951370824267,0.428589507940103,
-2.07583146883631));
#67034=CARTESIAN_POINT('Ctrl Pts',(0.140581314116832,0.564910207919669,
-2.06192183889055));
#67035=CARTESIAN_POINT('Ctrl Pts',(-0.147128489229501,0.56324049618942,
-2.04801220894479));
#67036=CARTESIAN_POINT('Ctrl Pts',(-0.398899269845503,0.423988232628435,
-2.03410257899903));
#67037=CARTESIAN_POINT('Ctrl Pts',(-0.553231070416462,0.181168517178112,
-2.02019294905327));
#67038=CARTESIAN_POINT('Ctrl Pts',(-0.572425317961847,-0.105905166290112,
-2.00628331910751));
#67039=CARTESIAN_POINT('Ctrl Pts',(-0.451793440591628,-0.367109433179042,
-1.99237368916175));
#67040=CARTESIAN_POINT('Ctrl Pts',(-0.220802143262232,-0.538640011901701,
-1.97846405921599));
#67041=CARTESIAN_POINT('Ctrl Pts',(0.0641244135615362,-0.578597190172963,
-1.96455442927024));
#67042=CARTESIAN_POINT('Ctrl Pts',(0.333387323129587,-0.477220642540898,
-1.95064479932448));
#67043=CARTESIAN_POINT('Ctrl Pts',(0.521213832128952,-0.259273581546812,
-1.93673516937872));
#67044=CARTESIAN_POINT('Ctrl Pts',(0.581723627293058,0.0220061432256019,
-1.92282553943296));
#67045=CARTESIAN_POINT('Ctrl Pts',(0.500136002891841,0.297910435369479,
-1.9089159094872));
#67046=CARTESIAN_POINT('Ctrl Pts',(0.296380338362444,0.501044253457539,
-1.89500627954144));
#67047=CARTESIAN_POINT('Ctrl Pts',(0.0202279560184803,0.581788173380976,
-1.88109664959568));
#67048=CARTESIAN_POINT('Ctrl Pts',(-0.260865501809525,0.52041890708959,
-1.86718701964992));
#67049=CARTESIAN_POINT('Ctrl Pts',(-0.478237438073695,0.331927103014152,
-1.85327738970416));
#67050=CARTESIAN_POINT('Ctrl Pts',(-0.578790488699635,0.0623555858083014,
-1.8393677597584));
#67051=CARTESIAN_POINT('Ctrl Pts',(-0.537962596461209,-0.22244750773918,
-1.82545812981265));
#67052=CARTESIAN_POINT('Ctrl Pts',(-0.365726775795477,-0.452913429207948,
-1.81154849986689));
#67053=CARTESIAN_POINT('Ctrl Pts',(-0.104155008181343,-0.572746351504227,
-1.79763886992113));
#67054=CARTESIAN_POINT('Ctrl Pts',(0.182858665525284,-0.552674730137874,
-1.78372923997537));
#67055=CARTESIAN_POINT('Ctrl Pts',(0.425205519289921,-0.397601452784128,
-1.76981961002961));
#67056=CARTESIAN_POINT('Ctrl Pts',(0.56368757499368,-0.145406212688464,
-1.75590998008385));
#67057=CARTESIAN_POINT('Ctrl Pts',(0.564477871089254,0.142307350271176,
-1.74200035013809));
#67058=CARTESIAN_POINT('Ctrl Pts',(0.427383362235855,0.395259548366178,
-1.72809072019233));
#67059=CARTESIAN_POINT('Ctrl Pts',(0.185892074414644,0.551661839862501,
-1.71418109024657));
#67060=CARTESIAN_POINT('Ctrl Pts',(-0.101007003038359,0.573309893711828,
-1.70027146030082));
#67061=CARTESIAN_POINT('Ctrl Pts',(-0.363233136474001,0.454915747647758,
-1.68636183035506));
#67062=CARTESIAN_POINT('Ctrl Pts',(-0.536732443334361,0.225399496811739,
-1.6724522004093));
#67063=CARTESIAN_POINT('Ctrl Pts',(-0.579124310825782,-0.0591750074036544,
-1.65854257046354));
#67064=CARTESIAN_POINT('Ctrl Pts',(-0.48005369284309,-0.329294854011373,
-1.64463294051778));
#67065=CARTESIAN_POINT('Ctrl Pts',(-0.263720533328036,-0.518977965998399,
-1.63072331057202));
#67066=CARTESIAN_POINT('Ctrl Pts',(0.017031545264937,-0.581890518359379,
-1.61681368062626));
#67067=CARTESIAN_POINT('Ctrl Pts',(0.293623334469941,-0.502664884734763,
-1.6029040506805));
#67068=CARTESIAN_POINT('Ctrl Pts',(0.498491858201794,-0.300653481930913,
-1.58899442073474));
#67069=CARTESIAN_POINT('Ctrl Pts',(0.581593956432909,-0.0252015620820308,
-1.57508479078899));
#67070=CARTESIAN_POINT('Ctrl Pts',(0.522630309752701,0.256406334201118,
-1.56117516084322));
#67071=CARTESIAN_POINT('Ctrl Pts',(0.336003946761551,0.475381948175695,
-1.54726553089747));
#67072=CARTESIAN_POINT('Ctrl Pts',(0.0673020214956575,0.578236185994319,
-1.53335590095171));
#67073=CARTESIAN_POINT('Ctrl Pts',(-0.217839744164144,0.539844880269471,
-1.51944627100595));
#67074=CARTESIAN_POINT('Ctrl Pts',(-0.449769874483405,0.369585861333793,
-1.50553664106019));
#67075=CARTESIAN_POINT('Ctrl Pts',(-0.571834880603205,0.109048238024178,
-1.49162701111443));
#67076=CARTESIAN_POINT('Ctrl Pts',(-0.554217987726959,-0.17812655885785,
-1.47771738116867));
#67077=CARTESIAN_POINT('Ctrl Pts',(-0.401222467891465,-0.421790445778163,
-1.46380775122291));
#67078=CARTESIAN_POINT('Ctrl Pts',(-0.150220481266396,-0.562423733406362,
-1.44989812127715));
#67079=CARTESIAN_POINT('Ctrl Pts',(0.137475807863018,-0.565673979552772,
-1.4359884913314));
#67080=CARTESIAN_POINT('Ctrl Pts',(0.391590931240414,-0.430747247769412,
-1.42207886138564));
#67081=CARTESIAN_POINT('Ctrl Pts',(0.550052279794577,-0.190602041918361,
-1.40816923143988));
#67082=CARTESIAN_POINT('Ctrl Pts',(0.574152557356071,0.0961014556192658,
-1.39425960149412));
#67083=CARTESIAN_POINT('Ctrl Pts',(0.458004797861252,0.359330285429343,
-1.38034997154836));
#67084=CARTESIAN_POINT('Ctrl Pts',(0.229980372418605,0.534785636674041,
-1.3664403416026));
#67085=CARTESIAN_POINT('Ctrl Pts',(-0.05422127522735,0.579609094306998,
-1.35253071165684));
#67086=CARTESIAN_POINT('Ctrl Pts',(-0.325178311628612,0.482851648580621,
-1.33862108171108));
#67087=CARTESIAN_POINT('Ctrl Pts',(-0.516704159724784,0.26814820568813,
-1.32471145176532));
#67088=CARTESIAN_POINT('Ctrl Pts',(-0.582014870029119,-0.01205570220466,
-1.31080182181956));
#67089=CARTESIAN_POINT('Ctrl Pts',(-0.505157019010565,-0.289314768090083,
-1.2968921918738));
#67090=CARTESIAN_POINT('Ctrl Pts',(-0.304904646076622,-0.495903020450117,
-1.28298256192805));
#67091=CARTESIAN_POINT('Ctrl Pts',(-0.0301733257728146,-0.581357221768566,
-1.26907293198229));
#67092=CARTESIAN_POINT('Ctrl Pts',(0.251928421879756,-0.524803505266338,
-1.25516330203653));
#67093=CARTESIAN_POINT('Ctrl Pts',(0.472491705243263,-0.340056226772827,
-1.24125367209077));
#67094=CARTESIAN_POINT('Ctrl Pts',(0.577639611044211,-0.0722435370351632,
-1.22734404214501));
#67095=CARTESIAN_POINT('Ctrl Pts',(0.541687698448494,0.213216055305955,
-1.21343441219925));
#67096=CARTESIAN_POINT('Ctrl Pts',(0.373417928113377,0.446593439107845,
-1.19952478225349));
#67097=CARTESIAN_POINT('Ctrl Pts',(0.113933495841189,0.570881605428012,
-1.18561515230773));
#67098=CARTESIAN_POINT('Ctrl Pts',(-0.173381430159482,0.555720728933618,
-1.17170552236198));
#67099=CARTESIAN_POINT('Ctrl Pts',(-0.418344537065485,0.404814151430164,
-1.15779589241621));
#67100=CARTESIAN_POINT('Ctrl Pts',(-0.561118775551487,0.155023767901115,
-1.14388626247046));
#67101=CARTESIAN_POINT('Ctrl Pts',(-0.566828734137865,-0.132634215217362,
-1.1299766325247));
#67102=CARTESIAN_POINT('Ctrl Pts',(-0.434079643310568,-0.387893686664309,
-1.11606700257894));
#67103=CARTESIAN_POINT('Ctrl Pts',(-0.195298075364724,-0.548402507880383,
-1.10215737263318));
#67104=CARTESIAN_POINT('Ctrl Pts',(0.091188882655331,-0.574953247291231,
-1.08824774268742));
#67105=CARTESIAN_POINT('Ctrl Pts',(0.35540116536494,-0.461060365405552,
-1.07433811274166));
#67106=CARTESIAN_POINT('Ctrl Pts',(0.532799734243006,-0.23454443519564,
-1.0604284827959));
#67107=CARTESIAN_POINT('Ctrl Pts',(0.580051505176277,0.0492635791776641,
-1.04651885285014));
#67108=CARTESIAN_POINT('Ctrl Pts',(0.48561430520755,0.321037996923179,-1.03260922290439));
#67109=CARTESIAN_POINT('Ctrl Pts',(0.272556274939904,0.514392579535847,
-1.01869959295862));
#67110=CARTESIAN_POINT('Ctrl Pts',(-0.00707897780625726,0.582096673211485,
-1.00478996301287));
#67111=CARTESIAN_POINT('Ctrl Pts',(-0.284985051209799,0.507612223530529,
-0.990880333067108));
#67112=CARTESIAN_POINT('Ctrl Pts',(-0.493277929460783,0.309133520016096,
-0.976970703121349));
#67113=CARTESIAN_POINT('Ctrl Pts',(-0.581077986694556,0.03514288362756,
-0.96306107317559));
#67114=CARTESIAN_POINT('Ctrl Pts',(-0.526938334757956,-0.247432092205459,
-0.94915144322983));
#67115=CARTESIAN_POINT('Ctrl Pts',(-0.344083646804031,-0.469566920569047,
-0.935241813284073));
#67116=CARTESIAN_POINT('Ctrl Pts',(-0.0771797711748603,-0.577000807462221,
-0.921332183338313));
#67117=CARTESIAN_POINT('Ctrl Pts',(0.208576779181695,-0.543490916278138,
-0.907422553392554));
#67118=CARTESIAN_POINT('Ctrl Pts',(0.443384355296167,-0.377222695989068,
-0.893512923446795));
#67119=CARTESIAN_POINT('Ctrl Pts',(0.569886595668309,-0.118810424493158,
-0.879603293501035));
#67120=CARTESIAN_POINT('Ctrl Pts',(0.557182843899205,0.168623626325179,
-0.865693663555278));
#67121=CARTESIAN_POINT('Ctrl Pts',(0.408376240828409,0.414868045066761,
-0.851784033609518));
#67122=CARTESIAN_POINT('Ctrl Pts',(0.159815721445959,0.559772796828648,
-0.837874403663759));
#67123=CARTESIAN_POINT('Ctrl Pts',(-0.127782926281245,0.567942050425623,
-0.823964773718));
#67124=CARTESIAN_POINT('Ctrl Pts',(-0.384168084926761,0.437380305242891,
-0.810055143772241));
#67125=CARTESIAN_POINT('Ctrl Pts',(-0.546712644727315,0.199979831447884,
-0.796145513826482));
#67126=CARTESIAN_POINT('Ctrl Pts',(-0.57571190498247,-0.0862696432826438,
-0.782235883880722));
#67127=CARTESIAN_POINT('Ctrl Pts',(-0.46408222690187,-0.351446063521076,
-0.768326253934965));
#67128=CARTESIAN_POINT('Ctrl Pts',(-0.23909135148475,-0.530774881221648,
-0.754416623989205));
#67129=CARTESIAN_POINT('Ctrl Pts',(0.044302281689456,-0.58045151109095,
-0.740506994043447));
#67130=CARTESIAN_POINT('Ctrl Pts',(0.316874212574861,-0.488341460758475,
-0.726597364097687));
#67131=CARTESIAN_POINT('Ctrl Pts',(0.512043394420817,-0.276944418829243,
-0.712687734151928));
#67132=CARTESIAN_POINT('Ctrl Pts',(0.582135921926214,0.00210173589565668,
-0.698778104206169));
#67133=CARTESIAN_POINT('Ctrl Pts',(0.510030318805702,0.280634500355199,
-0.684868474260411));
#67134=CARTESIAN_POINT('Ctrl Pts',(0.313339794595404,0.490616777142373,
-0.670958844314651));
#67135=CARTESIAN_POINT('Ctrl Pts',(0.0401098723442771,0.580756271624496,
-0.657049214368893));
#67136=CARTESIAN_POINT('Ctrl Pts',(-0.242917673884644,0.529034642159786,
-0.643139584423133));
#67137=CARTESIAN_POINT('Ctrl Pts',(-0.46660780797089,0.348085912428613,
-0.629229954477375));
#67138=CARTESIAN_POINT('Ctrl Pts',(-0.576319821948403,0.0821103630488868,
-0.615320324531615));
#67139=CARTESIAN_POINT('Ctrl Pts',(-0.54525440193326,-0.203922254947967,
-0.601410694585856));
#67140=CARTESIAN_POINT('Ctrl Pts',(-0.380999886811408,-0.440142857650052,
-0.587501064640097));
#67141=CARTESIAN_POINT('Ctrl Pts',(-0.123678667449767,-0.568849924064782,
-0.573591434694338));
#67142=CARTESIAN_POINT('Ctrl Pts',(0.163853495176574,-0.558604225735071,
-0.55968180474858));
#67143=CARTESIAN_POINT('Ctrl Pts',(0.411361223932671,-0.411908475677878,
-0.545772174802822));
#67144=CARTESIAN_POINT('Ctrl Pts',(0.558385895636291,-0.164595991582775,
-0.531862544857061));
#67145=CARTESIAN_POINT('Ctrl Pts',(0.569013847026506,0.12292229571057,-0.517952914911304));
#67146=CARTESIAN_POINT('Ctrl Pts',(0.440648992269832,0.380414398389757,
-0.504043284965543));
#67147=CARTESIAN_POINT('Ctrl Pts',(0.204646967905711,0.544982813873664,
-0.490133655019786));
#67148=CARTESIAN_POINT('Ctrl Pts',(-0.0813440971246574,0.57642847496774,
-0.476224025074025));
#67149=CARTESIAN_POINT('Ctrl Pts',(-0.347465269037444,0.467070161435511,
-0.462314395128267));
#67150=CARTESIAN_POINT('Ctrl Pts',(-0.528711225637859,0.243620788881355,
-0.448404765182507));
#67151=CARTESIAN_POINT('Ctrl Pts',(-0.580809082808382,-0.0393377454608579,
-0.434495135236749));
#67152=CARTESIAN_POINT('Ctrl Pts',(-0.491032915863341,-0.312687262979163,
-0.42058550529099));
#67153=CARTESIAN_POINT('Ctrl Pts',(-0.281312316558704,-0.509656776118064,
-0.406675875345232));
#67154=CARTESIAN_POINT('Ctrl Pts',(-0.00287565966342121,-0.582132613303954,
-0.392766245399472));
#67155=CARTESIAN_POINT('Ctrl Pts',(0.27626343357552,-0.512411128060141,
-0.378856615453714));
#67156=CARTESIAN_POINT('Ctrl Pts',(0.487919758039686,-0.317523162312504,
-0.364946985507953));
#67157=CARTESIAN_POINT('Ctrl Pts',(0.580392100077682,-0.0450739288092028,
-0.351037355562195));
#67158=CARTESIAN_POINT('Ctrl Pts',(0.531092274219919,0.23838549694698,-0.337127725616436));
#67159=CARTESIAN_POINT('Ctrl Pts',(0.352062731059539,0.46361458377452,-0.323218095670677));
#67160=CARTESIAN_POINT('Ctrl Pts',(0.0870349522026898,0.57559670428983,
-0.309308465724917));
#67161=CARTESIAN_POINT('Ctrl Pts',(-0.199252822873789,0.546978026486944,
-0.295398835779159));
#67162=CARTESIAN_POINT('Ctrl Pts',(-0.436869183145239,0.38474922445954,
-0.2814892058334));
#67163=CARTESIAN_POINT('Ctrl Pts',(-0.567771666395103,0.12853786879123,
-0.267579575887641));
#67164=CARTESIAN_POINT('Ctrl Pts',(-0.559984770547422,-0.159071385388608,
-0.253669945941883));
#67165=CARTESIAN_POINT('Ctrl Pts',(-0.415410597719517,-0.40782433012463,
-0.239760315996123));
#67166=CARTESIAN_POINT('Ctrl Pts',(-0.169364228912487,-0.556958173181869,
-0.225850686050364));
#67167=CARTESIAN_POINT('Ctrl Pts',(0.118052678971086,-0.570044045943112,
-0.211941056104605));
#67168=CARTESIAN_POINT('Ctrl Pts',(0.376632901220441,-0.443885464735316,
-0.198031426158846));
#67169=CARTESIAN_POINT('Ctrl Pts',(0.543213142264004,-0.209299144906713,
-0.184121796213087));
#67170=CARTESIAN_POINT('Ctrl Pts',(0.577102903915469,0.0764126069263521,
-0.170212166267328));
#67171=CARTESIAN_POINT('Ctrl Pts',(0.470023952420832,0.343459067734565,
-0.156302536321569));
#67172=CARTESIAN_POINT('Ctrl Pts',(0.248132412646873,0.526608928509874,
-0.14239290637581));
#67173=CARTESIAN_POINT('Ctrl Pts',(-0.0343703263707898,0.581124174352056,
-0.128483276430052));
#67174=CARTESIAN_POINT('Ctrl Pts',(-0.308477468009576,0.493688512513425,
-0.114573646484293));
#67175=CARTESIAN_POINT('Ctrl Pts',(-0.507232872173408,0.285659573106642,
-0.100664016538534));
#67176=CARTESIAN_POINT('Ctrl Pts',(-0.582086800194928,0.00785299289084335,
-0.0867543865927742));
#67177=CARTESIAN_POINT('Ctrl Pts',(-0.514754374468628,-0.271872459345322,
-0.0728447566470155));
#67178=CARTESIAN_POINT('Ctrl Pts',(-0.321683518120199,-0.485186504876865,
-0.0589351267012566));
#67179=CARTESIAN_POINT('Ctrl Pts',(-0.0500342978791844,-0.579986601383926,
-0.0450254967554975));
#67180=CARTESIAN_POINT('Ctrl Pts',(0.233835126413185,-0.533108926076464,
-0.0311158668097387));
#67181=CARTESIAN_POINT('Ctrl Pts',(0.460588964113884,-0.356018023025415,
-0.0172062368639799));
#67182=CARTESIAN_POINT('Ctrl Pts',(0.574828579379531,-0.0919449288341774,
-0.00329660691822081));
#67183=CARTESIAN_POINT('Ctrl Pts',(0.548667414168985,0.194552461871164,
0.010613023027538));
#67184=CARTESIAN_POINT('Ctrl Pts',(0.388458879975545,0.433598146048481,
0.0245226529732968));
#67185=CARTESIAN_POINT('Ctrl Pts',(0.21842861762083,0.522236456518856,0.033795739603803));
#67186=CARTESIAN_POINT('Ctrl Pts',(0.127946201224893,0.543535668558097,
0.0384322829190561));
#67187=CARTESIAN_POINT('Ctrl Pts',(-0.258391981634413,0.532271443393351,
-3.948325));
#67188=CARTESIAN_POINT('Ctrl Pts',(-0.346999241769787,0.489256914213255,
-3.94368845668475));
#67189=CARTESIAN_POINT('Ctrl Pts',(-0.502226568239526,0.358164595428381,
-3.93441537005424));
#67190=CARTESIAN_POINT('Ctrl Pts',(-0.612402242308734,0.0738461192841877,
-3.92050574010848));
#67191=CARTESIAN_POINT('Ctrl Pts',(-0.572977832471654,-0.228431041127055,
-3.90659611016272));
#67192=CARTESIAN_POINT('Ctrl Pts',(-0.393597009266127,-0.474948554308979,
-3.89268648021697));
#67193=CARTESIAN_POINT('Ctrl Pts',(-0.118069979218058,-0.60543068831445,
-3.8787768502712));
#67194=CARTESIAN_POINT('Ctrl Pts',(0.186296727754779,-0.588034642792585,
-3.86486722032545));
#67195=CARTESIAN_POINT('Ctrl Pts',(0.445157432417822,-0.426994391371127,
-3.85095759037968));
#67196=CARTESIAN_POINT('Ctrl Pts',(0.595279368990698,-0.161655034790457,
-3.83704796043393));
#67197=CARTESIAN_POINT('Ctrl Pts',(0.599992795452154,0.143173100143741,
-3.82313833048817));
#67198=CARTESIAN_POINT('Ctrl Pts',(0.458146114515487,0.413027696829806,
-3.80922870054241));
#67199=CARTESIAN_POINT('Ctrl Pts',(0.204388291644403,0.581992524500238,
-3.79531907059665));
#67200=CARTESIAN_POINT('Ctrl Pts',(-0.0992954073423366,0.608794066560272,
-3.78140944065089));
#67201=CARTESIAN_POINT('Ctrl Pts',(-0.378724241805151,0.486885796148415,
-3.76749981070513));
#67202=CARTESIAN_POINT('Ctrl Pts',(-0.565642248827353,0.246046060955832,
-3.75359018075937));
#67203=CARTESIAN_POINT('Ctrl Pts',(-0.614391025794256,-0.0548952318615489,
-3.73968055081362));
#67204=CARTESIAN_POINT('Ctrl Pts',(-0.51306273113035,-0.342427298829336,
-3.72577092086785));
#67205=CARTESIAN_POINT('Ctrl Pts',(-0.286408788336976,-0.546314767223382,
-3.71186129092209));
#67206=CARTESIAN_POINT('Ctrl Pts',(0.0102061249614486,-0.616754128750851,
-3.69795166097634));
#67207=CARTESIAN_POINT('Ctrl Pts',(0.304327992019713,-0.536539181138772,
-3.68404203103058));
#67208=CARTESIAN_POINT('Ctrl Pts',(0.52411177068089,-0.325264003104992,
-3.67013240108482));
#67209=CARTESIAN_POINT('Ctrl Pts',(0.6158709571608,-0.034536704499633,-3.65622277113906));
#67210=CARTESIAN_POINT('Ctrl Pts',(0.557191568159499,0.264626862168828,
-3.6423131411933));
#67211=CARTESIAN_POINT('Ctrl Pts',(0.362407196798647,0.499150121257423,
-3.62840351124754));
#67212=CARTESIAN_POINT('Ctrl Pts',(0.0790977508404253,0.611746161108203,
-3.61449388130178));
#67213=CARTESIAN_POINT('Ctrl Pts',(-0.223532874039147,0.574911187971986,
-3.60058425135602));
#67214=CARTESIAN_POINT('Ctrl Pts',(-0.471561204809241,0.397642867338423,
-3.58667462141027));
#67215=CARTESIAN_POINT('Ctrl Pts',(-0.604401451019528,0.123242467652703,
-3.57276499146451));
#67216=CARTESIAN_POINT('Ctrl Pts',(-0.58960477388398,-0.181262324935473,
-3.55885536151875));
#67217=CARTESIAN_POINT('Ctrl Pts',(-0.430785552361987,-0.441490235116783,
-3.54494573157299));
#67218=CARTESIAN_POINT('Ctrl Pts',(-0.166738500123487,-0.593875485606428,
-3.53103610162723));
#67219=CARTESIAN_POINT('Ctrl Pts',(0.1380377050979,-0.601194986505021,-3.51712647168147));
#67220=CARTESIAN_POINT('Ctrl Pts',(0.409095490133358,-0.461660805982183,
-3.50321684173571));
#67221=CARTESIAN_POINT('Ctrl Pts',(0.580223668090182,-0.209356907732974,
-3.48930721178996));
#67222=CARTESIAN_POINT('Ctrl Pts',(0.609620820972426,0.0940865264766722,
-3.4753975818442));
#67223=CARTESIAN_POINT('Ctrl Pts',(0.490106116901962,0.37454747897006,-3.46148795189844));
#67224=CARTESIAN_POINT('Ctrl Pts',(0.250873369318255,0.563517854548059,
-3.44757832195268));
#67225=CARTESIAN_POINT('Ctrl Pts',(-0.0496401252477701,0.614837928069609,
-3.43366869200692));
#67226=CARTESIAN_POINT('Ctrl Pts',(-0.338028044413961,0.515971763779004,
-3.41975906206116));
#67227=CARTESIAN_POINT('Ctrl Pts',(-0.543845975705585,0.291069363788744,
-3.4058494321154));
#67228=CARTESIAN_POINT('Ctrl Pts',(-0.616818847654587,-0.00493244418218084,
-3.39193980216964));
#67229=CARTESIAN_POINT('Ctrl Pts',(-0.539121603282495,-0.299729405800725,
-3.37803017222388));
#67230=CARTESIAN_POINT('Ctrl Pts',(-0.329733320306996,-0.521311574115583,
-3.36412054227812));
#67231=CARTESIAN_POINT('Ctrl Pts',(-0.0398011987077191,-0.61555315319554,
-3.35021091233237));
#67232=CARTESIAN_POINT('Ctrl Pts',(0.259853147272044,-0.559433786681102,
-3.3363012823866));
#67233=CARTESIAN_POINT('Ctrl Pts',(0.496033259163867,-0.366661731887602,
-3.32239165244085));
#67234=CARTESIAN_POINT('Ctrl Pts',(0.611047506650708,-0.0843253487599979,
-3.30848202249508));
#67235=CARTESIAN_POINT('Ctrl Pts',(0.576801401191375,0.218609156741456,
-3.29457239254933));
#67236=CARTESIAN_POINT('Ctrl Pts',(0.401660226552276,0.468144082771018,
-3.28066276260357));
#67237=CARTESIAN_POINT('Ctrl Pts',(0.128405653974211,0.603325623403315,
-3.26675313265781));
#67238=CARTESIAN_POINT('Ctrl Pts',(-0.176214521153363,0.59113303271111,
-3.25284350271205));
#67239=CARTESIAN_POINT('Ctrl Pts',(-0.437790839076186,0.434544590403002,
-3.23893387276629));
#67240=CARTESIAN_POINT('Ctrl Pts',(-0.592428147436097,0.17181009851862,
-3.22502424282053));
#67241=CARTESIAN_POINT('Ctrl Pts',(-0.602353246975706,-0.132892383850119,
-3.21111461287477));
#67242=CARTESIAN_POINT('Ctrl Pts',(-0.465141737228301,-0.405133291788988,
-3.19720498292902));
#67243=CARTESIAN_POINT('Ctrl Pts',(-0.214310223941008,-0.578412437402498,
-3.18329535298325));
#67244=CARTESIAN_POINT('Ctrl Pts',(0.0888707700613648,-0.61040298660495,
-3.1693857230375));
#67245=CARTESIAN_POINT('Ctrl Pts',(0.37034333327631,-0.493290619539167,
-3.15547609309174));
#67246=CARTESIAN_POINT('Ctrl Pts',(0.561352264720504,-0.255682331655327,
-3.14156646314598));
#67247=CARTESIAN_POINT('Ctrl Pts',(0.615239881950394,0.0443813866976684,
-3.12765683320022));
#67248=CARTESIAN_POINT('Ctrl Pts',(0.518843076239383,0.333604079810181,
-3.11374720325446));
#67249=CARTESIAN_POINT('Ctrl Pts',(0.295708660374863,0.541337425278215,
-3.0998375733087));
#67250=CARTESIAN_POINT('Ctrl Pts',(0.000341597234319436,0.616838474107179,
-3.08592794336294));
#67251=CARTESIAN_POINT('Ctrl Pts',(-0.295108907738821,0.541664612468586,
-3.07201831341719));
#67252=CARTESIAN_POINT('Ctrl Pts',(-0.518473266794936,0.334178532294536,
-3.05810868347143));
#67253=CARTESIAN_POINT('Ctrl Pts',(-0.615190348916484,0.0450627831758913,
-3.04419905352566));
#67254=CARTESIAN_POINT('Ctrl Pts',(-0.561635107513367,-0.255060435653969,
-3.03028942357991));
#67255=CARTESIAN_POINT('Ctrl Pts',(-0.370889461989462,-0.492880134325488,
-3.01637979363415));
#67256=CARTESIAN_POINT('Ctrl Pts',(-0.0895467820320154,-0.610304181253294,
-3.00247016368839));
#67257=CARTESIAN_POINT('Ctrl Pts',(0.213669457911877,-0.578649447060298,
-2.98856053374263));
#67258=CARTESIAN_POINT('Ctrl Pts',(0.464692736826349,-0.405648222193048,
-2.97465090379687));
#67259=CARTESIAN_POINT('Ctrl Pts',(0.602205689366357,-0.133559453137302,
-2.96074127385111));
#67260=CARTESIAN_POINT('Ctrl Pts',(0.592618076463096,0.171153835121284,
-2.94683164390535));
#67261=CARTESIAN_POINT('Ctrl Pts',(0.438271860844959,0.434059438117684,
-2.9329220139596));
#67262=CARTESIAN_POINT('Ctrl Pts',(0.176869136650822,0.590937499510681,
-2.91901238401383));
#67263=CARTESIAN_POINT('Ctrl Pts',(-0.127737347438336,0.603467472111763,
-2.90510275406808));
#67264=CARTESIAN_POINT('Ctrl Pts',(-0.401141475973243,0.46858866405575,
-2.89119312412232));
#67265=CARTESIAN_POINT('Ctrl Pts',(-0.576558921585075,0.219247872893211,
-2.87728349417656));
#67266=CARTESIAN_POINT('Ctrl Pts',(-0.61114052842268,-0.0836485167040743,
-2.8633738642308));
#67267=CARTESIAN_POINT('Ctrl Pts',(-0.496439059919587,-0.366112113448463,
-2.84946423428504));
#67268=CARTESIAN_POINT('Ctrl Pts',(-0.260472602208015,-0.55914563695564,
-2.83555460433928));
#67269=CARTESIAN_POINT('Ctrl Pts',(0.0391194036241582,-0.615596858412739,
-2.82164497439352));
#67270=CARTESIAN_POINT('Ctrl Pts',(0.329155726913755,-0.521676458417879,
-2.80773534444777));
#67271=CARTESIAN_POINT('Ctrl Pts',(0.538789300108363,-0.300326339031866,
-2.793825714502));
#67272=CARTESIAN_POINT('Ctrl Pts',(0.616813006275451,-0.00561561367818421,
-2.77991608455625));
#67273=CARTESIAN_POINT('Ctrl Pts',(0.54416802299301,0.29046683559302,-2.76600645461049));
#67274=CARTESIAN_POINT('Ctrl Pts',(0.338599313993788,0.515597056227515,
-2.75209682466473));
#67275=CARTESIAN_POINT('Ctrl Pts',(0.0503210733068214,0.614782570840124,
-2.73818719471897));
#67276=CARTESIAN_POINT('Ctrl Pts',(-0.250249077715523,0.563795369730963,
-2.72427756477321));
#67277=CARTESIAN_POINT('Ctrl Pts',(-0.489690977239046,0.375090078032214,
-2.71036793482745));
#67278=CARTESIAN_POINT('Ctrl Pts',(-0.609516239264299,0.094761668941873,
-2.69645830488169));
#67279=CARTESIAN_POINT('Ctrl Pts',(-0.580455190472774,-0.208714138669999,
-2.68254867493593));
#67280=CARTESIAN_POINT('Ctrl Pts',(-0.409606562718208,-0.461207419287372,
-2.66863904499017));
#67281=CARTESIAN_POINT('Ctrl Pts',(-0.138703488369955,-0.601041730782106,
-2.65472941504442));
#67282=CARTESIAN_POINT('Ctrl Pts',(0.166080636802718,-0.594059796575014,
-2.64081978509865));
#67283=CARTESIAN_POINT('Ctrl Pts',(0.430296305027459,-0.441967091203926,
-2.6269101551529));
#67284=CARTESIAN_POINT('Ctrl Pts',(0.589403650804615,-0.181915244676564,
-2.61300052520714));
#67285=CARTESIAN_POINT('Ctrl Pts',(0.60453758045727,0.12257297272406,-2.59909089526138));
#67286=CARTESIAN_POINT('Ctrl Pts',(0.472001334475186,0.397120334509814,
-2.58518126531562));
#67287=CARTESIAN_POINT('Ctrl Pts',(0.224169493620305,0.574663256140115,
-2.57127163536986));
#67288=CARTESIAN_POINT('Ctrl Pts',(-0.0784201481802541,0.61183339250725,
-2.5573620054241));
#67289=CARTESIAN_POINT('Ctrl Pts',(-0.361854128811955,0.499551207874913,
-2.54345237547834));
#67290=CARTESIAN_POINT('Ctrl Pts',(-0.556898132570094,0.265243830781198,
-2.52954274553259));
#67291=CARTESIAN_POINT('Ctrl Pts',(-0.615908831359701,-0.0338545607071286,
-2.51563311558682));
#67292=CARTESIAN_POINT('Ctrl Pts',(-0.524471703178682,-0.324683310923731,
-2.50172348564107));
#67293=CARTESIAN_POINT('Ctrl Pts',(-0.304922062182061,-0.536201786477984,
-2.48781385569531));
#67294=CARTESIAN_POINT('Ctrl Pts',(-0.0108892195898121,-0.616742446021246,
-2.47390422574955));
#67295=CARTESIAN_POINT('Ctrl Pts',(0.285803528724323,-0.54663165184269,
-2.45999459580379));
#67296=CARTESIAN_POINT('Ctrl Pts',(0.512683152680125,-0.342995342221306,
-2.44608496585803));
#67297=CARTESIAN_POINT('Ctrl Pts',(0.61432984877728,-0.0555756846905864,
-2.43217533591227));
#67298=CARTESIAN_POINT('Ctrl Pts',(0.565914415406841,0.245419425193436,
-2.41826570596651));
#67299=CARTESIAN_POINT('Ctrl Pts',(0.379263272927718,0.486466021049465,
-2.40435607602075));
#67300=CARTESIAN_POINT('Ctrl Pts',(0.0999696282526544,0.608683738286615,
-2.390446446075));
#67301=CARTESIAN_POINT('Ctrl Pts',(-0.203743561276915,0.582218499419028,
-2.37653681612924));
#67302=CARTESIAN_POINT('Ctrl Pts',(-0.45768838494997,0.413534958751291,
-2.36262718618348));
#67303=CARTESIAN_POINT('Ctrl Pts',(-0.599833832742337,0.143837383614901,
-2.34871755623772));
#67304=CARTESIAN_POINT('Ctrl Pts',(-0.595458087649196,-0.160995297076361,
-2.33480792629196));
#67305=CARTESIAN_POINT('Ctrl Pts',(-0.445630011338248,-0.426501714911226,
-2.3208982963462));
#67306=CARTESIAN_POINT('Ctrl Pts',(-0.186948053697615,-0.58782671345067,
-2.30698866640044));
#67307=CARTESIAN_POINT('Ctrl Pts',(0.117399637251469,-0.605563493781425,
-2.29307903645468));
#67308=CARTESIAN_POINT('Ctrl Pts',(0.393070161366252,-0.475379499001643,
-2.27916940650892));
#67309=CARTESIAN_POINT('Ctrl Pts',(0.57272557965118,-0.22907472632476,-2.26525977656316));
#67310=CARTESIAN_POINT('Ctrl Pts',(0.612481528206489,0.0731860467123818,
-2.2513501466174));
#67311=CARTESIAN_POINT('Ctrl Pts',(0.50262683589002,0.357569690648873,-2.23744051667165));
#67312=CARTESIAN_POINT('Ctrl Pts',(0.269995668571828,0.554609915868798,
-2.22353088672589));
#67313=CARTESIAN_POINT('Ctrl Pts',(-0.0285872428355586,0.616175777984337,
-2.20962125678013));
#67314=CARTESIAN_POINT('Ctrl Pts',(-0.320187158798318,0.527228606174024,
-2.19571162683437));
#67315=CARTESIAN_POINT('Ctrl Pts',(-0.53357507354856,0.309495493852806,
-2.18180199688861));
#67316=CARTESIAN_POINT('Ctrl Pts',(-0.6166267985029,0.0161620294396055,
-2.16789236694285));
#67317=CARTESIAN_POINT('Ctrl Pts',(-0.549055318912811,-0.281119328046106,
-2.15398273699709));
#67318=CARTESIAN_POINT('Ctrl Pts',(-0.34736629560325,-0.509731769175141,
-2.14007310705134));
#67319=CARTESIAN_POINT('Ctrl Pts',(-0.0608262331862064,-0.613832215824423,
-2.12616347710557));
#67320=CARTESIAN_POINT('Ctrl Pts',(0.240571831161854,-0.567992089627114,
-2.11225384715982));
#67321=CARTESIAN_POINT('Ctrl Pts',(0.483205501518772,-0.383408741592487,
-2.09834421721406));
#67322=CARTESIAN_POINT('Ctrl Pts',(0.607806739180643,-0.1051702792339,-2.0844345872683));
#67323=CARTESIAN_POINT('Ctrl Pts',(0.583939244991481,0.198758089109155,
-2.07052495732254));
#67324=CARTESIAN_POINT('Ctrl Pts',(0.417433123104956,0.454135891074891,
-2.05661532737678));
#67325=CARTESIAN_POINT('Ctrl Pts',(0.148960763556184,0.598582083551038,
-2.04270569743102));
#67326=CARTESIAN_POINT('Ctrl Pts',(-0.155898187708505,0.596812847462877,
-2.02879606748526));
#67327=CARTESIAN_POINT('Ctrl Pts',(-0.422675945174393,0.449260353468318,
-2.0148864375395));
#67328=CARTESIAN_POINT('Ctrl Pts',(-0.586206802731642,0.19196719578795,
-2.00097680759374));
#67329=CARTESIAN_POINT('Ctrl Pts',(-0.606545137084321,-0.112217719219845,
-1.98706717764799));
#67330=CARTESIAN_POINT('Ctrl Pts',(-0.478722910672709,-0.388991252632488,
-1.97315754770223));
#67331=CARTESIAN_POINT('Ctrl Pts',(-0.233963212407088,-0.570746033773078,
-1.95924791775647));
#67332=CARTESIAN_POINT('Ctrl Pts',(0.067946594942059,-0.613084888138114,
-1.94533828781071));
#67333=CARTESIAN_POINT('Ctrl Pts',(0.353259112175203,-0.505665719119589,
-1.93142865786495));
#67334=CARTESIAN_POINT('Ctrl Pts',(0.552281154132965,-0.274727768194447,
-1.91751902791919));
#67335=CARTESIAN_POINT('Ctrl Pts',(0.616397678771389,0.023317835079334,
-1.90360939797343));
#67336=CARTESIAN_POINT('Ctrl Pts',(0.529946965859142,0.31566759923095,-1.88969976802767));
#67337=CARTESIAN_POINT('Ctrl Pts',(0.314046299701105,0.530909353347243,
-1.87579013808191));
#67338=CARTESIAN_POINT('Ctrl Pts',(0.0214336577561771,0.616466072174888,
-1.86188050813615));
#67339=CARTESIAN_POINT('Ctrl Pts',(-0.276414575999195,0.551438847019983,
-1.84797087819039));
#67340=CARTESIAN_POINT('Ctrl Pts',(-0.506743121474926,0.351711854598891,
-1.83406124824464));
#67341=CARTESIAN_POINT('Ctrl Pts',(-0.613289708361258,0.0660723349497104,
-1.82015161829888));
#67342=CARTESIAN_POINT('Ctrl Pts',(-0.570028240502371,-0.235706650006559,
-1.80624198835312));
#67343=CARTESIAN_POINT('Ctrl Pts',(-0.387526180969968,-0.479909657008872,
-1.79233235840736));
#67344=CARTESIAN_POINT('Ctrl Pts',(-0.11036324168943,-0.60688530605984,
-1.7784227284616));
#67345=CARTESIAN_POINT('Ctrl Pts',(0.193758086632153,-0.585617301394169,
-1.76451309851584));
#67346=CARTESIAN_POINT('Ctrl Pts',(0.450550197368985,-0.421300770801945,
-1.75060346857009));
#67347=CARTESIAN_POINT('Ctrl Pts',(0.59728657471796,-0.154073253646539,
-1.73669383862432));
#67348=CARTESIAN_POINT('Ctrl Pts',(0.598123976975661,0.150789681325887,
-1.72278420867856));
#67349=CARTESIAN_POINT('Ctrl Pts',(0.452857852196158,0.418819275501768,
-1.7088745787328));
#67350=CARTESIAN_POINT('Ctrl Pts',(0.196972304020687,0.584544037071908,
-1.69496494878705));
#67351=CARTESIAN_POINT('Ctrl Pts',(-0.107027597455884,0.607482438602438,
-1.68105531884129));
#67352=CARTESIAN_POINT('Ctrl Pts',(-0.38488390649918,0.482031325066612,
-1.66714568889553));
#67353=CARTESIAN_POINT('Ctrl Pts',(-0.568724763221498,0.238834594492074,
-1.65323605894977));
#67354=CARTESIAN_POINT('Ctrl Pts',(-0.613643428193194,-0.0627021759020232,
-1.63932642900401));
#67355=CARTESIAN_POINT('Ctrl Pts',(-0.508667635404544,-0.348922708517937,
-1.62541679905825));
#67356=CARTESIAN_POINT('Ctrl Pts',(-0.279439783706537,-0.549912017607897,
-1.61150716911249));
#67357=CARTESIAN_POINT('Ctrl Pts',(0.0180467226611512,-0.616574517498683,
-1.59759753916674));
#67358=CARTESIAN_POINT('Ctrl Pts',(0.311124962626296,-0.53262658350699,
-1.58368790922097));
#67359=CARTESIAN_POINT('Ctrl Pts',(0.52820482075284,-0.318574147038023,
-1.56977827927522));
#67360=CARTESIAN_POINT('Ctrl Pts',(0.616260278787186,-0.0267037191545109,
-1.55586864932946));
#67361=CARTESIAN_POINT('Ctrl Pts',(0.553782061915196,0.271689616526834,
-1.5419590193837));
#67362=CARTESIAN_POINT('Ctrl Pts',(0.356031701523973,0.503717428066061,
-1.52804938943794));
#67363=CARTESIAN_POINT('Ctrl Pts',(0.071313606462209,0.612702366048064,
-1.51413975949218));
#67364=CARTESIAN_POINT('Ctrl Pts',(-0.230824237399053,0.572022719178783,
-1.50023012954642));
#67365=CARTESIAN_POINT('Ctrl Pts',(-0.476578728464133,0.391615290052691,
-1.48632049960066));
#67366=CARTESIAN_POINT('Ctrl Pts',(-0.605919506286032,0.115548135985117,
-1.4724108696549));
#67367=CARTESIAN_POINT('Ctrl Pts',(-0.587252545951943,-0.18874391937359,
-1.45850123970914));
#67368=CARTESIAN_POINT('Ctrl Pts',(-0.425137619095944,-0.446931565966172,
-1.44459160976338));
#67369=CARTESIAN_POINT('Ctrl Pts',(-0.159174480134843,-0.595947400951918,
-1.43068197981763));
#67370=CARTESIAN_POINT('Ctrl Pts',(0.145670151388394,-0.599391380336776,
-1.41677234987187));
#67371=CARTESIAN_POINT('Ctrl Pts',(0.414931987837101,-0.456422244524842,
-1.40286271992611));
#67372=CARTESIAN_POINT('Ctrl Pts',(0.582838538028783,-0.201963012494897,
-1.38895308998035));
#67373=CARTESIAN_POINT('Ctrl Pts',(0.608375329813878,0.101829651386026,
-1.37504346003459));
#67374=CARTESIAN_POINT('Ctrl Pts',(0.485304500320067,0.380748423235913,
-1.36113383008883));
#67375=CARTESIAN_POINT('Ctrl Pts',(0.2436885164549,0.566661915762435,-1.34722420014307));
#67376=CARTESIAN_POINT('Ctrl Pts',(-0.0574531729881512,0.61415710753938,
-1.33331457019731));
#67377=CARTESIAN_POINT('Ctrl Pts',(-0.344560796692032,0.511632365288294,
-1.31940494025155));
#67378=CARTESIAN_POINT('Ctrl Pts',(-0.547502679490492,0.284131370633859,
-1.3054953103058));
#67379=CARTESIAN_POINT('Ctrl Pts',(-0.61670628123834,-0.0127742909283064,
-1.29158568036004));
#67380=CARTESIAN_POINT('Ctrl Pts',(-0.535267263222785,-0.306559581076066,
-1.27767605041428));
#67381=CARTESIAN_POINT('Ctrl Pts',(-0.32307870485302,-0.525461673481557,
-1.26376642046852));
#67382=CARTESIAN_POINT('Ctrl Pts',(-0.031971828364136,-0.616009433384423,
-1.24985679052276));
#67383=CARTESIAN_POINT('Ctrl Pts',(0.26694479504954,-0.556084792296555,
-1.235947160577));
#67384=CARTESIAN_POINT('Ctrl Pts',(0.500654910143371,-0.360325520573934,
-1.22203753063124));
#67385=CARTESIAN_POINT('Ctrl Pts',(0.612070231822795,-0.0765496645579366,
-1.20812790068548));
#67386=CARTESIAN_POINT('Ctrl Pts',(0.573975379848994,0.22592495027054,-1.19421827073972));
#67387=CARTESIAN_POINT('Ctrl Pts',(0.395675769904307,0.473212959393736,
-1.18030864079397));
#67388=CARTESIAN_POINT('Ctrl Pts',(0.120724583076698,0.604909410464494,
-1.1663990108482));
#67389=CARTESIAN_POINT('Ctrl Pts',(-0.183715953896658,0.588844859119433,
-1.15248938090245));
#67390=CARTESIAN_POINT('Ctrl Pts',(-0.443280261408307,0.428943387492249,
-1.13857975095669));
#67391=CARTESIAN_POINT('Ctrl Pts',(-0.59456466015388,0.16426407009338,-1.12467012101093));
#67392=CARTESIAN_POINT('Ctrl Pts',(-0.600614964892065,-0.140539972161831,
-1.11076049106517));
#67393=CARTESIAN_POINT('Ctrl Pts',(-0.459953269877679,-0.411014366362508,
-1.09685086111941));
#67394=CARTESIAN_POINT('Ctrl Pts',(-0.206938956362332,-0.581090430283628,
-1.08294123117365));
#67395=CARTESIAN_POINT('Ctrl Pts',(0.0966242610087171,-0.609223745443381,
-1.06903160122789));
#67396=CARTESIAN_POINT('Ctrl Pts',(0.376585105169253,-0.488542197145964,
-1.05512197128214));
#67397=CARTESIAN_POINT('Ctrl Pts',(0.564557642201376,-0.248524623447187,
-1.04121234133637));
#67398=CARTESIAN_POINT('Ctrl Pts',(0.614625888623889,0.0521999699313994,
-1.02730271139062));
#67399=CARTESIAN_POINT('Ctrl Pts',(0.514559692032791,0.340173695577218,
-1.01339308144486));
#67400=CARTESIAN_POINT('Ctrl Pts',(0.288802185995616,0.545053315916615,
-0.999483451499097));
#67401=CARTESIAN_POINT('Ctrl Pts',(-0.00750092532454894,0.616792960357703,
-0.985573821553339));
#67402=CARTESIAN_POINT('Ctrl Pts',(-0.301971788334754,0.53786881195832,
-0.97166419160758));
#67403=CARTESIAN_POINT('Ctrl Pts',(-0.522680112072545,0.32755964383815,
-0.957754561661821));
#67404=CARTESIAN_POINT('Ctrl Pts',(-0.615713554304776,0.0372376002572928,
-0.943844931716061));
#67405=CARTESIAN_POINT('Ctrl Pts',(-0.558346869821805,-0.262180458439861,
-0.929935301770303));
#67406=CARTESIAN_POINT('Ctrl Pts',(-0.364592997846987,-0.497555791593757,
-0.916025671824543));
#67407=CARTESIAN_POINT('Ctrl Pts',(-0.0817801264522559,-0.611393351897938,
-0.902116041878785));
#67408=CARTESIAN_POINT('Ctrl Pts',(0.221009146785851,-0.575886079762772,
-0.888206411933026));
#67409=CARTESIAN_POINT('Ctrl Pts',(0.469812595853912,-0.399707323681405,
-0.874296781987267));
#67410=CARTESIAN_POINT('Ctrl Pts',(0.603855092438784,-0.125892204537418,
-0.860387152041508));
#67411=CARTESIAN_POINT('Ctrl Pts',(0.590394124489792,0.178674557773277,
-0.846477522095749));
#67412=CARTESIAN_POINT('Ctrl Pts',(0.432717797768262,0.439596550625831,
-0.83256789214999));
#67413=CARTESIAN_POINT('Ctrl Pts',(0.16934165144514,0.593138453409806,-0.818658262204231));
#67414=CARTESIAN_POINT('Ctrl Pts',(-0.135399518690504,0.601794641190765,
-0.804748632258472));
#67415=CARTESIAN_POINT('Ctrl Pts',(-0.407066697477651,0.463450670117309,
-0.790839002312714));
#67416=CARTESIAN_POINT('Ctrl Pts',(-0.579299841632726,0.211899771854153,
-0.776929372366953));
#67417=CARTESIAN_POINT('Ctrl Pts',(-0.610027623467106,-0.0914118068666102,
-0.763019742421195));
#67418=CARTESIAN_POINT('Ctrl Pts',(-0.491744178850862,-0.372394256660645,
-0.749110112475436));
#67419=CARTESIAN_POINT('Ctrl Pts',(-0.253342561922915,-0.562412096372292,
-0.735200482529677));
#67420=CARTESIAN_POINT('Ctrl Pts',(0.0469429507698155,-0.615049737176244,
-0.721290852583919));
#67421=CARTESIAN_POINT('Ctrl Pts',(0.335761725894722,-0.517449401634344,
-0.707381222638159));
#67422=CARTESIAN_POINT('Ctrl Pts',(0.54256410594822,-0.293451888329505,
-0.6934715926924));
#67423=CARTESIAN_POINT('Ctrl Pts',(0.616834548520052,0.00222701136191001,
-0.679561962746641));
#67424=CARTESIAN_POINT('Ctrl Pts',(0.540431039526075,0.297361919795237,
-0.665652332800882));
#67425=CARTESIAN_POINT('Ctrl Pts',(0.332016636412141,0.519860339873232,
-0.651742702855123));
#67426=CARTESIAN_POINT('Ctrl Pts',(0.0425006498771184,0.615372663178635,
-0.637833072909365));
#67427=CARTESIAN_POINT('Ctrl Pts',(-0.257396954996995,0.560568129120644,
-0.623923442963605));
#67428=CARTESIAN_POINT('Ctrl Pts',(-0.494420298979825,0.36883382136708,
-0.610013813017847));
#67429=CARTESIAN_POINT('Ctrl Pts',(-0.610671775757138,0.0870046097696368,
-0.596104183072087));
#67430=CARTESIAN_POINT('Ctrl Pts',(-0.577754679237444,-0.216077186317258,
-0.582194553126328));
#67431=CARTESIAN_POINT('Ctrl Pts',(-0.403709656655228,-0.466377886429944,
-0.568284923180569));
#67432=CARTESIAN_POINT('Ctrl Pts',(-0.131050622585714,-0.602756629285352,
-0.55437529323481));
#67433=CARTESIAN_POINT('Ctrl Pts',(0.173620099557238,-0.591900228803197,
-0.540465663289051));
#67434=CARTESIAN_POINT('Ctrl Pts',(0.435880702918256,-0.436460573993837,
-0.526556033343293));
#67435=CARTESIAN_POINT('Ctrl Pts',(0.591668884983244,-0.174406852991011,
-0.512646403397534));
#67436=CARTESIAN_POINT('Ctrl Pts',(0.602930322992061,0.130249166769832,
-0.498736773451775));
#67437=CARTESIAN_POINT('Ctrl Pts',(0.466914189564528,0.403089269778846,
-0.484827143506015));
#67438=CARTESIAN_POINT('Ctrl Pts',(0.216845096307452,0.577466902977956,
-0.470917513560257));
#67439=CARTESIAN_POINT('Ctrl Pts',(-0.0861926700187708,0.610786905117146,
-0.457007883614498));
#67440=CARTESIAN_POINT('Ctrl Pts',(-0.368176184084162,0.494910211352286,
-0.443098253668738));
#67441=CARTESIAN_POINT('Ctrl Pts',(-0.560225435126384,0.258141979664292,
-0.42918862372298));
#67442=CARTESIAN_POINT('Ctrl Pts',(-0.615428622210783,-0.0416824998204124,
-0.415278993777221));
#67443=CARTESIAN_POINT('Ctrl Pts',(-0.520301282839302,-0.331325210183763,
-0.401369363831462));
#67444=CARTESIAN_POINT('Ctrl Pts',(-0.298080137716725,-0.540035231560265,
-0.387459733885703));
#67445=CARTESIAN_POINT('Ctrl Pts',(-0.00304706540753377,-0.616831042685003,
-0.373550103939944));
#67446=CARTESIAN_POINT('Ctrl Pts',(0.292730312464302,-0.542953758613251,
-0.359640473994185));
#67447=CARTESIAN_POINT('Ctrl Pts',(0.517002563024396,-0.336449356744073,
-0.345730844048426));
#67448=CARTESIAN_POINT('Ctrl Pts',(0.61498678492718,-0.0477605924661943,
-0.331821214102667));
#67449=CARTESIAN_POINT('Ctrl Pts',(0.562748407806475,0.252594634422262,
-0.317911584156908));
#67450=CARTESIAN_POINT('Ctrl Pts',(0.373047681107323,0.491248661521552,
-0.304001954211149));
#67451=CARTESIAN_POINT('Ctrl Pts',(0.0922227325703765,0.609905556155062,
-0.290092324265389));
#67452=CARTESIAN_POINT('Ctrl Pts',(-0.211129429415761,0.579581041661311,
-0.276182694319631));
#67453=CARTESIAN_POINT('Ctrl Pts',(-0.462909082222679,0.407682476246539,
-0.262273064373872));
#67454=CARTESIAN_POINT('Ctrl Pts',(-0.601614101298651,0.136199460086949,
-0.248363434428113));
#67455=CARTESIAN_POINT('Ctrl Pts',(-0.59336306197319,-0.168552948706501,
-0.234453804482354));
#67456=CARTESIAN_POINT('Ctrl Pts',(-0.440171442516207,-0.432132990033561,
-0.220544174536595));
#67457=CARTESIAN_POINT('Ctrl Pts',(-0.179459304505732,-0.590156062114196,
-0.206634544590836));
#67458=CARTESIAN_POINT('Ctrl Pts',(0.125089293053353,-0.604021927649452,
-0.192724914645077));
#67459=CARTESIAN_POINT('Ctrl Pts',(0.399082373775165,-0.470343574278392,
-0.178815284699318));
#67460=CARTESIAN_POINT('Ctrl Pts',(0.575591748830518,-0.221774569634837,
-0.164905654753559));
#67461=CARTESIAN_POINT('Ctrl Pts',(0.61150153388306,0.0809672348318517,
-0.1509960248078));
#67462=CARTESIAN_POINT('Ctrl Pts',(0.498040065154857,0.363931190296861,
-0.137086394862041));
#67463=CARTESIAN_POINT('Ctrl Pts',(0.2629225219804,0.557997829079493,-0.123176764916282));
#67464=CARTESIAN_POINT('Ctrl Pts',(-0.0364189941745252,0.615762495010526,
-0.109267134970524));
#67465=CARTESIAN_POINT('Ctrl Pts',(-0.326864487384122,0.523115168220719,
-0.0953575050247646));
#67466=CARTESIAN_POINT('Ctrl Pts',(-0.537466849093141,0.302686515590083,
-0.0814478750790057));
#67467=CARTESIAN_POINT('Ctrl Pts',(-0.616782498852957,0.00832107612999849,
-0.0675382451332462));
#67468=CARTESIAN_POINT('Ctrl Pts',(-0.545436675894266,-0.288077611085068,
-0.0536286151874875));
#67469=CARTESIAN_POINT('Ctrl Pts',(-0.340857693525337,-0.514106392358444,
-0.0397189852417285));
#67470=CARTESIAN_POINT('Ctrl Pts',(-0.0530166278705213,-0.614557116194729,
-0.0258093552959695));
#67471=CARTESIAN_POINT('Ctrl Pts',(0.247773035809132,-0.56488526363447,
-0.0118997253502107));
#67472=CARTESIAN_POINT('Ctrl Pts',(0.488042697644273,-0.3772387310703,0.00200990459554817));
#67473=CARTESIAN_POINT('Ctrl Pts',(0.609091646611938,-0.0974253718589915,
0.0159195345413072));
#67474=CARTESIAN_POINT('Ctrl Pts',(0.581371126500397,0.206148900044987,
0.0298291644870661));
#67475=CARTESIAN_POINT('Ctrl Pts',(0.411613248423951,0.459443072628057,
0.0437387944328249));
#67476=CARTESIAN_POINT('Ctrl Pts',(0.231448211077896,0.553364732778595,
0.053011881063331));
#67477=CARTESIAN_POINT('Ctrl Pts',(0.135572525753558,0.575933499534279,
0.0576484243785842));
#67478=CARTESIAN_POINT('',(0.440852672434193,-0.394665718124065,-4.71844785465692E-16));
#67479=CARTESIAN_POINT('Ctrl Pts',(0.440852672434205,-0.394665718124053,
3.19189119579733E-16));
#67480=CARTESIAN_POINT('Ctrl Pts',(0.449473509661235,-0.383319951516819,
2.21718747786181E-16));
#67481=CARTESIAN_POINT('Ctrl Pts',(0.457669236756327,-0.371675141957999,
4.69429510016819E-16));
#67482=CARTESIAN_POINT('Ctrl Pts',(0.465417977049806,-0.359748402674913,
3.60822483003176E-16));
#67483=CARTESIAN_POINT('Ctrl Pts',(0.478522792578465,-0.339577676564143,
1.76477524638973E-16));
#67484=CARTESIAN_POINT('Ctrl Pts',(0.49035035518446,-0.318600789054235,
-4.07976529536807E-18));
#67485=CARTESIAN_POINT('Ctrl Pts',(0.500848641456442,-0.296948624890611,
2.77555756156289E-17));
#67486=CARTESIAN_POINT('Ctrl Pts',(0.505567169591327,-0.287216908385617,
4.20641920774481E-17));
#67487=CARTESIAN_POINT('Ctrl Pts',(0.510016871609266,-0.277348695241159,
-2.85300624831399E-16));
#67488=CARTESIAN_POINT('Ctrl Pts',(0.514191524236475,-0.26735564627476,
-1.59594559789866E-16));
#67489=CARTESIAN_POINT('Ctrl Pts',(0.517202709096176,-0.260147641097573,
-6.89225365995604E-17));
#67490=CARTESIAN_POINT('Ctrl Pts',(0.520070283326975,-0.252875404171917,
-8.31119041629936E-16));
#67491=CARTESIAN_POINT('Ctrl Pts',(0.522787666333145,-0.245555707113886,
-8.04911692853238E-16));
#67492=CARTESIAN_POINT('Ctrl Pts',(0.532118251028885,-0.220422314731567,
-7.14924419488921E-16));
#67493=CARTESIAN_POINT('Ctrl Pts',(0.53969714499334,-0.194692026166733,
-1.18934555017748E-15));
#67494=CARTESIAN_POINT('Ctrl Pts',(0.545444196280439,-0.168547995663248,
-9.43689570931383E-16));
#67495=CARTESIAN_POINT('Ctrl Pts',(0.549056990058101,-0.152112960371672,
-7.89261787198568E-16));
#67496=CARTESIAN_POINT('Ctrl Pts',(0.551945138461182,-0.135514277280572,
-7.18348360232636E-16));
#67497=CARTESIAN_POINT('Ctrl Pts',(0.554080825173503,-0.118797873410177,
-9.29811783123569E-16));
#67498=CARTESIAN_POINT('Ctrl Pts',(0.554897574044646,-0.112405033153251,
-1.01068156188733E-15));
#67499=CARTESIAN_POINT('Ctrl Pts',(0.555603692483668,-0.105998251700886,
-1.76377181419899E-16));
#67500=CARTESIAN_POINT('Ctrl Pts',(0.556197239913037,-0.0995885671750501,
-1.87350135405495E-16));
#67501=CARTESIAN_POINT('Ctrl Pts',(0.556520563146984,-0.0960970181817748,
-1.93327435269043E-16));
#67502=CARTESIAN_POINT('Ctrl Pts',(0.556810578854251,-0.0926038658318057,
-1.40863978828908E-15));
#67503=CARTESIAN_POINT('Ctrl Pts',(0.557067136889026,-0.089109521299019,
-1.346145417358E-15));
#67504=CARTESIAN_POINT('Ctrl Pts',(0.559148466251058,-0.0607616198835184,
-8.46098165632735E-16));
#67505=CARTESIAN_POINT('Ctrl Pts',(0.559032168734981,-0.0323347809399321,
-4.55844185429651E-16));
#67506=CARTESIAN_POINT('Ctrl Pts',(0.556766473320541,-0.0040747224533165,
1.87350135405495E-16));
#67507=CARTESIAN_POINT('Ctrl Pts',(0.554526618031147,0.0238630317021695,
8.23208862244566E-16));
#67508=CARTESIAN_POINT('Ctrl Pts',(0.550185657357224,0.0516390508176347,
-7.9422394213067E-16));
#67509=CARTESIAN_POINT('Ctrl Pts',(0.543742991249869,0.0789988052988092,
-5.89805981832114E-16));
#67510=CARTESIAN_POINT('Ctrl Pts',(0.542274703309206,0.08523411175344,-5.43218991142229E-16));
#67511=CARTESIAN_POINT('Ctrl Pts',(0.540697075429711,0.0914476831063459,
1.45157397677984E-16));
#67512=CARTESIAN_POINT('Ctrl Pts',(0.539009788839933,0.0976362763365649,
2.42861286636753E-16));
#67513=CARTESIAN_POINT('Ctrl Pts',(0.537244937498979,0.104109359882143,
3.45056634178706E-16));
#67514=CARTESIAN_POINT('Ctrl Pts',(0.535362451489014,0.110546340367326,
-1.62037308714591E-15));
#67515=CARTESIAN_POINT('Ctrl Pts',(0.533364232540718,0.116939620311351,
-1.51961776495568E-15));
#67516=CARTESIAN_POINT('Ctrl Pts',(0.526576398179125,0.138657223041689,
-1.17735775453025E-15));
#67517=CARTESIAN_POINT('Ctrl Pts',(0.518450319389671,0.159887678821144,
6.33155996280266E-16));
#67518=CARTESIAN_POINT('Ctrl Pts',(0.508999488902565,0.180499514917125,
3.98986399474666E-16));
#67519=CARTESIAN_POINT('Ctrl Pts',(0.499647078040256,0.200896702239358,
1.70100247173171E-16));
#67520=CARTESIAN_POINT('Ctrl Pts',(0.488996977302556,0.220688443939696,
-4.72088927560211E-16));
#67521=CARTESIAN_POINT('Ctrl Pts',(0.477125179451088,0.239761360845527,
-4.64905891561784E-16));
#67522=CARTESIAN_POINT('Ctrl Pts',(0.47033617898477,0.250668389703985,-4.60798204137098E-16));
#67523=CARTESIAN_POINT('Ctrl Pts',(0.463147348768218,0.261340063898874,
-1.21895900032892E-16));
#67524=CARTESIAN_POINT('Ctrl Pts',(0.455570893148401,0.27175245401761,-6.93889390390723E-17));
#67525=CARTESIAN_POINT('Ctrl Pts',(0.451960029834125,0.276714895478408,
-4.43646442090714E-17));
#67526=CARTESIAN_POINT('Ctrl Pts',(0.448259716184265,0.281620175565426,
-6.41205537235798E-16));
#67527=CARTESIAN_POINT('Ctrl Pts',(0.444475691970243,0.286459782798141,
-6.27969898303604E-16));
#67528=CARTESIAN_POINT('Ctrl Pts',(0.427914097738285,0.30764136269746,-5.70041283422271E-16));
#67529=CARTESIAN_POINT('Ctrl Pts',(0.409817642639405,0.327486298662323,
7.7277447926029E-16));
#67530=CARTESIAN_POINT('Ctrl Pts',(0.390329877941827,0.345809367181636,
3.92047505570758E-16));
#67531=CARTESIAN_POINT('Ctrl Pts',(0.375751687837344,0.359516284332848,
1.07237508812116E-16));
#67532=CARTESIAN_POINT('Ctrl Pts',(0.360393975723452,0.372370990775624,
-6.33097378333802E-16));
#67533=CARTESIAN_POINT('Ctrl Pts',(0.344306626863597,0.384279754800389,
-6.34908792207511E-16));
#67534=CARTESIAN_POINT('Ctrl Pts',(0.332937466072583,0.392695849596323,
-6.35893524695548E-16));
#67535=CARTESIAN_POINT('Ctrl Pts',(0.32120367197883,0.400639160697862,6.99898877407392E-16));
#67536=CARTESIAN_POINT('Ctrl Pts',(0.309136986598197,0.408089796563423,
1.08246744900953E-15));
#67537=CARTESIAN_POINT('Ctrl Pts',(0.304304445479439,0.411073673497764,
1.23568088705765E-15));
#67538=CARTESIAN_POINT('Ctrl Pts',(0.29941766815734,0.413978964054048,1.25373440441593E-15));
#67539=CARTESIAN_POINT('Ctrl Pts',(0.294481278576378,0.416802725091794,
1.11195774810113E-15));
#67540=CARTESIAN_POINT('Ctrl Pts',(0.271684194616619,0.42984333228132,4.57209113591521E-16));
#67541=CARTESIAN_POINT('Ctrl Pts',(0.247966811548276,0.44107191162788,4.1615832323067E-17));
#67542=CARTESIAN_POINT('Ctrl Pts',(0.223548691019426,0.45040451255921,2.97505076130022E-16));
#67543=CARTESIAN_POINT('Ctrl Pts',(0.199611204723685,0.459553415179844,
5.48357522354108E-16));
#67544=CARTESIAN_POINT('Ctrl Pts',(0.174999006015723,0.466880411586669,
-3.64733594368152E-16));
#67545=CARTESIAN_POINT('Ctrl Pts',(0.149912367171149,0.472257916219641,
-1.23165366794353E-16));
#67546=CARTESIAN_POINT('Ctrl Pts',(0.137612004500597,0.474894588978313,
-4.7207705593021E-18));
#67547=CARTESIAN_POINT('Ctrl Pts',(0.125197600089965,0.477061825059574,
-3.93939898786201E-18));
#67548=CARTESIAN_POINT('Ctrl Pts',(0.112693552167563,0.478740006605732,
0.));
#67549=CARTESIAN_POINT('Ctrl Pts',(-0.591724986204225,2.85874560315911E-6,
-0.0671625192204902));
#67550=CARTESIAN_POINT('Ctrl Pts',(-0.591699563611128,-0.0958074619682504,
-0.0626512178761559));
#67551=CARTESIAN_POINT('Ctrl Pts',(-0.567976406750561,-0.19163001081242,
-0.0581399165318217));
#67552=CARTESIAN_POINT('Ctrl Pts',(-0.523231149325893,-0.27634929342812,
-0.0536286151874874));
#67553=CARTESIAN_POINT('Ctrl Pts',(-0.47724368177129,-0.363420538176193,
-0.0489920718722345));
#67554=CARTESIAN_POINT('Ctrl Pts',(-0.409050687648318,-0.438763465267315,
-0.0443555285569818));
#67555=CARTESIAN_POINT('Ctrl Pts',(-0.326980679644361,-0.493176716118926,
-0.0397189852417288));
#67556=CARTESIAN_POINT('Ctrl Pts',(-0.244910671640404,-0.547589966970536,
-0.0350824419264758));
#67557=CARTESIAN_POINT('Ctrl Pts',(-0.148963649755454,-0.581073541582635,
-0.0304458986112222));
#67558=CARTESIAN_POINT('Ctrl Pts',(-0.0508585281997095,-0.589536686795305,
-0.0258093552959693));
#67559=CARTESIAN_POINT('Ctrl Pts',(0.0472465933560355,-0.597999832007976,
-0.0211728119807163));
#67560=CARTESIAN_POINT('Ctrl Pts',(0.147509814582582,-0.581442547821224,
-0.0165362686654636));
#67561=CARTESIAN_POINT('Ctrl Pts',(0.237686368835047,-0.541889483633819,
-0.0118997253502107));
#67562=CARTESIAN_POINT('Ctrl Pts',(0.314832650426807,-0.508051732203712,
-0.00793315023347389));
#67563=CARTESIAN_POINT('Ctrl Pts',(0.384596653849161,-0.457383719090204,
-0.00396657511673726));
#67564=CARTESIAN_POINT('Ctrl Pts',(0.440852672434193,-0.394665718124065,
-4.71844785465692E-16));
#67565=CARTESIAN_POINT('',(-0.285727948592038,-0.40034239738492,-3.948325));
#67566=CARTESIAN_POINT('Ctrl Pts',(-0.285727948592038,-0.40034239738492,
-3.948325));
#67567=CARTESIAN_POINT('Ctrl Pts',(-0.296082595521109,-0.394398284770688,
-3.948325));
#67568=CARTESIAN_POINT('Ctrl Pts',(-0.306205674003326,-0.388080952767024,
-3.948325));
#67569=CARTESIAN_POINT('Ctrl Pts',(-0.316075703283998,-0.381402204064925,
-3.948325));
#67570=CARTESIAN_POINT('Ctrl Pts',(-0.333628984468336,-0.369524432419702,
-3.948325));
#67571=CARTESIAN_POINT('Ctrl Pts',(-0.350382541823529,-0.356504844564474,
-3.948325));
#67572=CARTESIAN_POINT('Ctrl Pts',(-0.366265661797884,-0.342458377831604,
-3.948325));
#67573=CARTESIAN_POINT('Ctrl Pts',(-0.373067338029369,-0.336443217141036,
-3.948325));
#67574=CARTESIAN_POINT('Ctrl Pts',(-0.379709280111531,-0.330239464740281,
-3.948325));
#67575=CARTESIAN_POINT('Ctrl Pts',(-0.386185328609897,-0.32385498795212,
-3.948325));
#67576=CARTESIAN_POINT('Ctrl Pts',(-0.390906098569952,-0.319200969959539,
-3.948325));
#67577=CARTESIAN_POINT('Ctrl Pts',(-0.395536981686774,-0.314452441162492,
-3.948325));
#67578=CARTESIAN_POINT('Ctrl Pts',(-0.400069693202905,-0.309619281567598,
-3.948325));
#67579=CARTESIAN_POINT('Ctrl Pts',(-0.416474734625152,-0.292126841761447,
-3.948325));
#67580=CARTESIAN_POINT('Ctrl Pts',(-0.431618982752109,-0.273504975619171,
-3.948325));
#67581=CARTESIAN_POINT('Ctrl Pts',(-0.445400119986255,-0.253908755436526,
-3.948325));
#67582=CARTESIAN_POINT('Ctrl Pts',(-0.451206944048774,-0.24565168630227,
-3.948325));
#67583=CARTESIAN_POINT('Ctrl Pts',(-0.456771538061931,-0.237221261837567,
-3.948325));
#67584=CARTESIAN_POINT('Ctrl Pts',(-0.462085123502627,-0.228627650838076,
-3.948325));
#67585=CARTESIAN_POINT('Ctrl Pts',(-0.46560519169573,-0.222934678158739,
-3.948325));
#67586=CARTESIAN_POINT('Ctrl Pts',(-0.469016405936867,-0.217167713895661,
-3.948325));
#67587=CARTESIAN_POINT('Ctrl Pts',(-0.472311582807742,-0.211337460706846,
-3.948325));
#67588=CARTESIAN_POINT('Ctrl Pts',(-0.475847180328577,-0.205081824202959,
-3.948325));
#67589=CARTESIAN_POINT('Ctrl Pts',(-0.479246974049362,-0.19875752364046,
-3.948325));
#67590=CARTESIAN_POINT('Ctrl Pts',(-0.482508590030484,-0.192368808372637,
-3.948325));
#67591=CARTESIAN_POINT('Ctrl Pts',(-0.494734148213928,-0.168421902704926,
-3.948325));
#67592=CARTESIAN_POINT('Ctrl Pts',(-0.505021436671191,-0.14357295390494,
-3.948325));
#67593=CARTESIAN_POINT('Ctrl Pts',(-0.513371142735674,-0.118078037500813,
-3.948325));
#67594=CARTESIAN_POINT('Ctrl Pts',(-0.518853109089587,-0.101339451394439,
-3.948325));
#67595=CARTESIAN_POINT('Ctrl Pts',(-0.523499115474155,-0.0843215126712255,
-3.948325));
#67596=CARTESIAN_POINT('Ctrl Pts',(-0.527299444230766,-0.0670897043369155,
-3.948325));
#67597=CARTESIAN_POINT('Ctrl Pts',(-0.530337067689686,-0.053316226149045,
-3.948325));
#67598=CARTESIAN_POINT('Ctrl Pts',(-0.532834254606844,-0.0394059791423619,
-3.948325));
#67599=CARTESIAN_POINT('Ctrl Pts',(-0.534782029141017,-0.0253909900826123,
-3.948325));
#67600=CARTESIAN_POINT('Ctrl Pts',(-0.535644228960787,-0.0191871298157362,
-3.948325));
#67601=CARTESIAN_POINT('Ctrl Pts',(-0.536398045645329,-0.0129667940238257,
-3.948325));
#67602=CARTESIAN_POINT('Ctrl Pts',(-0.537042228310059,-0.00674248143224362,
-3.948325));
#67603=CARTESIAN_POINT('Ctrl Pts',(-0.539515522073872,0.0171553263785874,
-3.948325));
#67604=CARTESIAN_POINT('Ctrl Pts',(-0.54038057067284,0.0411519544184588,
-3.948325));
#67605=CARTESIAN_POINT('Ctrl Pts',(-0.539627056960311,0.0650829329353078,
-3.948325));
#67606=CARTESIAN_POINT('Ctrl Pts',(-0.538898018290729,0.0882366041288409,
-3.948325));
#67607=CARTESIAN_POINT('Ctrl Pts',(-0.536653985044464,0.111329445677917,
-3.948325));
#67608=CARTESIAN_POINT('Ctrl Pts',(-0.532953652586977,0.134229883485741,
-3.948325));
#67609=CARTESIAN_POINT('Ctrl Pts',(-0.530626779492689,0.148630322688061,
-3.948325));
#67610=CARTESIAN_POINT('Ctrl Pts',(-0.527723528323636,0.162954790975836,
-3.948325));
#67611=CARTESIAN_POINT('Ctrl Pts',(-0.524253375751702,0.177170538350544,
-3.948325));
#67612=CARTESIAN_POINT('Ctrl Pts',(-0.522340300985194,0.185007596527629,
-3.948325));
#67613=CARTESIAN_POINT('Ctrl Pts',(-0.520253718058824,0.192814707355631,
-3.948325));
#67614=CARTESIAN_POINT('Ctrl Pts',(-0.518002646091187,0.200561489135888,
-3.948325));
#67615=CARTESIAN_POINT('Ctrl Pts',(-0.510004128433378,0.228087384243376,
-3.948325));
#67616=CARTESIAN_POINT('Ctrl Pts',(-0.499919583291045,0.254914254992326,
-3.948325));
#67617=CARTESIAN_POINT('Ctrl Pts',(-0.487866003040689,0.280804612238299,
-3.948325));
#67618=CARTESIAN_POINT('Ctrl Pts',(-0.480108922853125,0.297466348674306,
-3.948325));
#67619=CARTESIAN_POINT('Ctrl Pts',(-0.471535246924139,0.313740425559195,
-3.948325));
#67620=CARTESIAN_POINT('Ctrl Pts',(-0.462164839595945,0.329562331281333,
-3.948325));
#67621=CARTESIAN_POINT('Ctrl Pts',(-0.454710650331234,0.34214870833523,
-3.948325));
#67622=CARTESIAN_POINT('Ctrl Pts',(-0.446752088203126,0.354448939593675,
-3.948325));
#67623=CARTESIAN_POINT('Ctrl Pts',(-0.438312880065648,0.366442036514319,
-3.948325));
#67624=CARTESIAN_POINT('Ctrl Pts',(-0.434649842629724,0.371647639016038,
-3.948325));
#67625=CARTESIAN_POINT('Ctrl Pts',(-0.430896211124093,0.376795355434164,
-3.948325));
#67626=CARTESIAN_POINT('Ctrl Pts',(-0.427053747527973,0.381883355554364,
-3.948325));
#67627=CARTESIAN_POINT('Ctrl Pts',(-0.423072494282475,0.387155134059201,
-3.948325));
#67628=CARTESIAN_POINT('Ctrl Pts',(-0.419000871875213,0.392356106729907,
-3.948325));
#67629=CARTESIAN_POINT('Ctrl Pts',(-0.414844342099757,0.397481307504267,
-3.948325));
#67630=CARTESIAN_POINT('Ctrl Pts',(-0.396507671020364,0.42009130331621,
-3.948325));
#67631=CARTESIAN_POINT('Ctrl Pts',(-0.37650644191244,0.441249440744765,
-3.948325));
#67632=CARTESIAN_POINT('Ctrl Pts',(-0.355056904178872,0.460812670257216,
-3.948325));
#67633=CARTESIAN_POINT('Ctrl Pts',(-0.333444871567189,0.480524104576441,
-3.948325));
#67634=CARTESIAN_POINT('Ctrl Pts',(-0.310361705037122,0.49861742897275,
-3.948325));
#67635=CARTESIAN_POINT('Ctrl Pts',(-0.285984798569953,0.5149186212662,-3.948325));
#67636=CARTESIAN_POINT('Ctrl Pts',(-0.276962187040763,0.5209521729691,-3.948325));
#67637=CARTESIAN_POINT('Ctrl Pts',(-0.267761970436877,0.526739857966417,
-3.948325));
#67638=CARTESIAN_POINT('Ctrl Pts',(-0.258391981634414,0.532271443393351,
-3.948325));
#67639=CARTESIAN_POINT('Ctrl Pts',(-0.285727948592038,-0.40034239738492,
-3.948325));
#67640=CARTESIAN_POINT('Ctrl Pts',(-0.228684894383911,-0.440971740204431,
-3.94435842488326));
#67641=CARTESIAN_POINT('Ctrl Pts',(-0.08595864849882,-0.50256281066439,
-3.93575530645127));
#67642=CARTESIAN_POINT('Ctrl Pts',(0.154857629827177,-0.488798982873136,
-3.92251564470403));
#67643=CARTESIAN_POINT('Ctrl Pts',(0.37003347141403,-0.354935592235777,
-3.90860601475827));
#67644=CARTESIAN_POINT('Ctrl Pts',(0.494821102216335,-0.134374424279909,
-3.89469638481251));
#67645=CARTESIAN_POINT('Ctrl Pts',(0.498739099375933,0.119011467407269,
-3.88078675486675));
#67646=CARTESIAN_POINT('Ctrl Pts',(0.380830207075808,0.343325891736714,
-3.86687712492099));
#67647=CARTESIAN_POINT('Ctrl Pts',(0.169896094203756,0.483776521506451,
-3.85296749497524));
#67648=CARTESIAN_POINT('Ctrl Pts',(-0.0825384944710284,0.506055083932911,
-3.83905786502947));
#67649=CARTESIAN_POINT('Ctrl Pts',(-0.314811425572855,0.404719832155649,
-3.82514823508372));
#67650=CARTESIAN_POINT('Ctrl Pts',(-0.46094408502887,0.21643111900778,-3.81206592794025));
#67651=CARTESIAN_POINT('Ctrl Pts',(-0.491770333220413,0.0672463213179462,
-3.80362016411204));
#67652=CARTESIAN_POINT('Ctrl Pts',(-0.491838560105423,-1.18860308867142E-5,
-3.79981094359907));
#67653=CARTESIAN_POINT('Origin',(-7.01450167938425E-17,0.,-3.948325));
#67654=CARTESIAN_POINT('',(-0.591675,-7.2459289488551E-17,-3.948325));
#67655=CARTESIAN_POINT('Origin',(0.,0.,-3.948325));
#67656=CARTESIAN_POINT('Origin',(0.,0.,-3.948325));
#67657=CARTESIAN_POINT('',(0.285706463458477,-0.400329423553965,-3.948325));
#67658=CARTESIAN_POINT('Ctrl Pts',(0.258414858989731,0.532291148796132,
-3.948325));
#67659=CARTESIAN_POINT('Ctrl Pts',(0.270692196855467,0.525058429447917,
-3.948325));
#67660=CARTESIAN_POINT('Ctrl Pts',(0.282689452115837,0.517387875687169,
-3.948325));
#67661=CARTESIAN_POINT('Ctrl Pts',(0.294379894662667,0.509287034300484,
-3.948325));
#67662=CARTESIAN_POINT('Ctrl Pts',(0.314150991282511,0.495586738771328,
-3.948325));
#67663=CARTESIAN_POINT('Ctrl Pts',(0.333045588916465,0.480656394447447,
-3.948325));
#67664=CARTESIAN_POINT('Ctrl Pts',(0.350965945749258,0.464597409889149,
-3.948325));
#67665=CARTESIAN_POINT('Ctrl Pts',(0.359020375799688,0.457379586660928,
-3.948325));
#67666=CARTESIAN_POINT('Ctrl Pts',(0.366877754573242,0.44993357574956,-3.948325));
#67667=CARTESIAN_POINT('Ctrl Pts',(0.374527904104896,0.44226780995476,-3.948325));
#67668=CARTESIAN_POINT('Ctrl Pts',(0.380045971174055,0.436738478845983,
-3.948325));
#67669=CARTESIAN_POINT('Ctrl Pts',(0.385455478952879,0.431095285495367,
-3.948325));
#67670=CARTESIAN_POINT('Ctrl Pts',(0.39074398206846,0.425351256933648,-3.948325));
#67671=CARTESIAN_POINT('Ctrl Pts',(0.408902933400678,0.405628183537733,
-3.948325));
#67672=CARTESIAN_POINT('Ctrl Pts',(0.425667032165364,0.384688931004672,
-3.948325));
#67673=CARTESIAN_POINT('Ctrl Pts',(0.440892698522948,0.362672619611768,
-3.948325));
#67674=CARTESIAN_POINT('Ctrl Pts',(0.450464075156269,0.34883241035794,-3.948325));
#67675=CARTESIAN_POINT('Ctrl Pts',(0.459426866363713,0.334566154978976,
-3.948325));
#67676=CARTESIAN_POINT('Ctrl Pts',(0.467737926515355,0.319905814085685,
-3.948325));
#67677=CARTESIAN_POINT('Ctrl Pts',(0.470916318295014,0.314299272184647,
-3.948325));
#67678=CARTESIAN_POINT('Ctrl Pts',(0.473997613735816,0.308637905559322,
-3.948325));
#67679=CARTESIAN_POINT('Ctrl Pts',(0.476975834115326,0.302931193698179,
-3.948325));
#67680=CARTESIAN_POINT('Ctrl Pts',(0.478598160818049,0.29982257517526,-3.948325));
#67681=CARTESIAN_POINT('Ctrl Pts',(0.480190271744143,0.296699851021107,
-3.948325));
#67682=CARTESIAN_POINT('Ctrl Pts',(0.481751872132746,0.293563344844831,
-3.948325));
#67683=CARTESIAN_POINT('Ctrl Pts',(0.494420368969739,0.268118411004285,
-3.948325));
#67684=CARTESIAN_POINT('Ctrl Pts',(0.505085056951574,0.241767638286393,
-3.948325));
#67685=CARTESIAN_POINT('Ctrl Pts',(0.513697452978676,0.214756695707742,
-3.948325));
#67686=CARTESIAN_POINT('Ctrl Pts',(0.52221162370046,0.188053815841646,-3.948325));
#67687=CARTESIAN_POINT('Ctrl Pts',(0.528720105838612,0.160704397593371,
-3.948325));
#67688=CARTESIAN_POINT('Ctrl Pts',(0.533125889963004,0.132943760576394,
-3.948325));
#67689=CARTESIAN_POINT('Ctrl Pts',(0.534129969718082,0.126617101614028,
-3.948325));
#67690=CARTESIAN_POINT('Ctrl Pts',(0.535024628194969,0.120269122589768,
-3.948325));
#67691=CARTESIAN_POINT('Ctrl Pts',(0.535808341459282,0.113902703852351,
-3.948325));
#67692=CARTESIAN_POINT('Ctrl Pts',(0.536628084967519,0.107243596920824,
-3.948325));
#67693=CARTESIAN_POINT('Ctrl Pts',(0.537325285579543,0.100573322813461,
-3.948325));
#67694=CARTESIAN_POINT('Ctrl Pts',(0.537898824104105,0.0938996332282421,
-3.948325));
#67695=CARTESIAN_POINT('Ctrl Pts',(0.539847098021773,0.0712295338423138,
-3.948325));
#67696=CARTESIAN_POINT('Ctrl Pts',(0.540372332158008,0.048503123801434,
-3.948325));
#67697=CARTESIAN_POINT('Ctrl Pts',(0.539437191193445,0.0258471839316688,
-3.948325));
#67698=CARTESIAN_POINT('Ctrl Pts',(0.538511788225682,0.00342716942321664,
-3.948325));
#67699=CARTESIAN_POINT('Ctrl Pts',(0.536156044637272,-0.0189243113481171,
-3.948325));
#67700=CARTESIAN_POINT('Ctrl Pts',(0.532397321112644,-0.0410735384121692,
-3.948325));
#67701=CARTESIAN_POINT('Ctrl Pts',(0.530247857204089,-0.0537397970142222,
-3.948325));
#67702=CARTESIAN_POINT('Ctrl Pts',(0.527639194833725,-0.066339768733417,
-3.948325));
#67703=CARTESIAN_POINT('Ctrl Pts',(0.524573560199496,-0.0788466840532584,
-3.948325));
#67704=CARTESIAN_POINT('Ctrl Pts',(0.523112516145411,-0.0848073272619983,
-3.948325));
#67705=CARTESIAN_POINT('Ctrl Pts',(0.52154703257174,-0.0907489695288106,
-3.948325));
#67706=CARTESIAN_POINT('Ctrl Pts',(0.519879195788693,-0.0966615590501735,
-3.948325));
#67707=CARTESIAN_POINT('Ctrl Pts',(0.512579525727885,-0.122539362651615,
-3.948325));
#67708=CARTESIAN_POINT('Ctrl Pts',(0.503352948066008,-0.147761845315584,
-3.948325));
#67709=CARTESIAN_POINT('Ctrl Pts',(0.492262118340815,-0.172103200481393,
-3.948325));
#67710=CARTESIAN_POINT('Ctrl Pts',(0.483965425647558,-0.190312184709993,
-3.948325));
#67711=CARTESIAN_POINT('Ctrl Pts',(0.474624408392381,-0.20802791865184,
-3.948325));
#67712=CARTESIAN_POINT('Ctrl Pts',(0.464249712096462,-0.225144758296707,
-3.948325));
#67713=CARTESIAN_POINT('Ctrl Pts',(0.456917754127682,-0.237241493011135,
-3.948325));
#67714=CARTESIAN_POINT('Ctrl Pts',(0.449069197429663,-0.249038883086192,
-3.948325));
#67715=CARTESIAN_POINT('Ctrl Pts',(0.440725878633132,-0.260506491692914,
-3.948325));
#67716=CARTESIAN_POINT('Ctrl Pts',(0.437384497280559,-0.26509910699284,
-3.948325));
#67717=CARTESIAN_POINT('Ctrl Pts',(0.433963144714414,-0.269639549928986,
-3.948325));
#67718=CARTESIAN_POINT('Ctrl Pts',(0.430464984712528,-0.274123344607859,
-3.948325));
#67719=CARTESIAN_POINT('Ctrl Pts',(0.414309880260752,-0.294830279493182,
-3.948325));
#67720=CARTESIAN_POINT('Ctrl Pts',(0.396616450072697,-0.314209078958056,
-3.948325));
#67721=CARTESIAN_POINT('Ctrl Pts',(0.377556066500118,-0.332098849600154,
-3.948325));
#67722=CARTESIAN_POINT('Ctrl Pts',(0.358870868001475,-0.349636477542946,
-3.948325));
#67723=CARTESIAN_POINT('Ctrl Pts',(0.338870871116485,-0.365743763761861,
-3.948325));
#67724=CARTESIAN_POINT('Ctrl Pts',(0.317693061872851,-0.380226744315664,
-3.948325));
#67725=CARTESIAN_POINT('Ctrl Pts',(0.307309243671757,-0.387327981055998,
-3.948325));
#67726=CARTESIAN_POINT('Ctrl Pts',(0.296641996093472,-0.39403800768009,
-3.948325));
#67727=CARTESIAN_POINT('Ctrl Pts',(0.28570646345848,-0.400329423553963,
-3.948325));
#67728=CARTESIAN_POINT('Origin',(0.,0.,-3.948325));
#67729=CARTESIAN_POINT('Origin',(0.,0.,-4.27183905640093));
#67730=CARTESIAN_POINT('Ctrl Pts',(0.285706463458477,-0.400329423553965,
-3.948325));
#67731=CARTESIAN_POINT('Ctrl Pts',(0.35234932738247,-0.352767850893538,
-3.94368845668475));
#67732=CARTESIAN_POINT('Ctrl Pts',(0.461355386710151,-0.223767338793563,
-3.93441537005424));
#67733=CARTESIAN_POINT('Ctrl Pts',(0.512153850375005,0.024551470863185,
-3.92050574010848));
#67734=CARTESIAN_POINT('Ctrl Pts',(0.437852459283724,0.266806684479465,
-3.90659611016272));
#67735=CARTESIAN_POINT('Ctrl Pts',(0.256595437328703,0.443921775016828,
-3.89268648021697));
#67736=CARTESIAN_POINT('Ctrl Pts',(0.0126607096365889,0.51258367325088,
-3.8787768502712));
#67737=CARTESIAN_POINT('Ctrl Pts',(-0.234367035151384,0.456045416423434,
-3.86486722032544));
#67738=CARTESIAN_POINT('Ctrl Pts',(-0.424145829883178,0.288104776438461,
-3.85095759037969));
#67739=CARTESIAN_POINT('Ctrl Pts',(-0.487188530294114,0.113758445818203,
-3.84078153573818));
#67740=CARTESIAN_POINT('Ctrl Pts',(-0.491850800983448,0.0159562304202861,
-3.83524202441192));
#67741=CARTESIAN_POINT('Ctrl Pts',(-0.491834365111822,1.24153615857388E-5,
-3.83433905640092));
#67742=CARTESIAN_POINT('Ctrl Pts',(0.343710408716095,-0.481604049573106,
-4.00597342437858));
#67743=CARTESIAN_POINT('Ctrl Pts',(0.423883064665323,-0.424386556554537,
-4.00133688106333));
#67744=CARTESIAN_POINT('Ctrl Pts',(0.555019465118139,-0.269196442191191,
-3.99206379443282));
#67745=CARTESIAN_POINT('Ctrl Pts',(0.616131000702752,0.0295358949280207,
-3.97815416448707));
#67746=CARTESIAN_POINT('Ctrl Pts',(0.526744988251306,0.320973608579041,
-3.9642445345413));
#67747=CARTESIAN_POINT('Ctrl Pts',(0.308689280499083,0.534046492620507,
-3.95033490459555));
#67748=CARTESIAN_POINT('Ctrl Pts',(0.015231078888283,0.616648085946656,
-3.93642527464979));
#67749=CARTESIAN_POINT('Ctrl Pts',(-0.281948082190197,0.548631468026912,
-3.92251564470403));
#67750=CARTESIAN_POINT('Ctrl Pts',(-0.510255647631026,0.346595625678295,
-3.90860601475827));
#67751=CARTESIAN_POINT('Ctrl Pts',(-0.613923373668732,0.0598996637254193,
-3.89469638481251));
#67752=CARTESIAN_POINT('Ctrl Pts',(-0.567628196994441,-0.241429332723434,
-3.88078675486675));
#67753=CARTESIAN_POINT('Ctrl Pts',(-0.382678718524923,-0.483783774923831,
-3.86687712492099));
#67754=CARTESIAN_POINT('Ctrl Pts',(-0.104252431765138,-0.607964887305674,
-3.85296749497524));
#67755=CARTESIAN_POINT('Ctrl Pts',(0.199639550299989,-0.583638454109383,
-3.83905786502947));
#67756=CARTESIAN_POINT('Ctrl Pts',(0.454765656086047,-0.416746960908529,
-3.82514823508372));
#67757=CARTESIAN_POINT('Ctrl Pts',(0.59880631770923,-0.148056790733748,
-3.81123860513795));
#67758=CARTESIAN_POINT('Ctrl Pts',(0.596576778298504,0.156799133531066,
-3.7973289751922));
#67759=CARTESIAN_POINT('Ctrl Pts',(0.448621644933921,0.423353802830726,
-3.78341934524643));
#67760=CARTESIAN_POINT('Ctrl Pts',(0.191081865280786,0.586495985759321,
-3.76950971530068));
#67761=CARTESIAN_POINT('Ctrl Pts',(-0.113133412488725,0.606375010134377,
-3.75560008535492));
#67762=CARTESIAN_POINT('Ctrl Pts',(-0.389713632522964,0.47813502891289,
-3.74169045540916));
#67763=CARTESIAN_POINT('Ctrl Pts',(-0.571098644850701,0.233101178361757,
-3.72778082546341));
#67764=CARTESIAN_POINT('Ctrl Pts',(-0.61298159820254,-0.0688722129692012,
-3.71387119551764));
#67765=CARTESIAN_POINT('Ctrl Pts',(-0.505131758776296,-0.354022213579012,
-3.69996156557189));
#67766=CARTESIAN_POINT('Ctrl Pts',(-0.27389356773763,-0.55269533652539,
-3.68605193562612));
#67767=CARTESIAN_POINT('Ctrl Pts',(0.0242485058037712,-0.616361769910605,
-3.67214230568037));
#67768=CARTESIAN_POINT('Ctrl Pts',(0.316467405623905,-0.52946973721973,
-3.6582326757346));
#67769=CARTESIAN_POINT('Ctrl Pts',(0.531382926990323,-0.313244323734379,
-3.64432304578885));
#67770=CARTESIAN_POINT('Ctrl Pts',(0.616497733406334,-0.0205028328487188,
-3.63041341584309));
#67771=CARTESIAN_POINT('Ctrl Pts',(0.551020861962079,0.27724687758871,-3.61650378589733));
#67772=CARTESIAN_POINT('Ctrl Pts',(0.350946324310309,0.507273593736863,
-3.60259415595157));
#67773=CARTESIAN_POINT('Ctrl Pts',(0.0651462552364883,0.613388773029548,
-3.58868452600582));
#67774=CARTESIAN_POINT('Ctrl Pts',(-0.236567065988548,0.569671699085858,
-3.57477489606005));
#67775=CARTESIAN_POINT('Ctrl Pts',(-0.480494235759622,0.386801125711496,
-3.5608652661143));
#67776=CARTESIAN_POINT('Ctrl Pts',(-0.6070512527398,0.109446781574009,-3.54695563616854));
#67777=CARTESIAN_POINT('Ctrl Pts',(-0.585324080267991,-0.194642088224266,
-3.53304600622278));
#67778=CARTESIAN_POINT('Ctrl Pts',(-0.420620006887823,-0.451185805689371,
-3.51913637627702));
#67779=CARTESIAN_POINT('Ctrl Pts',(-0.153171236899005,-0.597518529952587,
-3.50522674633126));
#67780=CARTESIAN_POINT('Ctrl Pts',(0.151692615602894,-0.597895619503463,
-3.4913171163855));
#67781=CARTESIAN_POINT('Ctrl Pts',(0.419502567879716,-0.452224962814082,
-3.47740748643974));
#67782=CARTESIAN_POINT('Ctrl Pts',(0.584840779969329,-0.196089478388676,
-3.46349785649398));
#67783=CARTESIAN_POINT('Ctrl Pts',(0.607320146739344,0.107944711840726,
-3.44958822654823));
#67784=CARTESIAN_POINT('Ctrl Pts',(0.481449641417571,0.385611286438515,
-3.43567859660246));
#67785=CARTESIAN_POINT('Ctrl Pts',(0.237975606711176,0.569084731881223,
-3.42176896665671));
#67786=CARTESIAN_POINT('Ctrl Pts',(-0.0636286431809187,0.613548056159279,
-3.40785933671094));
#67787=CARTESIAN_POINT('Ctrl Pts',(-0.349690347468453,0.508140219169145,
-3.39394970676519));
#67788=CARTESIAN_POINT('Ctrl Pts',(-0.55033331734186,0.27860915504229,-3.38004007681943));
#67789=CARTESIAN_POINT('Ctrl Pts',(-0.616546567282803,-0.0189776663915349,
-3.36613044687367));
#67790=CARTESIAN_POINT('Ctrl Pts',(-0.532156210730363,-0.311928820135262,
-3.35222081692791));
#67791=CARTESIAN_POINT('Ctrl Pts',(-0.317776249488288,-0.528685234058066,
-3.33831118698215));
#67792=CARTESIAN_POINT('Ctrl Pts',(-0.0257731989769087,-0.616299897504756,
-3.32440155703639));
#67793=CARTESIAN_POINT('Ctrl Pts',(0.272525461505833,-0.55337120839533,
-3.31049192709064));
#67794=CARTESIAN_POINT('Ctrl Pts',(0.504254426296432,-0.355270734807036,
-3.29658229714487));
#67795=CARTESIAN_POINT('Ctrl Pts',(0.612809345166734,-0.0703884076122953,
-3.28267266719912));
#67796=CARTESIAN_POINT('Ctrl Pts',(0.57167354743521,0.231687670394254,-3.26876303725335));
#67797=CARTESIAN_POINT('Ctrl Pts',(0.390895259502109,0.477169485139876,
-3.25485340730761));
#67798=CARTESIAN_POINT('Ctrl Pts',(0.114633128229106,0.606093282723282,
-3.24094377736183));
#67799=CARTESIAN_POINT('Ctrl Pts',(-0.189630395722162,0.586966893843369,
-3.22703414741608));
#67800=CARTESIAN_POINT('Ctrl Pts',(-0.447572971650981,0.424462314578555,
-3.21312451747032));
#67801=CARTESIAN_POINT('Ctrl Pts',(-0.596187060038844,0.158274479598307,
-3.19921488752456));
#67802=CARTESIAN_POINT('Ctrl Pts',(-0.599170751387531,-0.146575005139266,
-3.1853052575788));
#67803=CARTESIAN_POINT('Ctrl Pts',(-0.455795220492882,-0.415620666504591,
-3.17139562763305));
#67804=CARTESIAN_POINT('Ctrl Pts',(-0.201082756313209,-0.58314281832443,
-3.15748599768728));
#67805=CARTESIAN_POINT('Ctrl Pts',(0.102748119859029,-0.608220885300159,
-3.14357636774153));
#67806=CARTESIAN_POINT('Ctrl Pts',(0.38148075003927,-0.484729057102369,
-3.12966673779576));
#67807=CARTESIAN_POINT('Ctrl Pts',(0.567029215693361,-0.242832637839412,
-3.11575710785001));
#67808=CARTESIAN_POINT('Ctrl Pts',(0.614069660376893,0.0583804218422761,
-3.10184747790425));
#67809=CARTESIAN_POINT('Ctrl Pts',(0.511111531719077,0.345332917043329,
-3.0879378479585));
#67810=CARTESIAN_POINT('Ctrl Pts',(0.283304374485059,0.547931065780637,
-3.07402821801273));
#67811=CARTESIAN_POINT('Ctrl Pts',(-0.0137054396072017,0.616686291703527,
-3.06011858806698));
#67812=CARTESIAN_POINT('Ctrl Pts',(-0.307367430934806,0.534803780699439,
-3.04620895812121));
#67813=CARTESIAN_POINT('Ctrl Pts',(-0.525948891327989,0.322284944049105,
-3.03229932817546));
#67814=CARTESIAN_POINT('Ctrl Pts',(-0.616057006691815,0.0310416809434863,
-3.01838969822969));
#67815=CARTESIAN_POINT('Ctrl Pts',(-0.555681100350354,-0.267784122313653,
-3.00448006828394));
#67816=CARTESIAN_POINT('Ctrl Pts',(-0.359569173059506,-0.5011983950844,
-2.99057043833818));
#67817=CARTESIAN_POINT('Ctrl Pts',(-0.0756254142084532,-0.612185117571209,
-2.97666080839242));
#67818=CARTESIAN_POINT('Ctrl Pts',(0.226791337157252,-0.573633603304672,
-2.96275117844666));
#67819=CARTESIAN_POINT('Ctrl Pts',(0.47380985080692,-0.394960816699834,
-2.9488415485009));
#67820=CARTESIAN_POINT('Ctrl Pts',(0.605091003955021,-0.119811094572164,
-2.93493191855514));
#67821=CARTESIAN_POINT('Ctrl Pts',(0.588566796911201,0.184604840195385,
-2.92102228860939));
#67822=CARTESIAN_POINT('Ctrl Pts',(0.428273591740068,0.443927417567261,
-2.90711265866362));
#67823=CARTESIAN_POINT('Ctrl Pts',(0.163366151562832,0.594812005572706,
-2.89320302871787));
#67824=CARTESIAN_POINT('Ctrl Pts',(-0.141446679236782,0.600402080594964,
-2.87929339877211));
#67825=CARTESIAN_POINT('Ctrl Pts',(-0.411708380973339,0.459332157034739,
-2.86538376882635));
#67826=CARTESIAN_POINT('Ctrl Pts',(-0.581402225732933,0.206061333982548,
-2.85147413888059));
#67827=CARTESIAN_POINT('Ctrl Pts',(-0.609077159569785,-0.0975440164247773,
-2.83756450893483));
#67828=CARTESIAN_POINT('Ctrl Pts',(-0.487973036427672,-0.377322325299515,
-2.82365487898907));
#67829=CARTESIAN_POINT('Ctrl Pts',(-0.247671916566535,-0.564932246551864,
-2.80974524904331));
#67830=CARTESIAN_POINT('Ctrl Pts',(0.0531279325737788,-0.614546372725696,
-2.79583561909755));
#67831=CARTESIAN_POINT('Ctrl Pts',(0.340950240883056,-0.514045479205549,
-2.7819259891518));
#67832=CARTESIAN_POINT('Ctrl Pts',(0.545488757445549,-0.287978882820228,
-2.76801635920603));
#67833=CARTESIAN_POINT('Ctrl Pts',(0.616780932965306,0.00843221087987096,
-2.75410672926028));
#67834=CARTESIAN_POINT('Ctrl Pts',(0.537412253571372,0.302783571485002,
-2.74019709931452));
#67835=CARTESIAN_POINT('Ctrl Pts',(0.326770077808336,0.523174098841876,
-2.72628746936876));
#67836=CARTESIAN_POINT('Ctrl Pts',(0.0363078935924984,0.615769078724119,
-2.712377839423));
#67837=CARTESIAN_POINT('Ctrl Pts',(-0.263023206629647,0.557950368961374,
-2.69846820947724));
#67838=CARTESIAN_POINT('Ctrl Pts',(-0.498105723513708,0.363841324828228,
-2.68455857953148));
#67839=CARTESIAN_POINT('Ctrl Pts',(-0.611516135877317,0.0808568921709814,
-2.67064894958572));
#67840=CARTESIAN_POINT('Ctrl Pts',(-0.575551723403444,-0.221878424226423,
-2.65673931963997));
#67841=CARTESIAN_POINT('Ctrl Pts',(-0.398997500090059,-0.470415578368488,
-2.6428296896942));
#67842=CARTESIAN_POINT('Ctrl Pts',(-0.1249803020654,-0.604044489707105,
-2.62892005974845));
#67843=CARTESIAN_POINT('Ctrl Pts',(0.179565789039688,-0.59012367250978,
-2.61501042980268));
#67844=CARTESIAN_POINT('Ctrl Pts',(0.440249409948256,-0.432053559747037,
-2.60110079985693));
#67845=CARTESIAN_POINT('Ctrl Pts',(0.593393467078218,-0.168445880563364,
-2.58719116991117));
#67846=CARTESIAN_POINT('Ctrl Pts',(0.601589517108825,0.136308012804258,
-2.57328153996541));
#67847=CARTESIAN_POINT('Ctrl Pts',(0.462835513870151,0.407765997295543,
-2.55937191001965));
#67848=CARTESIAN_POINT('Ctrl Pts',(0.211024847435283,0.579619129441731,
-2.54546228007389));
#67849=CARTESIAN_POINT('Ctrl Pts',(-0.0923327819865527,0.609888906949863,
-2.53155265012813));
#67850=CARTESIAN_POINT('Ctrl Pts',(-0.373136316222966,0.491181342240755,
-2.51764302018237));
#67851=CARTESIAN_POINT('Ctrl Pts',(-0.5627939777567,0.252493089114664,-2.50373339023661));
#67852=CARTESIAN_POINT('Ctrl Pts',(-0.614978158355398,-0.0478715593612716,
-2.48982376029085));
#67853=CARTESIAN_POINT('Ctrl Pts',(-0.516941847140863,-0.336542639385364,
-2.4759141303451));
#67854=CARTESIAN_POINT('Ctrl Pts',(-0.292632338315525,-0.54300657088277,
-2.46200450039934));
#67855=CARTESIAN_POINT('Ctrl Pts',(0.00315836571155932,-0.616830484149337,
-2.44809487045358));
#67856=CARTESIAN_POINT('Ctrl Pts',(0.29817757689118,-0.539981438652459,
-2.43418524050782));
#67857=CARTESIAN_POINT('Ctrl Pts',(0.520361059452317,-0.331231322878041,
-2.42027561056206));
#67858=CARTESIAN_POINT('Ctrl Pts',(0.615436134650789,-0.0415714519348385,
-2.4063659806163));
#67859=CARTESIAN_POINT('Ctrl Pts',(0.560178848332374,0.258243062502926,
-2.39245635067054));
#67860=CARTESIAN_POINT('Ctrl Pts',(0.368086877795425,0.494976637675649,
-2.37854672072479));
#67861=CARTESIAN_POINT('Ctrl Pts',(0.0860824590500775,0.610802448991298,
-2.36463709077902));
#67862=CARTESIAN_POINT('Ctrl Pts',(-0.216949290762728,0.5774277675064,-2.35072746083327));
#67863=CARTESIAN_POINT('Ctrl Pts',(-0.466986915964566,0.403005014569022,
-2.3368178308875));
#67864=CARTESIAN_POINT('Ctrl Pts',(-0.60295381648548,0.130140372811313,
-2.32290820094175));
#67865=CARTESIAN_POINT('Ctrl Pts',(-0.591637406822937,-0.174513610637414,
-2.30899857099599));
#67866=CARTESIAN_POINT('Ctrl Pts',(-0.435801942263024,-0.436539217676546,
-2.29508894105023));
#67867=CARTESIAN_POINT('Ctrl Pts',(-0.173513295243778,-0.591931548258345,
-2.28117931110447));
#67868=CARTESIAN_POINT('Ctrl Pts',(0.131159381506471,-0.602732974120973,
-2.26726968115871));
#67869=CARTESIAN_POINT('Ctrl Pts',(0.403793803681125,-0.466305034884467,
-2.25336005121295));
#67870=CARTESIAN_POINT('Ctrl Pts',(0.577793659804967,-0.215972933811292,
-2.2394504212672));
#67871=CARTESIAN_POINT('Ctrl Pts',(0.610656068097196,0.0871147975142503,
-2.22554079132143));
#67872=CARTESIAN_POINT('Ctrl Pts',(0.494353739996816,0.368923028829912,
-2.21163116137568));
#67873=CARTESIAN_POINT('Ctrl Pts',(0.257295803029569,0.560614565627085,
-2.19772153142991));
#67874=CARTESIAN_POINT('Ctrl Pts',(-0.0426116864745436,0.615364985700089,
-2.18381190148416));
#67875=CARTESIAN_POINT('Ctrl Pts',(-0.33211043477016,0.5198004237846,-2.1699022715384));
#67876=CARTESIAN_POINT('Ctrl Pts',(-0.540484687553777,0.297264400777774,
-2.15599264159264));
#67877=CARTESIAN_POINT('Ctrl Pts',(-0.616834941633162,0.00211571035066239,
-2.14208301164688));
#67878=CARTESIAN_POINT('Ctrl Pts',(-0.542511148121141,-0.293549783876869,
-2.12817338170112));
#67879=CARTESIAN_POINT('Ctrl Pts',(-0.335668353116679,-0.517509978807957,
-2.11426375175536));
#67880=CARTESIAN_POINT('Ctrl Pts',(-0.0468319711754508,-0.615058198811867,
-2.10035412180961));
#67881=CARTESIAN_POINT('Ctrl Pts',(0.253444039388315,-0.562366375549258,
-2.08644449186384));
#67882=CARTESIAN_POINT('Ctrl Pts',(0.491811366323612,-0.372305521587819,
-2.07253486191809));
#67883=CARTESIAN_POINT('Ctrl Pts',(0.610044109087587,-0.0913017328280638,
-2.05862523197233));
#67884=CARTESIAN_POINT('Ctrl Pts',(0.5792615984644,0.212004297112923,-2.04471560202657));
#67885=CARTESIAN_POINT('Ctrl Pts',(0.406983067165381,0.46352411424923,-2.03080597208081));
#67886=CARTESIAN_POINT('Ctrl Pts',(0.135290929580357,0.60181906402436,-2.01689634213505));
#67887=CARTESIAN_POINT('Ctrl Pts',(-0.169448674330592,0.593107889188367,
-2.00298671218929));
#67888=CARTESIAN_POINT('Ctrl Pts',(-0.432797111987588,0.439518465260651,
-1.98907708224353));
#67889=CARTESIAN_POINT('Ctrl Pts',(-0.590426355987388,0.178568025148203,
-1.97516745229777));
#67890=CARTESIAN_POINT('Ctrl Pts',(-0.603832368038419,-0.126001161736678,
-1.96125782235201));
#67891=CARTESIAN_POINT('Ctrl Pts',(-0.46974046643662,-0.399792090519286,
-1.94734819240625));
#67892=CARTESIAN_POINT('Ctrl Pts',(-0.220905231378247,-0.575925950274512,
-1.9334385624605));
#67893=CARTESIAN_POINT('Ctrl Pts',(0.0818904444712269,-0.611378586928083,
-1.91952893251474));
#67894=CARTESIAN_POINT('Ctrl Pts',(0.364682771134822,-0.49748999777614,
-1.90561930256898));
#67895=CARTESIAN_POINT('Ctrl Pts',(0.558394169490021,-0.262079707206459,
-1.89170967262322));
#67896=CARTESIAN_POINT('Ctrl Pts',(0.615706826480567,0.0373486984392127,
-1.87780004267746));
#67897=CARTESIAN_POINT('Ctrl Pts',(0.522621000159094,0.327653951055963,
-1.8638904127317));
#67898=CARTESIAN_POINT('Ctrl Pts',(0.301874731577736,0.537923291822119,
-1.84998078278594));
#67899=CARTESIAN_POINT('Ctrl Pts',(0.00738963174281488,0.616794305090912,
-1.83607115284018));
#67900=CARTESIAN_POINT('Ctrl Pts',(-0.288900530759199,0.545001197041739,
-1.82216152289442));
#67901=CARTESIAN_POINT('Ctrl Pts',(-0.514621065338475,0.340080844152928,
-1.80825189294867));
#67902=CARTESIAN_POINT('Ctrl Pts',(-0.614635298836539,0.052089066741446,
-1.79434226300291));
#67903=CARTESIAN_POINT('Ctrl Pts',(-0.564512790691757,-0.248626488120793,
-1.78043263305715));
#67904=CARTESIAN_POINT('Ctrl Pts',(-0.376496947799364,-0.488610140856324,
-1.76652300311139));
#67905=CARTESIAN_POINT('Ctrl Pts',(-0.0965143319473462,-0.609241171605,
-1.75261337316563));
#67906=CARTESIAN_POINT('Ctrl Pts',(0.207043804783216,-0.581053082214322,
-1.73870374321987));
#67907=CARTESIAN_POINT('Ctrl Pts',(0.460027426372314,-0.410931367061632,
-1.72479411327411));
#67908=CARTESIAN_POINT('Ctrl Pts',(0.600640315280387,-0.140431595838519,
-1.71088448332835));
#67909=CARTESIAN_POINT('Ctrl Pts',(0.594535012105725,0.164371350393919,
-1.69697485338259));
#67910=CARTESIAN_POINT('Ctrl Pts',(0.443202857041646,0.429023366449892,
-1.68306522343683));
#67911=CARTESIAN_POINT('Ctrl Pts',(0.183609700748073,0.588878000303185,
-1.66915559349108));
#67912=CARTESIAN_POINT('Ctrl Pts',(-0.120833730589114,0.604887618489413,
-1.65524596354532));
#67913=CARTESIAN_POINT('Ctrl Pts',(-0.39576115035726,0.473141557377675,
-1.64133633359956));
#67914=CARTESIAN_POINT('Ctrl Pts',(-0.574016137390193,0.225821379558084,
-1.6274267036538));
#67915=CARTESIAN_POINT('Ctrl Pts',(-0.61205641062243,-0.0766601047864005,
-1.61351707370804));
#67916=CARTESIAN_POINT('Ctrl Pts',(-0.500589886301045,-0.360415853123835,
-1.59960744376228));
#67917=CARTESIAN_POINT('Ctrl Pts',(-0.266844451915646,-0.556132951668676,
-1.58569781381652));
#67918=CARTESIAN_POINT('Ctrl Pts',(0.0320829800086549,-0.616003655706393,
-1.57178818387076));
#67919=CARTESIAN_POINT('Ctrl Pts',(0.323173514036252,-0.525403370064692,
-1.557878553925));
#67920=CARTESIAN_POINT('Ctrl Pts',(0.53532257093991,-0.306462993674867,
-1.54396892397925));
#67921=CARTESIAN_POINT('Ctrl Pts',(0.61670857749334,-0.0126630129122495,
-1.53005929403348));
#67922=CARTESIAN_POINT('Ctrl Pts',(0.54745140337799,0.284230157424129,-1.51614966408773));
#67923=CARTESIAN_POINT('Ctrl Pts',(0.344468473409441,0.511694530239325,
-1.50224003414196));
#67924=CARTESIAN_POINT('Ctrl Pts',(0.0573423543102443,0.614167465641117,
-1.48833040419621));
#67925=CARTESIAN_POINT('Ctrl Pts',(-0.243790760889837,0.566617936845128,
-1.47442077425045));
#67926=CARTESIAN_POINT('Ctrl Pts',(-0.485373195300982,0.38066085001375,
-1.46051114430469));
#67927=CARTESIAN_POINT('Ctrl Pts',(-0.608393695242684,0.101719875338241,
-1.44660151435893));
#67928=CARTESIAN_POINT('Ctrl Pts',(-0.582802087788846,-0.202068176412908,
-1.43269188441317));
#67929=CARTESIAN_POINT('Ctrl Pts',(-0.414849625615314,-0.456497107960948,
-1.41878225446741));
#67930=CARTESIAN_POINT('Ctrl Pts',(-0.145561995774814,-0.599417656426576,
-1.40487262452166));
#67931=CARTESIAN_POINT('Ctrl Pts',(0.159282010007692,-0.595918671244479,
-1.3909629945759));
#67932=CARTESIAN_POINT('Ctrl Pts',(0.425218256945002,-0.446854848256713,
-1.37705336463014));
#67933=CARTESIAN_POINT('Ctrl Pts',(0.587286594399046,-0.188637953469192,
-1.36314373468438));
#67934=CARTESIAN_POINT('Ctrl Pts',(0.60589864832935,0.115657465831397,-1.34923410473862));
#67935=CARTESIAN_POINT('Ctrl Pts',(0.47650805906919,0.391701277878931,-1.33532447479286));
#67936=CARTESIAN_POINT('Ctrl Pts',(0.230721018953334,0.572064360769845,
-1.3214148448471));
#67937=CARTESIAN_POINT('Ctrl Pts',(-0.0714241608263882,0.612689489627594,
-1.30750521490134));
#67938=CARTESIAN_POINT('Ctrl Pts',(-0.356122586732152,0.503653178952617,
-1.29359558495559));
#67939=CARTESIAN_POINT('Ctrl Pts',(-0.553831077470514,0.271589688828064,
-1.27968595500982));
#67940=CARTESIAN_POINT('Ctrl Pts',(-0.616255451677714,-0.0268149161358486,
-1.26577632506407));
#67941=CARTESIAN_POINT('Ctrl Pts',(-0.528147330094856,-0.318669451255607,
-1.2518666951183));
#67942=CARTESIAN_POINT('Ctrl Pts',(-0.311028851641987,-0.53268271503414,
-1.23795706517255));
#67943=CARTESIAN_POINT('Ctrl Pts',(-0.0179354683458115,-0.616577765107606,
-1.22404743522679));
#67944=CARTESIAN_POINT('Ctrl Pts',(0.279539005301622,-0.54986158800634,
-1.21013780528103));
#67945=CARTESIAN_POINT('Ctrl Pts',(0.508730587456313,-0.348830920126398,
-1.19622817533527));
#67946=CARTESIAN_POINT('Ctrl Pts',(0.613654733426786,-0.0625914498376293,
-1.18231854538951));
#67947=CARTESIAN_POINT('Ctrl Pts',(0.568681660111602,0.238937211213715,
-1.16840891544375));
#67948=CARTESIAN_POINT('Ctrl Pts',(0.384796923826821,0.482100766296105,
-1.15449928549799));
#67949=CARTESIAN_POINT('Ctrl Pts',(0.106917982446909,0.607501741955822,
-1.14058965555223));
#67950=CARTESIAN_POINT('Ctrl Pts',(-0.197077775747773,0.584508487326049,
-1.12668002560648));
#67951=CARTESIAN_POINT('Ctrl Pts',(-0.452933417100812,0.418737556380195,
-1.11277039566072));
#67952=CARTESIAN_POINT('Ctrl Pts',(-0.598151176846013,0.150681754328804,
-1.09886076571496));
#67953=CARTESIAN_POINT('Ctrl Pts',(-0.597258765451536,-0.154181025230674,
-1.0849511357692));
#67954=CARTESIAN_POINT('Ctrl Pts',(-0.45047417192522,-0.421382061647338,
-1.07104150582344));
#67955=CARTESIAN_POINT('Ctrl Pts',(-0.193652415718641,-0.585652254615492,
-1.05713187587768));
#67956=CARTESIAN_POINT('Ctrl Pts',(0.110472745876953,-0.606865383646391,
-1.04322224593192));
#67957=CARTESIAN_POINT('Ctrl Pts',(0.387612769883316,-0.479839725401367,
-1.02931261598616));
#67958=CARTESIAN_POINT('Ctrl Pts',(0.570070763099067,-0.235603791373405,
-1.0154029860404));
#67959=CARTESIAN_POINT('Ctrl Pts',(0.613277777662018,0.0661829953674764,
-1.00149335609464));
#67960=CARTESIAN_POINT('Ctrl Pts',(0.506679651787328,0.351803285821137,
-0.987583726148887));
#67961=CARTESIAN_POINT('Ctrl Pts',(0.276315071040818,0.55148871517519,-0.973674096203127));
#67962=CARTESIAN_POINT('Ctrl Pts',(-0.021544891945215,0.61646219598686,
-0.959764466257368));
#67963=CARTESIAN_POINT('Ctrl Pts',(-0.314142091985768,0.530852679651031,
-0.94585483631161));
#67964=CARTESIAN_POINT('Ctrl Pts',(-0.530003917092785,0.315571971689786,
-0.931945206365851));
#67965=CARTESIAN_POINT('Ctrl Pts',(-0.616401877496817,0.0232066125980274,
-0.918035576420091));
#67966=CARTESIAN_POINT('Ctrl Pts',(-0.552231574729038,-0.274827417340706,
-0.904125946474334));
#67967=CARTESIAN_POINT('Ctrl Pts',(-0.353167865384941,-0.505729453669963,
-0.890216316528573));
#67968=CARTESIAN_POINT('Ctrl Pts',(-0.0678359695858457,-0.613097139677086,
-0.876306686582815));
#67969=CARTESIAN_POINT('Ctrl Pts',(0.234066193913592,-0.570703809621663,
-0.862397056637055));
#67970=CARTESIAN_POINT('Ctrl Pts',(0.478793093074244,-0.388904866868846,
-0.848487426691297));
#67971=CARTESIAN_POINT('Ctrl Pts',(0.6065653769511,-0.112108273263145,-0.834577796745537));
#67972=CARTESIAN_POINT('Ctrl Pts',(0.586172156078744,0.192072967613535,
-0.820668166799778));
#67973=CARTESIAN_POINT('Ctrl Pts',(0.422594875127169,0.449336614317292,
-0.806758536854021));
#67974=CARTESIAN_POINT('Ctrl Pts',(0.155790497218003,0.596840969125313,
-0.79284890690826));
#67975=CARTESIAN_POINT('Ctrl Pts',(-0.149068768972891,0.598555196758647,
-0.778939276962503));
#67976=CARTESIAN_POINT('Ctrl Pts',(-0.417515061003882,0.454060563454701,
-0.765029647016743));
#67977=CARTESIAN_POINT('Ctrl Pts',(-0.583975100431752,0.198652720911643,
-0.751120017070985));
#67978=CARTESIAN_POINT('Ctrl Pts',(-0.607787753766864,-0.105279949757325,
-0.737210387125225));
#67979=CARTESIAN_POINT('Ctrl Pts',(-0.48313631281108,-0.383495925262826,
-0.723300757179466));
#67980=CARTESIAN_POINT('Ctrl Pts',(-0.240469339860789,-0.568035490120813,
-0.709391127233706));
#67981=CARTESIAN_POINT('Ctrl Pts',(0.0609369915676775,-0.613821231718611,
-0.695481497287948));
#67982=CARTESIAN_POINT('Ctrl Pts',(0.34745826615543,-0.509669083553375,
-0.681571867342189));
#67983=CARTESIAN_POINT('Ctrl Pts',(0.549106036022265,-0.281020253102492,
-0.667662237396431));
#67984=CARTESIAN_POINT('Ctrl Pts',(0.616623873519691,0.0162732927045065,
-0.653752607450671));
#67985=CARTESIAN_POINT('Ctrl Pts',(0.533519220957275,0.309591767201617,
-0.639842977504913));
#67986=CARTESIAN_POINT('Ctrl Pts',(0.320092021691175,0.527286372950726,
-0.625933347559153));
#67987=CARTESIAN_POINT('Ctrl Pts',(0.0284760603192387,0.61618092751932,
-0.612023717613395));
#67988=CARTESIAN_POINT('Ctrl Pts',(-0.270095737984369,0.554561190287018,
-0.598114087667635));
#67989=CARTESIAN_POINT('Ctrl Pts',(-0.502691348279656,0.357478992130528,
-0.584204457721876));
#67990=CARTESIAN_POINT('Ctrl Pts',(-0.612494725155188,0.0730755301516669,
-0.570294827776117));
#67991=CARTESIAN_POINT('Ctrl Pts',(-0.572684237545063,-0.229178065087615,
-0.556385197830358));
#67992=CARTESIAN_POINT('Ctrl Pts',(-0.392984378826605,-0.475450417444492,
-0.542475567884599));
#67993=CARTESIAN_POINT('Ctrl Pts',(-0.117290368348157,-0.60558466868195,
-0.52856593793884));
#67994=CARTESIAN_POINT('Ctrl Pts',(0.187054117889196,-0.587792972423601,
-0.514656307993082));
#67995=CARTESIAN_POINT('Ctrl Pts',(0.44570696255647,-0.426421299865004,
-0.500746678047323));
#67996=CARTESIAN_POINT('Ctrl Pts',(0.595487129047879,-0.160887850965181,
-0.486837048101563));
#67997=CARTESIAN_POINT('Ctrl Pts',(0.599807870389539,0.143945614968422,
-0.472927418155804));
#67998=CARTESIAN_POINT('Ctrl Pts',(0.457613760660216,0.413617537713629,
-0.459017788210046));
#67999=CARTESIAN_POINT('Ctrl Pts',(0.203638503498379,0.58225525445705,-0.445108158264286));
#68000=CARTESIAN_POINT('Ctrl Pts',(-0.100079457094422,0.608665691260386,
-0.431198528318528));
#68001=CARTESIAN_POINT('Ctrl Pts',(-0.379351044981491,0.486397580299782,
-0.417288898372769));
#68002=CARTESIAN_POINT('Ctrl Pts',(-0.565958690624595,0.245317308716941,
-0.40337926842701));
#68003=CARTESIAN_POINT('Ctrl Pts',(-0.61431981206814,-0.0556865329382699,
-0.389469638481251));
#68004=CARTESIAN_POINT('Ctrl Pts',(-0.512621255706389,-0.343087845380705,
-0.375560008535491));
#68005=CARTESIAN_POINT('Ctrl Pts',(-0.2857048910393,-0.546683214197066,
-0.361650378589733));
#68006=CARTESIAN_POINT('Ctrl Pts',(0.0110005037984258,-0.61674047245988,
-0.347740748643974));
#68007=CARTESIAN_POINT('Ctrl Pts',(0.305018809553407,-0.536146759068512,
-0.333831118698214));
#68008=CARTESIAN_POINT('Ctrl Pts',(0.524530281282194,-0.324588671217872,
-0.319921488752457));
#68009=CARTESIAN_POINT('Ctrl Pts',(0.615914931314421,-0.0337434262600359,
-0.306011858806697));
#68010=CARTESIAN_POINT('Ctrl Pts',(0.55685026439868,0.265344313097788,-0.292102228860939));
#68011=CARTESIAN_POINT('Ctrl Pts',(0.361763985145107,0.499616493478627,
-0.278192598915179));
#68012=CARTESIAN_POINT('Ctrl Pts',(0.0783097485940909,0.61184753372299,
-0.26428296896942));
#68013=CARTESIAN_POINT('Ctrl Pts',(-0.224273182279628,0.574622799449323,
-0.250373339023661));
#68014=CARTESIAN_POINT('Ctrl Pts',(-0.47207298339421,0.397035160785883,
-0.236463709077903));
#68015=CARTESIAN_POINT('Ctrl Pts',(-0.60455968958736,0.122463890190093,
-0.222554079132143));
#68016=CARTESIAN_POINT('Ctrl Pts',(-0.58937081641643,-0.182021596075152,
-0.208644449186384));
#68017=CARTESIAN_POINT('Ctrl Pts',(-0.430216553701672,-0.442044722094857,
-0.194734819240625));
#68018=CARTESIAN_POINT('Ctrl Pts',(-0.165973437374469,-0.594089765496738,
-0.180825189294867));
#68019=CARTESIAN_POINT('Ctrl Pts',(0.138811926899389,-0.601016675400649,
-0.166915559349108));
#68020=CARTESIAN_POINT('Ctrl Pts',(0.409689797907612,-0.461133541629717,
-0.153005929403349));
#68021=CARTESIAN_POINT('Ctrl Pts',(0.580492800990502,-0.208609325030388,
-0.13909629945759));
#68022=CARTESIAN_POINT('Ctrl Pts',(0.609499212910961,0.0948715035369464,
-0.12518666951183));
#68023=CARTESIAN_POINT('Ctrl Pts',(0.489623131224122,0.375178714510168,
-0.111277039566072));
#68024=CARTESIAN_POINT('Ctrl Pts',(0.250147652741445,0.563839964446146,
-0.0973674096203128));
#68025=CARTESIAN_POINT('Ctrl Pts',(-0.0504326075969051,0.614774560998643,
-0.0834577796745534));
#68026=CARTESIAN_POINT('Ctrl Pts',(-0.338691162031732,0.515533844114401,
-0.0695481497287943));
#68027=CARTESIAN_POINT('Ctrl Pts',(-0.544222735363936,0.290372764715117,
-0.0556385197830353));
#68028=CARTESIAN_POINT('Ctrl Pts',(-0.61680746585949,-0.00573499015792564,
-0.0417288898372768));
#68029=CARTESIAN_POINT('Ctrl Pts',(-0.538744006451602,-0.300407514267951,
-0.0278192598915181));
#68030=CARTESIAN_POINT('Ctrl Pts',(-0.329043395961403,-0.521769848422279,
-0.0139096299457593));
#68031=CARTESIAN_POINT('Ctrl Pts',(-0.135716027844311,-0.584261894770184,
-0.00463654331525315));
#68032=CARTESIAN_POINT('Ctrl Pts',(-0.0374170035146652,-0.590490705661811,
0.));
#68033=CARTESIAN_POINT('Ctrl Pts',(0.324375760296889,-0.454512507566726,
-3.98675728291906));
#68034=CARTESIAN_POINT('Ctrl Pts',(0.400038485571038,-0.400513654667537,
-3.9821207396038));
#68035=CARTESIAN_POINT('Ctrl Pts',(0.52379810564881,-0.254053407725315,
-3.97284765297329));
#68036=CARTESIAN_POINT('Ctrl Pts',(0.581471950593503,0.0278744202397417,
-3.95893802302754));
#68037=CARTESIAN_POINT('Ctrl Pts',(0.497114145262111,0.302917967212516,
-3.94502839308178));
#68038=CARTESIAN_POINT('Ctrl Pts',(0.291324666108956,0.504004920085947,
-3.93111876313602));
#68039=CARTESIAN_POINT('Ctrl Pts',(0.0143742891377185,0.581959948381398,
-3.91720913319026));
#68040=CARTESIAN_POINT('Ctrl Pts',(-0.26608773317726,0.517769450825752,
-3.9032995032445));
#68041=CARTESIAN_POINT('Ctrl Pts',(-0.48155237504841,0.327098675931684,
-3.88938987329875));
#68042=CARTESIAN_POINT('Ctrl Pts',(-0.579388508604397,0.0565301441845764,
-3.87548024335298));
#68043=CARTESIAN_POINT('Ctrl Pts',(-0.535697561949923,-0.227848273936975,
-3.86157061340723));
#68044=CARTESIAN_POINT('Ctrl Pts',(-0.36115199634089,-0.456569617418363,
-3.84766098346147));
#68045=CARTESIAN_POINT('Ctrl Pts',(-0.098387947990684,-0.573765203358985,
-3.8337513535157));
#68046=CARTESIAN_POINT('Ctrl Pts',(0.188409280812262,-0.550807198412802,
-3.81984172356995));
#68047=CARTESIAN_POINT('Ctrl Pts',(0.429183846950857,-0.393303807123812,
-3.80593209362419));
#68048=CARTESIAN_POINT('Ctrl Pts',(0.565121828294565,-0.139728192232451,
-3.79202246367843));
#68049=CARTESIAN_POINT('Ctrl Pts',(0.563017706559736,0.147978754391011,
-3.77811283373267));
#68050=CARTESIAN_POINT('Ctrl Pts',(0.423385453192029,0.399538996158907,
-3.76420320378691));
#68051=CARTESIAN_POINT('Ctrl Pts',(0.180332988927896,0.553503986109699,
-3.75029357384115));
#68052=CARTESIAN_POINT('Ctrl Pts',(-0.106769349313841,0.572264761117087,
-3.7363839438954));
#68053=CARTESIAN_POINT('Ctrl Pts',(-0.367791177229423,0.451238628785029,
-3.72247431394964));
#68054=CARTESIAN_POINT('Ctrl Pts',(-0.53897278764399,0.2199886009843,-3.70856468400387));
#68055=CARTESIAN_POINT('Ctrl Pts',(-0.578499710578128,-0.064997963048793,
-3.69465505405812));
#68056=CARTESIAN_POINT('Ctrl Pts',(-0.476716718924004,-0.334107497997054,
-3.68074542411236));
#68057=CARTESIAN_POINT('Ctrl Pts',(-0.258486307142088,-0.521604715631567,
-3.6668357941666));
#68058=CARTESIAN_POINT('Ctrl Pts',(0.0228844611821437,-0.581689738403682,
-3.65292616422084));
#68059=CARTESIAN_POINT('Ctrl Pts',(0.298665250470289,-0.499685619665673,
-3.63901653427508));
#68060=CARTESIAN_POINT('Ctrl Pts',(0.501491187290892,-0.295623475732306,
-3.62510690432932));
#68061=CARTESIAN_POINT('Ctrl Pts',(0.581818053581754,-0.0193494925521338,
-3.61119727438356));
#68062=CARTESIAN_POINT('Ctrl Pts',(0.520024434831806,0.261650984163416,
-3.5972876444378));
#68063=CARTESIAN_POINT('Ctrl Pts',(0.331204635893308,0.478738069823327,
-3.58337801449205));
#68064=CARTESIAN_POINT('Ctrl Pts',(0.0614816006060668,0.578883980710003,
-3.56946838454629));
#68065=CARTESIAN_POINT('Ctrl Pts',(-0.223259522974249,0.537626111472319,
-3.55555875460053));
#68066=CARTESIAN_POINT('Ctrl Pts',(-0.453465123808749,0.365042506873849,
-3.54164912465477));
#68067=CARTESIAN_POINT('Ctrl Pts',(-0.5729029632306,0.103290101448284,-3.52773949470901));
#68068=CARTESIAN_POINT('Ctrl Pts',(-0.552398003500193,-0.183692939615547,
-3.51382986476325));
#68069=CARTESIAN_POINT('Ctrl Pts',(-0.396958983697868,-0.425805372907814,
-3.49992023481749));
#68070=CARTESIAN_POINT('Ctrl Pts',(-0.144554936844433,-0.563906482113393,
-3.48601060487173));
#68071=CARTESIAN_POINT('Ctrl Pts',(0.143159492031142,-0.564262359348016,
-3.47210097492597));
#68072=CARTESIAN_POINT('Ctrl Pts',(0.395904403683274,-0.426786074608572,
-3.45819134498022));
#68073=CARTESIAN_POINT('Ctrl Pts',(0.551941890162178,-0.185058910133518,
-3.44428171503445));
#68074=CARTESIAN_POINT('Ctrl Pts',(0.573156731208902,0.101872527236398,
-3.4303720850887));
#68075=CARTESIAN_POINT('Ctrl Pts',(0.454366785291294,0.36391959930685,-3.41646245514293));
#68076=CARTESIAN_POINT('Ctrl Pts',(0.224588829437554,0.537072162774681,
-3.40255282519718));
#68077=CARTESIAN_POINT('Ctrl Pts',(-0.0600493583699365,0.57903430372903,
-3.38864319525142));
#68078=CARTESIAN_POINT('Ctrl Pts',(-0.330019311176162,0.479555945210164,
-3.37473356530566));
#68079=CARTESIAN_POINT('Ctrl Pts',(-0.51937556647267,0.262936629792801,
-3.3608239353599));
#68080=CARTESIAN_POINT('Ctrl Pts',(-0.581864140419413,-0.0179101208700953,
-3.34691430541415));
#68081=CARTESIAN_POINT('Ctrl Pts',(-0.50222097171039,-0.294381972800433,
-3.33300467546838));
#68082=CARTESIAN_POINT('Ctrl Pts',(-0.299900468295682,-0.498945246947632,
-3.31909504552263));
#68083=CARTESIAN_POINT('Ctrl Pts',(-0.0243233862036543,-0.581631346489502,
-3.30518541557686));
#68084=CARTESIAN_POINT('Ctrl Pts',(0.257195160619166,-0.522242567864479,
-3.29127578563111));
#68085=CARTESIAN_POINT('Ctrl Pts',(0.475888738790229,-0.335285786498994,
-3.27736615568535));
#68086=CARTESIAN_POINT('Ctrl Pts',(0.578337147245635,-0.0664288676057664,
-3.26345652573959));
#68087=CARTESIAN_POINT('Ctrl Pts',(0.539515350389306,0.218654606697199,
-3.24954689579383));
#68088=CARTESIAN_POINT('Ctrl Pts',(0.368906334466525,0.450327399484059,
-3.23563726584807));
#68089=CARTESIAN_POINT('Ctrl Pts',(0.108184701951348,0.571998881641653,
-3.22172763590231));
#68090=CARTESIAN_POINT('Ctrl Pts',(-0.178963168492766,0.553948404328989,
-3.20781800595655));
#68091=CARTESIAN_POINT('Ctrl Pts',(-0.422395770642912,0.400585151095974,
-3.19390837601079));
#68092=CARTESIAN_POINT('Ctrl Pts',(-0.562649911015658,0.149371108215993,
-3.17999874606504));
#68093=CARTESIAN_POINT('Ctrl Pts',(-0.565465761583983,-0.138329761121207,
-3.16608911611927));
#68094=CARTESIAN_POINT('Ctrl Pts',(-0.430155495550294,-0.392240869853568,
-3.15217948617352));
#68095=CARTESIAN_POINT('Ctrl Pts',(-0.189771302548966,-0.550339443493261,
-3.13826985622776));
#68096=CARTESIAN_POINT('Ctrl Pts',(0.0969682577343136,-0.574006800767704,
-3.124360226282));
#68097=CARTESIAN_POINT('Ctrl Pts',(0.360021416851612,-0.457461724894838,
-3.11045059633624));
#68098=CARTESIAN_POINT('Ctrl Pts',(0.53513227498155,-0.22917263931079,-3.09654096639048));
#68099=CARTESIAN_POINT('Ctrl Pts',(0.579526566286031,0.0550963638031215,
-3.08263133644472));
#68100=CARTESIAN_POINT('Ctrl Pts',(0.482360113320941,0.325906998103159,
-3.06872170649896));
#68101=CARTESIAN_POINT('Ctrl Pts',(0.267367730329437,0.517108448117112,
-3.05481207655321));
#68102=CARTESIAN_POINT('Ctrl Pts',(-0.0129344712294171,0.581996004960188,
-3.04090244660744));
#68103=CARTESIAN_POINT('Ctrl Pts',(-0.290077174189779,0.504719608643924,
-3.02699281666169));
#68104=CARTESIAN_POINT('Ctrl Pts',(-0.496362830963149,0.30415553648397,
-3.01308318671593));
#68105=CARTESIAN_POINT('Ctrl Pts',(-0.581402118947598,0.0292955016827951,
-2.99917355677017));
#68106=CARTESIAN_POINT('Ctrl Pts',(-0.524422522093719,-0.252720534694878,
-2.98526392682441));
#68107=CARTESIAN_POINT('Ctrl Pts',(-0.339342425870034,-0.473004617673278,
-2.97135429687865));
#68108=CARTESIAN_POINT('Ctrl Pts',(-0.0713712782899644,-0.577748034155773,
-2.95744466693289));
#68109=CARTESIAN_POINT('Ctrl Pts',(0.214033705566062,-0.541365147767442,
-2.94353503698713));
#68110=CARTESIAN_POINT('Ctrl Pts',(0.447156753750219,-0.372743192977644,
-2.92962540704137));
#68111=CARTESIAN_POINT('Ctrl Pts',(0.571052983789159,-0.113071393557795,
-2.91571577709561));
#68112=CARTESIAN_POINT('Ctrl Pts',(0.555458308483385,0.174220314178282,
-2.90180614714986));
#68113=CARTESIAN_POINT('Ctrl Pts',(0.404182033516805,0.418955288924514,
-2.8878965172041));
#68114=CARTESIAN_POINT('Ctrl Pts',(0.154176359738182,0.561352207115539,
-2.87398688725834));
#68115=CARTESIAN_POINT('Ctrl Pts',(-0.133489917545092,0.566627825163402,
-2.86007725731258));
#68116=CARTESIAN_POINT('Ctrl Pts',(-0.388548661059429,0.433493469759958,
-2.84616762736682));
#68117=CARTESIAN_POINT('Ctrl Pts',(-0.548696763984826,0.194469821638688,
-2.83225799742106));
#68118=CARTESIAN_POINT('Ctrl Pts',(-0.574814907273033,-0.092056899319377,
-2.8183483674753));
#68119=CARTESIAN_POINT('Ctrl Pts',(-0.46052322153081,-0.356096914851124,
-2.80443873752954));
#68120=CARTESIAN_POINT('Ctrl Pts',(-0.23373969540392,-0.533153266076544,
-2.79052910758379));
#68121=CARTESIAN_POINT('Ctrl Pts',(0.0501393413891527,-0.579976462264345,
-2.77661947763802));
#68122=CARTESIAN_POINT('Ctrl Pts',(0.3217708594365,-0.48512901825504,-2.76270984769227));
#68123=CARTESIAN_POINT('Ctrl Pts',(0.51480352629053,-0.271779284814791,
-2.74880021774651));
#68124=CARTESIAN_POINT('Ctrl Pts',(0.58208532239273,0.00795787600776863,
-2.73489058780075));
#68125=CARTESIAN_POINT('Ctrl Pts',(0.507181347798721,0.285751169342622,
-2.72098095785499));
#68126=CARTESIAN_POINT('Ctrl Pts',(0.308388369230054,0.493744128126331,
-2.70707132790923));
#68127=CARTESIAN_POINT('Ctrl Pts',(0.0342654754996764,0.581130387713793,
-2.69316169796347));
#68128=CARTESIAN_POINT('Ctrl Pts',(-0.248227433509849,0.526564138152911,
-2.67925206801771));
#68129=CARTESIAN_POINT('Ctrl Pts',(-0.470085917317827,0.343374257443769,
-2.66534243807196));
#68130=CARTESIAN_POINT('Ctrl Pts',(-0.577116684507702,0.0763084713412617,
-2.65143280812619));
#68131=CARTESIAN_POINT('Ctrl Pts',(-0.543175368376425,-0.209397157394121,
-2.63752317818044));
#68132=CARTESIAN_POINT('Ctrl Pts',(-0.376552801911728,-0.443953418398857,
-2.62361354823468));
#68133=CARTESIAN_POINT('Ctrl Pts',(-0.117949819023622,-0.570065338823453,
-2.60970391828892));
#68134=CARTESIAN_POINT('Ctrl Pts',(0.169464723400831,-0.556927605581088,
-2.59579428834316));
#68135=CARTESIAN_POINT('Ctrl Pts',(0.415484179270755,-0.407749368008474,
-2.5818846583974));
#68136=CARTESIAN_POINT('Ctrl Pts',(0.560013465282322,-0.158970340120692,
-2.56797502845164));
#68137=CARTESIAN_POINT('Ctrl Pts',(0.567748465133041,0.128640315121969,
-2.55406539850589));
#68138=CARTESIAN_POINT('Ctrl Pts',(0.436799753213296,0.384828047221623,
-2.54015576856012));
#68139=CARTESIAN_POINT('Ctrl Pts',(0.199154123915099,0.54701397172578,-2.52624613861437));
#68140=CARTESIAN_POINT('Ctrl Pts',(-0.0871388110389003,0.575580991647856,
-2.5123365086686));
#68141=CARTESIAN_POINT('Ctrl Pts',(-0.352146380208058,0.46355105138697,
-2.49842687872284));
#68142=CARTESIAN_POINT('Ctrl Pts',(-0.531135280736092,0.238289663840034,
-2.48451724877709));
#68143=CARTESIAN_POINT('Ctrl Pts',(-0.580383958774104,-0.0451786535136231,
-2.47060761883133));
#68144=CARTESIAN_POINT('Ctrl Pts',(-0.487862457590284,-0.317611197550671,
-2.45669798888557));
#68145=CARTESIAN_POINT('Ctrl Pts',(-0.276170970739966,-0.512460969495384,
-2.44278835893981));
#68146=CARTESIAN_POINT('Ctrl Pts',(0.00298069902162641,-0.582132086187444,
-2.42887872899405));
#68147=CARTESIAN_POINT('Ctrl Pts',(0.281404274513702,-0.509606009208113,
-2.41496909904829));
#68148=CARTESIAN_POINT('Ctrl Pts',(0.491089329878754,-0.312598657090589,
-2.40105946910253));
#68149=CARTESIAN_POINT('Ctrl Pts',(0.580816172653138,-0.0392329443218781,
-2.38714983915677));
#68150=CARTESIAN_POINT('Ctrl Pts',(0.528667259478138,0.243716185534479,
-2.37324020921101));
#68151=CARTESIAN_POINT('Ctrl Pts',(0.347380986471149,0.467132851096918,
-2.35933057926526));
#68152=CARTESIAN_POINT('Ctrl Pts',(0.0812400858236996,0.576443144456556,
-2.3454209493195));
#68153=CARTESIAN_POINT('Ctrl Pts',(-0.20474530113855,0.544945879879174,
-2.33151131937374));
#68154=CARTESIAN_POINT('Ctrl Pts',(-0.44071762761141,0.380334882765405,
-2.31760168942798));
#68155=CARTESIAN_POINT('Ctrl Pts',(-0.569036018946812,0.122819621709097,
-2.30369205948222));
#68156=CARTESIAN_POINT('Ctrl Pts',(-0.558356188208398,-0.164696743820245,
-2.28978242953646));
#68157=CARTESIAN_POINT('Ctrl Pts',(-0.411286893779221,-0.41198269543883,
-2.2758727995907));
#68158=CARTESIAN_POINT('Ctrl Pts',(-0.163752698897196,-0.558633783385402,
-2.26196316964495));
#68159=CARTESIAN_POINT('Ctrl Pts',(0.123781308384447,-0.568827599567951,
-2.24805353969918));
#68160=CARTESIAN_POINT('Ctrl Pts',(0.381079300337477,-0.440074104202806,
-2.23414390975343));
#68161=CARTESIAN_POINT('Ctrl Pts',(0.545291189737489,-0.203823866929948,
-2.22023427980766));
#68162=CARTESIAN_POINT('Ctrl Pts',(0.576304997887196,0.0822143524321826,
-2.20632464986191));
#68163=CARTESIAN_POINT('Ctrl Pts',(0.466544993112303,0.348170101728228,
-2.19241501991615));
#68164=CARTESIAN_POINT('Ctrl Pts',(0.242822211991412,0.529078466486023,
-2.17850538997039));
#68165=CARTESIAN_POINT('Ctrl Pts',(-0.0402146628300982,0.580749026025068,
-2.16459576002463));
#68166=CARTESIAN_POINT('Ctrl Pts',(-0.313428316539825,0.490560231497228,
-2.15068613007887));
#68167=CARTESIAN_POINT('Ctrl Pts',(-0.510080948985451,0.280542467048581,
-2.13677650013311));
#68168=CARTESIAN_POINT('Ctrl Pts',(-0.582136292925639,0.00199669587001278,
-2.12286687018735));
#68169=CARTESIAN_POINT('Ctrl Pts',(-0.511993415616024,-0.277036807484928,
-2.10895724024159));
#68170=CARTESIAN_POINT('Ctrl Pts',(-0.31678609227038,-0.488398630300768,
-2.09504761029584));
#68171=CARTESIAN_POINT('Ctrl Pts',(-0.0441975450001183,-0.580459496736478,
-2.08113798035008));
#68172=CARTESIAN_POINT('Ctrl Pts',(0.239187120565808,-0.530731732319673,
-2.06722835040432));
#68173=CARTESIAN_POINT('Ctrl Pts',(0.464145634895935,-0.351362320038238,
-2.05331872045856));
#68174=CARTESIAN_POINT('Ctrl Pts',(0.575727463241813,-0.0861657612091384,
-2.0394090905128));
#68175=CARTESIAN_POINT('Ctrl Pts',(0.546676552841566,0.200078476875617,
-2.02549946056704));
#68176=CARTESIAN_POINT('Ctrl Pts',(0.384089159047769,0.437449617941975,
-2.01158983062128));
#68177=CARTESIAN_POINT('Ctrl Pts',(0.127680445604864,0.567965099408182,
-1.99768020067552));
#68178=CARTESIAN_POINT('Ctrl Pts',(-0.159916724002057,0.559743951928069,
-1.98377057072976));
#68179=CARTESIAN_POINT('Ctrl Pts',(-0.408451093406464,0.414794352216454,
-1.969860940784));
#68180=CARTESIAN_POINT('Ctrl Pts',(-0.557213262287108,0.168523086450973,
-1.95595131083824));
#68181=CARTESIAN_POINT('Ctrl Pts',(-0.569865149577474,-0.118913252552635,
-1.94204168089249));
#68182=CARTESIAN_POINT('Ctrl Pts',(-0.443316283355426,-0.377302694461006,
-1.92813205094673));
#68183=CARTESIAN_POINT('Ctrl Pts',(-0.208478709299335,-0.543528543964792,
-1.91422242100097));
#68184=CARTESIAN_POINT('Ctrl Pts',(0.0772838835042257,-0.576986873062212,
-1.90031279105521));
#68185=CARTESIAN_POINT('Ctrl Pts',(0.34416837009945,-0.46950482783321,-1.88640316110945));
#68186=CARTESIAN_POINT('Ctrl Pts',(0.526982973690763,-0.247337008503869,
-1.87249353116369));
#68187=CARTESIAN_POINT('Ctrl Pts',(0.581071637328817,0.0352477322335796,
-1.85858390121793));
#68188=CARTESIAN_POINT('Ctrl Pts',(0.493222142753769,0.30922252219556,-1.84467427127217));
#68189=CARTESIAN_POINT('Ctrl Pts',(0.284893454160213,0.507663638753324,
-1.83076464132642));
#68190=CARTESIAN_POINT('Ctrl Pts',(0.00697394479219623,0.582097942299781,
-1.81685501138065));
#68191=CARTESIAN_POINT('Ctrl Pts',(-0.272649087542171,0.514343392489906,
-1.8029453814349));
#68192=CARTESIAN_POINT('Ctrl Pts',(-0.485672226097312,0.320950368644881,
-1.78903575148914));
#68193=CARTESIAN_POINT('Ctrl Pts',(-0.580060386038787,0.0491589145947808,
-1.77512612154338));
#68194=CARTESIAN_POINT('Ctrl Pts',(-0.532757405753194,-0.234640569703385,
-1.76121649159762));
#68195=CARTESIAN_POINT('Ctrl Pts',(-0.355317967087673,-0.461124487096798,
-1.74730686165186));
#68196=CARTESIAN_POINT('Ctrl Pts',(-0.0910851374036396,-0.574969693183704,
-1.7333972317061));
#68197=CARTESIAN_POINT('Ctrl Pts',(0.19539702577582,-0.548367260741893,
-1.71948760176034));
#68198=CARTESIAN_POINT('Ctrl Pts',(0.434149628300019,-0.387815356300597,
-1.70557797181458));
#68199=CARTESIAN_POINT('Ctrl Pts',(0.566852658497668,-0.132531935357976,
-1.69166834186883));
#68200=CARTESIAN_POINT('Ctrl Pts',(0.561090795286944,0.155125013392,-1.67775871192306));
#68201=CARTESIAN_POINT('Ctrl Pts',(0.418271486905671,0.404889631353191,
-1.66384908197731));
#68202=CARTESIAN_POINT('Ctrl Pts',(0.173281154040451,0.555752005835349,
-1.64993945203155));
#68203=CARTESIAN_POINT('Ctrl Pts',(-0.114036503508187,0.570861039310996,
-1.63602982208579));
#68204=CARTESIAN_POINT('Ctrl Pts',(-0.373498505682864,0.446526053650032,
-1.62212019214003));
#68205=CARTESIAN_POINT('Ctrl Pts',(-0.54172616326678,0.213118310728701,
-1.60821056219427));
#68206=CARTESIAN_POINT('Ctrl Pts',(-0.577626567324083,-0.0723477646994037,
-1.59430093224851));
#68207=CARTESIAN_POINT('Ctrl Pts',(-0.472430339169505,-0.340141477870296,
-1.58039130230275));
#68208=CARTESIAN_POINT('Ctrl Pts',(-0.251833723320963,-0.524848955542358,
-1.566481672357));
#68209=CARTESIAN_POINT('Ctrl Pts',(0.0302782248340165,-0.581351769100692,
-1.55257204241123));
#68210=CARTESIAN_POINT('Ctrl Pts',(0.30499412198458,-0.49584799675955,-1.53866241246548));
#68211=CARTESIAN_POINT('Ctrl Pts',(0.505209215517677,-0.289223613993771,
-1.52475278251972));
#68212=CARTESIAN_POINT('Ctrl Pts',(0.582017037113508,-0.0119506838806641,
-1.51084315257396));
#68213=CARTESIAN_POINT('Ctrl Pts',(0.516655768033535,0.268241435451875,
-1.4969335226282));
#68214=CARTESIAN_POINT('Ctrl Pts',(0.325091181782599,0.48291031658352,-1.48302389268244));
#68215=CARTESIAN_POINT('Ctrl Pts',(0.0541166904024802,0.579618869737247,
-1.46911426273668));
#68216=CARTESIAN_POINT('Ctrl Pts',(-0.23007686532507,0.534744131690842,
-1.45520463279092));
#68217=CARTESIAN_POINT('Ctrl Pts',(-0.458069628562033,0.359247638439899,
-1.44129500284516));
#68218=CARTESIAN_POINT('Ctrl Pts',(-0.574169889679393,0.0959978547737282,
-1.4273853728994));
#68219=CARTESIAN_POINT('Ctrl Pts',(-0.550017879980101,-0.190701290079009,
-1.41347574295365));
#68220=CARTESIAN_POINT('Ctrl Pts',(-0.391513202118355,-0.430817899932948,
-1.39956611300789));
#68221=CARTESIAN_POINT('Ctrl Pts',(-0.13737373629784,-0.565698777540818,
-1.38565648306213));
#68222=CARTESIAN_POINT('Ctrl Pts',(0.150321962290467,-0.562396619823365,
-1.37174685311637));
#68223=CARTESIAN_POINT('Ctrl Pts',(0.401298569641467,-0.42171804364921,
-1.35783722317061));
#68224=CARTESIAN_POINT('Ctrl Pts',(0.554250120856,-0.178026553824736,-1.34392759322485));
#68225=CARTESIAN_POINT('Ctrl Pts',(0.571815195963504,0.109151417768263,
-1.33001796327909));
#68226=CARTESIAN_POINT('Ctrl Pts',(0.449703180434771,0.369667012110162,
-1.31610833333333));
#68227=CARTESIAN_POINT('Ctrl Pts',(0.217742332037662,0.539884179407402,
-1.30219870338757));
#68228=CARTESIAN_POINT('Ctrl Pts',(-0.0674063568751685,0.578224033907638,
-1.28828907344181));
#68229=CARTESIAN_POINT('Ctrl Pts',(-0.336089719428759,0.475321313250208,
-1.27437944349606));
#68230=CARTESIAN_POINT('Ctrl Pts',(-0.522676568049277,0.256312027708089,
-1.2604698135503));
#68231=CARTESIAN_POINT('Ctrl Pts',(-0.581589400861518,-0.0253065039297315,
-1.24656018360454));
#68232=CARTESIAN_POINT('Ctrl Pts',(-0.498437601550204,-0.30074342502619,
-1.23265055365878));
#68233=CARTESIAN_POINT('Ctrl Pts',(-0.293532629990769,-0.502717858710337,
-1.21874092371302));
#68234=CARTESIAN_POINT('Ctrl Pts',(-0.0169265493084289,-0.581893583281438,
-1.20483129376726));
#68235=CARTESIAN_POINT('Ctrl Pts',(0.263814173437639,-0.518930373199543,
-1.1909216638215));
#68236=CARTESIAN_POINT('Ctrl Pts',(0.480113103670162,-0.329208228967331,
-1.17701203387574));
#68237=CARTESIAN_POINT('Ctrl Pts',(0.579134980109133,-0.0590705099825352,
-1.16310240392998));
#68238=CARTESIAN_POINT('Ctrl Pts',(0.536691764892018,0.225496341062766,
-1.14919277398422));
#68239=CARTESIAN_POINT('Ctrl Pts',(0.363151046814323,0.454981282618599,
-1.13528314403847));
#68240=CARTESIAN_POINT('Ctrl Pts',(0.100903554172759,0.573328111198909,
-1.1213735140927));
#68241=CARTESIAN_POINT('Ctrl Pts',(-0.185991613069268,0.551628289886855,
-1.10746388414695));
#68242=CARTESIAN_POINT('Ctrl Pts',(-0.427454676408419,0.395182426168191,
-1.09355425420119));
#68243=CARTESIAN_POINT('Ctrl Pts',(-0.564503540892674,0.142205494462193,
-1.07964462425543));
#68244=CARTESIAN_POINT('Ctrl Pts',(-0.56366133007438,-0.145507921826901,
-1.06573499430967));
#68245=CARTESIAN_POINT('Ctrl Pts',(-0.425133770484826,-0.397678170797639,
-1.05182536436391));
#68246=CARTESIAN_POINT('Ctrl Pts',(-0.182758938889015,-0.552707717145115,
-1.03791573441815));
#68247=CARTESIAN_POINT('Ctrl Pts',(0.104258352459501,-0.5727275497809,-1.02400610447239));
#68248=CARTESIAN_POINT('Ctrl Pts',(0.365808493846163,-0.452847431444196,
-1.01009647452664));
#68249=CARTESIAN_POINT('Ctrl Pts',(0.538002727045805,-0.222350435184824,
-0.996186844580877));
#68250=CARTESIAN_POINT('Ctrl Pts',(0.578779229134785,0.0624600212755955,
-0.982277214635117));
#68251=CARTESIAN_POINT('Ctrl Pts',(0.478177538729221,0.332013390980647,
-0.968367584689359));
#68252=CARTESIAN_POINT('Ctrl Pts',(0.260771594276588,0.520465970024985,
-0.954457954743599));
#68253=CARTESIAN_POINT('Ctrl Pts',(-0.0203329329808465,0.581784515239103,
-0.940548324797841));
#68254=CARTESIAN_POINT('Ctrl Pts',(-0.296470742069694,0.500990767811392,
-0.926638694852082));
#68255=CARTESIAN_POINT('Ctrl Pts',(-0.500189750463181,0.297820187138455,
-0.912729064906322));
#68256=CARTESIAN_POINT('Ctrl Pts',(-0.581727589828724,0.0219011773123757,
-0.898819434960564));
#68257=CARTESIAN_POINT('Ctrl Pts',(-0.521167041701788,-0.25936762515667,
-0.884909805014805));
#68258=CARTESIAN_POINT('Ctrl Pts',(-0.333301209220274,-0.477280791848893,
-0.871000175069045));
#68259=CARTESIAN_POINT('Ctrl Pts',(-0.0640200111834863,-0.578608752529436,
-0.857090545123287));
#68260=CARTESIAN_POINT('Ctrl Pts',(0.220899331777977,-0.538600162974025,
-0.843180915177526));
#68261=CARTESIAN_POINT('Ctrl Pts',(0.451859675041561,-0.367027906850336,
-0.82927128523177));
#68262=CARTESIAN_POINT('Ctrl Pts',(0.572444419280888,-0.105801876967134,
-0.815361655286009));
#68263=CARTESIAN_POINT('Ctrl Pts',(0.553198372732334,0.181268339049875,
-0.801452025340251));
#68264=CARTESIAN_POINT('Ctrl Pts',(0.398822760209661,0.424060203596552,
-0.787542395394492));
#68265=CARTESIAN_POINT('Ctrl Pts',(0.147026856622959,0.563267035931604,
-0.773632765448732));
#68266=CARTESIAN_POINT('Ctrl Pts',(-0.140683243934122,0.564884833582719,
-0.759723135502974));
#68267=CARTESIAN_POINT('Ctrl Pts',(-0.394028699492784,0.428518417704104,
-0.745813505557215));
#68268=CARTESIAN_POINT('Ctrl Pts',(-0.551124907460887,0.187477963269903,
-0.731903875611457));
#68269=CARTESIAN_POINT('Ctrl Pts',(-0.573598034065102,-0.0993576652918848,
-0.717994245665696));
#68270=CARTESIAN_POINT('Ctrl Pts',(-0.45595857681627,-0.361923232969764,
-0.704084615719939));
#68271=CARTESIAN_POINT('Ctrl Pts',(-0.226942283292515,-0.536081943726502,
-0.690174985774178));
#68272=CARTESIAN_POINT('Ctrl Pts',(0.0575091195050125,-0.579292112417698,
-0.67626535582842));
#68273=CARTESIAN_POINT('Ctrl Pts',(0.327912790527978,-0.480998806800763,
-0.66235572588266));
#68274=CARTESIAN_POINT('Ctrl Pts',(0.518217323076349,-0.265212097007629,
-0.648446095936903));
#68275=CARTESIAN_POINT('Ctrl Pts',(0.581937097969522,0.0153578755827512,
-0.634536465991143));
#68276=CARTESIAN_POINT('Ctrl Pts',(0.503507308892608,0.292176385471736,
-0.620626836045384));
#68277=CARTESIAN_POINT('Ctrl Pts',(0.302085971992796,0.497625075594841,
-0.606717206099625));
#68278=CARTESIAN_POINT('Ctrl Pts',(0.026874204219816,0.581519068890397,
-0.592807576153866));
#68279=CARTESIAN_POINT('Ctrl Pts',(-0.254902115676097,0.523365610027496,
-0.578897946208108));
#68280=CARTESIAN_POINT('Ctrl Pts',(-0.474413588177279,0.33736982332207,
-0.564988316262347));
#68281=CARTESIAN_POINT('Ctrl Pts',(-0.578040225468284,0.0689648321695848,
-0.551078686316589));
#68282=CARTESIAN_POINT('Ctrl Pts',(-0.540469186422474,-0.216286173537356,
-0.537169056370829));
#68283=CARTESIAN_POINT('Ctrl Pts',(-0.370877935128156,-0.448705034037593,
-0.523259426425072));
#68284=CARTESIAN_POINT('Ctrl Pts',(-0.110692465062534,-0.571518878528068,
-0.509349796479312));
#68285=CARTESIAN_POINT('Ctrl Pts',(0.176531813318142,-0.554728013734852,
-0.495440166533554));
#68286=CARTESIAN_POINT('Ctrl Pts',(0.420634729651996,-0.402433938114313,
-0.481530536587794));
#68287=CARTESIAN_POINT('Ctrl Pts',(0.561989353052933,-0.151837470312021,
-0.467620906642035));
#68288=CARTESIAN_POINT('Ctrl Pts',(0.566067040903533,0.135848281322644,
-0.453711276696276));
#68289=CARTESIAN_POINT('Ctrl Pts',(0.431871737870722,0.390350422523305,
-0.439801646750518));
#68290=CARTESIAN_POINT('Ctrl Pts',(0.192183281980758,0.549501807515437,
-0.425892016804758));
#68291=CARTESIAN_POINT('Ctrl Pts',(-0.0944497145325559,0.574426585178866,
-0.411982386859));
#68292=CARTESIAN_POINT('Ctrl Pts',(-0.358011513514948,0.459036389109272,
-0.398072756913241));
#68293=CARTESIAN_POINT('Ctrl Pts',(-0.534121969869188,0.231517540671202,
-0.384163126967482));
#68294=CARTESIAN_POINT('Ctrl Pts',(-0.579762646262023,-0.0525540135011436,
-0.370253497021723));
#68295=CARTESIAN_POINT('Ctrl Pts',(-0.48378491121418,-0.323788217847987,
-0.356343867075963));
#68296=CARTESIAN_POINT('Ctrl Pts',(-0.269633211276888,-0.515930791590299,
-0.342434237130205));
#68297=CARTESIAN_POINT('Ctrl Pts',(0.0103816954412071,-0.582047137901145,
-0.328524607184445));
#68298=CARTESIAN_POINT('Ctrl Pts',(0.287860669170086,-0.505987040814971,
-0.314614977238687));
#68299=CARTESIAN_POINT('Ctrl Pts',(0.495024021603582,-0.306329672713003,
-0.300705347292928));
#68300=CARTESIAN_POINT('Ctrl Pts',(0.581268035697884,-0.031845266452672,
-0.28679571734717));
#68301=CARTESIAN_POINT('Ctrl Pts',(0.525525917473871,0.250417971405241,
-0.272886087401411));
#68302=CARTESIAN_POINT('Ctrl Pts',(0.34141377378654,0.471511702349578,-0.258976457455652));
#68303=CARTESIAN_POINT('Ctrl Pts',(0.0739046115413053,0.577429440320225,
-0.245066827509892));
#68304=CARTESIAN_POINT('Ctrl Pts',(-0.211657203771934,0.542298698929604,
-0.231157197564133));
#68305=CARTESIAN_POINT('Ctrl Pts',(-0.445517589869098,0.37470084954831,
-0.217247567618374));
#68306=CARTESIAN_POINT('Ctrl Pts',(-0.570551557304549,0.115574962183174,
-0.203337937672615));
#68307=CARTESIAN_POINT('Ctrl Pts',(-0.556217099697408,-0.171782384589059,
-0.189428307726856));
#68308=CARTESIAN_POINT('Ctrl Pts',(-0.406015698566048,-0.417178500209998,
-0.175518677781097));
#68309=CARTESIAN_POINT('Ctrl Pts',(-0.156636978608061,-0.560670595014718,
-0.161609047835338));
#68310=CARTESIAN_POINT('Ctrl Pts',(0.131003377216481,-0.56720784733414,
-0.14769941788958));
#68311=CARTESIAN_POINT('Ctrl Pts',(0.386643628799531,-0.435193521555786,
-0.133789787943821));
#68312=CARTESIAN_POINT('Ctrl Pts',(0.547838496865826,-0.196874481237042,
-0.119880157998062));
#68313=CARTESIAN_POINT('Ctrl Pts',(0.575213218962054,0.0895347225743331,
-0.105970528052302));
#68314=CARTESIAN_POINT('Ctrl Pts',(0.462080493992123,0.354073888018237,
-0.0920608981065435));
#68315=CARTESIAN_POINT('Ctrl Pts',(0.236076164663117,0.532122427819931,
-0.0781512681607847));
#68316=CARTESIAN_POINT('Ctrl Pts',(-0.047595635797325,0.580191814324249,
-0.0642416382150254));
#68317=CARTESIAN_POINT('Ctrl Pts',(-0.319638859935216,0.486533658576269,
-0.0503320082692662));
#68318=CARTESIAN_POINT('Ctrl Pts',(-0.513608721405772,0.274038504320584,
-0.0364223783235072));
#68319=CARTESIAN_POINT('Ctrl Pts',(-0.582110362739213,-0.00541238131170235,
-0.0225127483777487));
#68320=CARTESIAN_POINT('Ctrl Pts',(-0.508438185945303,-0.283508771827898,
-0.00860311843199003));
#68321=CARTESIAN_POINT('Ctrl Pts',(-0.310533807033502,-0.492418870624804,
0.00530651151376876));
#68322=CARTESIAN_POINT('Ctrl Pts',(-0.128081630931447,-0.551395568835168,
0.0145795981442749));
#68323=CARTESIAN_POINT('Ctrl Pts',(-0.0353121949621431,-0.557273992116744,
0.0192161414595281));
#68324=CARTESIAN_POINT('Ctrl Pts',(0.305041111877683,-0.427420965560345,
-3.96754114145953));
#68325=CARTESIAN_POINT('Ctrl Pts',(0.376193906476754,-0.376640752780538,
-3.96290459814427));
#68326=CARTESIAN_POINT('Ctrl Pts',(0.49257674617948,-0.238910373259439,
-3.95363151151377));
#68327=CARTESIAN_POINT('Ctrl Pts',(0.546812900484255,0.0262129455514636,
-3.93972188156801));
#68328=CARTESIAN_POINT('Ctrl Pts',(0.467483302272917,0.28486232584599,-3.92581225162225));
#68329=CARTESIAN_POINT('Ctrl Pts',(0.27396005171883,0.473963347551388,-3.91190262167649));
#68330=CARTESIAN_POINT('Ctrl Pts',(0.0135174993871538,0.547271810816138,
-3.89799299173073));
#68331=CARTESIAN_POINT('Ctrl Pts',(-0.250227384164322,0.486907433624593,
-3.88408336178497));
#68332=CARTESIAN_POINT('Ctrl Pts',(-0.452849102465794,0.307601726185072,
-3.87017373183922));
#68333=CARTESIAN_POINT('Ctrl Pts',(-0.54485364354006,0.0531606246437338,
-3.85626410189345));
#68334=CARTESIAN_POINT('Ctrl Pts',(-0.503766926905405,-0.214267215150516,
-3.84235447194771));
#68335=CARTESIAN_POINT('Ctrl Pts',(-0.339625274156856,-0.429355459912895,
-3.82844484200193));
#68336=CARTESIAN_POINT('Ctrl Pts',(-0.0925234642162299,-0.539565519412296,
-3.81453521205618));
#68337=CARTESIAN_POINT('Ctrl Pts',(0.177179011324535,-0.517975942716222,
-3.80062558211042));
#68338=CARTESIAN_POINT('Ctrl Pts',(0.403602037815667,-0.369860653339095,
-3.78671595216466));
#68339=CARTESIAN_POINT('Ctrl Pts',(0.531437338879899,-0.131399593731153,
-3.7728063222189));
#68340=CARTESIAN_POINT('Ctrl Pts',(0.529458634820968,0.139158375250956,
-3.75889669227314));
#68341=CARTESIAN_POINT('Ctrl Pts',(0.398149261450136,0.375724189487086,
-3.74498706232739));
#68342=CARTESIAN_POINT('Ctrl Pts',(0.169584112575006,0.520511986460079,
-3.73107743238162));
#68343=CARTESIAN_POINT('Ctrl Pts',(-0.100405286138957,0.538154512099795,
-3.71716780243587));
#68344=CARTESIAN_POINT('Ctrl Pts',(-0.345868721935883,0.424342228657172,
-3.7032581724901));
#68345=CARTESIAN_POINT('Ctrl Pts',(-0.506846930437278,0.206876023606841,
-3.68934854254435));
#68346=CARTESIAN_POINT('Ctrl Pts',(-0.544017822953714,-0.0611237131283834,
-3.67543891259859));
#68347=CARTESIAN_POINT('Ctrl Pts',(-0.448301679071712,-0.314192782415098,
-3.66152928265283));
#68348=CARTESIAN_POINT('Ctrl Pts',(-0.243079046546545,-0.490514094737742,
-3.64761965270707));
#68349=CARTESIAN_POINT('Ctrl Pts',(0.0215204165605152,-0.547017706896761,
-3.63371002276131));
#68350=CARTESIAN_POINT('Ctrl Pts',(0.280863095316674,-0.469901502111615,
-3.61980039281555));
#68351=CARTESIAN_POINT('Ctrl Pts',(0.47159944759146,-0.278002627730234,
-3.6058907628698));
#68352=CARTESIAN_POINT('Ctrl Pts',(0.547138373757176,-0.0181961522555487,
-3.59198113292403));
#68353=CARTESIAN_POINT('Ctrl Pts',(0.489028007701532,0.246055090738122,
-3.57807150297828));
#68354=CARTESIAN_POINT('Ctrl Pts',(0.311462947476309,0.45020254590979,-3.56416187303252));
#68355=CARTESIAN_POINT('Ctrl Pts',(0.0578169459756449,0.544379188390458,
-3.55025224308676));
#68356=CARTESIAN_POINT('Ctrl Pts',(-0.209951979959951,0.505580523858779,
-3.536342613141));
#68357=CARTESIAN_POINT('Ctrl Pts',(-0.426436011857877,0.343283888036202,
-3.52243298319524));
#68358=CARTESIAN_POINT('Ctrl Pts',(-0.538754673721399,0.0971334213225582,
-3.50852335324948));
#68359=CARTESIAN_POINT('Ctrl Pts',(-0.519471926732396,-0.172743791006827,
-3.49461372330373));
#68360=CARTESIAN_POINT('Ctrl Pts',(-0.373297960507913,-0.400424940126257,
-3.48070409335796));
#68361=CARTESIAN_POINT('Ctrl Pts',(-0.135938636789861,-0.5302944342742,
-3.46679446341221));
#68362=CARTESIAN_POINT('Ctrl Pts',(0.134626368459391,-0.53062909919257,
-3.45288483346644));
#68363=CARTESIAN_POINT('Ctrl Pts',(0.372306239486833,-0.401347186403061,
-3.43897520352069));
#68364=CARTESIAN_POINT('Ctrl Pts',(0.519043000355028,-0.174028341878362,
-3.42506557357493));
#68365=CARTESIAN_POINT('Ctrl Pts',(0.538993315678459,0.0958003426320719,
-3.41115594362917));
#68366=CARTESIAN_POINT('Ctrl Pts',(0.427283929165017,0.342227912175184,
-3.39724631368341));
#68367=CARTESIAN_POINT('Ctrl Pts',(0.211202052163931,0.505059593668139,
-3.38333668373765));
#68368=CARTESIAN_POINT('Ctrl Pts',(-0.0564700735589543,0.544520551298779,
-3.36942705379189));
#68369=CARTESIAN_POINT('Ctrl Pts',(-0.310348274883871,0.450971671251184,
-3.35551742384613));
#68370=CARTESIAN_POINT('Ctrl Pts',(-0.48841781560348,0.247264104543312,
-3.34160779390037));
#68371=CARTESIAN_POINT('Ctrl Pts',(-0.547181713556024,-0.0168425753486551,
-3.32769816395462));
#68372=CARTESIAN_POINT('Ctrl Pts',(-0.472285732690417,-0.276835125465604,
-3.31378853400885));
#68373=CARTESIAN_POINT('Ctrl Pts',(-0.282024687103075,-0.469205259837199,
-3.2998789040631));
#68374=CARTESIAN_POINT('Ctrl Pts',(-0.0228735734304004,-0.546962795474249,
-3.28596927411734));
#68375=CARTESIAN_POINT('Ctrl Pts',(0.241864859732498,-0.491113927333628,
-3.27205964417158));
#68376=CARTESIAN_POINT('Ctrl Pts',(0.447523051284027,-0.315300838190951,
-3.25815001422582));
#68377=CARTESIAN_POINT('Ctrl Pts',(0.543864949324536,-0.0624693275992378,
-3.24424038428006));
#68378=CARTESIAN_POINT('Ctrl Pts',(0.507357153343402,0.205621543000143,
-3.2303307543343));
#68379=CARTESIAN_POINT('Ctrl Pts',(0.346917409430942,0.423485313828243,
-3.21642112438854));
#68380=CARTESIAN_POINT('Ctrl Pts',(0.10173627567359,0.537904480560023,-3.20251149444279));
#68381=CARTESIAN_POINT('Ctrl Pts',(-0.168295941263372,0.52092991481461,
-3.18860186449702));
#68382=CARTESIAN_POINT('Ctrl Pts',(-0.397218569634841,0.376707987613393,
-3.17469223455126));
#68383=CARTESIAN_POINT('Ctrl Pts',(-0.529112761992475,0.140467736833678,
-3.16078260460551));
#68384=CARTESIAN_POINT('Ctrl Pts',(-0.531760771780433,-0.130084517103148,
-3.14687297465975));
#68385=CARTESIAN_POINT('Ctrl Pts',(-0.404515770607708,-0.368861073202545,
-3.13296334471399));
#68386=CARTESIAN_POINT('Ctrl Pts',(-0.178459848784724,-0.517536068662093,
-3.11905371476823));
#68387=CARTESIAN_POINT('Ctrl Pts',(0.0911883956095983,-0.539792716235249,
-3.10514408482247));
#68388=CARTESIAN_POINT('Ctrl Pts',(0.338562083663956,-0.430194392687307,
-3.09123445487671));
#68389=CARTESIAN_POINT('Ctrl Pts',(0.50323533426974,-0.215512640782169,
-3.07732482493095));
#68390=CARTESIAN_POINT('Ctrl Pts',(0.544983472195168,0.051812305763967,
-3.0634151949852));
#68391=CARTESIAN_POINT('Ctrl Pts',(0.453608694922806,0.306481079162989,
-3.04950556503943));
#68392=CARTESIAN_POINT('Ctrl Pts',(0.251431086173814,0.486285830453589,
-3.03559593509368));
#68393=CARTESIAN_POINT('Ctrl Pts',(-0.0121635028516318,0.547305718216847,
-3.02168630514792));
#68394=CARTESIAN_POINT('Ctrl Pts',(-0.272786917444753,0.47463543658841,
-3.00777667520216));
#68395=CARTESIAN_POINT('Ctrl Pts',(-0.46677677059831,0.286026128918834,
-2.9938670452564));
#68396=CARTESIAN_POINT('Ctrl Pts',(-0.546747231203381,0.0275493224221043,
-2.97995741531064));
#68397=CARTESIAN_POINT('Ctrl Pts',(-0.493163943837085,-0.237656947076102,
-2.96604778536488));
#68398=CARTESIAN_POINT('Ctrl Pts',(-0.319115678680562,-0.444810840262156,
-2.95213815541912));
#68399=CARTESIAN_POINT('Ctrl Pts',(-0.0671171423714758,-0.543310950740336,
-2.93822852547336));
#68400=CARTESIAN_POINT('Ctrl Pts',(0.201276073974873,-0.509096692230211,
-2.9243188955276));
#68401=CARTESIAN_POINT('Ctrl Pts',(0.420503656693519,-0.350525569255455,
-2.91040926558185));
#68402=CARTESIAN_POINT('Ctrl Pts',(0.537014963623297,-0.106331692543425,
-2.89649963563608));
#68403=CARTESIAN_POINT('Ctrl Pts',(0.522349820055569,0.163835788161179,
-2.88259000569033));
#68404=CARTESIAN_POINT('Ctrl Pts',(0.380090475293543,0.393983160281768,
-2.86868037574457));
#68405=CARTESIAN_POINT('Ctrl Pts',(0.144986567913532,0.527892408658371,
-2.85477074579881));
#68406=CARTESIAN_POINT('Ctrl Pts',(-0.125533155853402,0.532853569731841,
-2.84086111585305));
#68407=CARTESIAN_POINT('Ctrl Pts',(-0.36538894114552,0.407654782485176,
-2.82695148590729));
#68408=CARTESIAN_POINT('Ctrl Pts',(-0.515991302236719,0.182878309294829,
-2.81304185596153));
#68409=CARTESIAN_POINT('Ctrl Pts',(-0.540552654976281,-0.0865697822139766,
-2.79913222601577));
#68410=CARTESIAN_POINT('Ctrl Pts',(-0.433073406633946,-0.334871504402733,
-2.78522259607001));
#68411=CARTESIAN_POINT('Ctrl Pts',(-0.219807474241307,-0.501374285601225,
-2.77131296612426));
#68412=CARTESIAN_POINT('Ctrl Pts',(0.0471507502045272,-0.545406551802993,
-2.7574033361785));
#68413=CARTESIAN_POINT('Ctrl Pts',(0.302591477989944,-0.456212557304533,
-2.74349370623274));
#68414=CARTESIAN_POINT('Ctrl Pts',(0.484118295135511,-0.255579686809354,
-2.72958407628698));
#68415=CARTESIAN_POINT('Ctrl Pts',(0.547389711820154,0.00748354113566584,
-2.71567444634122));
#68416=CARTESIAN_POINT('Ctrl Pts',(0.476950442026069,0.268718767200243,
-2.70176481639546));
#68417=CARTESIAN_POINT('Ctrl Pts',(0.290006660651773,0.464314157410786,
-2.6878551864497));
#68418=CARTESIAN_POINT('Ctrl Pts',(0.032223057406854,0.546491696703467,
-2.67394555650394));
#68419=CARTESIAN_POINT('Ctrl Pts',(-0.233431660390051,0.495177907344447,
-2.66003592655819));
#68420=CARTESIAN_POINT('Ctrl Pts',(-0.442066111121947,0.32290719005931,
-2.64612629661242));
#68421=CARTESIAN_POINT('Ctrl Pts',(-0.542717233138088,0.071760050511542,
-2.63221666666667));
#68422=CARTESIAN_POINT('Ctrl Pts',(-0.510799013349406,-0.196915890561819,
-2.61830703672091));
#68423=CARTESIAN_POINT('Ctrl Pts',(-0.354108103733396,-0.417491258429227,
-2.60439740677515));
#68424=CARTESIAN_POINT('Ctrl Pts',(-0.110919335981845,-0.536086187939802,
-2.59048777682939));
#68425=CARTESIAN_POINT('Ctrl Pts',(0.159363657761974,-0.523731538652395,
-2.57657814688363));
#68426=CARTESIAN_POINT('Ctrl Pts',(0.390718948593253,-0.383445176269912,
-2.56266851693787));
#68427=CARTESIAN_POINT('Ctrl Pts',(0.526633463486426,-0.14949479967802,
-2.54875888699211));
#68428=CARTESIAN_POINT('Ctrl Pts',(0.533907413157257,0.120972617439681,
-2.53484925704635));
#68429=CARTESIAN_POINT('Ctrl Pts',(0.41076399255644,0.361890097147703,-2.52093962710059));
#68430=CARTESIAN_POINT('Ctrl Pts',(0.187283400394916,0.514408814009829,
-2.50702999715484));
#68431=CARTESIAN_POINT('Ctrl Pts',(-0.0819448400912485,0.541273076345849,
-2.49312036720907));
#68432=CARTESIAN_POINT('Ctrl Pts',(-0.33115644419315,0.435920760533185,
-2.47921073726332));
#68433=CARTESIAN_POINT('Ctrl Pts',(-0.499476583715483,0.224086238565404,
-2.46530110731756));
#68434=CARTESIAN_POINT('Ctrl Pts',(-0.545789759192809,-0.0424857476659746,
-2.4513914773718));
#68435=CARTESIAN_POINT('Ctrl Pts',(-0.458783068039706,-0.298679755715977,
-2.43748184742604));
#68436=CARTESIAN_POINT('Ctrl Pts',(-0.259709603164407,-0.481915368107998,
-2.42357221748028));
#68437=CARTESIAN_POINT('Ctrl Pts',(0.00280303233169327,-0.54743368822555,
-2.40966258753452));
#68438=CARTESIAN_POINT('Ctrl Pts',(0.264630972136224,-0.479230579763768,
-2.39575295758876));
#68439=CARTESIAN_POINT('Ctrl Pts',(0.461817600305192,-0.293965991303136,
-2.381843327643));
#68440=CARTESIAN_POINT('Ctrl Pts',(0.546196210655486,-0.0368944367089179,
-2.36793369769724));
#68441=CARTESIAN_POINT('Ctrl Pts',(0.497155670623904,0.229189308566033,
-2.35402406775149));
#68442=CARTESIAN_POINT('Ctrl Pts',(0.326675095146872,0.439289064518186,
-2.34011443780572));
#68443=CARTESIAN_POINT('Ctrl Pts',(0.0763977125973221,0.542083839921813,
-2.32620480785997));
#68444=CARTESIAN_POINT('Ctrl Pts',(-0.192541311514372,0.51246399225195,
-2.31229517791421));
#68445=CARTESIAN_POINT('Ctrl Pts',(-0.414448339258253,0.357664750961786,
-2.29838554796845));
#68446=CARTESIAN_POINT('Ctrl Pts',(-0.535118221408144,0.115498870606881,
-2.28447591802269));
#68447=CARTESIAN_POINT('Ctrl Pts',(-0.52507496959386,-0.154879877003077,
-2.27056628807693));
#68448=CARTESIAN_POINT('Ctrl Pts',(-0.386771845295417,-0.387426173201114,
-2.25665665813117));
#68449=CARTESIAN_POINT('Ctrl Pts',(-0.153992102550614,-0.525336018512459,
-2.24274702818542));
#68450=CARTESIAN_POINT('Ctrl Pts',(0.116403235262424,-0.534922225014928,
-2.22883739823965));
#68451=CARTESIAN_POINT('Ctrl Pts',(0.358364796993828,-0.413843173521145,
-2.2149277682939));
#68452=CARTESIAN_POINT('Ctrl Pts',(0.512788719670011,-0.191674800048603,
-2.20101813834814));
#68453=CARTESIAN_POINT('Ctrl Pts',(0.541953927677195,0.0773139073501151,
-2.18710850840238));
#68454=CARTESIAN_POINT('Ctrl Pts',(0.43873624622779,0.327417174626545,-2.17319887845662));
#68455=CARTESIAN_POINT('Ctrl Pts',(0.228348620953256,0.49754236734496,-2.15928924851086));
#68456=CARTESIAN_POINT('Ctrl Pts',(-0.0378176391856524,0.546133066350047,
-2.1453796185651));
#68457=CARTESIAN_POINT('Ctrl Pts',(-0.294746198309491,0.461320039209855,
-2.13146998861934));
#68458=CARTESIAN_POINT('Ctrl Pts',(-0.479677210417124,0.263820533319387,
-2.11756035867358));
#68459=CARTESIAN_POINT('Ctrl Pts',(-0.547437644218116,0.00187768138936353,
-2.10365072872783));
#68460=CARTESIAN_POINT('Ctrl Pts',(-0.481475683110906,-0.260523831092987,
-2.08974109878207));
#68461=CARTESIAN_POINT('Ctrl Pts',(-0.297903831424081,-0.459287281793578,
-2.07583146883631));
#68462=CARTESIAN_POINT('Ctrl Pts',(-0.0415631188247858,-0.545860794661091,
-2.06192183889055));
#68463=CARTESIAN_POINT('Ctrl Pts',(0.2249302017433,-0.499097089090089,-2.04801220894479));
#68464=CARTESIAN_POINT('Ctrl Pts',(0.436479903468258,-0.330419118488657,
-2.03410257899903));
#68465=CARTESIAN_POINT('Ctrl Pts',(0.541410817396038,-0.0810297895902128,
-2.02019294905327));
#68466=CARTESIAN_POINT('Ctrl Pts',(0.514091507218732,0.188152656638311,
-2.00628331910751));
#68467=CARTESIAN_POINT('Ctrl Pts',(0.361195250930158,0.41137512163472,-1.99237368916175));
#68468=CARTESIAN_POINT('Ctrl Pts',(0.120069961629371,0.534111134792003,
-1.97846405921599));
#68469=CARTESIAN_POINT('Ctrl Pts',(-0.150384773673522,0.526380014667772,
-1.96455442927023));
#68470=CARTESIAN_POINT('Ctrl Pts',(-0.38410507482534,0.390070239172256,
-1.95064479932448));
#68471=CARTESIAN_POINT('Ctrl Pts',(-0.524000168586827,0.158478147753744,
-1.93673516937872));
#68472=CARTESIAN_POINT('Ctrl Pts',(-0.535897931116531,-0.111825343368592,
-1.92282553943296));
#68473=CARTESIAN_POINT('Ctrl Pts',(-0.416892100274231,-0.354813298402725,
-1.9089159094872));
#68474=CARTESIAN_POINT('Ctrl Pts',(-0.196052187220425,-0.511131137655072,
-1.89500627954144));
#68475=CARTESIAN_POINT('Ctrl Pts',(0.0726773225372251,-0.54259515919634,
-1.88109664959568));
#68476=CARTESIAN_POINT('Ctrl Pts',(0.323653969064078,-0.44151965789028,
-1.86718701964992));
#68477=CARTESIAN_POINT('Ctrl Pts',(0.495571777891505,-0.232594309801278,
-1.85327738970416));
#68478=CARTESIAN_POINT('Ctrl Pts',(0.546436448177067,0.0331467660279462,
-1.8393677597584));
#68479=CARTESIAN_POINT('Ctrl Pts',(0.463823285348445,0.290791093335156,
-1.82545812981264));
#68480=CARTESIAN_POINT('Ctrl Pts',(0.267912176742691,0.477403985684529,
-1.81154849986689));
#68481=CARTESIAN_POINT('Ctrl Pts',(0.00655825784157817,0.54740157950865,
-1.79763886992113));
#68482=CARTESIAN_POINT('Ctrl Pts',(-0.256397644325143,0.483685587938072,
-1.78372923997537));
#68483=CARTESIAN_POINT('Ctrl Pts',(-0.456723386856148,0.301819893136834,
-1.76981961002961));
#68484=CARTESIAN_POINT('Ctrl Pts',(-0.545485473241036,0.0462287624481154,
-1.75590998008385));
#68485=CARTESIAN_POINT('Ctrl Pts',(-0.501002020814631,-0.220654651285976,
-1.74200035013809));
#68486=CARTESIAN_POINT('Ctrl Pts',(-0.334138986375984,-0.433638833337272,
-1.72809072019233));
#68487=CARTESIAN_POINT('Ctrl Pts',(-0.085655942859932,-0.540698214762409,
-1.71418109024657));
#68488=CARTESIAN_POINT('Ctrl Pts',(0.183750246768424,-0.515681439269462,
-1.70027146030081));
#68489=CARTESIAN_POINT('Ctrl Pts',(0.408271830227724,-0.364699345539563,
-1.68636183035505));
#68490=CARTESIAN_POINT('Ctrl Pts',(0.533065001714948,-0.124632274877432,
-1.6724522004093));
#68491=CARTESIAN_POINT('Ctrl Pts',(0.527646578468163,0.145878676390081,
-1.65854257046354));
#68492=CARTESIAN_POINT('Ctrl Pts',(0.393340116769695,0.380755896256491,
-1.64463294051778));
#68493=CARTESIAN_POINT('Ctrl Pts',(0.16295260733283,0.522626011367511,-1.63072331057202));
#68494=CARTESIAN_POINT('Ctrl Pts',(-0.107239276427261,0.53683446013258,
-1.61681368062626));
#68495=CARTESIAN_POINT('Ctrl Pts',(-0.351235861008467,0.419910549922387,
-1.6029040506805));
#68496=CARTESIAN_POINT('Ctrl Pts',(-0.509436189143367,0.200415241899318,
-1.58899442073474));
#68497=CARTESIAN_POINT('Ctrl Pts',(-0.543196724025735,-0.0680354246124073,
-1.57508479078898));
#68498=CARTESIAN_POINT('Ctrl Pts',(-0.444270792037967,-0.319867102616756,
-1.56117516084323));
#68499=CARTESIAN_POINT('Ctrl Pts',(-0.236822994726279,-0.49356495941604,
-1.54726553089746));
#68500=CARTESIAN_POINT('Ctrl Pts',(0.0284734696593775,-0.546699882494992,
-1.53335590095171));
#68501=CARTESIAN_POINT('Ctrl Pts',(0.286814729932908,-0.466292623454408,
-1.51944627100595));
#68502=CARTESIAN_POINT('Ctrl Pts',(0.475095860095443,-0.271984234312676,
-1.50553664106019));
#68503=CARTESIAN_POINT('Ctrl Pts',(0.547325496733678,-0.0112383548490794,
-1.49162701111443));
#68504=CARTESIAN_POINT('Ctrl Pts',(0.485860132689079,0.252252713479623,
-1.47771738116867));
#68505=CARTESIAN_POINT('Ctrl Pts',(0.305713890155758,0.454126102927714,
-1.46380775122291));
#68506=CARTESIAN_POINT('Ctrl Pts',(0.0508910264947163,0.545070273833379,
-1.44989812127715));
#68507=CARTESIAN_POINT('Ctrl Pts',(-0.216362969760304,0.502870326536555,
-1.43598849133139));
#68508=CARTESIAN_POINT('Ctrl Pts',(-0.430766061823084,0.337834426866049,
-1.42207886138564));
#68509=CARTESIAN_POINT('Ctrl Pts',(-0.539946084116101,0.0902758342092153,
-1.40816923143988));
#68510=CARTESIAN_POINT('Ctrl Pts',(-0.517233672171357,-0.179334403745111,
-1.39425960149412));
#68511=CARTESIAN_POINT('Ctrl Pts',(-0.368176778621395,-0.405138691904949,
-1.38034997154836));
#68512=CARTESIAN_POINT('Ctrl Pts',(-0.129185476820866,-0.531979898655059,
-1.3664403416026));
#68513=CARTESIAN_POINT('Ctrl Pts',(0.141361914573243,-0.528874568402252,
-1.35253071165684));
#68514=CARTESIAN_POINT('Ctrl Pts',(0.377378882337932,-0.396581239041707,
-1.33862108171108));
#68515=CARTESIAN_POINT('Ctrl Pts',(0.521213647312955,-0.16741515418028,
-1.32471145176532));
#68516=CARTESIAN_POINT('Ctrl Pts',(0.537731743597658,0.102645369705129,
-1.31080182181956));
#68517=CARTESIAN_POINT('Ctrl Pts',(0.422898301800352,0.347632746341392,
-1.29689219187381));
#68518=CARTESIAN_POINT('Ctrl Pts',(0.204763645121989,0.50770399804496,-1.28298256192804));
#68519=CARTESIAN_POINT('Ctrl Pts',(-0.0633885529239486,0.543758578187681,
-1.26907293198229));
#68520=CARTESIAN_POINT('Ctrl Pts',(-0.316056852125366,0.446989447547798,
-1.25516330203653));
#68521=CARTESIAN_POINT('Ctrl Pts',(-0.491522058628041,0.241034366588115,
-1.24125367209077));
#68522=CARTESIAN_POINT('Ctrl Pts',(-0.54692335004532,-0.0237980917236146,
-1.22734404214501));
#68523=CARTESIAN_POINT('Ctrl Pts',(-0.468727873005551,-0.282817398796772,
-1.21343441219925));
#68524=CARTESIAN_POINT('Ctrl Pts',(-0.276036408339551,-0.472753002386535,
-1.19952478225349));
#68525=CARTESIAN_POINT('Ctrl Pts',(-0.0159176302710459,-0.547209401455269,
-1.18561515230773));
#68526=CARTESIAN_POINT('Ctrl Pts',(0.248089341573656,-0.487999158392747,
-1.17170552236197));
#68527=CARTESIAN_POINT('Ctrl Pts',(0.451495619884012,-0.309585537808265,
-1.15779589241622));
#68528=CARTESIAN_POINT('Ctrl Pts',(0.544615226791482,-0.0555495701274412,
-1.14388626247046));
#68529=CARTESIAN_POINT('Ctrl Pts',(0.504701869672432,0.212055470911817,
-1.1299766325247));
#68530=CARTESIAN_POINT('Ctrl Pts',(0.341505169801825,0.427861798941093,
-1.11606700257894));
#68531=CARTESIAN_POINT('Ctrl Pts',(0.0948891258986073,0.539154480441997,
-1.10215737263318));
#68532=CARTESIAN_POINT('Ctrl Pts',(-0.174905450390763,0.51874809244766,
-1.08824774268742));
#68533=CARTESIAN_POINT('Ctrl Pts',(-0.401975935716025,0.371627295956186,
-1.07433811274166));
#68534=CARTESIAN_POINT('Ctrl Pts',(-0.530855904939337,0.133729234595581,
-1.0604284827959));
#68535=CARTESIAN_POINT('Ctrl Pts',(-0.530063894697224,-0.136834818423128,
-1.04651885285014));
#68536=CARTESIAN_POINT('Ctrl Pts',(-0.399793369044433,-0.373974279947941,
-1.03260922290438));
#68537=CARTESIAN_POINT('Ctrl Pts',(-0.171865462059389,-0.519763179674737,
-1.01869959295862));
#68538=CARTESIAN_POINT('Ctrl Pts',(0.0980439590420491,-0.53858971591541,
-1.00478996301287));
#68539=CARTESIAN_POINT('Ctrl Pts',(0.344004217809009,-0.425855137487025,
-0.990880333067106));
#68540=CARTESIAN_POINT('Ctrl Pts',(0.505934690992543,-0.209097078996244,
-0.976970703121349));
#68541=CARTESIAN_POINT('Ctrl Pts',(0.544280680607551,0.058737047183714,
-0.963061073175588));
#68542=CARTESIAN_POINT('Ctrl Pts',(0.449675425671115,0.312223496140158,
-0.949151443229832));
#68543=CARTESIAN_POINT('Ctrl Pts',(0.245228117512358,0.48944322487478,-0.93524181328407));
#68544=CARTESIAN_POINT('Ctrl Pts',(-0.0191209740164775,0.547106834491346,
-0.921332183338313));
#68545=CARTESIAN_POINT('Ctrl Pts',(-0.278799392153621,0.471128855971752,
-0.907422553392553));
#68546=CARTESIAN_POINT('Ctrl Pts',(-0.470375583833576,0.280068402587124,
-0.893512923446795));
#68547=CARTESIAN_POINT('Ctrl Pts',(-0.54705330216063,0.0205957420267234,
-0.879603293501035));
#68548=CARTESIAN_POINT('Ctrl Pts',(-0.490102508674538,-0.243907832972633,
-0.865693663555277));
#68549=CARTESIAN_POINT('Ctrl Pts',(-0.313434553055607,-0.448832130027823,
-0.851784033609516));
#68550=CARTESIAN_POINT('Ctrl Pts',(-0.0602040527811273,-0.544120365381786,
-0.83787440366376));
#68551=CARTESIAN_POINT('Ctrl Pts',(0.207732469642362,-0.506496516326388,
-0.823964773717998));
#68552=CARTESIAN_POINT('Ctrl Pts',(0.424926257008878,-0.345150946831826,
-0.810055143772242));
#68553=CARTESIAN_POINT('Ctrl Pts',(0.538323461610678,-0.0994954806711237,
-0.79614551382648));
#68554=CARTESIAN_POINT('Ctrl Pts',(0.520224589385922,0.170463710486215,
-0.782235883880723));
#68555=CARTESIAN_POINT('Ctrl Pts',(0.375050645292154,0.398783792875813,
-0.768326253934963));
#68556=CARTESIAN_POINT('Ctrl Pts',(0.138263216027914,0.529693102737896,
-0.754416623989205));
#68557=CARTESIAN_POINT('Ctrl Pts',(-0.132297718895352,0.531214470406791,
-0.740506994043446));
#68558=CARTESIAN_POINT('Ctrl Pts',(-0.370542337981686,0.402976271953508,
-0.726597364097687));
#68559=CARTESIAN_POINT('Ctrl Pts',(-0.518274714490022,0.176303205628164,
-0.712687734151928));
#68560=CARTESIAN_POINT('Ctrl Pts',(-0.539408314363338,-0.0934353808264442,
-0.698778104206169));
#68561=CARTESIAN_POINT('Ctrl Pts',(-0.428780840821461,-0.340350540676703,
-0.68486847426041));
#68562=CARTESIAN_POINT('Ctrl Pts',(-0.213415226724241,-0.50412839733219,
-0.670958844314651));
#68563=CARTESIAN_POINT('Ctrl Pts',(0.0540812474423478,-0.544762993116785,
-0.657049214368891));
#68564=CARTESIAN_POINT('Ctrl Pts',(0.308367314900525,-0.45232853004815,
-0.643139584423134));
#68565=CARTESIAN_POINT('Ctrl Pts',(0.487328610130435,-0.249403940912765,
-0.629229954477374));
#68566=CARTESIAN_POINT('Ctrl Pts',(0.547250322419351,0.0144424584609956,
-0.615320324531616));
#68567=CARTESIAN_POINT('Ctrl Pts',(0.473495396827942,0.274761003741857,
-0.601410694585855));
#68568=CARTESIAN_POINT('Ctrl Pts',(0.284079922294417,0.467963778238956,
-0.587501064640098));
#68569=CARTESIAN_POINT('Ctrl Pts',(0.0252723481203937,0.546857210261474,
-0.573591434694337));
#68570=CARTESIAN_POINT('Ctrl Pts',(-0.239708493367827,0.492170029767972,
-0.55968180474858));
#68571=CARTESIAN_POINT('Ctrl Pts',(-0.446135828074901,0.317260654513612,
-0.545772174802819));
#68572=CARTESIAN_POINT('Ctrl Pts',(-0.543585725781381,0.0648541341875027,
-0.531862544857062));
#68573=CARTESIAN_POINT('Ctrl Pts',(-0.508254135299884,-0.203394281987098,
-0.517952914911301));
#68574=CARTESIAN_POINT('Ctrl Pts',(-0.348771491429709,-0.421959650630693,
-0.504043284965544));
#68575=CARTESIAN_POINT('Ctrl Pts',(-0.10409456177691,-0.537453088374187,
-0.490133655019784));
#68576=CARTESIAN_POINT('Ctrl Pts',(0.166009508747088,-0.521663055046103,
-0.476224025074026));
#68577=CARTESIAN_POINT('Ctrl Pts',(0.395562496747523,-0.378446576363621,
-0.462314395128266));
#68578=CARTESIAN_POINT('Ctrl Pts',(0.528491577057985,-0.142787089658862,
-0.448404765182507));
#68579=CARTESIAN_POINT('Ctrl Pts',(0.532326211417529,0.127750947676867,
-0.434495135236748));
#68580=CARTESIAN_POINT('Ctrl Pts',(0.406129715081226,0.367083307332981,
-0.42058550529099));
#68581=CARTESIAN_POINT('Ctrl Pts',(0.180728060463137,0.516748360573824,
-0.40667587534523));
#68582=CARTESIAN_POINT('Ctrl Pts',(-0.0888199719706895,0.540187479097346,
-0.392766245399471));
#68583=CARTESIAN_POINT('Ctrl Pts',(-0.336671982048404,0.431675197918763,
-0.378856615453713));
#68584=CARTESIAN_POINT('Ctrl Pts',(-0.502285249113782,0.217717772625464,
-0.364946985507953));
#68585=CARTESIAN_POINT('Ctrl Pts',(-0.545205480455905,-0.0494214940640173,
-0.351037355562195));
#68586=CARTESIAN_POINT('Ctrl Pts',(-0.454948566721971,-0.304488590315269,
-0.337127725616434));
#68587=CARTESIAN_POINT('Ctrl Pts',(-0.253561531514476,-0.485178368983532,
-0.323218095670677));
#68588=CARTESIAN_POINT('Ctrl Pts',(0.00976288708398863,-0.547353803342409,
-0.309308465724917));
#68589=CARTESIAN_POINT('Ctrl Pts',(0.270702528786763,-0.47582732256143,
-0.295398835779159));
#68590=CARTESIAN_POINT('Ctrl Pts',(0.465517761924972,-0.288070674208134,
-0.2814892058334));
#68591=CARTESIAN_POINT('Ctrl Pts',(0.546621140081346,-0.0299471066453085,
-0.267579575887642));
#68592=CARTESIAN_POINT('Ctrl Pts',(0.494201570549062,0.235491629712694,
-0.253669945941882));
#68593=CARTESIAN_POINT('Ctrl Pts',(0.321063562427973,0.443406911220529,
-0.239760315996123));
#68594=CARTESIAN_POINT('Ctrl Pts',(0.0694994744885192,0.543011346917461,
-0.225850686050364));
#68595=CARTESIAN_POINT('Ctrl Pts',(-0.199041225264239,0.509974598409885,
-0.211941056104605));
#68596=CARTESIAN_POINT('Ctrl Pts',(-0.418962196343987,0.352366538310738,
-0.198031426158846));
#68597=CARTESIAN_POINT('Ctrl Pts',(-0.536543425021737,0.108686034176255,
-0.184121796213087));
#68598=CARTESIAN_POINT('Ctrl Pts',(-0.523063382978388,-0.161543173102966,
-0.170212166267328));
#68599=CARTESIAN_POINT('Ctrl Pts',(-0.381814843430422,-0.392312278325139,
-0.156302536321569));
#68600=CARTESIAN_POINT('Ctrl Pts',(-0.147300519841655,-0.527251424532697,
-0.14239290637581));
#68601=CARTESIAN_POINT('Ctrl Pts',(0.123194827533574,-0.53339901926763,
-0.128483276430052));
#68602=CARTESIAN_POINT('Ctrl Pts',(0.363597459691447,-0.409253501481856,
-0.114573646484293));
#68603=CARTESIAN_POINT('Ctrl Pts',(0.515184192741152,-0.185139637443695,
-0.100664016538534));
#68604=CARTESIAN_POINT('Ctrl Pts',(0.540927225013145,0.0841979416117195,
-0.0867543865927742));
#68605=CARTESIAN_POINT('Ctrl Pts',(0.434537856760124,0.332969061526306,
-0.0728447566470156));
#68606=CARTESIAN_POINT('Ctrl Pts',(0.222004676584789,0.500404891193716,
-0.0589351267012565));
#68607=CARTESIAN_POINT('Ctrl Pts',(-0.0447586639977449,0.545609067649857,
-0.0450254967554974));
#68608=CARTESIAN_POINT('Ctrl Pts',(-0.3005865578387,0.457533473038136,-0.0311158668097381));
#68609=CARTESIAN_POINT('Ctrl Pts',(-0.48299470744761,0.257704243926052,
-0.0172062368639793));
#68610=CARTESIAN_POINT('Ctrl Pts',(-0.547413259618935,-0.00508977246547882,
-0.00329660691822061));
#68611=CARTESIAN_POINT('Ctrl Pts',(-0.478132365439005,-0.266610029387846,
0.010613023027538));
#68612=CARTESIAN_POINT('Ctrl Pts',(-0.292024218105601,-0.463067892827328,
0.0245226529732968));
#68613=CARTESIAN_POINT('Ctrl Pts',(-0.120447234018584,-0.518529242900151,
0.033795739603803));
#68614=CARTESIAN_POINT('Ctrl Pts',(-0.0332073864096211,-0.524057278571678,
0.0384322829190561));
#68615=CARTESIAN_POINT('Ctrl Pts',(0.285706463458477,-0.400329423553965,
-3.948325));
#68616=CARTESIAN_POINT('Ctrl Pts',(0.35234932738247,-0.352767850893538,
-3.94368845668475));
#68617=CARTESIAN_POINT('Ctrl Pts',(0.461355386710151,-0.223767338793563,
-3.93441537005424));
#68618=CARTESIAN_POINT('Ctrl Pts',(0.512153850375005,0.024551470863185,
-3.92050574010848));
#68619=CARTESIAN_POINT('Ctrl Pts',(0.437852459283724,0.266806684479465,
-3.90659611016272));
#68620=CARTESIAN_POINT('Ctrl Pts',(0.256595437328703,0.443921775016828,
-3.89268648021697));
#68621=CARTESIAN_POINT('Ctrl Pts',(0.0126607096365889,0.51258367325088,
-3.8787768502712));
#68622=CARTESIAN_POINT('Ctrl Pts',(-0.234367035151384,0.456045416423434,
-3.86486722032544));
#68623=CARTESIAN_POINT('Ctrl Pts',(-0.424145829883178,0.288104776438461,
-3.85095759037969));
#68624=CARTESIAN_POINT('Ctrl Pts',(-0.510318778475725,0.0497911051028911,
-3.83704796043392));
#68625=CARTESIAN_POINT('Ctrl Pts',(-0.471836291860887,-0.200686156364057,
-3.82313833048817));
#68626=CARTESIAN_POINT('Ctrl Pts',(-0.318098551972822,-0.402141302407426,
-3.80922870054241));
#68627=CARTESIAN_POINT('Ctrl Pts',(-0.086658980441776,-0.505365835465607,
-3.79531907059665));
#68628=CARTESIAN_POINT('Ctrl Pts',(0.165948741836808,-0.485144687019642,
-3.7814094406509));
#68629=CARTESIAN_POINT('Ctrl Pts',(0.378020228680476,-0.346417499554377,
-3.76749981070513));
#68630=CARTESIAN_POINT('Ctrl Pts',(0.497752849465234,-0.123070995229855,
-3.75359018075938));
#68631=CARTESIAN_POINT('Ctrl Pts',(0.495899563082201,0.130337996110901,
-3.73968055081361));
#68632=CARTESIAN_POINT('Ctrl Pts',(0.372913069708243,0.351909382815266,
-3.72577092086785));
#68633=CARTESIAN_POINT('Ctrl Pts',(0.158835236222117,0.487519986810459,
-3.7118612909221));
#68634=CARTESIAN_POINT('Ctrl Pts',(-0.0940412229640735,0.504044263082503,
-3.69795166097634));
#68635=CARTESIAN_POINT('Ctrl Pts',(-0.323946266642341,0.397445828529313,
-3.68404203103058));
#68636=CARTESIAN_POINT('Ctrl Pts',(-0.474721073230568,0.193763446229383,
-3.67013240108482));
#68637=CARTESIAN_POINT('Ctrl Pts',(-0.509535935329301,-0.0572494632079747,
-3.65622277113906));
#68638=CARTESIAN_POINT('Ctrl Pts',(-0.419886639219421,-0.294278066833141,
-3.6423131411933));
#68639=CARTESIAN_POINT('Ctrl Pts',(-0.227671785951002,-0.459423473843918,
-3.62840351124754));
#68640=CARTESIAN_POINT('Ctrl Pts',(0.0201563719388868,-0.512345675389839,
-3.61449388130178));
#68641=CARTESIAN_POINT('Ctrl Pts',(0.263060940163059,-0.440117384557558,
-3.60058425135602));
#68642=CARTESIAN_POINT('Ctrl Pts',(0.441707707892028,-0.260381779728162,
-3.58667462141027));
#68643=CARTESIAN_POINT('Ctrl Pts',(0.512458693932598,-0.0170428119589638,
-3.57276499146451));
#68644=CARTESIAN_POINT('Ctrl Pts',(0.458031580571258,0.230459197312829,
-3.55885536151875));
#68645=CARTESIAN_POINT('Ctrl Pts',(0.291721259059309,0.421667021996254,
-3.54494573157299));
#68646=CARTESIAN_POINT('Ctrl Pts',(0.0541522913452231,0.509874396070913,
-3.53103610162723));
#68647=CARTESIAN_POINT('Ctrl Pts',(-0.196644436945652,0.473534936245239,
-3.51712647168147));
#68648=CARTESIAN_POINT('Ctrl Pts',(-0.399406899907004,0.321525269198555,
-3.50321684173571));
#68649=CARTESIAN_POINT('Ctrl Pts',(-0.504606384212198,0.0909767411968328,
-3.48930721178995));
#68650=CARTESIAN_POINT('Ctrl Pts',(-0.486545849964599,-0.161794642398108,
-3.4753975818442));
#68651=CARTESIAN_POINT('Ctrl Pts',(-0.349636937317957,-0.3750445073447,
-3.46148795189843));
#68652=CARTESIAN_POINT('Ctrl Pts',(-0.127322336735289,-0.496682386435005,
-3.44757832195268));
#68653=CARTESIAN_POINT('Ctrl Pts',(0.12609324488764,-0.496995839037123,
-3.43366869200692));
#68654=CARTESIAN_POINT('Ctrl Pts',(0.348708075290391,-0.375908298197551,
-3.41975906206116));
#68655=CARTESIAN_POINT('Ctrl Pts',(0.486144110547877,-0.162997773623204,
-3.4058494321154));
#68656=CARTESIAN_POINT('Ctrl Pts',(0.504829900148016,0.0897281580277445,
-3.39193980216964));
#68657=CARTESIAN_POINT('Ctrl Pts',(0.40020107303874,0.320536225043519,-3.37803017222388));
#68658=CARTESIAN_POINT('Ctrl Pts',(0.197815274890308,0.473047024561597,
-3.36412054227812));
#68659=CARTESIAN_POINT('Ctrl Pts',(-0.0528907887479718,0.51000679886853,
-3.35021091233236));
#68660=CARTESIAN_POINT('Ctrl Pts',(-0.29067723859158,0.422387397292203,
-3.3363012823866));
#68661=CARTESIAN_POINT('Ctrl Pts',(-0.457460064734289,0.231591579293824,
-3.32239165244084));
#68662=CARTESIAN_POINT('Ctrl Pts',(-0.512499286692634,-0.0157750298272154,
-3.30848202249509));
#68663=CARTESIAN_POINT('Ctrl Pts',(-0.442350493670444,-0.259288278130775,
-3.29457239254933));
#68664=CARTESIAN_POINT('Ctrl Pts',(-0.264148905910468,-0.439465272726765,
-3.28066276260357));
#68665=CARTESIAN_POINT('Ctrl Pts',(-0.0214237606571462,-0.512294244458996,
-3.26675313265781));
#68666=CARTESIAN_POINT('Ctrl Pts',(0.226534558845831,-0.459985286802776,
-3.25284350271205));
#68667=CARTESIAN_POINT('Ctrl Pts',(0.419157363777824,-0.295315889882908,
-3.2389338727663));
#68668=CARTESIAN_POINT('Ctrl Pts',(0.509392751403437,-0.0585097875927088,
-3.22502424282053));
#68669=CARTESIAN_POINT('Ctrl Pts',(0.475198956297498,0.192588479303088,
-3.21111461287478));
#68670=CARTESIAN_POINT('Ctrl Pts',(0.324928484395358,0.396643228172426,
-3.19720498292901));
#68671=CARTESIAN_POINT('Ctrl Pts',(0.0952878493958325,0.503810079478394,
-3.18329535298326));
#68672=CARTESIAN_POINT('Ctrl Pts',(-0.157628714033977,0.487911425300231,
-3.1693857230375));
#68673=CARTESIAN_POINT('Ctrl Pts',(-0.372041368626771,0.35283082413081,
-3.15547609309174));
#68674=CARTESIAN_POINT('Ctrl Pts',(-0.49557561296929,0.131564365451365,
-3.14156646314598));
#68675=CARTESIAN_POINT('Ctrl Pts',(-0.498055781976883,-0.12183927308509,
-3.12765683320022));
#68676=CARTESIAN_POINT('Ctrl Pts',(-0.378876045665121,-0.345481276551521,
-3.11374720325446));
#68677=CARTESIAN_POINT('Ctrl Pts',(-0.167148395020481,-0.484732693830926,
-3.0998375733087));
#68678=CARTESIAN_POINT('Ctrl Pts',(0.0854085334848828,-0.505578631702793,
-3.08592794336294));
#68679=CARTESIAN_POINT('Ctrl Pts',(0.317102750476299,-0.402927060479777,
-3.07201831341718));
#68680=CARTESIAN_POINT('Ctrl Pts',(0.47133839355793,-0.201852642253547,
-3.05810868347143));
#68681=CARTESIAN_POINT('Ctrl Pts',(0.510440378104306,0.0485282477248127,
-3.04419905352566));
#68682=CARTESIAN_POINT('Ctrl Pts',(0.424857276524671,0.287055160222818,
-3.03028942357991));
#68683=CARTESIAN_POINT('Ctrl Pts',(0.235494442018191,0.455463212790065,
-3.01637979363415));
#68684=CARTESIAN_POINT('Ctrl Pts',(-0.0113925344738468,0.512615431473507,
-3.00247016368839));
#68685=CARTESIAN_POINT('Ctrl Pts',(-0.255496660699727,0.444551264532895,
-2.98856053374263));
#68686=CARTESIAN_POINT('Ctrl Pts',(-0.437190710233471,0.267896721353699,
-2.97465090379687));
#68687=CARTESIAN_POINT('Ctrl Pts',(-0.512092343459165,0.0258031431614133,
-2.96074127385111));
#68688=CARTESIAN_POINT('Ctrl Pts',(-0.46190536558045,-0.222593359457327,
-2.94683164390536));
#68689=CARTESIAN_POINT('Ctrl Pts',(-0.29888893149109,-0.416617062851034,
-2.93292201395959));
#68690=CARTESIAN_POINT('Ctrl Pts',(-0.0628630064529875,-0.5088738673249,
-2.91901238401384));
#68691=CARTESIAN_POINT('Ctrl Pts',(0.188518442383684,-0.476828236692982,
-2.90510275406808));
#68692=CARTESIAN_POINT('Ctrl Pts',(0.393850559636817,-0.328307945533265,
-2.89119312412232));
#68693=CARTESIAN_POINT('Ctrl Pts',(0.502976943457436,-0.0995919915290553,
-2.87728349417656));
#68694=CARTESIAN_POINT('Ctrl Pts',(0.489241331627754,0.153451262144076,
-2.8633738642308));
#68695=CARTESIAN_POINT('Ctrl Pts',(0.35599891707028,0.369011031639022,-2.84946423428504));
#68696=CARTESIAN_POINT('Ctrl Pts',(0.135796776088882,0.494432610201203,
-2.83555460433928));
#68697=CARTESIAN_POINT('Ctrl Pts',(-0.117576394161712,0.499079314300279,
-2.82164497439352));
#68698=CARTESIAN_POINT('Ctrl Pts',(-0.342229221231611,0.381816095210394,
-2.80773534444777));
#68699=CARTESIAN_POINT('Ctrl Pts',(-0.483285840488613,0.17128679695097,
-2.793825714502));
#68700=CARTESIAN_POINT('Ctrl Pts',(-0.506290402679528,-0.0810826651085765,
-2.77991608455625));
#68701=CARTESIAN_POINT('Ctrl Pts',(-0.405623591737084,-0.313646093954341,
-2.76600645461048));
#68702=CARTESIAN_POINT('Ctrl Pts',(-0.205875253078692,-0.469595305125906,
-2.75209682466473));
#68703=CARTESIAN_POINT('Ctrl Pts',(0.0441621590199009,-0.510836641341642,
-2.73818719471897));
#68704=CARTESIAN_POINT('Ctrl Pts',(0.283412096543389,-0.427296096354025,
-2.72427756477321));
#68705=CARTESIAN_POINT('Ctrl Pts',(0.453433063980492,-0.239380088803917,
-2.71036793482745));
#68706=CARTESIAN_POINT('Ctrl Pts',(0.512694101247579,0.00700920626356338,
-2.69645830488169));
#68707=CARTESIAN_POINT('Ctrl Pts',(0.446719536253416,0.251686365057864,
-2.68254867493593));
#68708=CARTESIAN_POINT('Ctrl Pts',(0.271624952073492,0.434884186695241,
-2.66863904499017));
#68709=CARTESIAN_POINT('Ctrl Pts',(0.0301806393140316,0.511853005693142,
-2.65472941504441));
#68710=CARTESIAN_POINT('Ctrl Pts',(-0.218635887270253,0.463791676535983,
-2.64081978509866));
#68711=CARTESIAN_POINT('Ctrl Pts',(-0.414046304926066,0.302440122674851,
-2.6269101551529));
#68712=CARTESIAN_POINT('Ctrl Pts',(-0.508317781768474,0.0672116296818217,
-2.61300052520714));
#68713=CARTESIAN_POINT('Ctrl Pts',(-0.478422658322387,-0.184434623729516,
-2.59909089526138));
#68714=CARTESIAN_POINT('Ctrl Pts',(-0.331663405555064,-0.391029098459597,
-2.58518126531562));
#68715=CARTESIAN_POINT('Ctrl Pts',(-0.103888852940067,-0.502107037056149,
-2.57127163536986));
#68716=CARTESIAN_POINT('Ctrl Pts',(0.149262592123117,-0.490535471723703,
-2.5573620054241));
#68717=CARTESIAN_POINT('Ctrl Pts',(0.365953717915752,-0.359140984531349,
-2.54345237547834));
#68718=CARTESIAN_POINT('Ctrl Pts',(0.49325346169053,-0.140019259235349,
-2.52954274553259));
#68719=CARTESIAN_POINT('Ctrl Pts',(0.500066361181473,0.113304919757393,
-2.51563311558682));
#68720=CARTESIAN_POINT('Ctrl Pts',(0.384728231899584,0.338952147073784,
-2.50172348564107));
#68721=CARTESIAN_POINT('Ctrl Pts',(0.175412676874732,0.481803656293877,
-2.48781385569531));
#68722=CARTESIAN_POINT('Ctrl Pts',(-0.0767508691435963,0.506965161043843,
-2.47390422574955));
#68723=CARTESIAN_POINT('Ctrl Pts',(-0.310166508178242,0.4082904696794,-2.45999459580379));
#68724=CARTESIAN_POINT('Ctrl Pts',(-0.467817886694874,0.209882813290774,
-2.44608496585803));
#68725=CARTESIAN_POINT('Ctrl Pts',(-0.511195559611515,-0.0397928418183265,
-2.43217533591227));
#68726=CARTESIAN_POINT('Ctrl Pts',(-0.429703678489127,-0.279748313881283,
-2.41826570596651));
#68727=CARTESIAN_POINT('Ctrl Pts',(-0.243248235588849,-0.451369766720613,
-2.40435607602075));
#68728=CARTESIAN_POINT('Ctrl Pts',(0.00262536564176082,-0.512735290263655,
-2.39044644607499));
#68729=CARTESIAN_POINT('Ctrl Pts',(0.247857669758745,-0.448855150319423,
-2.37653681612923));
#68730=CARTESIAN_POINT('Ctrl Pts',(0.432545870731629,-0.275333325515683,
-2.36262718618348));
#68731=CARTESIAN_POINT('Ctrl Pts',(0.511576248657834,-0.0345559290959576,
-2.34871755623772));
#68732=CARTESIAN_POINT('Ctrl Pts',(0.46564408176967,0.214662431597587,-2.33480792629196));
#68733=CARTESIAN_POINT('Ctrl Pts',(0.305969203822596,0.411445277939455,
-2.3208982963462));
#68734=CARTESIAN_POINT('Ctrl Pts',(0.0715553393709438,0.507724535387071,
-2.30698866640044));
#68735=CARTESIAN_POINT('Ctrl Pts',(-0.180337321890193,0.479982104624726,
-2.29307903645468));
#68736=CARTESIAN_POINT('Ctrl Pts',(-0.388179050905097,0.334994619158167,
-2.27916940650892));
#68737=CARTESIAN_POINT('Ctrl Pts',(-0.501200423869475,0.108178119504665,
-2.26525977656316));
#68738=CARTESIAN_POINT('Ctrl Pts',(-0.491793750979322,-0.145063010185908,
-2.2513501466174));
#68739=CARTESIAN_POINT('Ctrl Pts',(-0.362256796811613,-0.362869650963398,
-2.23744051667165));
#68740=CARTESIAN_POINT('Ctrl Pts',(-0.144231506204031,-0.492038253639516,
-2.22353088672589));
#68741=CARTESIAN_POINT('Ctrl Pts',(0.1090251621404,-0.501016850461905,-2.20962125678013));
#68742=CARTESIAN_POINT('Ctrl Pts',(0.33565029365018,-0.387612242839485,
-2.19571162683437));
#68743=CARTESIAN_POINT('Ctrl Pts',(0.480286249602533,-0.179525733167259,
-2.18180199688861));
#68744=CARTESIAN_POINT('Ctrl Pts',(0.507602857467195,0.0724134622680479,
-2.16789236694285));
#68745=CARTESIAN_POINT('Ctrl Pts',(0.410927499343277,0.306664247524861,
-2.15398273699709));
#68746=CARTESIAN_POINT('Ctrl Pts',(0.213875029915099,0.466006268203898,
-2.14007310705133));
#68747=CARTESIAN_POINT('Ctrl Pts',(-0.0354206155412066,0.511517106675026,
-2.12616347710558));
#68748=CARTESIAN_POINT('Ctrl Pts',(-0.276064080079156,0.432079846922483,
-2.11225384715981));
#68749=CARTESIAN_POINT('Ctrl Pts',(-0.449273471848797,0.247098599590194,
-2.09834421721406));
#68750=CARTESIAN_POINT('Ctrl Pts',(-0.512738995510593,0.00175866690871404,
-2.0844345872683));
#68751=CARTESIAN_POINT('Ctrl Pts',(-0.450957950605788,-0.244010854701047,
-2.07052495732254));
#68752=CARTESIAN_POINT('Ctrl Pts',(-0.279021570577783,-0.430175933286389,
-2.05661532737678));
#68753=CARTESIAN_POINT('Ctrl Pts',(-0.0389286926494526,-0.511262092585704,
-2.04270569743102));
#68754=CARTESIAN_POINT('Ctrl Pts',(0.210673282920791,-0.467462445860503,
-2.02879606748526));
#68755=CARTESIAN_POINT('Ctrl Pts',(0.408814172040582,-0.309475916939077,
-2.0148864375395));
#68756=CARTESIAN_POINT('Ctrl Pts',(0.507094171550263,-0.0758938179712873,
-2.00097680759374));
#68757=CARTESIAN_POINT('Ctrl Pts',(0.481506461595899,0.176226836401005,
-1.98706717764799));
#68758=CARTESIAN_POINT('Ctrl Pts',(0.338301342812545,0.385300625327465,
-1.97315754770222));
#68759=CARTESIAN_POINT('Ctrl Pts',(0.112459477653878,0.500257170175825,
-1.95924791775647));
#68760=CARTESIAN_POINT('Ctrl Pts',(-0.140852823344986,0.493016077407475,
-1.94533828781071));
#68761=CARTESIAN_POINT('Ctrl Pts',(-0.359759056244216,0.365346126128058,
-1.93142865786495));
#68762=CARTESIAN_POINT('Ctrl Pts',(-0.490787074886546,0.148433209056515,
-1.91751902791919));
#68763=CARTESIAN_POINT('Ctrl Pts',(-0.501930712655587,-0.104737434184549,
-1.90360939797343));
#68764=CARTESIAN_POINT('Ctrl Pts',(-0.390467917193037,-0.332323902344444,
-1.88969976802767));
#68765=CARTESIAN_POINT('Ctrl Pts',(-0.183625665141514,-0.478733731345353,
-1.87579013808191));
#68766=CARTESIAN_POINT('Ctrl Pts',(0.0680707615702241,-0.508203445330468,
-1.86188050813615));
#68767=CARTESIAN_POINT('Ctrl Pts',(0.303139568028706,-0.413534487947351,
-1.8479708781904));
#68768=CARTESIAN_POINT('Ctrl Pts',(0.464160582092247,-0.217851611098688,
-1.83406124824463));
#68769=CARTESIAN_POINT('Ctrl Pts',(0.511801259025317,0.0310457998223131,
-1.82015161829888));
#68770=CARTESIAN_POINT('Ctrl Pts',(0.43442442794312,0.272359664474753,-1.80624198835312));
#68771=CARTESIAN_POINT('Ctrl Pts',(0.250930899325168,0.447144332615734,
-1.79233235840736));
#68772=CARTESIAN_POINT('Ctrl Pts',(0.00614257089095992,0.512705216717518,
-1.7784227284616));
#68773=CARTESIAN_POINT('Ctrl Pts',(-0.240146201108115,0.453027783386239,
-1.76451309851584));
#68774=CARTESIAN_POINT('Ctrl Pts',(-0.427774547614985,0.282689417628787,
-1.75060346857008));
#68775=CARTESIAN_POINT('Ctrl Pts',(-0.510910560443286,0.0432986103014504,
-1.73669383862433));
#68776=CARTESIAN_POINT('Ctrl Pts',(-0.469246635876068,-0.206668732868568,
-1.72278420867856));
#68777=CARTESIAN_POINT('Ctrl Pts',(-0.312960005664294,-0.406153179577745,
-1.70887457873281));
#68778=CARTESIAN_POINT('Ctrl Pts',(-0.0802267483162252,-0.506426736341114,
-1.69496494878705));
#68779=CARTESIAN_POINT('Ctrl Pts',(0.172103467761028,-0.482995617797032,
-1.68105531884129));
#68780=CARTESIAN_POINT('Ctrl Pts',(0.38239403215543,-0.341583334778529,
-1.66714568889553));
#68781=CARTESIAN_POINT('Ctrl Pts',(0.499277344932229,-0.116732614396888,
-1.65323605894977));
#68782=CARTESIAN_POINT('Ctrl Pts',(0.494202361649382,0.136632339388161,
-1.63932642900401));
#68783=CARTESIAN_POINT('Ctrl Pts',(0.36840874663372,0.35662216115979,-1.62541679905825));
#68784=CARTESIAN_POINT('Ctrl Pts',(0.152624060625208,0.489500016899674,
-1.61150716911249));
#68785=CARTESIAN_POINT('Ctrl Pts',(-0.100442049346334,0.502807880954164,
-1.59759753916673));
#68786=CARTESIAN_POINT('Ctrl Pts',(-0.328973216334069,0.393295046194743,
-1.58368790922097));
#68787=CARTESIAN_POINT('Ctrl Pts',(-0.477146215019956,0.187712173069935,
-1.56977827927521));
#68788=CARTESIAN_POINT('Ctrl Pts',(-0.508766880727387,-0.0637230845254107,
-1.55586864932946));
#68789=CARTESIAN_POINT('Ctrl Pts',(-0.416111244906428,-0.299592727363217,
-1.5419590193837));
#68790=CARTESIAN_POINT('Ctrl Pts',(-0.221812266131596,-0.462280963289723,
-1.52804938943794));
#68791=CARTESIAN_POINT('Ctrl Pts',(0.0266687144847388,-0.512047995889291,
-1.51413975949218));
#68792=CARTESIAN_POINT('Ctrl Pts',(0.268635337881236,-0.436737250149265,
-1.50023012954642));
#68793=CARTESIAN_POINT('Ctrl Pts',(0.44498250467321,-0.254744854631581,
-1.48632049960066));
#68794=CARTESIAN_POINT('Ctrl Pts',(0.512633956353846,-0.0105260258174941,
-1.4724108696549));
#68795=CARTESIAN_POINT('Ctrl Pts',(0.455064497344623,0.23626399150737,-1.45850123970914));
#68796=CARTESIAN_POINT('Ctrl Pts',(0.286336598528917,0.425341889271909,
-1.44459160976338));
#68797=CARTESIAN_POINT('Ctrl Pts',(0.047665362586952,0.510521677929509,
-1.43068197981763));
#68798=CARTESIAN_POINT('Ctrl Pts',(-0.202649074195538,0.47099652138227,
-1.41677234987187));
#68799=CARTESIAN_POINT('Ctrl Pts',(-0.403462495084136,0.316421215292198,
-1.40286271992611));
#68800=CARTESIAN_POINT('Ctrl Pts',(-0.505722278552809,0.0845538136447024,
-1.38895308998035));
#68801=CARTESIAN_POINT('Ctrl Pts',(-0.484449464362613,-0.167967517411213,
-1.37504346003459));
#68802=CARTESIAN_POINT('Ctrl Pts',(-0.344840355124436,-0.379459483876949,
-1.36113383008883));
#68803=CARTESIAN_POINT('Ctrl Pts',(-0.120997217343892,-0.498261019769301,
-1.34722420014307));
#68804=CARTESIAN_POINT('Ctrl Pts',(0.132401866856018,-0.495352516981138,
-1.33331457019731));
#68805=CARTESIAN_POINT('Ctrl Pts',(0.353459195034396,-0.371444434434203,
-1.31940494025155));
#68806=CARTESIAN_POINT('Ctrl Pts',(0.488177173769909,-0.156803754535824,
-1.30549531030579));
#68807=CARTESIAN_POINT('Ctrl Pts',(0.503648291231812,0.0961393216419958,
-1.29158568036004));
#68808=CARTESIAN_POINT('Ctrl Pts',(0.396093423165933,0.325598480572622,
-1.27767605041428));
#68809=CARTESIAN_POINT('Ctrl Pts',(0.191784958206317,0.475523816682518,
-1.26376642046852));
#68810=CARTESIAN_POINT('Ctrl Pts',(-0.0593707489727289,0.509293122467725,
-1.24985679052276));
#68811=CARTESIAN_POINT('Ctrl Pts',(-0.296023984821974,0.418657581845388,
-1.235947160577));
#68812=CARTESIAN_POINT('Ctrl Pts',(-0.460367549206804,0.22575670546814,
-1.22203753063124));
#68813=CARTESIAN_POINT('Ctrl Pts',(-0.512257299229123,-0.0222896795174969,
-1.20812790068548));
#68814=CARTESIAN_POINT('Ctrl Pts',(-0.439018144460899,-0.264891372567355,
-1.19421827073972));
#68815=CARTESIAN_POINT('Ctrl Pts',(-0.258540186688332,-0.442788146062732,
-1.18030864079396));
#68816=CARTESIAN_POINT('Ctrl Pts',(-0.0149087112336633,-0.512525219629101,
-1.1663990108482));
#68817=CARTESIAN_POINT('Ctrl Pts',(0.232364509709674,-0.45706794358595,
-1.15248938090245));
#68818=CARTESIAN_POINT('Ctrl Pts',(0.422878136097861,-0.289962846649199,
-1.13857975095669));
#68819=CARTESIAN_POINT('Ctrl Pts',(0.51009547347383,-0.052028630272347,
-1.12467012101093));
#68820=CARTESIAN_POINT('Ctrl Pts',(0.472711974452847,0.198614600760868,
-1.11076049106517));
#68821=CARTESIAN_POINT('Ctrl Pts',(0.319859292789327,0.400742315263586,
-1.09685086111941));
#68822=CARTESIAN_POINT('Ctrl Pts',(0.0888746976244564,0.504980849685084,
-1.08294123117365));
#68823=CARTESIAN_POINT('Ctrl Pts',(-0.163819287712257,0.485867895008465,
-1.06903160122789));
#68824=CARTESIAN_POINT('Ctrl Pts',(-0.376497195023632,0.348072165744182,
-1.05512197128213));
#68825=CARTESIAN_POINT('Ctrl Pts',(-0.497208268985998,0.125252974728969,
-1.04121234133637));
#68826=CARTESIAN_POINT('Ctrl Pts',(-0.496466459320068,-0.128161715019355,
-1.02730271139061));
#68827=CARTESIAN_POINT('Ctrl Pts',(-0.37445296760404,-0.350270389098243,
-1.01339308144486));
#68828=CARTESIAN_POINT('Ctrl Pts',(-0.160971985229762,-0.48681864220436,
-0.999483451499097));
#68829=CARTESIAN_POINT('Ctrl Pts',(0.091829565624597,-0.50445188204992,
-0.985573821553339));
#68830=CARTESIAN_POINT('Ctrl Pts',(0.322199941771856,-0.398862843529854,
-0.971664191607578));
#68831=CARTESIAN_POINT('Ctrl Pts',(0.473866654939281,-0.195843722807663,
-0.957754561661822));
#68832=CARTESIAN_POINT('Ctrl Pts',(0.509782132080318,0.0550140730918329,
-0.94384493171606));
#68833=CARTESIAN_POINT('Ctrl Pts',(0.421173312613008,0.292433601299668,
-0.929935301770304));
#68834=CARTESIAN_POINT('Ctrl Pts',(0.229684640748129,0.458420479724576,
-0.916025671824541));
#68835=CARTESIAN_POINT('Ctrl Pts',(-0.017909015052109,0.512429153743588,
-0.902116041878785));
#68836=CARTESIAN_POINT('Ctrl Pts',(-0.261128042237548,0.441266944132112,
-0.888206411933025));
#68837=CARTESIAN_POINT('Ctrl Pts',(-0.440561417203972,0.262316618035793,
-0.874296781987266));
#68838=CARTESIAN_POINT('Ctrl Pts',(-0.512379014492537,0.0192903067410717,
-0.860387152041508));
#68839=CARTESIAN_POINT('Ctrl Pts',(-0.459037975647287,-0.228448040788597,
-0.846477522095749));
#68840=CARTESIAN_POINT('Ctrl Pts',(-0.293567896890941,-0.420383468206752,
-0.832567892149989));
#68841=CARTESIAN_POINT('Ctrl Pts',(-0.0563880943787678,-0.509631978234137,
-0.818658262204231));
#68842=CARTESIAN_POINT('Ctrl Pts',(0.194565607506746,-0.474392869678749,
-0.804748632258471));
#68843=CARTESIAN_POINT('Ctrl Pts',(0.397992838976195,-0.323273986813317,
-0.790839002312714));
#68844=CARTESIAN_POINT('Ctrl Pts',(0.504202503940466,-0.0931890843751128,
-0.776929372366952));
#68845=CARTESIAN_POINT('Ctrl Pts',(0.487250806039511,0.159659081922555,
-0.763019742421195));
#68846=CARTESIAN_POINT('Ctrl Pts',(0.351278530374647,0.373507382155073,
-0.749110112475436));
#68847=CARTESIAN_POINT('Ctrl Pts',(0.12949957543287,0.496119169544188,-0.735200482529676));
#68848=CARTESIAN_POINT('Ctrl Pts',(-0.123912193856582,0.497544107230863,
-0.721290852583919));
#68849=CARTESIAN_POINT('Ctrl Pts',(-0.347055976470588,0.377434126202911,
-0.707381222638158));
#68850=CARTESIAN_POINT('Ctrl Pts',(-0.485424521519157,0.165128447986424,
-0.6934715926924));
#68851=CARTESIAN_POINT('Ctrl Pts',(-0.505218594661576,-0.0875130963610043,
-0.67956196274664));
#68852=CARTESIAN_POINT('Ctrl Pts',(-0.401603104826651,-0.318777848383641,
-0.665652332800882));
#68853=CARTESIAN_POINT('Ctrl Pts',(-0.199888170155967,-0.472174850937878,
-0.651742702855122));
#68854=CARTESIAN_POINT('Ctrl Pts',(0.0506533753796834,-0.510233873815872,
-0.637833072909363));
#68855=CARTESIAN_POINT('Ctrl Pts',(0.288821839273072,-0.423658253295539,
-0.623923442963605));
#68856=CARTESIAN_POINT('Ctrl Pts',(0.45643989718452,-0.233595784817902,
-0.610013813017846));
#68857=CARTESIAN_POINT('Ctrl Pts',(0.512563546869181,0.0135270413392405,
-0.596104183072087));
#68858=CARTESIAN_POINT('Ctrl Pts',(0.443483484763275,0.257345622011976,
-0.582194553126329));
#68859=CARTESIAN_POINT('Ctrl Pts',(0.266073872596039,0.438302480883072,
-0.568284923180568));
#68860=CARTESIAN_POINT('Ctrl Pts',(0.0236704920209714,0.51219535163255,
-0.55437529323481));
#68861=CARTESIAN_POINT('Ctrl Pts',(-0.224514871059556,0.460974449508451,
-0.540465663289051));
#68862=CARTESIAN_POINT('Ctrl Pts',(-0.417858067972524,0.297151485705153,
-0.526556033343292));
#68863=CARTESIAN_POINT('Ctrl Pts',(-0.509131226094477,0.0607434362054208,
-0.512646403397532));
#68864=CARTESIAN_POINT('Ctrl Pts',(-0.476039084177294,-0.19050239043684,
-0.498736773451774));
#68865=CARTESIAN_POINT('Ctrl Pts',(-0.326665047731261,-0.395214267223794,
-0.484827143506015));
#68866=CARTESIAN_POINT('Ctrl Pts',(-0.0974966584912855,-0.503387298220306,
-0.470917513560256));
#68867=CARTESIAN_POINT('Ctrl Pts',(0.155487204176033,-0.488598096357353,
-0.457007883614497));
#68868=CARTESIAN_POINT('Ctrl Pts',(0.37049026384305,-0.354459214612929,
-0.443098253668739));
#68869=CARTESIAN_POINT('Ctrl Pts',(0.494993801063038,-0.133736709005703,
-0.429188623722979));
#68870=CARTESIAN_POINT('Ctrl Pts',(0.498585381931524,0.11965361403109,-0.41527899377722));
#68871=CARTESIAN_POINT('Ctrl Pts',(0.380387692291731,0.343816192142657,
-0.401369363831462));
#68872=CARTESIAN_POINT('Ctrl Pts',(0.169272838945517,0.483994913632211,
-0.387459733885702));
#68873=CARTESIAN_POINT('Ctrl Pts',(-0.0831902294088231,0.505948373015826,
-0.373550103939943));
#68874=CARTESIAN_POINT('Ctrl Pts',(-0.315332450581861,0.404314006728254,
-0.359640473994185));
#68875=CARTESIAN_POINT('Ctrl Pts',(-0.470448528358375,0.203918004579725,
-0.345730844048426));
#68876=CARTESIAN_POINT('Ctrl Pts',(-0.510648314649788,-0.0462889746268909,
-0.331821214102667));
#68877=CARTESIAN_POINT('Ctrl Pts',(-0.426112222229761,-0.285188962782551,
-0.317911584156906));
#68878=CARTESIAN_POINT('Ctrl Pts',(-0.237489851752064,-0.454425946376765,
-0.304001954211149));
#68879=CARTESIAN_POINT('Ctrl Pts',(0.00914407872677023,-0.512660468783674,
-0.290092324265389));
#68880=CARTESIAN_POINT('Ctrl Pts',(0.253544388403441,-0.445667604307889,
-0.27618269431963));
#68881=CARTESIAN_POINT('Ctrl Pts',(0.436011502246361,-0.269811675703265,
-0.262273064373872));
#68882=CARTESIAN_POINT('Ctrl Pts',(0.511974244464808,-0.0280489468379449,
-0.248363434428113));
#68883=CARTESIAN_POINT('Ctrl Pts',(0.462877223624254,0.220565288020147,
-0.234453804482355));
#68884=CARTESIAN_POINT('Ctrl Pts',(0.300713351069406,0.41530212009148,-0.220544174536595));
#68885=CARTESIAN_POINT('Ctrl Pts',(0.0650943374357338,0.508593253514698,
-0.206634544590836));
#68886=CARTESIAN_POINT('Ctrl Pts',(-0.186425246756546,0.477650497890165,
-0.192724914645077));
#68887=CARTESIAN_POINT('Ctrl Pts',(-0.392406802818875,0.330032227073166,
-0.178815284699318));
#68888=CARTESIAN_POINT('Ctrl Pts',(-0.502535292738926,0.101797106169335,
-0.164905654753559));
#68889=CARTESIAN_POINT('Ctrl Pts',(-0.489909666259365,-0.151303961616872,
-0.1509960248078));
#68890=CARTESIAN_POINT('Ctrl Pts',(-0.357613988294798,-0.367446056440282,
-0.137086394862041));
#68891=CARTESIAN_POINT('Ctrl Pts',(-0.137964061075247,-0.493832254050675,
-0.123176764916282));
#68892=CARTESIAN_POINT('Ctrl Pts',(0.115386277850666,-0.499590191201122,
-0.109267134970524));
#68893=CARTESIAN_POINT('Ctrl Pts',(0.340551290583365,-0.383313481407925,
-0.0953575050247649));
#68894=CARTESIAN_POINT('Ctrl Pts',(0.482529888616476,-0.173404793650348,
-0.0814478750790055));
#68895=CARTESIAN_POINT('Ctrl Pts',(0.506641231064238,0.0788611606491063,
-0.0675382451332463));
#68896=CARTESIAN_POINT('Ctrl Pts',(0.406995219528124,0.311864235034375,
-0.0536286151874873));
#68897=CARTESIAN_POINT('Ctrl Pts',(0.207933188506461,0.468687354567501,
-0.0397189852417286));
#68898=CARTESIAN_POINT('Ctrl Pts',(-0.0419216921981646,0.511026320975463,
-0.0258093552959692));
#68899=CARTESIAN_POINT('Ctrl Pts',(-0.281534255742185,0.428533287500004,
-0.01189972535021));
#68900=CARTESIAN_POINT('Ctrl Pts',(-0.452380693489446,0.241369983531519,
0.00200990459554883));
#68901=CARTESIAN_POINT('Ctrl Pts',(-0.512716156498659,-0.00476716361925517,
0.0159195345413075));
#68902=CARTESIAN_POINT('Ctrl Pts',(-0.447826544932705,-0.249711286947794,
0.0298291644870661));
#68903=CARTESIAN_POINT('Ctrl Pts',(-0.273514629177701,-0.433716915029852,
0.0437387944328249));
#68904=CARTESIAN_POINT('Ctrl Pts',(-0.112812837105721,-0.485662916965135,
0.053011881063331));
#68905=CARTESIAN_POINT('Ctrl Pts',(-0.0311025778570991,-0.490840565026611,
0.0576484243785842));
#68906=CARTESIAN_POINT('',(-0.0374170035146652,-0.590490705661811,0.));
#68907=CARTESIAN_POINT('Ctrl Pts',(-0.416126897194384,0.262207742448202,
-3.46944695195361E-16));
#68908=CARTESIAN_POINT('Ctrl Pts',(-0.423456757845617,0.252783076367721,
-2.81103177996561E-16));
#68909=CARTESIAN_POINT('Ctrl Pts',(-0.430430889999018,0.243100779102031,
-6.06387724157159E-16));
#68910=CARTESIAN_POINT('Ctrl Pts',(-0.437033887600588,0.23317991320548,
-4.92661467177413E-16));
#68911=CARTESIAN_POINT('Ctrl Pts',(-0.448776940256658,0.215536222014478,
-2.9040583955556E-16));
#68912=CARTESIAN_POINT('Ctrl Pts',(-0.459347224703845,0.197138928554313,
-2.70434607762433E-17));
#68913=CARTESIAN_POINT('Ctrl Pts',(-0.468722856687143,0.178121194347624,
-2.15105711021124E-16));
#68914=CARTESIAN_POINT('Ctrl Pts',(-0.472737812302806,0.169977171748789,
-2.9564018475687E-16));
#68915=CARTESIAN_POINT('Ctrl Pts',(-0.476533480487776,0.161719154066443,
5.04918675384624E-16));
#68916=CARTESIAN_POINT('Ctrl Pts',(-0.480107142500344,0.153356755948507,
4.9960036108132E-16));
#68917=CARTESIAN_POINT('Ctrl Pts',(-0.482712193460394,0.147260915555978,
4.95723531170447E-16));
#68918=CARTESIAN_POINT('Ctrl Pts',(-0.485198246772411,0.141111675674135,
1.86231101641602E-15));
#68919=CARTESIAN_POINT('Ctrl Pts',(-0.487561379590333,0.134921318921676,
1.80411241501588E-15));
#68920=CARTESIAN_POINT('Ctrl Pts',(-0.496114159650689,0.112516839834682,
1.59347684099283E-15));
#68921=CARTESIAN_POINT('Ctrl Pts',(-0.503072184875732,0.0895449453933402,
1.51969670221732E-15));
#68922=CARTESIAN_POINT('Ctrl Pts',(-0.508399533149054,0.0661879148866036,
8.32667268468867E-16));
#68923=CARTESIAN_POINT('Ctrl Pts',(-0.510644266283795,0.0563461892066425,
5.43180331374654E-16));
#68924=CARTESIAN_POINT('Ctrl Pts',(-0.512599142677303,0.046435830069688,
1.58032048240269E-15));
#68925=CARTESIAN_POINT('Ctrl Pts',(-0.514259891977282,0.0364695744349397,
1.59594559789866E-15));
#68926=CARTESIAN_POINT('Ctrl Pts',(-0.515360081604947,0.0298672708385183,
1.60629670266802E-15));
#68927=CARTESIAN_POINT('Ctrl Pts',(-0.516331496812872,0.0232377441031986,
9.27056533275263E-16));
#68928=CARTESIAN_POINT('Ctrl Pts',(-0.517171545692938,0.0165936208095082,
8.95117313604032E-16));
#68929=CARTESIAN_POINT('Ctrl Pts',(-0.518072885339055,0.00946473595482552,
8.60847778058109E-16));
#68930=CARTESIAN_POINT('Ctrl Pts',(-0.518822529669948,0.00232377075164661,
9.51323429436439E-16));
#68931=CARTESIAN_POINT('Ctrl Pts',(-0.519419892085964,-0.00482444278728938,
9.99200722162641E-16));
#68932=CARTESIAN_POINT('Ctrl Pts',(-0.521658993972392,-0.0316181914237927,
1.17847232452288E-15));
#68933=CARTESIAN_POINT('Ctrl Pts',(-0.521762558905488,-0.0585122034193784,
7.45081943606969E-16));
#68934=CARTESIAN_POINT('Ctrl Pts',(-0.51982826242077,-0.0852697613657021,
6.80011602582908E-16));
#68935=CARTESIAN_POINT('Ctrl Pts',(-0.518558307423402,-0.102837334227329,
6.37289917765324E-16));
#68936=CARTESIAN_POINT('Ctrl Pts',(-0.516408879605909,-0.120346639156886,
9.3813456749543E-16));
#68937=CARTESIAN_POINT('Ctrl Pts',(-0.51339580078198,-0.137733394192191,
9.99200722162641E-16));
#68938=CARTESIAN_POINT('Ctrl Pts',(-0.510987430814588,-0.151630720184754,
1.04801122514605E-15));
#68939=CARTESIAN_POINT('Ctrl Pts',(-0.508027102869678,-0.165449816645127,
8.85342351292076E-16));
#68940=CARTESIAN_POINT('Ctrl Pts',(-0.504518647045066,-0.179157643895939,
9.99200722162641E-16));
#68941=CARTESIAN_POINT('Ctrl Pts',(-0.502965597266262,-0.185225537905152,
1.04960116228077E-15));
#68942=CARTESIAN_POINT('Ctrl Pts',(-0.501306004368436,-0.191267606929154,
1.52465683996833E-15));
#68943=CARTESIAN_POINT('Ctrl Pts',(-0.499543447133405,-0.197271810403005,
1.46410661372443E-15));
#68944=CARTESIAN_POINT('Ctrl Pts',(-0.492776236939559,-0.220324512548841,
1.23162842797623E-15));
#68945=CARTESIAN_POINT('Ctrl Pts',(-0.484483280990387,-0.242859221574429,
8.43887503199872E-16));
#68946=CARTESIAN_POINT('Ctrl Pts',(-0.47471735717438,-0.26471982397249,
4.92661467177413E-16));
#68947=CARTESIAN_POINT('Ctrl Pts',(-0.465268640557773,-0.285870371633841,
1.53167248280808E-16));
#68948=CARTESIAN_POINT('Ctrl Pts',(-0.454440972414739,-0.306390519760755,
1.13612733355049E-15));
#68949=CARTESIAN_POINT('Ctrl Pts',(-0.442338530304677,-0.32618075080411,
1.13450915328883E-15));
#68950=CARTESIAN_POINT('Ctrl Pts',(-0.434728174109778,-0.338625405035842,
1.13349159600024E-15));
#68951=CARTESIAN_POINT('Ctrl Pts',(-0.426613216462773,-0.350781336469998,
3.00879890662803E-16));
#68952=CARTESIAN_POINT('Ctrl Pts',(-0.418014837814341,-0.362621829072243,
4.30211422042248E-16));
#68953=CARTESIAN_POINT('Ctrl Pts',(-0.413274602275642,-0.36914942295055,
5.01511134044471E-16));
#68954=CARTESIAN_POINT('Ctrl Pts',(-0.408385147719558,-0.375583552328859,
6.51549061365782E-16));
#68955=CARTESIAN_POINT('Ctrl Pts',(-0.403366333700444,-0.381899519271175,
7.11236625150491E-16));
#68956=CARTESIAN_POINT('Ctrl Pts',(-0.385533464976329,-0.404341436608463,
9.23318699796284E-16));
#68957=CARTESIAN_POINT('Ctrl Pts',(-0.366035043915957,-0.425345967666594,
-5.57238779820851E-16));
#68958=CARTESIAN_POINT('Ctrl Pts',(-0.345069333505709,-0.444737671558352,
-3.64291929955129E-16));
#68959=CARTESIAN_POINT('Ctrl Pts',(-0.331576851910909,-0.457217201358757,
-2.40120997053403E-16));
#68960=CARTESIAN_POINT('Ctrl Pts',(-0.317475581157184,-0.469028537099824,
9.23032294553399E-16));
#68961=CARTESIAN_POINT('Ctrl Pts',(-0.302808350652492,-0.480119506590464,
9.03790930983916E-16));
#68962=CARTESIAN_POINT('Ctrl Pts',(-0.291140523150296,-0.488942407328781,
8.87259861740289E-16));
#68963=CARTESIAN_POINT('Ctrl Pts',(-0.279114374699222,-0.497309373181222,
1.62196618340084E-15));
#68964=CARTESIAN_POINT('Ctrl Pts',(-0.266759816115952,-0.505209972003307,
1.64451785522601E-15));
#68965=CARTESIAN_POINT('Ctrl Pts',(-0.261397323725431,-0.508639224515927,
1.65430640151368E-15));
#68966=CARTESIAN_POINT('Ctrl Pts',(-0.255972929899824,-0.51198057793193,
5.15295006550516E-16));
#68967=CARTESIAN_POINT('Ctrl Pts',(-0.250488958758761,-0.515233006220709,
4.82253126321552E-16));
#68968=CARTESIAN_POINT('Ctrl Pts',(-0.244806899749902,-0.518602916270116,
4.48017732225684E-16));
#68969=CARTESIAN_POINT('Ctrl Pts',(-0.239068043186357,-0.521873056054226,
8.87214571818307E-16));
#68970=CARTESIAN_POINT('Ctrl Pts',(-0.233279325439751,-0.525040899581259,
8.62157567560473E-16));
#68971=CARTESIAN_POINT('Ctrl Pts',(-0.207742211930793,-0.539015942633911,
7.51617791752285E-16));
#68972=CARTESIAN_POINT('Ctrl Pts',(-0.181214866084196,-0.551016628517353,
1.89496927408592E-15));
#68973=CARTESIAN_POINT('Ctrl Pts',(-0.15395161752934,-0.560992522191175,
1.26027660529715E-15));
#68974=CARTESIAN_POINT('Ctrl Pts',(-0.126481843682384,-0.571043985522471,
6.20775995570898E-16));
#68975=CARTESIAN_POINT('Ctrl Pts',(-0.0982638372323879,-0.5790405373196,
-4.73556415712161E-16));
#68976=CARTESIAN_POINT('Ctrl Pts',(-0.0695277070223783,-0.584888355781468,
-1.35763796038635E-15));
#68977=CARTESIAN_POINT('Ctrl Pts',(-0.0588916184022295,-0.587052805724463,
-1.68486259320477E-15));
#68978=CARTESIAN_POINT('Ctrl Pts',(-0.04818434176478,-0.58892242285403,
2.76336445804202E-17));
#68979=CARTESIAN_POINT('Ctrl Pts',(-0.0374170035146651,-0.590490705661811,
0.));
#68980=CARTESIAN_POINT('Ctrl Pts',(-0.0374170035146651,-0.590490705661811,
0.));
#68981=CARTESIAN_POINT('Ctrl Pts',(-0.135716027844311,-0.584261894770184,
-0.00463654331525316));
#68982=CARTESIAN_POINT('Ctrl Pts',(-0.23237971190286,-0.553015871596231,
-0.00927308663050638));
#68983=CARTESIAN_POINT('Ctrl Pts',(-0.315661655680501,-0.500499137650197,
-0.0139096299457595));
#68984=CARTESIAN_POINT('Ctrl Pts',(-0.398943599458139,-0.447982403704166,
-0.0185461732610124));
#68985=CARTESIAN_POINT('Ctrl Pts',(-0.468843802954871,-0.374194958986059,
-0.0231827165762653));
#68986=CARTESIAN_POINT('Ctrl Pts',(-0.516804481271218,-0.288189149275334,
-0.0278192598915181));
#68987=CARTESIAN_POINT('Ctrl Pts',(-0.564765159587562,-0.202183339564614,
-0.0324558032067708));
#68988=CARTESIAN_POINT('Ctrl Pts',(-0.590786312723525,-0.103959164861278,
-0.0370923465220234));
#68989=CARTESIAN_POINT('Ctrl Pts',(-0.591699434208916,-0.00549578503077282,
-0.041728889837276));
#68990=CARTESIAN_POINT('Ctrl Pts',(-0.591716409854293,-0.00366527348840485,
-0.0418150868180202));
#68991=CARTESIAN_POINT('Ctrl Pts',(-0.591724707729724,-0.0018346792726083,
-0.0419012837987644));
#68992=CARTESIAN_POINT('Ctrl Pts',(-0.591724346791278,-4.07989592221547E-6,
-0.0419874807795086));
#68993=CARTESIAN_POINT('Origin',(0.,0.,0.682383483348824));
#68994=CARTESIAN_POINT('',(0.9,-0.519615242270664,0.64363448015713));
#68995=CARTESIAN_POINT('',(-1.90903542970483E-16,-1.03923048454133,0.64363448015713));
#68996=CARTESIAN_POINT('Ctrl Pts',(0.9,-0.519615242270664,0.64363448015713));
#68997=CARTESIAN_POINT('Ctrl Pts',(0.45,-0.779422863405995,0.79363448015713));
#68998=CARTESIAN_POINT('Ctrl Pts',(-1.90903542970483E-16,-1.03923048454133,
0.64363448015713));
#68999=CARTESIAN_POINT('',(0.9,0.519615242270663,0.64363448015713));
#69000=CARTESIAN_POINT('Ctrl Pts',(0.9,0.519615242270663,0.64363448015713));
#69001=CARTESIAN_POINT('Ctrl Pts',(0.9,-2.22044604925031E-16,0.79363448015713));
#69002=CARTESIAN_POINT('Ctrl Pts',(0.9,-0.519615242270664,0.64363448015713));
#69003=CARTESIAN_POINT('',(6.36345143234944E-17,1.03923048454133,0.64363448015713));
#69004=CARTESIAN_POINT('Ctrl Pts',(6.36345143234944E-17,1.03923048454133,
0.64363448015713));
#69005=CARTESIAN_POINT('Ctrl Pts',(0.45,0.779422863405995,0.79363448015713));
#69006=CARTESIAN_POINT('Ctrl Pts',(0.9,0.519615242270663,0.64363448015713));
#69007=CARTESIAN_POINT('',(-0.9,0.519615242270663,0.64363448015713));
#69008=CARTESIAN_POINT('Ctrl Pts',(-0.9,0.519615242270663,0.64363448015713));
#69009=CARTESIAN_POINT('Ctrl Pts',(-0.45,0.779422863405995,0.79363448015713));
#69010=CARTESIAN_POINT('Ctrl Pts',(6.36345143234944E-17,1.03923048454133,
0.64363448015713));
#69011=CARTESIAN_POINT('',(-0.9,-8.02243635933536E-17,0.724019237886466));
#69012=CARTESIAN_POINT('Ctrl Pts',(-0.9,-5.02305152634454E-17,0.724019237886467));
#69013=CARTESIAN_POINT('Ctrl Pts',(-0.9,0.24115427318801,0.724019237886467));
#69014=CARTESIAN_POINT('Ctrl Pts',(-0.9,0.519615242270663,0.64363448015713));
#69015=CARTESIAN_POINT('',(-0.855,-1.04707301327099E-16,0.75));
#69016=CARTESIAN_POINT('',(-0.972115242270663,-1.19049781984912E-16,0.682383483348824));
#69017=CARTESIAN_POINT('Origin',(0.,0.,0.75));
#69018=CARTESIAN_POINT('',(-0.9,-0.519615242270663,0.64363448015713));
#69019=CARTESIAN_POINT('Ctrl Pts',(-0.9,-0.519615242270663,0.64363448015713));
#69020=CARTESIAN_POINT('Ctrl Pts',(-0.9,-0.24115427318801,0.724019237886466));
#69021=CARTESIAN_POINT('Ctrl Pts',(-0.9,-5.02305152634454E-17,0.724019237886467));
#69022=CARTESIAN_POINT('Ctrl Pts',(-1.90903542970483E-16,-1.03923048454133,
0.64363448015713));
#69023=CARTESIAN_POINT('Ctrl Pts',(-0.45,-0.779422863405995,0.79363448015713));
#69024=CARTESIAN_POINT('Ctrl Pts',(-0.9,-0.519615242270663,0.64363448015713));
#69025=CARTESIAN_POINT('Origin',(6.36345143234944E-17,1.03923048454133,
0.05));
#69026=CARTESIAN_POINT('',(6.36345143234944E-17,1.03923048454133,0.05));
#69027=CARTESIAN_POINT('',(6.36345143234944E-17,1.03923048454133,0.05));
#69028=CARTESIAN_POINT('',(-0.9,0.519615242270663,0.05));
#69029=CARTESIAN_POINT('',(6.36345143234944E-17,1.03923048454133,0.05));
#69030=CARTESIAN_POINT('',(-0.9,0.519615242270663,0.05));
#69031=CARTESIAN_POINT('Origin',(0.9,0.519615242270663,0.05));
#69032=CARTESIAN_POINT('',(0.9,0.519615242270663,0.05));
#69033=CARTESIAN_POINT('',(0.9,0.519615242270663,0.05));
#69034=CARTESIAN_POINT('',(0.9,0.519615242270663,0.05));
#69035=CARTESIAN_POINT('Origin',(0.9,-0.519615242270664,0.05));
#69036=CARTESIAN_POINT('',(0.9,-0.519615242270664,0.05));
#69037=CARTESIAN_POINT('',(0.9,-0.519615242270664,0.05));
#69038=CARTESIAN_POINT('',(0.9,-0.519615242270664,0.05));
#69039=CARTESIAN_POINT('Origin',(0.,0.,0.05));
#69040=CARTESIAN_POINT('',(-1.90903542970483E-16,-1.03923048454133,0.05));
#69041=CARTESIAN_POINT('',(-1.90903542970483E-16,-1.03923048454133,0.05));
#69042=CARTESIAN_POINT('',(-0.9,-0.519615242270663,0.05));
#69043=CARTESIAN_POINT('',(-0.9,-0.519615242270663,0.05));
#69044=CARTESIAN_POINT('',(-0.9,0.519615242270663,0.05));
#69045=CARTESIAN_POINT('',(-0.83,-1.0164568432923E-16,0.05));
#69046=CARTESIAN_POINT('Origin',(0.,0.,0.05));
#69047=CARTESIAN_POINT('Origin',(-1.90903542970483E-16,-1.03923048454133,
0.05));
#69048=CARTESIAN_POINT('',(-1.90903542970483E-16,-1.03923048454133,0.05));
#69049=CARTESIAN_POINT('Origin',(-0.9,-0.519615242270663,0.05));
#69050=CARTESIAN_POINT('',(-0.9,-0.519615242270663,0.05));
#69051=CARTESIAN_POINT('Origin',(-0.9,0.519615242270663,0.05));
#69052=CARTESIAN_POINT('Origin',(0.,0.,0.75));
#69053=CARTESIAN_POINT('Origin',(0.54,0.,-4.));
#69054=CARTESIAN_POINT('',(-0.54,-6.61309271539571E-17,-4.));
#69055=CARTESIAN_POINT('Origin',(0.,0.,-4.));
#69056=CARTESIAN_POINT('Origin',(0.,0.,-3.97));
#69057=CARTESIAN_POINT('',(-0.57,-6.98048675513991E-17,-3.97));
#69058=CARTESIAN_POINT('Origin',(0.,0.,-1.97));
#69059=CARTESIAN_POINT('Origin',(0.,0.,0.));
#69060=CARTESIAN_POINT('Origin',(0.83,0.,0.));
#69061=CARTESIAN_POINT('',(-0.83,-1.0164568432923E-16,0.));
#69062=CARTESIAN_POINT('Origin',(0.,0.,0.));
#69063=CARTESIAN_POINT('Origin',(0.,0.,0.025));
#69064=CARTESIAN_POINT('',(-0.83,-1.0164568432923E-16,0.025));
#69065=CARTESIAN_POINT('',(0.,0.,0.));
#69066=CARTESIAN_POINT('Origin',(0.,0.,-1.725));
#69067=CARTESIAN_POINT('',(-0.493073791100261,0.0002448543660152,-3.40911584740964));
#69068=CARTESIAN_POINT('',(-0.492742936816498,0.00014446300365779,-3.43088415259036));
#69069=CARTESIAN_POINT('',(-0.4925,-6.03138548580071E-17,-1.725));
#69070=CARTESIAN_POINT('',(0.217167145730328,0.442422208592295,-3.4575));
#69071=CARTESIAN_POINT('Ctrl Pts',(-0.493073791100261,0.0002448543660152,
-3.40911584740964));
#69072=CARTESIAN_POINT('Ctrl Pts',(-0.493182091264478,0.0161839881931373,
-3.40989118236287));
#69073=CARTESIAN_POINT('Ctrl Pts',(-0.492479030563148,0.0321141508308048,
-3.41066651731609));
#69074=CARTESIAN_POINT('Ctrl Pts',(-0.490933795885643,0.0479625955988295,
-3.41144185226931));
#69075=CARTESIAN_POINT('Ctrl Pts',(-0.475090734441219,0.21045434388385,
-3.41939124628873));
#69076=CARTESIAN_POINT('Ctrl Pts',(-0.370717535510866,0.364355831202377,
-3.42734064030814));
#69077=CARTESIAN_POINT('Ctrl Pts',(-0.225430438464366,0.438880232373327,
-3.43529003432755));
#69078=CARTESIAN_POINT('Ctrl Pts',(-0.0901236284872688,0.508285287556358,
-3.44269335621837));
#69079=CARTESIAN_POINT('Ctrl Pts',(0.0806691021356228,0.508844079982147,
-3.45009667810918));
#69080=CARTESIAN_POINT('Ctrl Pts',(0.217494704229605,0.442648936192906,
-3.4575));
#69081=CARTESIAN_POINT('',(-0.21683958723106,0.44219548099168,-3.4575));
#69082=CARTESIAN_POINT('Origin',(0.,0.,-3.4575));
#69083=CARTESIAN_POINT('Ctrl Pts',(-0.216839587231058,0.442195480991681,
-3.4575));
#69084=CARTESIAN_POINT('Ctrl Pts',(-0.290461473000918,0.406093485363624,
-3.45352530299029));
#69085=CARTESIAN_POINT('Ctrl Pts',(-0.354334152100823,0.351257047124773,
-3.44955060598059));
#69086=CARTESIAN_POINT('Ctrl Pts',(-0.401848390604011,0.284326789074269,
-3.44557590897088));
#69087=CARTESIAN_POINT('Ctrl Pts',(-0.449362629107199,0.217396531023764,
-3.44160121196118));
#69088=CARTESIAN_POINT('Ctrl Pts',(-0.480518427013668,0.138372453161606,
-3.43762651495147));
#69089=CARTESIAN_POINT('Ctrl Pts',(-0.489782485247723,0.0570344034865685,
-3.43365181794177));
#69090=CARTESIAN_POINT('Ctrl Pts',(-0.491932738287992,0.0381552703696876,
-3.43272926282463));
#69091=CARTESIAN_POINT('Ctrl Pts',(-0.492903602897926,0.019151475091413,
-3.4318067077075));
#69092=CARTESIAN_POINT('Ctrl Pts',(-0.492742936816498,0.00014446300365779,
-3.43088415259036));
#69093=CARTESIAN_POINT('Origin',(0.,0.,-1.725));
#69094=CARTESIAN_POINT('',(-0.491853744940756,0.000283605033675694,-3.25911584740964));
#69095=CARTESIAN_POINT('',(-0.491800415587683,0.00023852271259368,-3.28088415259036));
#69096=CARTESIAN_POINT('',(-0.4925,-6.03138548580071E-17,-1.725));
#69097=CARTESIAN_POINT('Ctrl Pts',(-0.491853744940756,0.000283605033675694,
-3.25911584740964));
#69098=CARTESIAN_POINT('Ctrl Pts',(-0.492187195010901,0.0639943662937747,
-3.2621948182464));
#69099=CARTESIAN_POINT('Ctrl Pts',(-0.480703508315908,0.127589580024711,
-3.26527378908315));
#69100=CARTESIAN_POINT('Ctrl Pts',(-0.456846036553436,0.186143136808157,
-3.26835275991991));
#69101=CARTESIAN_POINT('Ctrl Pts',(-0.395249985989105,0.337318746707772,
-3.27630215393932));
#69102=CARTESIAN_POINT('Ctrl Pts',(-0.251171881922387,0.454887322396288,
-3.28425154795873));
#69103=CARTESIAN_POINT('Ctrl Pts',(-0.0907115246557711,0.4849032574776,
-3.29220094197814));
#69104=CARTESIAN_POINT('Ctrl Pts',(0.0697488326108451,0.514919192558913,
-3.30015033599755));
#69105=CARTESIAN_POINT('Ctrl Pts',(0.246591443077359,0.457382487033021,
-3.30809973001697));
#69106=CARTESIAN_POINT('Ctrl Pts',(0.358668040949174,0.338698380513017,
-3.31604912403638));
#69107=CARTESIAN_POINT('Ctrl Pts',(0.470744638820989,0.220014273993013,
-3.32399851805579));
#69108=CARTESIAN_POINT('Ctrl Pts',(0.518055224098106,0.0401827664788985,
-3.3319479120752));
#69109=CARTESIAN_POINT('Ctrl Pts',(0.478912723457106,-0.118299377058885,
-3.33989730609461));
#69110=CARTESIAN_POINT('Ctrl Pts',(0.439770222816105,-0.276781520596668,
-3.34784670011402));
#69111=CARTESIAN_POINT('Ctrl Pts',(0.314174636256986,-0.41391430015812,
-3.35579609413343));
#69112=CARTESIAN_POINT('Ctrl Pts',(0.159713217153272,-0.46675503851712,
-3.36374548815285));
#69113=CARTESIAN_POINT('Ctrl Pts',(0.00525179804955778,-0.519595776876121,
-3.37169488217226));
#69114=CARTESIAN_POINT('Ctrl Pts',(-0.178075453598752,-0.488144474032672,
-3.37964427619167));
#69115=CARTESIAN_POINT('Ctrl Pts',(-0.306082617443658,-0.386877817985189,
-3.38759367021108));
#69116=CARTESIAN_POINT('Ctrl Pts',(-0.421604750586888,-0.295488088133343,
-3.39476772927727));
#69117=CARTESIAN_POINT('Ctrl Pts',(-0.49207170577992,-0.147237581533594,
-3.40194178834345));
#69118=CARTESIAN_POINT('Ctrl Pts',(-0.493073791100261,0.0002448543660152,
-3.40911584740964));
#69119=CARTESIAN_POINT('Ctrl Pts',(-0.492742936816498,0.00014446300365779,
-3.43088415259036));
#69120=CARTESIAN_POINT('Ctrl Pts',(-0.491519189150602,-0.144626520836325,
-3.42385731368808));
#69121=CARTESIAN_POINT('Ctrl Pts',(-0.424650436153211,-0.289584125752622,
-3.41683047478581));
#69122=CARTESIAN_POINT('Ctrl Pts',(-0.313283991213996,-0.3810642428305,
-3.40980363588353));
#69123=CARTESIAN_POINT('Ctrl Pts',(-0.187296222933706,-0.484554803195898,
-3.40185424186412));
#69124=CARTESIAN_POINT('Ctrl Pts',(-0.0043595285946734,-0.5196039373251,
-3.39390484784471));
#69125=CARTESIAN_POINT('Ctrl Pts',(0.151107539993508,-0.469682036256402,
-3.3859554538253));
#69126=CARTESIAN_POINT('Ctrl Pts',(0.30657460858169,-0.419760135187704,
-3.37800605980589));
#69127=CARTESIAN_POINT('Ctrl Pts',(0.43457205141902,-0.284867198921108,
-3.37005666578647));
#69128=CARTESIAN_POINT('Ctrl Pts',(0.47661233007598,-0.12711047662137,-3.36210727176706));
#69129=CARTESIAN_POINT('Ctrl Pts',(0.518652608732941,0.0306462456783684,
-3.35415787774765));
#69130=CARTESIAN_POINT('Ctrl Pts',(0.474735723209532,0.211266754011248,
-3.34620848372824));
#69131=CARTESIAN_POINT('Ctrl Pts',(0.364887977701248,0.331990579512092,
-3.33825908970883));
#69132=CARTESIAN_POINT('Ctrl Pts',(0.255040232192964,0.452714405012937,
-3.33030969568942));
#69133=CARTESIAN_POINT('Ctrl Pts',(0.0792616266998056,0.513541547681747,
-3.32236030167));
#69134=CARTESIAN_POINT('Ctrl Pts',(-0.0817338726622884,0.48650604301746,
-3.31441090765059));
#69135=CARTESIAN_POINT('Ctrl Pts',(-0.242729372024383,0.459470538353173,
-3.30646151363118));
#69136=CARTESIAN_POINT('Ctrl Pts',(-0.388941765255412,0.344572386355788,
-3.29851211961177));
#69137=CARTESIAN_POINT('Ctrl Pts',(-0.453320072358766,0.194558532483742,
-3.29056272559236));
#69138=CARTESIAN_POINT('Ctrl Pts',(-0.479447436848157,0.13367674147484,
-3.28733653459169));
#69139=CARTESIAN_POINT('Ctrl Pts',(-0.492096153073964,0.0670111479394572,
-3.28411034359102));
#69140=CARTESIAN_POINT('Ctrl Pts',(-0.491800415587683,0.00023852271259368,
-3.28088415259036));
#69141=CARTESIAN_POINT('Origin',(0.,0.,-1.725));
#69142=CARTESIAN_POINT('',(-0.492081943586782,-0.000397447809200757,-3.10911584740964));
#69143=CARTESIAN_POINT('',(-0.492160810488226,-0.000419635530953083,-3.13088415259036));
#69144=CARTESIAN_POINT('',(-0.4925,-6.03138548580071E-17,-1.725));
#69145=CARTESIAN_POINT('Ctrl Pts',(-0.492081943586782,-0.000397447809200757,
-3.10911584740964));
#69146=CARTESIAN_POINT('Ctrl Pts',(-0.491241598635805,0.110851625858574,
-3.11449845412993));
#69147=CARTESIAN_POINT('Ctrl Pts',(-0.453894375407504,0.222611533621158,
-3.11988106085021));
#69148=CARTESIAN_POINT('Ctrl Pts',(-0.38470206106664,0.308808692434093,
-3.1252636675705));
#69149=CARTESIAN_POINT('Ctrl Pts',(-0.282514218187923,0.436110428259485,
-3.13321306158991));
#69150=CARTESIAN_POINT('Ctrl Pts',(-0.110867900179577,0.507656331705935,
-3.14116245560932));
#69151=CARTESIAN_POINT('Ctrl Pts',(0.0514831441757647,0.490620021386414,
-3.14911184962873));
#69152=CARTESIAN_POINT('Ctrl Pts',(0.213834188531107,0.473583711066893,
-3.15706124364815));
#69153=CARTESIAN_POINT('Ctrl Pts',(0.366889959233445,0.3679651869814,-3.16501063766755));
#69154=CARTESIAN_POINT('Ctrl Pts',(0.44042601136825,0.222223912935534,-3.17296003168697));
#69155=CARTESIAN_POINT('Ctrl Pts',(0.513962063503055,0.0764826388896689,
-3.18090942570638));
#69156=CARTESIAN_POINT('Ctrl Pts',(0.507978397070326,-0.109381385116569,
-3.18885881972579));
#69157=CARTESIAN_POINT('Ctrl Pts',(0.425220800855701,-0.250091262149485,
-3.1968082137452));
#69158=CARTESIAN_POINT('Ctrl Pts',(0.342463204641076,-0.390801139182402,
-3.20475760776462));
#69159=CARTESIAN_POINT('Ctrl Pts',(0.182931678644556,-0.486356869241995,
-3.21270700178403));
#69160=CARTESIAN_POINT('Ctrl Pts',(0.0198208766646809,-0.492915594607009,
-3.22065639580344));
#69161=CARTESIAN_POINT('Ctrl Pts',(-0.143289925315194,-0.499474319972023,
-3.22860578982285));
#69162=CARTESIAN_POINT('Ctrl Pts',(-0.309980003278424,-0.417036040642455,
-3.23655518384226));
#69163=CARTESIAN_POINT('Ctrl Pts',(-0.403768043729067,-0.283425578922314,
-3.24450457786167));
#69164=CARTESIAN_POINT('Ctrl Pts',(-0.461229964141025,-0.201565315282324,
-3.24937500104433));
#69165=CARTESIAN_POINT('Ctrl Pts',(-0.491326282019541,-0.100496293535574,
-3.25424542422699));
#69166=CARTESIAN_POINT('Ctrl Pts',(-0.491853744940756,0.000283605033675694,
-3.25911584740964));
#69167=CARTESIAN_POINT('Ctrl Pts',(-0.491800415587683,0.00023852271259368,
-3.28088415259036));
#69168=CARTESIAN_POINT('Ctrl Pts',(-0.491367450463277,-0.0975178298951643,
-3.27616094957161));
#69169=CARTESIAN_POINT('Ctrl Pts',(-0.463189991711903,-0.195503588868632,
-3.27143774655287));
#69170=CARTESIAN_POINT('Ctrl Pts',(-0.40894429040333,-0.27590559389322,
-3.26671454353412));
#69171=CARTESIAN_POINT('Ctrl Pts',(-0.317645980368864,-0.411226310651424,
-3.25876514951471));
#69172=CARTESIAN_POINT('Ctrl Pts',(-0.152505139324254,-0.496738188421124,
-3.2508157554953));
#69173=CARTESIAN_POINT('Ctrl Pts',(0.0107001108864536,-0.493198978205245,
-3.24286636147589));
#69174=CARTESIAN_POINT('Ctrl Pts',(0.17390536109716,-0.489659767989366,
-3.23491696745648));
#69175=CARTESIAN_POINT('Ctrl Pts',(0.335175020473964,-0.397069469787909,
-3.22696757343707));
#69176=CARTESIAN_POINT('Ctrl Pts',(0.4205209257937,-0.257914117387704,-3.21901817941765));
#69177=CARTESIAN_POINT('Ctrl Pts',(0.505866831113436,-0.118758764987498,
-3.21106878539824));
#69178=CARTESIAN_POINT('Ctrl Pts',(0.515288982376103,0.0669616416114556,
-3.20311939137883));
#69179=CARTESIAN_POINT('Ctrl Pts',(0.444461893468698,0.2140380586944,-3.19516999735942));
#69180=CARTESIAN_POINT('Ctrl Pts',(0.373634804561292,0.361114475777343,
-3.18722060334001));
#69181=CARTESIAN_POINT('Ctrl Pts',(0.222558475483815,0.469546903344277,
-3.1792712093206));
#69182=CARTESIAN_POINT('Ctrl Pts',(0.0605502329573067,0.489583796109161,
-3.17132181530119));
#69183=CARTESIAN_POINT('Ctrl Pts',(-0.101458009569203,0.509620688874046,
-3.16337242128177));
#69184=CARTESIAN_POINT('Ctrl Pts',(-0.274398165544743,0.441262046836879,
-3.15542302726236));
#69185=CARTESIAN_POINT('Ctrl Pts',(-0.378923416489071,0.315872421142784,
-3.14747363324295));
#69186=CARTESIAN_POINT('Ctrl Pts',(-0.451634184295762,0.228647794778889,
-3.14194380635875));
#69187=CARTESIAN_POINT('Ctrl Pts',(-0.491239025177775,0.113825913452389,
-3.13641397947456));
#69188=CARTESIAN_POINT('Ctrl Pts',(-0.492160810488226,-0.000419635530953083,
-3.13088415259036));
#69189=CARTESIAN_POINT('Origin',(0.,0.,-1.725));
#69190=CARTESIAN_POINT('',(-0.493288832552248,-0.000100558029926257,-2.95911584740964));
#69191=CARTESIAN_POINT('',(-0.493308766107567,-4.46620548418582E-5,-2.98088415259036));
#69192=CARTESIAN_POINT('',(-0.4925,-6.03138548580071E-17,-1.725));
#69193=CARTESIAN_POINT('Ctrl Pts',(-0.493288832552248,-0.000100558029926257,
-2.95911584740964));
#69194=CARTESIAN_POINT('Ctrl Pts',(-0.492849426102292,0.15775946830591,
-2.96680209001346));
#69195=CARTESIAN_POINT('Ctrl Pts',(-0.410373732182605,0.316014099494504,
-2.97448833261728));
#69196=CARTESIAN_POINT('Ctrl Pts',(-0.280543525334876,0.405775594702927,
-2.98217457522109));
#69197=CARTESIAN_POINT('Ctrl Pts',(-0.146268363457757,0.498610225349239,
-2.9901239692405));
#69198=CARTESIAN_POINT('Ctrl Pts',(0.0386593403997117,0.518181480847482,
-2.99807336325992));
#69199=CARTESIAN_POINT('Ctrl Pts',(0.18939203724908,0.455509779881214,-3.00602275727933));
#69200=CARTESIAN_POINT('Ctrl Pts',(0.34012473409845,0.392838078914945,-3.01397215129874));
#69201=CARTESIAN_POINT('Ctrl Pts',(0.45666242393972,0.247923421484165,-3.02192154531815));
#69202=CARTESIAN_POINT('Ctrl Pts',(0.485535896090777,0.0872547869843185,
-3.02987093933756));
#69203=CARTESIAN_POINT('Ctrl Pts',(0.514409368241833,-0.0734138475155269,
-3.03782033335697));
#69204=CARTESIAN_POINT('Ctrl Pts',(0.455618622702678,-0.249836459084439,
-3.04576972737638));
#69205=CARTESIAN_POINT('Ctrl Pts',(0.336137726335389,-0.361067763092586,
-3.0537191213958));
#69206=CARTESIAN_POINT('Ctrl Pts',(0.216656829968098,-0.472299067100733,
-3.06166851541521));
#69207=CARTESIAN_POINT('Ctrl Pts',(0.0364857827726722,-0.518339063548116,
-3.06961790943462));
#69208=CARTESIAN_POINT('Ctrl Pts',(-0.121710303328504,-0.47806391507255,
-3.07756730345403));
#69209=CARTESIAN_POINT('Ctrl Pts',(-0.279906389429679,-0.437788766596985,
-3.08551669747344));
#69210=CARTESIAN_POINT('Ctrl Pts',(-0.416127514436606,-0.311198473198473,
-3.09346609149285));
#69211=CARTESIAN_POINT('Ctrl Pts',(-0.467873393065525,-0.156374542397051,
-3.10141548551226));
#69212=CARTESIAN_POINT('Ctrl Pts',(-0.484581668403554,-0.106383298006425,
-3.10398227281139));
#69213=CARTESIAN_POINT('Ctrl Pts',(-0.49248267632821,-0.0534484552799383,
-3.10654906011052));
#69214=CARTESIAN_POINT('Ctrl Pts',(-0.492081943586782,-0.000397447809200757,
-3.10911584740964));
#69215=CARTESIAN_POINT('Ctrl Pts',(-0.492160810488226,-0.000419635530953083,
-3.13088415259036));
#69216=CARTESIAN_POINT('Ctrl Pts',(-0.492564136214256,-0.0504075974425025,
-3.12846458545514));
#69217=CARTESIAN_POINT('Ctrl Pts',(-0.485561643610284,-0.100285221311515,
-3.12604501831993));
#69218=CARTESIAN_POINT('Ctrl Pts',(-0.47068614746544,-0.147692460569256,
-3.12362545118472));
#69219=CARTESIAN_POINT('Ctrl Pts',(-0.421813281584368,-0.303447107236178,
-3.1156760571653));
#69220=CARTESIAN_POINT('Ctrl Pts',(-0.287957203909111,-0.432535791218999,
-3.10772666314589));
#69221=CARTESIAN_POINT('Ctrl Pts',(-0.130533233909336,-0.475730562101413,
-3.09977726912648));
#69222=CARTESIAN_POINT('Ctrl Pts',(0.0268907360904382,-0.518925332983827,
-3.09182787510707));
#69223=CARTESIAN_POINT('Ctrl Pts',(0.207882598414731,-0.476226190765834,
-3.08387848108766));
#69224=CARTESIAN_POINT('Ctrl Pts',(0.329400718662921,-0.367224215067139,
-3.07592908706825));
#69225=CARTESIAN_POINT('Ctrl Pts',(0.450918838911112,-0.258222239368444,
-3.06797969304883));
#69226=CARTESIAN_POINT('Ctrl Pts',(0.512963217083201,-0.082917430189047,
-3.06003029902942));
#69227=CARTESIAN_POINT('Ctrl Pts',(0.487066930325681,0.0782578312794736,
-3.05208090501001));
#69228=CARTESIAN_POINT('Ctrl Pts',(0.461170643568161,0.239433092747993,
-3.0441315109906));
#69229=CARTESIAN_POINT('Ctrl Pts',(0.347333691881035,0.386478806505637,
-3.03618211697119));
#69230=CARTESIAN_POINT('Ctrl Pts',(0.197786169162767,0.451928212703762,
-3.02823272295178));
#69231=CARTESIAN_POINT('Ctrl Pts',(0.0482386464444978,0.517377618901888,
-3.02028332893236));
#69232=CARTESIAN_POINT('Ctrl Pts',(-0.137019447304913,0.501230717540495,
-3.01233393491295));
#69233=CARTESIAN_POINT('Ctrl Pts',(-0.272988986618268,0.410895956542165,
-3.00438454089354));
#69234=CARTESIAN_POINT('Ctrl Pts',(-0.406975592535066,0.321878606894628,
-2.99655107812582));
#69235=CARTESIAN_POINT('Ctrl Pts',(-0.493100776114359,0.160821480000113,
-2.98871761535809));
#69236=CARTESIAN_POINT('Ctrl Pts',(-0.493308766107567,-4.46620548418582E-5,
-2.98088415259036));
#69237=CARTESIAN_POINT('Origin',(0.,0.,-1.725));
#69238=CARTESIAN_POINT('',(-0.49238332947362,0.000451585811006003,-2.80911584740964));
#69239=CARTESIAN_POINT('',(-0.492294212910438,0.000443650235898252,-2.83088415259036));
#69240=CARTESIAN_POINT('',(-0.4925,-6.03138548580071E-17,-1.725));
#69241=CARTESIAN_POINT('Ctrl Pts',(-0.49238332947362,0.000451585811006003,
-2.80911584740964));
#69242=CARTESIAN_POINT('Ctrl Pts',(-0.492762312673717,0.0425594796056222,
-2.81115633187758));
#69243=CARTESIAN_POINT('Ctrl Pts',(-0.487812004432201,0.0845796032291862,
-2.81319681634551));
#69244=CARTESIAN_POINT('Ctrl Pts',(-0.477185120477568,0.125111406407132,
-2.81523730081345));
#69245=CARTESIAN_POINT('Ctrl Pts',(-0.435784517296601,0.283016687648826,
-2.82318669483286));
#69246=CARTESIAN_POINT('Ctrl Pts',(-0.30822744433155,0.418332921904744,
-2.83113608885227));
#69247=CARTESIAN_POINT('Ctrl Pts',(-0.153038963263602,0.468975030179542,
-2.83908548287168));
#69248=CARTESIAN_POINT('Ctrl Pts',(0.00214951780434441,0.519617138454339,
-2.84703487689109));
#69249=CARTESIAN_POINT('Ctrl Pts',(0.184969406975187,0.485585120748017,
-2.85498427091051));
#69250=CARTESIAN_POINT('Ctrl Pts',(0.311540249547337,0.382493367425997,
-2.86293366492992));
#69251=CARTESIAN_POINT('Ctrl Pts',(0.438111092119489,0.279401614103976,
-2.87088305894933));
#69252=CARTESIAN_POINT('Ctrl Pts',(0.508432888092948,0.107250125166256,
-2.87883245296874));
#69253=CARTESIAN_POINT('Ctrl Pts',(0.490240962838993,-0.0549754635675121,
-2.88678184698815));
#69254=CARTESIAN_POINT('Ctrl Pts',(0.472049037585039,-0.217201052301277,
-2.89473124100757));
#69255=CARTESIAN_POINT('Ctrl Pts',(0.365343391103676,-0.369500740831089,
-2.90268063502698));
#69256=CARTESIAN_POINT('Ctrl Pts',(0.219082143980931,-0.441997191571637,
-2.91063002904639));
#69257=CARTESIAN_POINT('Ctrl Pts',(0.0728208968581848,-0.514493642312186,
-2.9185794230658));
#69258=CARTESIAN_POINT('Ctrl Pts',(-0.112995950905944,-0.507186855263467,
-2.92652881708521));
#69259=CARTESIAN_POINT('Ctrl Pts',(-0.253112896177252,-0.423429291625341,
-2.93447821110462));
#69260=CARTESIAN_POINT('Ctrl Pts',(-0.39322984144856,-0.339671727987215,
-2.94242760512403));
#69261=CARTESIAN_POINT('Ctrl Pts',(-0.487646884227047,-0.179463387759685,
-2.95037699914345));
#69262=CARTESIAN_POINT('Ctrl Pts',(-0.493044095667907,-0.0163102147487279,
-2.95832639316286));
#69263=CARTESIAN_POINT('Ctrl Pts',(-0.493222761340719,-0.0109093013795094,
-2.95858954457845));
#69264=CARTESIAN_POINT('Ctrl Pts',(-0.493303876369531,-0.00550516097278517,
-2.95885269599405));
#69265=CARTESIAN_POINT('Ctrl Pts',(-0.493288832552248,-0.000100558029926257,
-2.95911584740964));
#69266=CARTESIAN_POINT('Ctrl Pts',(-0.493308766107567,-4.46620548418582E-5,
-2.98088415259036));
#69267=CARTESIAN_POINT('Ctrl Pts',(-0.493311844253333,-0.00242539887009011,
-2.98076822133867));
#69268=CARTESIAN_POINT('Ctrl Pts',(-0.493296104394717,-0.00480609385490379,
-2.98065229008699));
#69269=CARTESIAN_POINT('Ctrl Pts',(-0.493261423175586,-0.0071865128763955,
-2.98053635883531));
#69270=CARTESIAN_POINT('Ctrl Pts',(-0.490883335542247,-0.170411600661355,
-2.97258696481589));
#69271=CARTESIAN_POINT('Ctrl Pts',(-0.399446175398269,-0.332339155596008,
-2.96463757079648));
#69272=CARTESIAN_POINT('Ctrl Pts',(-0.26090266065602,-0.418674429978304,
-2.95668817677707));
#69273=CARTESIAN_POINT('Ctrl Pts',(-0.12235914591377,-0.505009704360601,
-2.94873878275766));
#69274=CARTESIAN_POINT('Ctrl Pts',(0.0632907234267497,-0.515752698190541,
-2.94078938873825));
#69275=CARTESIAN_POINT('Ctrl Pts',(0.210868057983077,-0.445974369553748,
-2.93283999471884));
#69276=CARTESIAN_POINT('Ctrl Pts',(0.358445392539404,-0.376196040916956,
-2.92489060069943));
#69277=CARTESIAN_POINT('Ctrl Pts',(0.467950192311538,-0.225896389813431,
-2.91694120668002));
#69278=CARTESIAN_POINT('Ctrl Pts',(0.489140043172359,-0.064035106446827,
-2.9089918126606));
#69279=CARTESIAN_POINT('Ctrl Pts',(0.51032989403318,0.0978261769197771,
-2.90104241864119));
#69280=CARTESIAN_POINT('Ctrl Pts',(0.443204795982688,0.27124909254946,-2.89309302462178));
#69281=CARTESIAN_POINT('Ctrl Pts',(0.318562732046716,0.376664654941548,
-2.88514363060237));
#69282=CARTESIAN_POINT('Ctrl Pts',(0.193920668110745,0.482080217333636,
-2.87719423658296));
#69283=CARTESIAN_POINT('Ctrl Pts',(0.0117616382892947,0.51948842648813,
-2.86924484256355));
#69284=CARTESIAN_POINT('Ctrl Pts',(-0.14433711493361,0.471725845947257,
-2.86129544854414));
#69285=CARTESIAN_POINT('Ctrl Pts',(-0.300435868156515,0.423963265406384,
-2.85334605452472));
#69286=CARTESIAN_POINT('Ctrl Pts',(-0.430474344780874,0.291029895170145,
-2.84539666050531));
#69287=CARTESIAN_POINT('Ctrl Pts',(-0.474788978503301,0.133917521054328,
-2.8374472664859));
#69288=CARTESIAN_POINT('Ctrl Pts',(-0.486984540733128,0.0906795751512453,
-2.83525956185405));
#69289=CARTESIAN_POINT('Ctrl Pts',(-0.492687617934248,0.0456103788587369,
-2.8330718572222));
#69290=CARTESIAN_POINT('Ctrl Pts',(-0.492294212910438,0.000443650235898252,
-2.83088415259036));
#69291=CARTESIAN_POINT('Origin',(0.,0.,-1.725));
#69292=CARTESIAN_POINT('',(-0.491717171688544,-0.000124746059964487,-2.65911584740964));
#69293=CARTESIAN_POINT('',(-0.491744581231444,-0.000172364191907249,-2.68088415259036));
#69294=CARTESIAN_POINT('',(-0.4925,-6.03138548580071E-17,-1.725));
#69295=CARTESIAN_POINT('Ctrl Pts',(-0.491717171688544,-0.000124746059964487,
-2.65911584740964));
#69296=CARTESIAN_POINT('Ctrl Pts',(-0.491513805740775,0.0898277571935297,
-2.66345996776111));
#69297=CARTESIAN_POINT('Ctrl Pts',(-0.467931427741527,0.179879518565837,
-2.66780408811258));
#69298=CARTESIAN_POINT('Ctrl Pts',(-0.42161619699015,0.256121622769783,
-2.67214820846404));
#69299=CARTESIAN_POINT('Ctrl Pts',(-0.336863016011095,0.395638597013269,
-2.68009760248345));
#69300=CARTESIAN_POINT('Ctrl Pts',(-0.175986415474485,0.48891243855205,
-2.68804699650286));
#69301=CARTESIAN_POINT('Ctrl Pts',(-0.0127989464766061,0.493147736670856,
-2.69599639052228));
#69302=CARTESIAN_POINT('Ctrl Pts',(0.150388522521273,0.497383034789663,
-2.70394578454169));
#69303=CARTESIAN_POINT('Ctrl Pts',(0.315886859980421,0.412579789488495,
-2.7118951785611));
#69304=CARTESIAN_POINT('Ctrl Pts',(0.40776299391215,0.277646977311601,-2.71984457258051));
#69305=CARTESIAN_POINT('Ctrl Pts',(0.499639127843881,0.142714165134706,
-2.72779396659992));
#69306=CARTESIAN_POINT('Ctrl Pts',(0.517893058248192,-0.042348213917915,
-2.73574336061933));
#69307=CARTESIAN_POINT('Ctrl Pts',(0.454149613307436,-0.192630817752104,
-2.74369275463874));
#69308=CARTESIAN_POINT('Ctrl Pts',(0.39040616836668,-0.342913421586293,
-2.75164214865816));
#69309=CARTESIAN_POINT('Ctrl Pts',(0.244665348080859,-0.45841625020205,
-2.75959154267757));
#69310=CARTESIAN_POINT('Ctrl Pts',(0.0837951848967256,-0.486144906588543,
-2.76754093669698));
#69311=CARTESIAN_POINT('Ctrl Pts',(-0.077074978287408,-0.513873562975036,
-2.77549033071639));
#69312=CARTESIAN_POINT('Ctrl Pts',(-0.253074484369854,-0.453828047132267,
-2.7834397247358));
#69313=CARTESIAN_POINT('Ctrl Pts',(-0.363452170712636,-0.333558125097149,
-2.79138911875521));
#69314=CARTESIAN_POINT('Ctrl Pts',(-0.445497640280255,-0.244159601218073,
-2.79729802830669));
#69315=CARTESIAN_POINT('Ctrl Pts',(-0.491285856061745,-0.121485993104857,
-2.80320693785816));
#69316=CARTESIAN_POINT('Ctrl Pts',(-0.49238332947362,0.000451585811006003,
-2.80911584740964));
#69317=CARTESIAN_POINT('Ctrl Pts',(-0.492294212910438,0.000443650235898252,
-2.83088415259036));
#69318=CARTESIAN_POINT('Ctrl Pts',(-0.491258114381547,-0.11851055280821,
-2.82512246320279));
#69319=CARTESIAN_POINT('Ctrl Pts',(-0.447935527320371,-0.23814126069821,
-2.81936077381523));
#69320=CARTESIAN_POINT('Ctrl Pts',(-0.369560505409501,-0.326777461536222,
-2.81359908442767));
#69321=CARTESIAN_POINT('Ctrl Pts',(-0.26142660777278,-0.449068692015562,
-2.80564969040825));
#69322=CARTESIAN_POINT('Ctrl Pts',(-0.0865680216788435,-0.512359774978848,
-2.79770029638884));
#69323=CARTESIAN_POINT('Ctrl Pts',(0.0747875611418878,-0.487611830476674,
-2.78975090236943));
#69324=CARTESIAN_POINT('Ctrl Pts',(0.236143143962619,-0.462863885974499,
-2.78180150835002));
#69325=CARTESIAN_POINT('Ctrl Pts',(0.383995723510146,-0.350076914006863,
-2.77385211433061));
#69326=CARTESIAN_POINT('Ctrl Pts',(0.450508361104208,-0.200999236583791,
-2.7659027203112));
#69327=CARTESIAN_POINT('Ctrl Pts',(0.517020998698271,-0.0519215591607172,
-2.75795332629178));
#69328=CARTESIAN_POINT('Ctrl Pts',(0.502193694338868,0.133446823717793,
-2.75000393227237));
#69329=CARTESIAN_POINT('Ctrl Pts',(0.412829433411397,0.270056170892213,
-2.74205453825296));
#69330=CARTESIAN_POINT('Ctrl Pts',(0.323465172483926,0.406665518066632,
-2.73410514423355));
#69331=CARTESIAN_POINT('Ctrl Pts',(0.159563954988387,0.494515829536961,
-2.72615575021414));
#69332=CARTESIAN_POINT('Ctrl Pts',(-0.0036739292267207,0.493300089977269,
-2.71820635619472));
#69333=CARTESIAN_POINT('Ctrl Pts',(-0.166911813441828,0.492084350417578,
-2.71025696217531));
#69334=CARTESIAN_POINT('Ctrl Pts',(-0.329486364376504,0.401802559827868,
-2.7023075681559));
#69335=CARTESIAN_POINT('Ctrl Pts',(-0.416805986309723,0.263877331927563,
-2.69435817413649));
#69336=CARTESIAN_POINT('Ctrl Pts',(-0.46614083558483,0.185950742473243,
-2.68986683362112));
#69337=CARTESIAN_POINT('Ctrl Pts',(-0.491453148001298,0.0928156312110853,
-2.68537549310574));
#69338=CARTESIAN_POINT('Ctrl Pts',(-0.491744581231444,-0.000172364191907249,
-2.68088415259036));
#69339=CARTESIAN_POINT('Origin',(0.,0.,-1.725));
#69340=CARTESIAN_POINT('',(-0.492842183013278,-0.000400497545981371,-2.50911584740964));
#69341=CARTESIAN_POINT('',(-0.492927675364674,-0.00037237350921324,-2.53088415259036));
#69342=CARTESIAN_POINT('',(-0.4925,-6.03138548580071E-17,-1.725));
#69343=CARTESIAN_POINT('Ctrl Pts',(-0.492842183013278,-0.000400497545981371,
-2.50911584740964));
#69344=CARTESIAN_POINT('Ctrl Pts',(-0.491635912823679,0.136456377594769,
-2.51576360364464));
#69345=CARTESIAN_POINT('Ctrl Pts',(-0.432193201139404,0.27423228448661,
-2.52241135987964));
#69346=CARTESIAN_POINT('Ctrl Pts',(-0.330961608144812,0.365818147648235,
-2.52905911611463));
#69347=CARTESIAN_POINT('Ctrl Pts',(-0.209908760916426,0.475336620820701,
-2.53700851013405));
#69348=CARTESIAN_POINT('Ctrl Pts',(-0.0291003124230802,0.518806093660808,
-2.54495790415346));
#69349=CARTESIAN_POINT('Ctrl Pts',(0.128506161165294,0.476282132519312,
-2.55290729817287));
#69350=CARTESIAN_POINT('Ctrl Pts',(0.286112634753665,0.433758171377816,
-2.56085669219228));
#69351=CARTESIAN_POINT('Ctrl Pts',(0.420517133437062,0.305240776254718,
-2.56880608621169));
#69352=CARTESIAN_POINT('Ctrl Pts',(0.470052895899761,0.149695618742931,
-2.5767554802311));
#69353=CARTESIAN_POINT('Ctrl Pts',(0.519588658362461,-0.00584953876885633,
-2.58470487425051));
#69354=CARTESIAN_POINT('Ctrl Pts',(0.484255684604462,-0.188422458669333,
-2.59265426826992));
#69355=CARTESIAN_POINT('Ctrl Pts',(0.380265262794311,-0.314255999348571,
-2.60060366228934));
#69356=CARTESIAN_POINT('Ctrl Pts',(0.276274840984159,-0.44008954002781,
-2.60855305630875));
#69357=CARTESIAN_POINT('Ctrl Pts',(0.103626971121853,-0.509183701485811,
-2.61650245032816));
#69358=CARTESIAN_POINT('Ctrl Pts',(-0.0584649641545909,-0.489837065952524,
-2.62445184434757));
#69359=CARTESIAN_POINT('Ctrl Pts',(-0.220556899431035,-0.470490430419237,
-2.63240123836698));
#69360=CARTESIAN_POINT('Ctrl Pts',(-0.372092900121619,-0.362702997894662,
-2.64035063238639));
#69361=CARTESIAN_POINT('Ctrl Pts',(-0.443546019756161,-0.215929228158279,
-2.64830002640581));
#69362=CARTESIAN_POINT('Ctrl Pts',(-0.47595201826144,-0.149363197353488,
-2.65190530007375));
#69363=CARTESIAN_POINT('Ctrl Pts',(-0.49188594921705,-0.0747781546000925,
-2.6555105737417));
#69364=CARTESIAN_POINT('Ctrl Pts',(-0.491717171688544,-0.000124746059964487,
-2.65911584740964));
#69365=CARTESIAN_POINT('Ctrl Pts',(-0.491744581231444,-0.000172364191907249,
-2.68088415259036));
#69366=CARTESIAN_POINT('Ctrl Pts',(-0.491968966734891,-0.0717673506409361,
-2.67742609908633));
#69367=CARTESIAN_POINT('Ctrl Pts',(-0.477360863836571,-0.143275126154708,
-2.67396804558229));
#69368=CARTESIAN_POINT('Ctrl Pts',(-0.447464606497128,-0.207687030072964,
-2.67050999207826));
#69369=CARTESIAN_POINT('Ctrl Pts',(-0.378738911819555,-0.355757498962288,
-2.66256059805885));
#69370=CARTESIAN_POINT('Ctrl Pts',(-0.229222829532647,-0.466329771530036,
-2.65461120403943));
#69371=CARTESIAN_POINT('Ctrl Pts',(-0.0675165378258877,-0.488671662415771,
-2.64666181002002));
#69372=CARTESIAN_POINT('Ctrl Pts',(0.0941897538808718,-0.511013553301507,
-2.63871241600061));
#69373=CARTESIAN_POINT('Ctrl Pts',(0.268086255007482,-0.44512506250523,
-2.6307630219812));
#69374=CARTESIAN_POINT('Ctrl Pts',(0.374386692522034,-0.321236798936182,
-2.62281362796179));
#69375=CARTESIAN_POINT('Ctrl Pts',(0.480687130036584,-0.197348535367138,
-2.61486423394238));
#69376=CARTESIAN_POINT('Ctrl Pts',(0.519391503939077,-0.0154604990253233,
-2.60691483992296));
#69377=CARTESIAN_POINT('Ctrl Pts',(0.472741678075792,0.140974403131689,
-2.59896544590355));
#69378=CARTESIAN_POINT('Ctrl Pts',(0.426091852212506,0.297409305288705,
-2.59101605188414));
#69379=CARTESIAN_POINT('Ctrl Pts',(0.29408782658344,0.428391073260918,-2.58306665786473));
#69380=CARTESIAN_POINT('Ctrl Pts',(0.137294990151839,0.473823344937194,
-2.57511726384532));
#69381=CARTESIAN_POINT('Ctrl Pts',(-0.0194978462797628,0.519255616613469,
-2.56716786982591));
#69382=CARTESIAN_POINT('Ctrl Pts',(-0.201079493513898,0.479138391993805,
-2.5592184758065));
#69383=CARTESIAN_POINT('Ctrl Pts',(-0.324137620423235,0.371878043926564,
-2.55126908178708));
#69384=CARTESIAN_POINT('Ctrl Pts',(-0.429325143648394,0.280194132942174,
-2.54447410538818));
#69385=CARTESIAN_POINT('Ctrl Pts',(-0.49175260747451,0.139452271736717,
-2.53767912898927));
#69386=CARTESIAN_POINT('Ctrl Pts',(-0.492927675364674,-0.00037237350921324,
-2.53088415259036));
#69387=CARTESIAN_POINT('Origin',(0.,0.,-1.725));
#69388=CARTESIAN_POINT('',(-0.493011002216929,0.000337434886769988,-2.35911584740964));
#69389=CARTESIAN_POINT('',(-0.492930612967012,0.000371277315277309,-2.38088415259036));
#69390=CARTESIAN_POINT('',(-0.4925,-6.03138548580071E-17,-1.725));
#69391=CARTESIAN_POINT('Ctrl Pts',(-0.493011002216929,0.000337434886769988,
-2.35911584740964));
#69392=CARTESIAN_POINT('Ctrl Pts',(-0.493172448397906,0.0209471144955579,
-2.36011784550876));
#69393=CARTESIAN_POINT('Ctrl Pts',(-0.49199234302067,0.0415381637358038,
-2.36111984360787));
#69394=CARTESIAN_POINT('Ctrl Pts',(-0.48940833138991,0.0619515002298427,
-2.36212184170699));
#69395=CARTESIAN_POINT('Ctrl Pts',(-0.468907966547148,0.223901562994389,
-2.3700712357264));
#69396=CARTESIAN_POINT('Ctrl Pts',(-0.360044213363923,0.374666191997443,
-2.37802062974581));
#69397=CARTESIAN_POINT('Ctrl Pts',(-0.212765363372498,0.445072357447139,
-2.38597002376523));
#69398=CARTESIAN_POINT('Ctrl Pts',(-0.0654865133810744,0.515478522896833,
-2.39391941778464));
#69399=CARTESIAN_POINT('Ctrl Pts',(0.120207433418549,0.505526224793171,
-2.40186881180405));
#69400=CARTESIAN_POINT('Ctrl Pts',(0.259117362359501,0.41978172392142,-2.40981820582346));
#69401=CARTESIAN_POINT('Ctrl Pts',(0.398027291300455,0.334037223049669,
-2.41776759984287));
#69402=CARTESIAN_POINT('Ctrl Pts',(0.490153202382736,0.172500519409826,
-2.42571699386228));
#69403=CARTESIAN_POINT('Ctrl Pts',(0.493226372272249,0.00928702911274082,
-2.43366638788169));
#69404=CARTESIAN_POINT('Ctrl Pts',(0.496299542161763,-0.153926461184346,
-2.44161578190111));
#69405=CARTESIAN_POINT('Ctrl Pts',(0.410319970858508,-0.318816738138676,
-2.44956517592052));
#69406=CARTESIAN_POINT('Ctrl Pts',(0.274736350582803,-0.409729716865921,
-2.45751456993993));
#69407=CARTESIAN_POINT('Ctrl Pts',(0.1391527303071,-0.500642695593164,-2.46546396395934));
#69408=CARTESIAN_POINT('Ctrl Pts',(-0.0460349389410497,-0.517578376093326,
-2.47341335797875));
#69409=CARTESIAN_POINT('Ctrl Pts',(-0.195859830083599,-0.452766419000138,
-2.48136275199816));
#69410=CARTESIAN_POINT('Ctrl Pts',(-0.345684721226149,-0.387954461906949,
-2.48931214601758));
#69411=CARTESIAN_POINT('Ctrl Pts',(-0.460146834263098,-0.24139486722041,
-2.49726154003699));
#69412=CARTESIAN_POINT('Ctrl Pts',(-0.48672926779986,-0.0803313331247288,
-2.5052109340564));
#69413=CARTESIAN_POINT('Ctrl Pts',(-0.491081888868664,-0.0539587088519548,
-2.50651257184081));
#69414=CARTESIAN_POINT('Ctrl Pts',(-0.493078372007202,-0.0271972201457358,
-2.50781420962523));
#69415=CARTESIAN_POINT('Ctrl Pts',(-0.492842183013278,-0.000400497545981371,
-2.50911584740964));
#69416=CARTESIAN_POINT('Ctrl Pts',(-0.492927675364674,-0.00037237350921324,
-2.53088415259036));
#69417=CARTESIAN_POINT('Ctrl Pts',(-0.49312731094809,-0.0241275751135129,
-2.52972973496985));
#69418=CARTESIAN_POINT('Ctrl Pts',(-0.491558983946496,-0.0478563025942449,
-2.52857531734935));
#69419=CARTESIAN_POINT('Ctrl Pts',(-0.488132013261578,-0.0713134921138267,
-2.52742089972885));
#69420=CARTESIAN_POINT('Ctrl Pts',(-0.464533672606046,-0.232841208572165,
-2.51947150570944));
#69421=CARTESIAN_POINT('Ctrl Pts',(-0.352802384710446,-0.381493169974031,
-2.51152211169003));
#69422=CARTESIAN_POINT('Ctrl Pts',(-0.204202108219394,-0.449065669503946,
-2.50357271767062));
#69423=CARTESIAN_POINT('Ctrl Pts',(-0.0556018317283395,-0.516638169033863,
-2.49562332365121));
#69424=CARTESIAN_POINT('Ctrl Pts',(0.129867433358168,-0.503131206691828,
-2.48767392963179));
#69425=CARTESIAN_POINT('Ctrl Pts',(0.267109659648677,-0.414741975510851,
-2.47972453561238));
#69426=CARTESIAN_POINT('Ctrl Pts',(0.404351885939185,-0.326352744329874,
-2.47177514159297));
#69427=CARTESIAN_POINT('Ctrl Pts',(0.493367073433696,-0.163081244309955,
-2.46382574757356));
#69428=CARTESIAN_POINT('Ctrl Pts',(0.493313744544244,0.000161158337056044,
-2.45587635355415));
#69429=CARTESIAN_POINT('Ctrl Pts',(0.493260415654792,0.163403560984069,
-2.44792695953474));
#69430=CARTESIAN_POINT('Ctrl Pts',(0.404138570381379,0.326616866258171,
-2.43997756551532));
#69431=CARTESIAN_POINT('Ctrl Pts',(0.266838622470047,0.41491640855305,-2.43202817149591));
#69432=CARTESIAN_POINT('Ctrl Pts',(0.129538674558719,0.503215950847926,
-2.4240787774765));
#69433=CARTESIAN_POINT('Ctrl Pts',(-0.0559393759905273,0.516601730163578,
-2.41612938345709));
#69434=CARTESIAN_POINT('Ctrl Pts',(-0.204495470886693,0.448932154022302,
-2.40817998943768));
#69435=CARTESIAN_POINT('Ctrl Pts',(-0.35305156578286,0.381262577881024,
-2.40023059541827));
#69436=CARTESIAN_POINT('Ctrl Pts',(-0.464685705025947,0.232537646282815,
-2.39228120139885));
#69437=CARTESIAN_POINT('Ctrl Pts',(-0.488178503202315,0.0709945458427664,
-2.38433180737944));
#69438=CARTESIAN_POINT('Ctrl Pts',(-0.491574781289422,0.0476407806578399,
-2.38318258911641));
#69439=CARTESIAN_POINT('Ctrl Pts',(-0.493128944776674,0.0240191214780956,
-2.38203337085339));
#69440=CARTESIAN_POINT('Ctrl Pts',(-0.492930612967012,0.000371277315277309,
-2.38088415259036));
#69441=CARTESIAN_POINT('Origin',(0.,0.,-1.725));
#69442=CARTESIAN_POINT('',(-0.491782200599552,0.000219480096867314,-2.20911584740964));
#69443=CARTESIAN_POINT('',(-0.491745711415915,0.000174011476622056,-2.23088415259036));
#69444=CARTESIAN_POINT('',(-0.4925,-6.03138548580071E-17,-1.725));
#69445=CARTESIAN_POINT('Ctrl Pts',(-0.491782200599552,0.000219480096867314,
-2.20911584740964));
#69446=CARTESIAN_POINT('Ctrl Pts',(-0.492056527069416,0.0686457329269439,
-2.21242148139229));
#69447=CARTESIAN_POINT('Ctrl Pts',(-0.478754286155654,0.136970012424534,
-2.21572711537494));
#69448=CARTESIAN_POINT('Ctrl Pts',(-0.45136026669906,0.199078911138115,
-2.21903274935758));
#69449=CARTESIAN_POINT('Ctrl Pts',(-0.385483083810998,0.348438492561131,
-2.226982143377));
#69450=CARTESIAN_POINT('Ctrl Pts',(-0.238112146179298,0.461854086097113,
-2.23493153739641));
#69451=CARTESIAN_POINT('Ctrl Pts',(-0.0768634080676502,0.487288948894606,
-2.24288093141582));
#69452=CARTESIAN_POINT('Ctrl Pts',(0.0843853300439994,0.5127238116921,-2.25083032543523));
#69453=CARTESIAN_POINT('Ctrl Pts',(0.259511868635597,0.450177943751104,
-2.25877971945464));
#69454=CARTESIAN_POINT('Ctrl Pts',(0.368165575390739,0.32834830943952,-2.26672911347405));
#69455=CARTESIAN_POINT('Ctrl Pts',(0.476819282145881,0.206518675127936,
-2.27467850749347));
#69456=CARTESIAN_POINT('Ctrl Pts',(0.519000157064568,0.025405274445765,
-2.28262790151288));
#69457=CARTESIAN_POINT('Ctrl Pts',(0.475354994181373,-0.131894399886466,
-2.29057729553229));
#69458=CARTESIAN_POINT('Ctrl Pts',(0.431709831298178,-0.289194074218698,
-2.2985266895517));
#69459=CARTESIAN_POINT('Ctrl Pts',(0.302238630613101,-0.42268002220099,
-2.30647608357111));
#69460=CARTESIAN_POINT('Ctrl Pts',(0.146344683743011,-0.471106927092717,
-2.31442547759052));
#69461=CARTESIAN_POINT('Ctrl Pts',(-0.00954926312707591,-0.519533831984444,
-2.32237487160993));
#69462=CARTESIAN_POINT('Ctrl Pts',(-0.191865956182174,-0.482901693785609,
-2.33032426562935));
#69463=CARTESIAN_POINT('Ctrl Pts',(-0.316955814458573,-0.378017876423175,
-2.33827365964876));
#69464=CARTESIAN_POINT('Ctrl Pts',(-0.426278458289986,-0.286354360553994,
-2.34522105556905));
#69465=CARTESIAN_POINT('Ctrl Pts',(-0.491891608337785,-0.142560644619424,
-2.35216845148935));
#69466=CARTESIAN_POINT('Ctrl Pts',(-0.493011002216929,0.000337434886769988,
-2.35911584740964));
#69467=CARTESIAN_POINT('Ctrl Pts',(-0.492930612967012,0.000371277315277309,
-2.38088415259036));
#69468=CARTESIAN_POINT('Ctrl Pts',(-0.491757040280975,-0.139558187556872,
-2.37408397683398));
#69469=CARTESIAN_POINT('Ctrl Pts',(-0.429222514293688,-0.280404479724611,
-2.36728380107759));
#69470=CARTESIAN_POINT('Ctrl Pts',(-0.323894577099873,-0.372089746504211,
-2.36048362532121));
#69471=CARTESIAN_POINT('Ctrl Pts',(-0.200766395711412,-0.479269669129251,
-2.3525342313018));
#69472=CARTESIAN_POINT('Ctrl Pts',(-0.0191585758248402,-0.519268245097442,
-2.34458483728238));
#69473=CARTESIAN_POINT('Ctrl Pts',(0.137604543034586,-0.473733539307189,
-2.33663544326297));
#69474=CARTESIAN_POINT('Ctrl Pts',(0.29436766189401,-0.428198833516938,
-2.32868604924356));
#69475=CARTESIAN_POINT('Ctrl Pts',(0.426286079726287,-0.297130845968246,
-2.32073665522415));
#69476=CARTESIAN_POINT('Ctrl Pts',(0.47283368568467,-0.140665497582472,
-2.31278726120474));
#69477=CARTESIAN_POINT('Ctrl Pts',(0.519381291643053,0.0157998508033048,
-2.30483786718533));
#69478=CARTESIAN_POINT('Ctrl Pts',(0.480558085727538,0.197662560026164,
-2.29688847316592));
#69479=CARTESIAN_POINT('Ctrl Pts',(0.37417672596785,0.321481343583503,-2.2889390791465));
#69480=CARTESIAN_POINT('Ctrl Pts',(0.267795366208163,0.445300127140841,
-2.28098968512709));
#69481=CARTESIAN_POINT('Ctrl Pts',(0.0938558526042994,0.511074985032659,
-2.27304029110768));
#69482=CARTESIAN_POINT('Ctrl Pts',(-0.0678358070548708,0.488627444797658,
-2.26509089708827));
#69483=CARTESIAN_POINT('Ctrl Pts',(-0.229527466714043,0.466179904562656,
-2.25714150306886));
#69484=CARTESIAN_POINT('Ctrl Pts',(-0.378971272428522,0.355509966200836,
-2.24919210904945));
#69485=CARTESIAN_POINT('Ctrl Pts',(-0.447600207562811,0.207394625576466,
-2.24124271503003));
#69486=CARTESIAN_POINT('Ctrl Pts',(-0.477409486442895,0.143060077962531,
-2.23778986088348));
#69487=CARTESIAN_POINT('Ctrl Pts',(-0.491971930291054,0.0716609410359785,
-2.23433700673692));
#69488=CARTESIAN_POINT('Ctrl Pts',(-0.491745711415915,0.000174011476622056,
-2.23088415259036));
#69489=CARTESIAN_POINT('Origin',(0.,0.,-1.725));
#69490=CARTESIAN_POINT('',(-0.49220542790095,-0.00042939446906537,-2.05911584740964));
#69491=CARTESIAN_POINT('',(-0.492291120116919,-0.000443263791466216,-2.08088415259036));
#69492=CARTESIAN_POINT('',(-0.4925,-6.03138548580071E-17,-1.725));
#69493=CARTESIAN_POINT('Ctrl Pts',(-0.49220542790095,-0.00042939446906537,
-2.05911584740964));
#69494=CARTESIAN_POINT('Ctrl Pts',(-0.49124239237179,0.115430969052258,
-2.06472511727582));
#69495=CARTESIAN_POINT('Ctrl Pts',(-0.45038633217708,0.231902596275435,
-2.070334387142));
#69496=CARTESIAN_POINT('Ctrl Pts',(-0.37575132226073,0.319639557992902,
-2.07594365700818));
#69497=CARTESIAN_POINT('Ctrl Pts',(-0.269979427589528,0.443979391054519,
-2.08389305102759));
#69498=CARTESIAN_POINT('Ctrl Pts',(-0.0963650834159402,0.510607835526395,
-2.091842445047));
#69499=CARTESIAN_POINT('Ctrl Pts',(0.0654348949895768,0.488954780866582,
-2.09979183906641));
#69500=CARTESIAN_POINT('Ctrl Pts',(0.227234873395094,0.46730172620677,-2.10774123308582));
#69501=CARTESIAN_POINT('Ctrl Pts',(0.377220486032541,0.357367172415269,
-2.11569062710523));
#69502=CARTESIAN_POINT('Ctrl Pts',(0.446576127279252,0.209590710096725,
-2.12364002112465));
#69503=CARTESIAN_POINT('Ctrl Pts',(0.515931768525963,0.061814247778182,
-2.13158941514406));
#69504=CARTESIAN_POINT('Ctrl Pts',(0.504657438381941,-0.123804123067402,
-2.13953880916347));
#69505=CARTESIAN_POINT('Ctrl Pts',(0.41792596538192,-0.262099963132723,
-2.14748820318288));
#69506=CARTESIAN_POINT('Ctrl Pts',(0.331194492381899,-0.400395803198045,
-2.15543759720229));
#69507=CARTESIAN_POINT('Ctrl Pts',(0.169005876525877,-0.491369112483102,
-2.1633869912217));
#69508=CARTESIAN_POINT('Ctrl Pts',(0.00577464084022879,-0.493279998315106,
-2.17133638524111));
#69509=CARTESIAN_POINT('Ctrl Pts',(-0.157456594845419,-0.49519088414711,
-2.17928577926053));
#69510=CARTESIAN_POINT('Ctrl Pts',(-0.321730450360695,-0.408039346526061,
-2.18723517327994));
#69511=CARTESIAN_POINT('Ctrl Pts',(-0.411675664046121,-0.27181179306051,
-2.19518456729935));
#69512=CARTESIAN_POINT('Ctrl Pts',(-0.464218535589615,-0.192232385228332,
-2.19982832733611));
#69513=CARTESIAN_POINT('Ctrl Pts',(-0.491396826325065,-0.0959058320295775,
-2.20447208737288));
#69514=CARTESIAN_POINT('Ctrl Pts',(-0.491782200599552,0.000219480096867314,
-2.20911584740964));
#69515=CARTESIAN_POINT('Ctrl Pts',(-0.491745711415915,0.000174011476622056,
-2.23088415259036));
#69516=CARTESIAN_POINT('Ctrl Pts',(-0.491451113918055,-0.0929210963697026,
-2.22638761271751));
#69517=CARTESIAN_POINT('Ctrl Pts',(-0.466076412307899,-0.186165091807305,
-2.22189107284465));
#69518=CARTESIAN_POINT('Ctrl Pts',(-0.416633487683608,-0.264149604332216,
-2.2173945329718));
#69519=CARTESIAN_POINT('Ctrl Pts',(-0.329223768116022,-0.402017750729617,
-2.20944513895239));
#69520=CARTESIAN_POINT('Ctrl Pts',(-0.166590264426753,-0.492193300637501,
-2.20149574493298));
#69521=CARTESIAN_POINT('Ctrl Pts',(-0.00335162072512794,-0.493302385121731,
-2.19354635091357));
#69522=CARTESIAN_POINT('Ctrl Pts',(0.159887022976497,-0.494411469605961,
-2.18559695689416));
#69523=CARTESIAN_POINT('Ctrl Pts',(0.323730806690478,-0.406454088666537,
-2.17764756287474));
#69524=CARTESIAN_POINT('Ctrl Pts',(0.413005792026864,-0.269786382681811,
-2.16969816885533));
#69525=CARTESIAN_POINT('Ctrl Pts',(0.502280777363249,-0.133118676697085,
-2.16174877483592));
#69526=CARTESIAN_POINT('Ctrl Pts',(0.516986964322038,0.0522593543329422,
-2.15379938081651));
#69527=CARTESIAN_POINT('Ctrl Pts',(0.450376937973405,0.20129354254415,-2.1458499867971));
#69528=CARTESIAN_POINT('Ctrl Pts',(0.383766911624772,0.350327730755355,
-2.13790059277768));
#69529=CARTESIAN_POINT('Ctrl Pts',(0.235840671968719,0.463018076147741,
-2.12995119875827));
#69530=CARTESIAN_POINT('Ctrl Pts',(0.0744689540071496,0.487660590387776,
-2.12200180473886));
#69531=CARTESIAN_POINT('Ctrl Pts',(-0.0869027639544218,0.512303104627812,
-2.11405241071945));
#69532=CARTESIAN_POINT('Ctrl Pts',(-0.261719960221509,0.448897787715494,
-2.10610301670004));
#69533=CARTESIAN_POINT('Ctrl Pts',(-0.369773933287149,0.32653593185073,
-2.09815362268063));
#69534=CARTESIAN_POINT('Ctrl Pts',(-0.448020352717991,0.237928573651006,
-2.09239713265054));
#69535=CARTESIAN_POINT('Ctrl Pts',(-0.491257364586673,0.118405489671946,
-2.08664064262045));
#69536=CARTESIAN_POINT('Ctrl Pts',(-0.492291120116919,-0.000443263791466216,
-2.08088415259036));
#69537=CARTESIAN_POINT('Origin',(0.,0.,-1.725));
#69538=CARTESIAN_POINT('',(-0.493313293442283,-1.40827548352207E-5,-1.90911584740964));
#69539=CARTESIAN_POINT('',(-0.493309198850653,4.2667367679637E-5,-1.93088415259036));
#69540=CARTESIAN_POINT('',(-0.4925,-6.03138548580071E-17,-1.725));
#69541=CARTESIAN_POINT('Ctrl Pts',(-0.493313293442283,-1.40827548352207E-5,
-1.90911584740964));
#69542=CARTESIAN_POINT('Ctrl Pts',(-0.49324531272362,0.162479492642686,
-1.91702875315935));
#69543=CARTESIAN_POINT('Ctrl Pts',(-0.405109814225056,0.325036240628224,
-1.92494165890906));
#69544=CARTESIAN_POINT('Ctrl Pts',(-0.2688734530373,0.413600736781722,-1.93285456465877));
#69545=CARTESIAN_POINT('Ctrl Pts',(-0.132008873942307,0.502573624659309,
-1.94080395867818));
#69546=CARTESIAN_POINT('Ctrl Pts',(0.0534011994185894,0.51687029601571,
-1.94875335269759));
#69547=CARTESIAN_POINT('Ctrl Pts',(0.202287897688472,0.449931227704149,
-1.956702746717));
#69548=CARTESIAN_POINT('Ctrl Pts',(0.351174595958352,0.382992159392589,
-1.96465214073641));
#69549=CARTESIAN_POINT('Ctrl Pts',(0.463537919137217,0.234817351413069,
-1.97260153475583));
#69550=CARTESIAN_POINT('Ctrl Pts',(0.487823921494154,0.0733915855711673,
-1.98055092877524));
#69551=CARTESIAN_POINT('Ctrl Pts',(0.512109923851091,-0.0880341802707372,
-1.98850032279465));
#69552=CARTESIAN_POINT('Ctrl Pts',(0.448318605386097,-0.262710903975027,
-1.99644971681406));
#69553=CARTESIAN_POINT('Ctrl Pts',(0.325718361490191,-0.370494334913139,
-2.00439911083347));
#69554=CARTESIAN_POINT('Ctrl Pts',(0.203118117594284,-0.478277765851253,
-2.01234850485288));
#69555=CARTESIAN_POINT('Ctrl Pts',(0.0217089482674663,-0.519167904023189,
-2.02029789887229));
#69556=CARTESIAN_POINT('Ctrl Pts',(-0.135275950764312,-0.474403752471875,
-2.02824729289171));
#69557=CARTESIAN_POINT('Ctrl Pts',(-0.292260849796088,-0.429639600920561,
-2.03619668691112));
#69558=CARTESIAN_POINT('Ctrl Pts',(-0.424821478532825,-0.299221159645997,
-2.04414608093053));
#69559=CARTESIAN_POINT('Ctrl Pts',(-0.472137070316785,-0.142986328183037,
-2.05209547494994));
#69560=CARTESIAN_POINT('Ctrl Pts',(-0.486065724361081,-0.0969942812685151,
-2.05443559910318));
#69561=CARTESIAN_POINT('Ctrl Pts',(-0.492607195467135,-0.0487650320024671,
-2.05677572325641));
#69562=CARTESIAN_POINT('Ctrl Pts',(-0.49220542790095,-0.00042939446906537,
-2.05911584740964));
#69563=CARTESIAN_POINT('Ctrl Pts',(-0.492291120116919,-0.000443263791466216,
-2.08088415259036));
#69564=CARTESIAN_POINT('Ctrl Pts',(-0.492684923739337,-0.0457180587157333,
-2.07869124860104));
#69565=CARTESIAN_POINT('Ctrl Pts',(-0.486954240838252,-0.0908949955950586,
-2.07649834461171));
#69566=CARTESIAN_POINT('Ctrl Pts',(-0.474701379384562,-0.134227705555401,
-2.07430544062239));
#69567=CARTESIAN_POINT('Ctrl Pts',(-0.430284102552143,-0.291311092279559,
-2.06635604660298));
#69568=CARTESIAN_POINT('Ctrl Pts',(-0.30015879902311,-0.424159470910667,
-2.05840665258357));
#69569=CARTESIAN_POINT('Ctrl Pts',(-0.144028872422113,-0.471820050906157,
-2.05045725856416));
#69570=CARTESIAN_POINT('Ctrl Pts',(0.0121010541788825,-0.519480630901646,
-2.04250786454475));
#69571=CARTESIAN_POINT('Ctrl Pts',(0.194235603851841,-0.481953412261521,
-2.03455847052533));
#69572=CARTESIAN_POINT('Ctrl Pts',(0.31880876569642,-0.376456434987368,
-2.02660907650592));
#69573=CARTESIAN_POINT('Ctrl Pts',(0.443381927541001,-0.270959457713215,
-2.01865968248651));
#69574=CARTESIAN_POINT('Ctrl Pts',(0.510393701557199,-0.0974927218050333,
-2.0107102884671));
#69575=CARTESIAN_POINT('Ctrl Pts',(0.489098099968701,0.0643546823104579,
-2.00276089444769));
#69576=CARTESIAN_POINT('Ctrl Pts',(0.467802498380204,0.226202086425949,
-1.99481150042828));
#69577=CARTESIAN_POINT('Ctrl Pts',(0.358199521187009,0.376430158748751,
-1.98686210640886));
#69578=CARTESIAN_POINT('Ctrl Pts',(0.210576626772402,0.446112049585561,
-1.97891271238945));
#69579=CARTESIAN_POINT('Ctrl Pts',(0.0629537323577946,0.515793940422371,
-1.97096331837004));
#69580=CARTESIAN_POINT('Ctrl Pts',(-0.122689079278224,0.504929649773189,
-1.96301392435063));
#69581=CARTESIAN_POINT('Ctrl Pts',(-0.261176155034131,0.418503874020135,
-1.95506453033122));
#69582=CARTESIAN_POINT('Ctrl Pts',(-0.399663230790036,0.332078098267084,
-1.94711513631181));
#69583=CARTESIAN_POINT('Ctrl Pts',(-0.490994570665829,0.170090837410162,
-1.9391657422924));
#69584=CARTESIAN_POINT('Ctrl Pts',(-0.493266012286453,0.00686422983988139,
-1.93121634827298));
#69585=CARTESIAN_POINT('Ctrl Pts',(-0.493297652564017,0.00459054817341155,
-1.93110561637878));
#69586=CARTESIAN_POINT('Ctrl Pts',(-0.493312012210231,0.00231662603177743,
-1.93099488448457));
#69587=CARTESIAN_POINT('Ctrl Pts',(-0.493309198850653,4.2667367679637E-5,
-1.93088415259036));
#69588=CARTESIAN_POINT('Origin',(0.,0.,-1.725));
#69589=CARTESIAN_POINT('',(-0.492247450406692,0.000436970853093216,-1.75911584740964));
#69590=CARTESIAN_POINT('',(-0.492163707300124,0.000420305474583196,-1.78088415259036));
#69591=CARTESIAN_POINT('',(-0.4925,-6.03138548580071E-17,-1.725));
#69592=CARTESIAN_POINT('Ctrl Pts',(-0.492247450406692,0.000436970853093216,
-1.75911584740964));
#69593=CARTESIAN_POINT('Ctrl Pts',(-0.492646083681307,0.0472551432774344,
-1.76138299502347));
#69594=CARTESIAN_POINT('Ctrl Pts',(-0.48651356696863,0.0939709787487651,
-1.7636501426373));
#69595=CARTESIAN_POINT('Ctrl Pts',(-0.473428455624523,0.13865064233376,
-1.76591729025113));
#69596=CARTESIAN_POINT('Ctrl Pts',(-0.427547585218155,0.295312805981787,
-1.77386668427054));
#69597=CARTESIAN_POINT('Ctrl Pts',(-0.296188516357401,0.426941393847813,
-1.78181607828995));
#69598=CARTESIAN_POINT('Ctrl Pts',(-0.139620722351902,0.473143273337493,
-1.78976547230936));
#69599=CARTESIAN_POINT('Ctrl Pts',(0.0169470716535901,0.519345152827171,
-1.79771486632877));
#69600=CARTESIAN_POINT('Ctrl Pts',(0.198723590803828,0.480120323940512,
-1.80566426034818));
#69601=CARTESIAN_POINT('Ctrl Pts',(0.322307093869532,0.373465715234961,
-1.8136136543676));
#69602=CARTESIAN_POINT('Ctrl Pts',(0.44589059693524,0.266811106529407,-1.82156304838701));
#69603=CARTESIAN_POINT('Ctrl Pts',(0.511281083916411,0.0927267180049563,
-1.82951244240642));
#69604=CARTESIAN_POINT('Ctrl Pts',(0.488476437380305,-0.0689149718046035,
-1.83746183642583));
#69605=CARTESIAN_POINT('Ctrl Pts',(0.465671790844199,-0.230556661614166,
-1.84541123044524));
#69606=CARTESIAN_POINT('Ctrl Pts',(0.354672010790817,-0.379755652708832,
-1.85336062446465));
#69607=CARTESIAN_POINT('Ctrl Pts',(0.206405429305048,-0.448057253002318,
-1.86131001848406));
#69608=CARTESIAN_POINT('Ctrl Pts',(0.0581388478192817,-0.516358853295804,
-1.86925941250348));
#69609=CARTESIAN_POINT('Ctrl Pts',(-0.127394535098869,-0.503763062788106,
-1.87720880652289));
#69610=CARTESIAN_POINT('Ctrl Pts',(-0.265069273853518,-0.416049015469756,
-1.8851582005423));
#69611=CARTESIAN_POINT('Ctrl Pts',(-0.402744012608164,-0.328334968151407,
-1.89310759456171));
#69612=CARTESIAN_POINT('Ctrl Pts',(-0.492560107199312,-0.165502664022405,
-1.90105698858112));
#69613=CARTESIAN_POINT('Ctrl Pts',(-0.493308612080344,-0.00226195975852084,
-1.90900638260053));
#69614=CARTESIAN_POINT('Ctrl Pts',(-0.493312047769644,-0.00151267360803209,
-1.90904287087024));
#69615=CARTESIAN_POINT('Ctrl Pts',(-0.493313606917367,-0.0007633788530685,
-1.90907935913994));
#69616=CARTESIAN_POINT('Ctrl Pts',(-0.493313293442283,-1.40827548352207E-5,
-1.90911584740964));
#69617=CARTESIAN_POINT('Ctrl Pts',(-0.493309198850653,4.2667367679637E-5,
-1.93088415259036));
#69618=CARTESIAN_POINT('Ctrl Pts',(-0.49311004236262,-0.160929867076482,
-1.92304549046516));
#69619=CARTESIAN_POINT('Ctrl Pts',(-0.406854173941428,-0.322085421498344,
-1.91520682833995));
#69620=CARTESIAN_POINT('Ctrl Pts',(-0.27272046309321,-0.411074233610547,
-1.90736816621475));
#69621=CARTESIAN_POINT('Ctrl Pts',(-0.136691928913891,-0.501320135207048,
-1.89941877219534));
#69622=CARTESIAN_POINT('Ctrl Pts',(0.0485766828101977,-0.517345984116404,
-1.89146937817593));
#69623=CARTESIAN_POINT('Ctrl Pts',(0.198081407402245,-0.451798885091386,
-1.88351998415651));
#69624=CARTESIAN_POINT('Ctrl Pts',(0.347586131994292,-0.386251786066369,
-1.8755705901371));
#69625=CARTESIAN_POINT('Ctrl Pts',(0.461326969454297,-0.239131739106977,
-1.86762119611769));
#69626=CARTESIAN_POINT('Ctrl Pts',(0.48711795023357,-0.0779395861454187,
-1.85967180209828));
#69627=CARTESIAN_POINT('Ctrl Pts',(0.512908931012843,0.0832525668161397,
-1.85172240807887));
#69628=CARTESIAN_POINT('Ctrl Pts',(0.450750055111385,0.258516825779865,
-1.84377301405946));
#69629=CARTESIAN_POINT('Ctrl Pts',(0.329160729256043,0.367439370296521,
-1.83582362004004));
#69630=CARTESIAN_POINT('Ctrl Pts',(0.207571403400702,0.476361914813175,
-1.82787422602063));
#69631=CARTESIAN_POINT('Ctrl Pts',(0.0265516275914822,0.518942744882762,
-1.81992483200122));
#69632=CARTESIAN_POINT('Ctrl Pts',(-0.130844061920186,0.475645149232598,
-1.81197543798181));
#69633=CARTESIAN_POINT('Ctrl Pts',(-0.288239751431856,0.432347553582433,
-1.8040260439624));
#69634=CARTESIAN_POINT('Ctrl Pts',(-0.422011354645973,0.303171532212515,
-1.79607664994299));
#69635=CARTESIAN_POINT('Ctrl Pts',(-0.470782491999074,0.147384944127326,
-1.78812725592358));
#69636=CARTESIAN_POINT('Ctrl Pts',(-0.485595125794996,0.100069876141216,
-1.78571288814584));
#69637=CARTESIAN_POINT('Ctrl Pts',(-0.492566964375401,0.050300139206298,
-1.7832985203681));
#69638=CARTESIAN_POINT('Ctrl Pts',(-0.492163707300124,0.000420305474583196,
-1.78088415259036));
#69639=CARTESIAN_POINT('Origin',(0.,0.,-1.725));
#69640=CARTESIAN_POINT('',(-0.491763056642317,-0.000197237602559575,-1.60911584740964));
#69641=CARTESIAN_POINT('',(-0.491803762672827,-0.000241441601782219,-1.63088415259036));
#69642=CARTESIAN_POINT('',(-0.4925,-6.03138548580071E-17,-1.725));
#69643=CARTESIAN_POINT('Ctrl Pts',(-0.491763056642317,-0.000197237602559575,
-1.60911584740964));
#69644=CARTESIAN_POINT('Ctrl Pts',(-0.491422941966957,0.0944266719329545,
-1.613686630907));
#69645=CARTESIAN_POINT('Ctrl Pts',(-0.465147652160607,0.189225351877548,
-1.61825741440436));
#69646=CARTESIAN_POINT('Ctrl Pts',(-0.414150969357646,0.268025143959866,
-1.62282819790172));
#69647=CARTESIAN_POINT('Ctrl Pts',(-0.325458795353369,0.405071800462394,
-1.63077759192113));
#69648=CARTESIAN_POINT('Ctrl Pts',(-0.161991059533466,0.493726126140734,
-1.63872698594054));
#69649=CARTESIAN_POINT('Ctrl Pts',(0.00125083601822007,0.493312212117073,
-1.64667637995995));
#69650=CARTESIAN_POINT('Ctrl Pts',(0.164492731569907,0.492898298093412,
-1.65462577397937));
#69651=CARTESIAN_POINT('Ctrl Pts',(0.327508786853377,0.403416144367749,
-1.66257516799878));
#69652=CARTESIAN_POINT('Ctrl Pts',(0.415504837459898,0.265921479504776,
-1.67052456201819));
#69653=CARTESIAN_POINT('Ctrl Pts',(0.503500888066418,0.128426814641802,
-1.6784739560376));
#69654=CARTESIAN_POINT('Ctrl Pts',(0.516476933995988,-0.0570803613584818,
-1.68642335005701));
#69655=CARTESIAN_POINT('Ctrl Pts',(0.448479374476317,-0.205486627019658,
-1.69437274407642));
#69656=CARTESIAN_POINT('Ctrl Pts',(0.380481814956647,-0.353892892680831,
-1.70232213809583));
#69657=CARTESIAN_POINT('Ctrl Pts',(0.231510649987738,-0.465198248002898,
-1.71027153211525));
#69658=CARTESIAN_POINT('Ctrl Pts',(0.0699160416776696,-0.488334158472158,
-1.71822092613466));
#69659=CARTESIAN_POINT('Ctrl Pts',(-0.0916785666324007,-0.511470068941419,
-1.72617032015407));
#69660=CARTESIAN_POINT('Ctrl Pts',(-0.26589661828363,-0.44643653455787,
-1.73411971417348));
#69661=CARTESIAN_POINT('Ctrl Pts',(-0.372804308133253,-0.323071897651082,
-1.74206910819289));
#69662=CARTESIAN_POINT('Ctrl Pts',(-0.449222187897897,-0.234890551635539,
-1.74775135459847));
#69663=CARTESIAN_POINT('Ctrl Pts',(-0.491248339242509,-0.116905362902091,
-1.75343360100406));
#69664=CARTESIAN_POINT('Ctrl Pts',(-0.492247450406692,0.000436970853093216,
-1.75911584740964));
#69665=CARTESIAN_POINT('Ctrl Pts',(-0.492163707300124,0.000420305474583196,
-1.78088415259036));
#69666=CARTESIAN_POINT('Ctrl Pts',(-0.491239225738378,-0.113931033696202,
-1.77534912634869));
#69667=CARTESIAN_POINT('Ctrl Pts',(-0.451553280043693,-0.228861011197853,
-1.76981410010701));
#69668=CARTESIAN_POINT('Ctrl Pts',(-0.378717055390082,-0.316120022277836,
-1.76427907386534));
#69669=CARTESIAN_POINT('Ctrl Pts',(-0.274109809935903,-0.441441245797349,
-1.75632967984593));
#69670=CARTESIAN_POINT('Ctrl Pts',(-0.101124647535461,-0.50968653803592,
-1.74838028582652));
#69671=CARTESIAN_POINT('Ctrl Pts',(0.0608702943946502,-0.489543954909651,
-1.74043089180711));
#69672=CARTESIAN_POINT('Ctrl Pts',(0.222865236324764,-0.469401371783382,
-1.7324814977877));
#69673=CARTESIAN_POINT('Ctrl Pts',(0.373869957784543,-0.36087091329227,
-1.72453210376828));
#69674=CARTESIAN_POINT('Ctrl Pts',(0.444601271030807,-0.2137479504605,-1.71658270974887));
#69675=CARTESIAN_POINT('Ctrl Pts',(0.51533258427707,-0.0666249876287323,
-1.70863331572946));
#69676=CARTESIAN_POINT('Ctrl Pts',(0.505790489309818,0.119090479543697,
-1.70068392171005));
#69677=CARTESIAN_POINT('Ctrl Pts',(0.420353039680544,0.258189462526263,
-1.69273452769064));
#69678=CARTESIAN_POINT('Ctrl Pts',(0.33491559005127,0.39728844550883,-1.68478513367123));
#69679=CARTESIAN_POINT('Ctrl Pts',(0.173582785759975,0.489770944301538,
-1.67683573965181));
#69680=CARTESIAN_POINT('Ctrl Pts',(0.0103764908966829,0.493204627882733,
-1.6688863456324));
#69681=CARTESIAN_POINT('Ctrl Pts',(-0.152829803966609,0.496638311463928,
-1.66093695161299));
#69682=CARTESIAN_POINT('Ctrl Pts',(-0.317909589401894,0.41102317983361,
-1.65298755759358));
#69683=CARTESIAN_POINT('Ctrl Pts',(-0.409121831245792,0.275640714928625,
-1.64503816357417));
#69684=CARTESIAN_POINT('Ctrl Pts',(-0.463256736361998,0.195290569554802,
-1.6403201599129));
#69685=CARTESIAN_POINT('Ctrl Pts',(-0.491371949157338,0.0974099820344272,
-1.63560215625163));
#69686=CARTESIAN_POINT('Ctrl Pts',(-0.491803762672827,-0.000241441601782219,
-1.63088415259036));
#69687=CARTESIAN_POINT('Origin',(0.,0.,-1.725));
#69688=CARTESIAN_POINT('',(-0.492971877712692,-0.00035487951936386,-1.45911584740964));
#69689=CARTESIAN_POINT('',(-0.493049169896767,-0.00031838663161669,-1.48088415259036));
#69690=CARTESIAN_POINT('',(-0.4925,-6.03138548580071E-17,-1.725));
#69691=CARTESIAN_POINT('Ctrl Pts',(-0.492971877712692,-0.00035487951936386,
-1.45911584740964));
#69692=CARTESIAN_POINT('Ctrl Pts',(-0.491822722696216,0.141071489966078,
-1.46599026679053));
#69693=CARTESIAN_POINT('Ctrl Pts',(-0.427747046070754,0.283406525101959,
-1.47286468617142));
#69694=CARTESIAN_POINT('Ctrl Pts',(-0.320409052113906,0.375095377921473,
-1.47973910555231));
#69695=CARTESIAN_POINT('Ctrl Pts',(-0.196286277529025,0.481121905816508,
-1.48768849957172));
#69696=CARTESIAN_POINT('Ctrl Pts',(-0.0143131810680683,0.519424415916717,
-1.49563789359113));
#69697=CARTESIAN_POINT('Ctrl Pts',(0.142018303477539,0.472429153092764,
-1.50358728761054));
#69698=CARTESIAN_POINT('Ctrl Pts',(0.298349788023149,0.42543389026881,-1.51153668162996));
#69699=CARTESIAN_POINT('Ctrl Pts',(0.429039660653408,0.293140854520689,
-1.51948607564937));
#69700=CARTESIAN_POINT('Ctrl Pts',(0.47412548513425,0.136248036906213,-1.52743546966878));
#69701=CARTESIAN_POINT('Ctrl Pts',(0.519211309615092,-0.0206447807082635,
-1.53538486368819));
#69702=CARTESIAN_POINT('Ctrl Pts',(0.478693085946517,-0.202137380189096,
-1.5433342577076));
#69703=CARTESIAN_POINT('Ctrl Pts',(0.371161171239962,-0.32495828682827,
-1.55128365172701));
#69704=CARTESIAN_POINT('Ctrl Pts',(0.263629256533406,-0.447779193467444,
-1.55923304574643));
#69705=CARTESIAN_POINT('Ctrl Pts',(0.0890836507888685,-0.511928407264959,
-1.56718243976584));
#69706=CARTESIAN_POINT('Ctrl Pts',(-0.0723915542139933,-0.487973325185985,
-1.57513183378525));
#69707=CARTESIAN_POINT('Ctrl Pts',(-0.233866759216855,-0.464018243107011,
-1.58308122780466));
#69708=CARTESIAN_POINT('Ctrl Pts',(-0.382271563478042,-0.351958865151547,
-1.59103062182407));
#69709=CARTESIAN_POINT('Ctrl Pts',(-0.449515659514308,-0.203209682510457,
-1.59898001584348));
#69710=CARTESIAN_POINT('Ctrl Pts',(-0.478095399033977,-0.139989070676324,
-1.60235862636554));
#69711=CARTESIAN_POINT('Ctrl Pts',(-0.492014461028795,-0.0701408996856698,
-1.60573723688759));
#69712=CARTESIAN_POINT('Ctrl Pts',(-0.491763056642317,-0.000197237602559575,
-1.60911584740964));
#69713=CARTESIAN_POINT('Ctrl Pts',(-0.491803762672827,-0.000241441601782219,
-1.63088415259036));
#69714=CARTESIAN_POINT('Ctrl Pts',(-0.49209951446334,-0.0671235153456273,
-1.62765276223222));
#69715=CARTESIAN_POINT('Ctrl Pts',(-0.479409077259817,-0.133898089086301,
-1.62442137187408));
#69716=CARTESIAN_POINT('Ctrl Pts',(-0.453197923274928,-0.194859228335653,
-1.62118998151593));
#69717=CARTESIAN_POINT('Ctrl Pts',(-0.388717075207656,-0.344826908515301,
-1.61324058749652));
#69718=CARTESIAN_POINT('Ctrl Pts',(-0.242410680820596,-0.459612470694942,
-1.60529119347711));
#69719=CARTESIAN_POINT('Ctrl Pts',(-0.0814062662755531,-0.48655061025483,
-1.5973417994577));
#69720=CARTESIAN_POINT('Ctrl Pts',(0.079598148269487,-0.513488749814717,
-1.58939240543829));
#69721=CARTESIAN_POINT('Ctrl Pts',(0.255300582972512,-0.452579466754855,
-1.58144301141888));
#69722=CARTESIAN_POINT('Ctrl Pts',(0.365086175908778,-0.331768836222721,
-1.57349361739946));
#69723=CARTESIAN_POINT('Ctrl Pts',(0.474871768845042,-0.21095820569059,
-1.56554422338005));
#69724=CARTESIAN_POINT('Ctrl Pts',(0.518740520014552,-0.0302462276861947,
-1.55759482936064));
#69725=CARTESIAN_POINT('Ctrl Pts',(0.47656480099646,0.127453783700125,-1.54964543534123));
#69726=CARTESIAN_POINT('Ctrl Pts',(0.434389081978368,0.285153795086447,
-1.54169604132182));
#69727=CARTESIAN_POINT('Ctrl Pts',(0.306168892772669,0.419841839854689,
-1.53374664730241));
#69728=CARTESIAN_POINT('Ctrl Pts',(0.150733542524981,0.469721061573934,
-1.525797253283));
#69729=CARTESIAN_POINT('Ctrl Pts',(-0.00470180772270484,0.519600283293178,
-1.51784785926358));
#69730=CARTESIAN_POINT('Ctrl Pts',(-0.187352319012382,0.484670681963428,
-1.50989846524417));
#69731=CARTESIAN_POINT('Ctrl Pts',(-0.313415249663277,0.380958472548885,
-1.50194907122476));
#69732=CARTESIAN_POINT('Ctrl Pts',(-0.424765681762926,0.289350263278393,
-1.49492743167996));
#69733=CARTESIAN_POINT('Ctrl Pts',(-0.491966171457023,0.144077483952644,
-1.48790579213516));
#69734=CARTESIAN_POINT('Ctrl Pts',(-0.493049169896767,-0.00031838663161669,
-1.48088415259036));
#69735=CARTESIAN_POINT('Origin',(0.,0.,-1.725));
#69736=CARTESIAN_POINT('',(-0.492885109875619,0.000387266687590468,-1.30911584740964));
#69737=CARTESIAN_POINT('',(-0.492797570805203,0.000412494226899228,-1.33088415259036));
#69738=CARTESIAN_POINT('',(-0.4925,-6.03138548580071E-17,-1.725));
#69739=CARTESIAN_POINT('Ctrl Pts',(-0.492885109875619,0.000387266687590468,
-1.30911584740964));
#69740=CARTESIAN_POINT('Ctrl Pts',(-0.493103291714472,0.025675910579845,
-1.31034450865465));
#69741=CARTESIAN_POINT('Ctrl Pts',(-0.49132560003428,0.0509337966894253,
-1.31157316989966));
#69742=CARTESIAN_POINT('Ctrl Pts',(-0.487445469794451,0.0758644659340029,
-1.31280183114467));
#69743=CARTESIAN_POINT('Ctrl Pts',(-0.46234116684007,0.237164998361211,
-1.32075122516408));
#69744=CARTESIAN_POINT('Ctrl Pts',(-0.349227873070351,0.384768090768282,
-1.32870061918349));
#69745=CARTESIAN_POINT('Ctrl Pts',(-0.200003631756639,0.450951272865195,
-1.3366500132029));
#69746=CARTESIAN_POINT('Ctrl Pts',(-0.0507793904429269,0.517134454962107,
-1.34459940722231));
#69747=CARTESIAN_POINT('Ctrl Pts',(0.134555798414777,0.501897726748859,
-1.35254880124173));
#69748=CARTESIAN_POINT('Ctrl Pts',(0.270967423571298,0.412231923287992,
-1.36049819526114));
#69749=CARTESIAN_POINT('Ctrl Pts',(0.407379048727822,0.322566119827124,
-1.36844758928055));
#69750=CARTESIAN_POINT('Ctrl Pts',(0.494867110183159,0.158471241118635,
-1.37639698329996));
#69751=CARTESIAN_POINT('Ctrl Pts',(0.493290798242749,-0.00476356837000694,
-1.38434637731937));
#69752=CARTESIAN_POINT('Ctrl Pts',(0.49171448630234,-0.167998377858649,
-1.39229577133878));
#69753=CARTESIAN_POINT('Ctrl Pts',(0.401073800966179,-0.330373118127449,
-1.4002451653582));
#69754=CARTESIAN_POINT('Ctrl Pts',(0.262956022145839,-0.417387869531233,
-1.40819455937761));
#69755=CARTESIAN_POINT('Ctrl Pts',(0.1248382433255,-0.504402620935016,-1.41614395339702));
#69756=CARTESIAN_POINT('Ctrl Pts',(-0.0607566289790167,-0.516057383473792,
-1.42409334741643));
#69757=CARTESIAN_POINT('Ctrl Pts',(-0.208674936936753,-0.447004780633302,
-1.43204274143584));
#69758=CARTESIAN_POINT('Ctrl Pts',(-0.356593244894491,-0.377952177792812,
-1.43999213545525));
#69759=CARTESIAN_POINT('Ctrl Pts',(-0.466834988505445,-0.228192209573053,
-1.44794152947466));
#69760=CARTESIAN_POINT('Ctrl Pts',(-0.48881963395652,-0.0664369526182409,
-1.45589092349408));
#69761=CARTESIAN_POINT('Ctrl Pts',(-0.491792556954056,-0.0445632351437636,
-1.4569658981326));
#69762=CARTESIAN_POINT('Ctrl Pts',(-0.493151574706721,-0.022470166933687,
-1.45804087277112));
#69763=CARTESIAN_POINT('Ctrl Pts',(-0.492971877712692,-0.00035487951936386,
-1.45911584740964));
#69764=CARTESIAN_POINT('Ctrl Pts',(-0.493049169896767,-0.00031838663161669,
-1.48088415259036));
#69765=CARTESIAN_POINT('Ctrl Pts',(-0.493192264204308,-0.0193971095132318,
-1.47995639811575));
#69766=CARTESIAN_POINT('Ctrl Pts',(-0.492181093798244,-0.0384605235136697,
-1.47902864364114));
#69767=CARTESIAN_POINT('Ctrl Pts',(-0.489964987012965,-0.0573828199869844,
-1.47810088916653));
#69768=CARTESIAN_POINT('Ctrl Pts',(-0.470976443699642,-0.219517085608957,
-1.47015149514712));
#69769=CARTESIAN_POINT('Ctrl Pts',(-0.363524007060886,-0.371290799353565,
-1.4622021011277));
#69770=CARTESIAN_POINT('Ctrl Pts',(-0.216908435835479,-0.443067948504154,
-1.45425270710829));
#69771=CARTESIAN_POINT('Ctrl Pts',(-0.0702928646100672,-0.514845097654745,
-1.44630331308888));
#69772=CARTESIAN_POINT('Ctrl Pts',(0.115485841202,-0.506625682211315,-1.43835391906947));
#69773=CARTESIAN_POINT('Ctrl Pts',(0.255189678251986,-0.422180890900952,
-1.43040452505006));
#69774=CARTESIAN_POINT('Ctrl Pts',(0.394893515301968,-0.337736099590592,
-1.42245513103065));
#69775=CARTESIAN_POINT('Ctrl Pts',(0.488522483589872,-0.17706593241331,
-1.41450573701123));
#69776=CARTESIAN_POINT('Ctrl Pts',(0.49311823502313,-0.0138882258026879,
-1.40655634299182));
#69777=CARTESIAN_POINT('Ctrl Pts',(0.497713986456388,0.149289480807939,
-1.39860694897241));
#69778=CARTESIAN_POINT('Ctrl Pts',(0.413276521034989,0.314974726851901,
-1.390657554953));
#69779=CARTESIAN_POINT('Ctrl Pts',(0.278546990113647,0.407148683931192,
-1.38270816093359));
#69780=CARTESIAN_POINT('Ctrl Pts',(0.143817459192309,0.49932264101048,-1.37475876691418));
#69781=CARTESIAN_POINT('Ctrl Pts',(-0.041204137228972,0.517985309125103,
-1.36680937289476));
#69782=CARTESIAN_POINT('Ctrl Pts',(-0.191627168728328,0.454573981584339,
-1.35885997887535));
#69783=CARTESIAN_POINT('Ctrl Pts',(-0.342050200227689,0.391162654043573,
-1.35091058485594));
#69784=CARTESIAN_POINT('Ctrl Pts',(-0.457874666805125,0.245677330847414,
-1.34296119083653));
#69785=CARTESIAN_POINT('Ctrl Pts',(-0.485958599219122,0.0848688186159221,
-1.33501179681712));
#69786=CARTESIAN_POINT('Ctrl Pts',(-0.490819367273069,0.0570360754112031,
-1.3336359154082));
#69787=CARTESIAN_POINT('Ctrl Pts',(-0.493051718544713,0.0287443000430391,
-1.33226003399928));
#69788=CARTESIAN_POINT('Ctrl Pts',(-0.492797570805203,0.000412494226899228,
-1.33088415259036));
#69789=CARTESIAN_POINT('Origin',(0.,0.,-1.725));
#69790=CARTESIAN_POINT('',(-0.491729663766022,0.000148572764139432,-1.15911584740964));
#69791=CARTESIAN_POINT('',(-0.491706700480042,0.000100130005186201,-1.18088415259036));
#69792=CARTESIAN_POINT('',(-0.4925,-6.03138548580071E-17,-1.725));
#69793=CARTESIAN_POINT('Ctrl Pts',(-0.491729663766022,0.000148572764139432,
-1.15911584740964));
#69794=CARTESIAN_POINT('Ctrl Pts',(-0.491926890574513,0.0732862396464759,
-1.16264814453818));
#69795=CARTESIAN_POINT('Ctrl Pts',(-0.476658155659677,0.146345621070356,
-1.16618044166672));
#69796=CARTESIAN_POINT('Ctrl Pts',(-0.44550752094592,0.211852665773185,
-1.16971273879526));
#69797=CARTESIAN_POINT('Ctrl Pts',(-0.37540337616897,0.359275515675158,
-1.17766213281467));
#69798=CARTESIAN_POINT('Ctrl Pts',(-0.224862198434001,0.468448057652222,
-1.18561152683408));
#69799=CARTESIAN_POINT('Ctrl Pts',(-0.0629544948037265,0.489280323330698,
-1.1935609208535));
#69800=CARTESIAN_POINT('Ctrl Pts',(0.0989532088265435,0.510112589009172,
-1.20151031487291));
#69801=CARTESIAN_POINT('Ctrl Pts',(0.27222743835212,0.442604578389054,-1.20945970889232));
#69802=CARTESIAN_POINT('Ctrl Pts',(0.377367428106713,0.317729959901029,
-1.21740910291173));
#69803=CARTESIAN_POINT('Ctrl Pts',(0.482507417861307,0.192855341413001,
-1.22535849693114));
#69804=CARTESIAN_POINT('Ctrl Pts',(0.519513167844922,0.010614115057068,
-1.23330789095055));
#69805=CARTESIAN_POINT('Ctrl Pts',(0.471405895547274,-0.145378763434889,
-1.24125728496997));
#69806=CARTESIAN_POINT('Ctrl Pts',(0.423298623249626,-0.301371641926843,
-1.24920667898938));
#69807=CARTESIAN_POINT('Ctrl Pts',(0.290078328670708,-0.431116172554822,
-1.25715607300879));
#69808=CARTESIAN_POINT('Ctrl Pts',(0.132868442861468,-0.475083655902993,
-1.2651054670282));
#69809=CARTESIAN_POINT('Ctrl Pts',(-0.0243414429477769,-0.519051139251165,
-1.27305486104761));
#69810=CARTESIAN_POINT('Ctrl Pts',(-0.205540919987342,-0.477241575319532,
-1.28100425506702));
#69811=CARTESIAN_POINT('Ctrl Pts',(-0.327593002437608,-0.368837807130042,
-1.28895364908643));
#69812=CARTESIAN_POINT('Ctrl Pts',(-0.430780670416379,-0.277188964971672,
-1.29567438186084));
#69813=CARTESIAN_POINT('Ctrl Pts',(-0.491691663072351,-0.137940704929582,
-1.30239511463524));
#69814=CARTESIAN_POINT('Ctrl Pts',(-0.492885109875619,0.000387266687590468,
-1.30911584740964));
#69815=CARTESIAN_POINT('Ctrl Pts',(-0.492797570805203,0.000412494226899228,
-1.33088415259036));
#69816=CARTESIAN_POINT('Ctrl Pts',(-0.491583335799359,-0.134947633181582,
-1.32431063997987));
#69817=CARTESIAN_POINT('Ctrl Pts',(-0.433611858386805,-0.271221502292443,
-1.31773712736938));
#69818=CARTESIAN_POINT('Ctrl Pts',(-0.334360120503988,-0.362714469445089,
-1.31116361475888));
#69819=CARTESIAN_POINT('Ctrl Pts',(-0.214334311124291,-0.473357544007792,
-1.30321422073947));
#69820=CARTESIAN_POINT('Ctrl Pts',(-0.0339392941143324,-0.518511991866373,
-1.29526482672006));
#69821=CARTESIAN_POINT('Ctrl Pts',(0.124057042802824,-0.477460288044243,
-1.28731543270065));
#69822=CARTESIAN_POINT('Ctrl Pts',(0.282053379719976,-0.436408584222115,
-1.27936603868124));
#69823=CARTESIAN_POINT('Ctrl Pts',(0.41765103654433,-0.309150728719275,
-1.27141664466183));
#69824=CARTESIAN_POINT('Ctrl Pts',(0.468635813451673,-0.1540744978209,-1.26346725064242));
#69825=CARTESIAN_POINT('Ctrl Pts',(0.519620590359018,0.00100173307748005,
-1.255517856623));
#69826=CARTESIAN_POINT('Ctrl Pts',(0.485992487349354,0.1838963393714,-1.24756846260359));
#69827=CARTESIAN_POINT('Ctrl Pts',(0.383180572810361,0.310694585001086,
-1.23961906858418));
#69828=CARTESIAN_POINT('Ctrl Pts',(0.280368658271367,0.437492830630774,
-1.23166967456477));
#69829=CARTESIAN_POINT('Ctrl Pts',(0.10837293220305,0.508194715596224,-1.22372028054536));
#69830=CARTESIAN_POINT('Ctrl Pts',(-0.0538924359234794,0.490361174929773,
-1.21577088652595));
#69831=CARTESIAN_POINT('Ctrl Pts',(-0.216157804050004,0.472527634263322,
-1.20782149250653));
#69832=CARTESIAN_POINT('Ctrl Pts',(-0.36869281423474,0.366158667964968,
-1.19987209848712));
#69833=CARTESIAN_POINT('Ctrl Pts',(-0.441512159754325,0.220057922641619,
-1.19192270446771));
#69834=CARTESIAN_POINT('Ctrl Pts',(-0.47521787875756,0.152432614656566,
-1.18824318717526));
#69835=CARTESIAN_POINT('Ctrl Pts',(-0.491844799023225,0.0762949137772939,
-1.18456366988281));
#69836=CARTESIAN_POINT('Ctrl Pts',(-0.491706700480042,0.000100130005186201,
-1.18088415259036));
#69837=CARTESIAN_POINT('Origin',(0.,0.,-1.725));
#69838=CARTESIAN_POINT('',(-0.492338823654994,-0.000448382455763341,-1.00911584740964));
#69839=CARTESIAN_POINT('',(-0.492429148680948,-0.000453349453110901,-1.03088415259036));
#69840=CARTESIAN_POINT('',(-0.4925,-6.03138548580071E-17,-1.725));
#69841=CARTESIAN_POINT('Ctrl Pts',(-0.492338823654994,-0.000448382455763341,
-1.00911584740964));
#69842=CARTESIAN_POINT('Ctrl Pts',(-0.491270535922525,0.120010930195667,
-1.01495178042171));
#69843=CARTESIAN_POINT('Ctrl Pts',(-0.446714827583699,0.241177295005307,
-1.02078771343378));
#69844=CARTESIAN_POINT('Ctrl Pts',(-0.366495740713805,0.330211107101538,
-1.02662364644585));
#69845=CARTESIAN_POINT('Ctrl Pts',(-0.257225615767691,0.451488176584551,
-1.03457304046526));
#69846=CARTESIAN_POINT('Ctrl Pts',(-0.0817841500725429,0.513145148861044,
-1.04252243448468));
#69847=CARTESIAN_POINT('Ctrl Pts',(0.0793335308670154,0.486892897971162,
-1.05047182850409));
#69848=CARTESIAN_POINT('Ctrl Pts',(0.240451211806571,0.460640647081281,
-1.0584212225235));
#69849=CARTESIAN_POINT('Ctrl Pts',(0.387245107990538,0.346479173025028,
-1.06637061654291));
#69850=CARTESIAN_POINT('Ctrl Pts',(0.452364020260708,0.196787439609733,
-1.07432001056232));
#69851=CARTESIAN_POINT('Ctrl Pts',(0.517482932530879,0.0470957061944376,
-1.08226940458173));
#69852=CARTESIAN_POINT('Ctrl Pts',(0.500926860887252,-0.138126286579906,
-1.09021879860114));
#69853=CARTESIAN_POINT('Ctrl Pts',(0.410291974568023,-0.273895963496465,
-1.09816819262056));
#69854=CARTESIAN_POINT('Ctrl Pts',(0.319657088248792,-0.409665640413027,
-1.10611758663997));
#69855=CARTESIAN_POINT('Ctrl Pts',(0.154943387253964,-0.495983001471805,
-1.11406698065938));
#69856=CARTESIAN_POINT('Ctrl Pts',(-0.00827605918009707,-0.493244371543186,
-1.12201637467879));
#69857=CARTESIAN_POINT('Ctrl Pts',(-0.171495505614156,-0.490505741614567,
-1.1299657686982));
#69858=CARTESIAN_POINT('Ctrl Pts',(-0.333220697487443,-0.398711120698549,
-1.13791516271761));
#69859=CARTESIAN_POINT('Ctrl Pts',(-0.419249737514621,-0.259977231327102,
-1.14586455673703));
#69860=CARTESIAN_POINT('Ctrl Pts',(-0.467051947884461,-0.182889464648957,
-1.1502816536279));
#69861=CARTESIAN_POINT('Ctrl Pts',(-0.491483033912735,-0.0913092376168913,
-1.15469875051877));
#69862=CARTESIAN_POINT('Ctrl Pts',(-0.491729663766022,0.000148572764139432,
-1.15911584740964));
#69863=CARTESIAN_POINT('Ctrl Pts',(-0.491706700480042,0.000100130005186201,
-1.18088415259036));
#69864=CARTESIAN_POINT('Ctrl Pts',(-0.491546444743027,-0.0883197109918345,
-1.1766142758634));
#69865=CARTESIAN_POINT('Ctrl Pts',(-0.468809875758622,-0.176816421647303,
-1.17234439913644));
#69866=CARTESIAN_POINT('Ctrl Pts',(-0.423987334998264,-0.252176954318478,
-1.16807452240948));
#69867=CARTESIAN_POINT('Ctrl Pts',(-0.340539483868178,-0.392478561606883,
-1.16012512839007));
#69868=CARTESIAN_POINT('Ctrl Pts',(-0.18054010075356,-0.487249251835348,
-1.15217573437065));
#69869=CARTESIAN_POINT('Ctrl Pts',(-0.0173992564916812,-0.493006838088287,
-1.14422634035124));
#69870=CARTESIAN_POINT('Ctrl Pts',(0.1457415877702,-0.498764424341226,-1.13627694633183));
#69871=CARTESIAN_POINT('Ctrl Pts',(0.312023893179346,-0.415508906618639,
-1.12832755231242));
#69872=CARTESIAN_POINT('Ctrl Pts',(0.405154891717245,-0.281439141282553,
-1.12037815829301));
#69873=CARTESIAN_POINT('Ctrl Pts',(0.498285890255143,-0.147369375946468,
-1.1124287642736));
#69874=CARTESIAN_POINT('Ctrl Pts',(0.518265581921795,0.0375146370031122,
-1.10447937025418));
#69875=CARTESIAN_POINT('Ctrl Pts',(0.455926990245143,0.188385392465231,
-1.09652997623477));
#69876=CARTESIAN_POINT('Ctrl Pts',(0.39358839856849,0.339256147927351,-1.08858058221536));
#69877=CARTESIAN_POINT('Ctrl Pts',(0.248931523548531,0.456113645902006,
-1.08063118819595));
#69878=CARTESIAN_POINT('Ctrl Pts',(0.0883270675941921,0.485341947144984,
-1.07268179417654));
#69879=CARTESIAN_POINT('Ctrl Pts',(-0.0722773883601444,0.514570248387963,
-1.06473240015713));
#69880=CARTESIAN_POINT('Ctrl Pts',(-0.248829425248864,0.456169352899263,
-1.05678300613772));
#69881=CARTESIAN_POINT('Ctrl Pts',(-0.360324371165323,0.336934450706051,
-1.0488336121183));
#69882=CARTESIAN_POINT('Ctrl Pts',(-0.444241628020003,0.247191675092816,
-1.04285045894232));
#69883=CARTESIAN_POINT('Ctrl Pts',(-0.491304697860191,0.122987047183034,
-1.03686730576634));
#69884=CARTESIAN_POINT('Ctrl Pts',(-0.492429148680948,-0.000453349453110901,
-1.03088415259036));
#69885=CARTESIAN_POINT('Origin',(0.,0.,-1.725));
#69886=CARTESIAN_POINT('',(-0.493300545452038,7.30209052610606E-5,-0.859115847409639));
#69887=CARTESIAN_POINT('',(-0.493273413985951,0.000128110117115081,-0.880884152590357));
#69888=CARTESIAN_POINT('',(-0.4925,-6.03138548580071E-17,-1.725));
#69889=CARTESIAN_POINT('Ctrl Pts',(-0.493300545452038,7.30209052610606E-5,
-0.859115847409639));
#69890=CARTESIAN_POINT('Ctrl Pts',(-0.493308612914771,0.00397858311580164,
-0.85930602228583));
#69891=CARTESIAN_POINT('Ctrl Pts',(-0.493266254174895,0.00788396578159667,
-0.859496197162021));
#69892=CARTESIAN_POINT('Ctrl Pts',(-0.493172934372577,0.0117881303439544,
-0.859686372038211));
#69893=CARTESIAN_POINT('Ctrl Pts',(-0.489272125320914,0.174983937510891,
-0.867635766057623));
#69894=CARTESIAN_POINT('Ctrl Pts',(-0.396328223367036,0.336051380543862,
-0.875585160077034));
#69895=CARTESIAN_POINT('Ctrl Pts',(-0.256985258091237,0.421090347002093,
-0.883534554096445));
#69896=CARTESIAN_POINT('Ctrl Pts',(-0.117642292815437,0.506129313460325,
-0.891483948115857));
#69897=CARTESIAN_POINT('Ctrl Pts',(0.0680997357822896,0.515139803343804,
-0.899433342135269));
#69898=CARTESIAN_POINT('Ctrl Pts',(0.215019652398866,0.443987671334291,
-0.90738273615468));
#69899=CARTESIAN_POINT('Ctrl Pts',(0.361939569015442,0.372835539324777,
-0.915332130174092));
#69900=CARTESIAN_POINT('Ctrl Pts',(0.470037373650875,0.221520785422272,
-0.923281524193504));
#69901=CARTESIAN_POINT('Ctrl Pts',(0.489716203234967,0.059468844815788,
-0.931230918212915));
#69902=CARTESIAN_POINT('Ctrl Pts',(0.509395032819059,-0.102583095790696,
-0.939180312232327));
#69903=CARTESIAN_POINT('Ctrl Pts',(0.44065488735181,-0.275372223101158,
-0.947129706251738));
#69904=CARTESIAN_POINT('Ctrl Pts',(0.315034756858612,-0.379620343482295,
-0.95507910027115));
#69905=CARTESIAN_POINT('Ctrl Pts',(0.189414626365416,-0.48386846386343,
-0.963028494290561));
#69906=CARTESIAN_POINT('Ctrl Pts',(0.00691451084627304,-0.519575577315242,
-0.970977888309973));
#69907=CARTESIAN_POINT('Ctrl Pts',(-0.148731851810166,-0.470358734873397,
-0.978927282329384));
#69908=CARTESIAN_POINT('Ctrl Pts',(-0.304378214466607,-0.421141892431551,
-0.986876676348796));
#69909=CARTESIAN_POINT('Ctrl Pts',(-0.433170824260342,-0.287001094096046,
-0.994826070368207));
#69910=CARTESIAN_POINT('Ctrl Pts',(-0.47601773705867,-0.129482111583526,
-1.00277546438762));
#69911=CARTESIAN_POINT('Ctrl Pts',(-0.487409206554715,-0.0876034191142425,
-1.00488892539496));
#69912=CARTESIAN_POINT('Ctrl Pts',(-0.492725700005788,-0.0440722656862921,
-1.0070023864023));
#69913=CARTESIAN_POINT('Ctrl Pts',(-0.492338823654994,-0.000448382455763341,
-1.00911584740964));
#69914=CARTESIAN_POINT('Ctrl Pts',(-0.492429148680948,-0.000453349453110901,
-1.03088415259036));
#69915=CARTESIAN_POINT('Ctrl Pts',(-0.492798676430811,-0.041019509545657,
-1.02891791174693));
#69916=CARTESIAN_POINT('Ctrl Pts',(-0.488206954099861,-0.0815031346698257,
-1.0269516709035));
#69917=CARTESIAN_POINT('Ctrl Pts',(-0.478331564969346,-0.120654011463565,
-1.02498543006007));
#69918=CARTESIAN_POINT('Ctrl Pts',(-0.438405957912708,-0.27893866254224,
-1.01703603604066));
#69919=CARTESIAN_POINT('Ctrl Pts',(-0.312116888855228,-0.415439055801866,
-1.00908664202125));
#69920=CARTESIAN_POINT('Ctrl Pts',(-0.157407640608445,-0.467526802660934,
-1.00113724800183));
#69921=CARTESIAN_POINT('Ctrl Pts',(-0.00269839236166527,-0.519614549520002,
-0.993187853982423));
#69922=CARTESIAN_POINT('Ctrl Pts',(0.180431035074421,-0.487289649978516,
-0.985238459963011));
#69923=CARTESIAN_POINT('Ctrl Pts',(0.307958166245391,-0.385383243500609,
-0.977289065943599));
#69924=CARTESIAN_POINT('Ctrl Pts',(0.435485297416365,-0.283476837022699,
-0.969339671924188));
#69925=CARTESIAN_POINT('Ctrl Pts',(0.507410132322223,-0.111988923608367,
-0.961390277904777));
#69926=CARTESIAN_POINT('Ctrl Pts',(0.490732498570953,0.0503993191877119,
-0.953440883885366));
#69927=CARTESIAN_POINT('Ctrl Pts',(0.474054864819683,0.212787561983789,
-0.945491489865954));
#69928=CARTESIAN_POINT('Ctrl Pts',(0.368774762411284,0.366076134161612,
-0.937542095846542));
#69929=CARTESIAN_POINT('Ctrl Pts',(0.223196251180912,0.439933983669209,
-0.92959270182713));
#69930=CARTESIAN_POINT('Ctrl Pts',(0.0776177399505409,0.513791833176806,
-0.921643307807718));
#69931=CARTESIAN_POINT('Ctrl Pts',(-0.108259180101798,0.50821896001418,
-0.913693913788307));
#69932=CARTESIAN_POINT('Ctrl Pts',(-0.249151443489066,0.425772280374832,
-0.905744519768896));
#69933=CARTESIAN_POINT('Ctrl Pts',(-0.390043706876331,0.343325600735486,
-0.897795125749484));
#69934=CARTESIAN_POINT('Ctrl Pts',(-0.485951313598522,0.184005114619417,
-0.889845731730073));
#69935=CARTESIAN_POINT('Ctrl Pts',(-0.492870442726711,0.0209094049332138,
-0.881896337710662));
#69936=CARTESIAN_POINT('Ctrl Pts',(-0.493164110375336,0.0139871560956824,
-0.88155894267056));
#69937=CARTESIAN_POINT('Ctrl Pts',(-0.493297474482374,0.00705810658322154,
-0.881221547630459));
#69938=CARTESIAN_POINT('Ctrl Pts',(-0.493273413985951,0.000128110117115081,
-0.880884152590357));
#69939=CARTESIAN_POINT('Origin',(0.,0.,-1.725));
#69940=CARTESIAN_POINT('',(-0.492120428308753,0.000409080293566094,-0.709115847409639));
#69941=CARTESIAN_POINT('',(-0.492044152078047,0.000384352874199066,-0.730884152590357));
#69942=CARTESIAN_POINT('',(-0.4925,-6.03138548580071E-17,-1.725));
#69943=CARTESIAN_POINT('Ctrl Pts',(-0.492120428308753,0.000409080293566094,
-0.709115847409639));
#69944=CARTESIAN_POINT('Ctrl Pts',(-0.492523321585198,0.0519416275023631,
-0.71160965816936));
#69945=CARTESIAN_POINT('Ctrl Pts',(-0.485074880445966,0.103360635220992,
-0.714103468929082));
#69946=CARTESIAN_POINT('Ctrl Pts',(-0.469287724172531,0.152077398581539,
-0.716597279688803));
#69947=CARTESIAN_POINT('Ctrl Pts',(-0.418963807181502,0.307369353191063,
-0.724546673708215));
#69948=CARTESIAN_POINT('Ctrl Pts',(-0.283909306830873,0.435203511586707,
-0.732496067727626));
#69949=CARTESIAN_POINT('Ctrl Pts',(-0.126089214777759,0.476927681237711,
-0.740445461747037));
#69950=CARTESIAN_POINT('Ctrl Pts',(0.0317308772753556,0.518651850888716,
-0.748394855766449));
#69951=CARTESIAN_POINT('Ctrl Pts',(0.212316561030953,0.474266031795081,
-0.756344249785862));
#69952=CARTESIAN_POINT('Ctrl Pts',(0.332812468065237,0.36413509074818,-0.764293643805273));
#69953=CARTESIAN_POINT('Ctrl Pts',(0.453308375099515,0.254004149701284,
-0.772243037824685));
#69954=CARTESIAN_POINT('Ctrl Pts',(0.513714505412483,0.078128086701122,
-0.780192431844096));
#69955=CARTESIAN_POINT('Ctrl Pts',(0.486315637735422,-0.0827985731104579,
-0.788141825863507));
#69956=CARTESIAN_POINT('Ctrl Pts',(0.45891677005836,-0.243725232922049,
-0.796091219882918));
#69957=CARTESIAN_POINT('Ctrl Pts',(0.343712904391259,-0.389702489545059,
-0.80404061390233));
#69958=CARTESIAN_POINT('Ctrl Pts',(0.193561269149825,-0.453753830066015,
-0.811990007921742));
#69959=CARTESIAN_POINT('Ctrl Pts',(0.0434096339083948,-0.517805170586969,
-0.819939401941154));
#69960=CARTESIAN_POINT('Ctrl Pts',(-0.141689770907357,-0.499930595005874,
-0.827888795960565));
#69961=CARTESIAN_POINT('Ctrl Pts',(-0.276810615240517,-0.408331221564878,
-0.835838189979976));
#69962=CARTESIAN_POINT('Ctrl Pts',(-0.408698937726213,-0.318923197484696,
-0.843597409123197));
#69963=CARTESIAN_POINT('Ctrl Pts',(-0.492971389400891,-0.159275646363948,
-0.851356628266418));
#69964=CARTESIAN_POINT('Ctrl Pts',(-0.493300545452038,7.30209052610606E-5,
-0.859115847409639));
#69965=CARTESIAN_POINT('Ctrl Pts',(-0.493273413985951,0.000128110117115081,
-0.880884152590357));
#69966=CARTESIAN_POINT('Ctrl Pts',(-0.492730583023898,-0.156220145656787,
-0.873272153611047));
#69967=CARTESIAN_POINT('Ctrl Pts',(-0.412058209599762,-0.313050403358555,
-0.865660154631737));
#69968=CARTESIAN_POINT('Ctrl Pts',(-0.284317021785768,-0.403140555701278,
-0.858048155652426));
#69969=CARTESIAN_POINT('Ctrl Pts',(-0.150913820182463,-0.49722387339321,
-0.850098761633015));
#69970=CARTESIAN_POINT('Ctrl Pts',(0.0338232345583237,-0.518519575520737,
-0.842149367613603));
#69971=CARTESIAN_POINT('Ctrl Pts',(0.185134063923977,-0.457256880651614,
-0.834199973594192));
#69972=CARTESIAN_POINT('Ctrl Pts',(0.33644489328963,-0.395994185782491,
-0.826250579574781));
#69973=CARTESIAN_POINT('Ctrl Pts',(0.454329497280149,-0.252173093916718,
-0.81830118555537));
#69974=CARTESIAN_POINT('Ctrl Pts',(0.484700685300486,-0.0917808378562355,
-0.810351791535958));
#69975=CARTESIAN_POINT('Ctrl Pts',(0.515071873320824,0.068611418204249,
-0.802402397516546));
#69976=CARTESIAN_POINT('Ctrl Pts',(0.457929645370978,0.245574838459443,
-0.794453003497134));
#69977=CARTESIAN_POINT('Ctrl Pts',(0.33949169629466,0.35791600226193,-0.786503609477722));
#69978=CARTESIAN_POINT('Ctrl Pts',(0.221053747218343,0.470257166064418,
-0.778554215458311));
#69979=CARTESIAN_POINT('Ctrl Pts',(0.0413200770155548,0.517976073414199,
-0.7706048214389));
#69980=CARTESIAN_POINT('Ctrl Pts',(-0.11724486223632,0.47917858759271,-0.762655427419488));
#69981=CARTESIAN_POINT('Ctrl Pts',(-0.275809801488195,0.440381101771221,
-0.754706033400077));
#69982=CARTESIAN_POINT('Ctrl Pts',(-0.413206009789156,0.315067222778461,
-0.746756639380665));
#69983=CARTESIAN_POINT('Ctrl Pts',(-0.466394085435827,0.16073280187724,
-0.738807245361253));
#69984=CARTESIAN_POINT('Ctrl Pts',(-0.484064784888934,0.109458204444321,
-0.736166214437621));
#69985=CARTESIAN_POINT('Ctrl Pts',(-0.492440836022914,0.0549804041547731,
-0.733525183513989));
#69986=CARTESIAN_POINT('Ctrl Pts',(-0.492044152078047,0.000384352874199066,
-0.730884152590357));
#69987=CARTESIAN_POINT('Origin',(0.,0.,-1.725));
#69988=CARTESIAN_POINT('',(-0.491829192176605,-0.000264117888597593,-0.559115847409639));
#69989=CARTESIAN_POINT('',(-0.491882295318969,-0.000303616531414571,-0.580884152590356));
#69990=CARTESIAN_POINT('',(-0.4925,-6.03138548580071E-17,-1.725));
#69991=CARTESIAN_POINT('Ctrl Pts',(-0.491829192176605,-0.000264117888597593,
-0.559115847409639));
#69992=CARTESIAN_POINT('Ctrl Pts',(-0.491347407742035,0.0990187616593992,
-0.563913294052891));
#69993=CARTESIAN_POINT('Ctrl Pts',(-0.462209103339611,0.198561720702376,
-0.568710740696144));
#69994=CARTESIAN_POINT('Ctrl Pts',(-0.406349763901535,0.27971123101388,
-0.573508187339396));
#69995=CARTESIAN_POINT('Ctrl Pts',(-0.313790548160828,0.414176391320723,
-0.581457581358807));
#69996=CARTESIAN_POINT('Ctrl Pts',(-0.147864289096749,0.498139280733203,
-0.589406975378218));
#69997=CARTESIAN_POINT('Ctrl Pts',(0.0152996038830409,0.493076490352761,
-0.597356369397629));
#69998=CARTESIAN_POINT('Ctrl Pts',(0.178463496862833,0.488013699972319,
-0.605305763417041));
#69999=CARTESIAN_POINT('Ctrl Pts',(0.338865023758333,0.393925229798948,
-0.613255157436453));
#70000=CARTESIAN_POINT('Ctrl Pts',(0.422909604609079,0.253980254149587,
-0.621204551455865));
#70001=CARTESIAN_POINT('Ctrl Pts',(0.506954185459824,0.114035278500226,
-0.629153945475276));
#70002=CARTESIAN_POINT('Ctrl Pts',(0.514641820265816,-0.0717662026251266,
-0.637103339494688));
#70003=CARTESIAN_POINT('Ctrl Pts',(0.442445308892405,-0.218175736228549,
-0.645052733514099));
#70004=CARTESIAN_POINT('Ctrl Pts',(0.370248797518995,-0.36458526983197,
-0.653002127533511));
#70005=CARTESIAN_POINT('Ctrl Pts',(0.21816813996618,-0.471602855913464,
-0.660951521552923));
#70006=CARTESIAN_POINT('Ctrl Pts',(0.0559801793831442,-0.490127251567516,
-0.668900915572334));
#70007=CARTESIAN_POINT('Ctrl Pts',(-0.106207781199894,-0.508651647221568,
-0.676850309591746));
#70008=CARTESIAN_POINT('Ctrl Pts',(-0.278503044813152,-0.43868285244818,
-0.684799703611157));
#70009=CARTESIAN_POINT('Ctrl Pts',(-0.381854009804069,-0.312323579649783,
-0.692749097630568));
#70010=CARTESIAN_POINT('Ctrl Pts',(-0.452782660856013,-0.225604575446169,
-0.698204680890258));
#70011=CARTESIAN_POINT('Ctrl Pts',(-0.491239039131227,-0.112326058403522,
-0.703660264149949));
#70012=CARTESIAN_POINT('Ctrl Pts',(-0.492120428308753,0.000409080293566094,
-0.709115847409639));
#70013=CARTESIAN_POINT('Ctrl Pts',(-0.492044152078047,0.000384352874199066,
-0.730884152590357));
#70014=CARTESIAN_POINT('Ctrl Pts',(-0.491246833729828,-0.109351455669271,
-0.725575789494578));
#70015=CARTESIAN_POINT('Ctrl Pts',(-0.455008244691688,-0.219564990411542,
-0.720267426398799));
#70016=CARTESIAN_POINT('Ctrl Pts',(-0.387566372929823,-0.30520613214935,
-0.714959063303019));
#70017=CARTESIAN_POINT('Ctrl Pts',(-0.286570641784764,-0.433455682465039,
-0.707009669283608));
#70018=CARTESIAN_POINT('Ctrl Pts',(-0.115599236502264,-0.506599820286735,
-0.699060275264196));
#70019=CARTESIAN_POINT('Ctrl Pts',(0.0469036468997333,-0.491078939107802,
-0.691110881244785));
#70020=CARTESIAN_POINT('Ctrl Pts',(0.209406530301733,-0.47555805792887,
-0.683161487225373));
#70021=CARTESIAN_POINT('Ctrl Pts',(0.363440891823226,-0.371372157749306,
-0.675212093205962));
#70022=CARTESIAN_POINT('Ctrl Pts',(0.438333500275854,-0.226323262321803,
-0.66726269918655));
#70023=CARTESIAN_POINT('Ctrl Pts',(0.513226108728484,-0.0812743668942985,
-0.659313305167138));
#70024=CARTESIAN_POINT('Ctrl Pts',(0.508976964112243,0.104637523781151,
-0.651363911147726));
#70025=CARTESIAN_POINT('Ctrl Pts',(0.427535636515494,0.246113299176732,
-0.643414517128314));
#70026=CARTESIAN_POINT('Ctrl Pts',(0.346094308918747,0.38758907457231,-0.635465123108903));
#70027=CARTESIAN_POINT('Ctrl Pts',(0.187460798341501,0.484628734688026,
-0.627515729089492));
#70028=CARTESIAN_POINT('Ctrl Pts',(0.0244184931561698,0.492709055851996,
-0.619566335070081));
#70029=CARTESIAN_POINT('Ctrl Pts',(-0.138623812029161,0.500789377015965,
-0.611616941050669));
#70030=CARTESIAN_POINT('Ctrl Pts',(-0.306074911822575,0.419910359228188,
-0.603667547031257));
#70031=CARTESIAN_POINT('Ctrl Pts',(-0.401105778050425,0.287180485702124,
-0.595718153011846));
#70032=CARTESIAN_POINT('Ctrl Pts',(-0.46021669502666,0.204620104578649,
-0.590773486204682));
#70033=CARTESIAN_POINT('Ctrl Pts',(-0.49130775347213,0.101998290745618,
-0.585828819397519));
#70034=CARTESIAN_POINT('Ctrl Pts',(-0.491882295318969,-0.000303616531414571,
-0.580884152590356));
#70035=CARTESIAN_POINT('Origin',(0.,0.,-1.725));
#70036=CARTESIAN_POINT('',(-0.493088042785032,-0.000296614551317576,-0.409115847409638));
#70037=CARTESIAN_POINT('',(-0.493153848081098,-0.000252729816838331,-0.430884152590357));
#70038=CARTESIAN_POINT('',(-0.4925,-6.03138548580071E-17,-1.725));
#70039=CARTESIAN_POINT('Ctrl Pts',(-0.493088042785032,-0.000296614551317576,
-0.409115847409638));
#70040=CARTESIAN_POINT('Ctrl Pts',(-0.492051112040595,0.145702757819977,
-0.416216929936422));
#70041=CARTESIAN_POINT('Ctrl Pts',(-0.42312608138996,0.292552439531534,
-0.423318012463205));
#70042=CARTESIAN_POINT('Ctrl Pts',(-0.309596575789553,0.384068313855645,
-0.430419094989988));
#70043=CARTESIAN_POINT('Ctrl Pts',(-0.18250457686648,0.486516882970195,
-0.438368489009399));
#70044=CARTESIAN_POINT('Ctrl Pts',(0.000485562329820693,0.51962135755884,
-0.446317883028811));
#70045=CARTESIAN_POINT('Ctrl Pts',(0.155415239341919,0.468192917728478,
-0.454267277048222));
#70046=CARTESIAN_POINT('Ctrl Pts',(0.310344916354022,0.416764477898114,
-0.462216671067634));
#70047=CARTESIAN_POINT('Ctrl Pts',(0.437214131181918,0.280803123648739,
-0.470166065087045));
#70048=CARTESIAN_POINT('Ctrl Pts',(0.477813439574123,0.122689924496489,
-0.478115459106457));
#70049=CARTESIAN_POINT('Ctrl Pts',(0.518412747966327,-0.035423274655759,
-0.486064853125868));
#70050=CARTESIAN_POINT('Ctrl Pts',(0.472742149922838,-0.215688318710885,
-0.49401424714528));
#70051=CARTESIAN_POINT('Ctrl Pts',(0.361755978352945,-0.335396953430194,
-0.501963641164691));
#70052=CARTESIAN_POINT('Ctrl Pts',(0.250769806783051,-0.455105588149505,
-0.509913035184103));
#70053=CARTESIAN_POINT('Ctrl Pts',(0.0744680616867539,-0.514257813533002,
-0.517862429203515));
#70054=CARTESIAN_POINT('Ctrl Pts',(-0.0862594177059559,-0.485713718354565,
-0.525811823222927));
#70055=CARTESIAN_POINT('Ctrl Pts',(-0.246986897098666,-0.457169623176128,
-0.533761217242338));
#70056=CARTESIAN_POINT('Ctrl Pts',(-0.392140110787785,-0.340929207435757,
-0.541710611261749));
#70057=CARTESIAN_POINT('Ctrl Pts',(-0.45512063142368,-0.190325283964967,
-0.549660005281161));
#70058=CARTESIAN_POINT('Ctrl Pts',(-0.480092508057637,-0.130610588698395,
-0.55281195265732));
#70059=CARTESIAN_POINT('Ctrl Pts',(-0.492145727053872,-0.0654934857084591,
-0.55596390003348));
#70060=CARTESIAN_POINT('Ctrl Pts',(-0.491829192176605,-0.000264117888597593,
-0.559115847409639));
#70061=CARTESIAN_POINT('Ctrl Pts',(-0.491882295318969,-0.000303616531414571,
-0.580884152590356));
#70062=CARTESIAN_POINT('Ctrl Pts',(-0.492231427341226,-0.0624694482543762,
-0.577879425378108));
#70063=CARTESIAN_POINT('Ctrl Pts',(-0.481311932613635,-0.124517150256906,
-0.57487469816586));
#70064=CARTESIAN_POINT('Ctrl Pts',(-0.458563585316289,-0.181873347975683,
-0.571869970953611));
#70065=CARTESIAN_POINT('Ctrl Pts',(-0.398379893692015,-0.333616578863071,
-0.5639205769342));
#70066=CARTESIAN_POINT('Ctrl Pts',(-0.255401877781181,-0.452522311373495,
-0.555971182914788));
#70067=CARTESIAN_POINT('Ctrl Pts',(-0.0952299543786173,-0.484034846183981,
-0.548021788895376));
#70068=CARTESIAN_POINT('Ctrl Pts',(0.0649419690239445,-0.515547380994467,
-0.540072394875965));
#70069=CARTESIAN_POINT('Ctrl Pts',(0.242307799918234,-0.459666718105021,
-0.532123000856554));
#70070=CARTESIAN_POINT('Ctrl Pts',(0.355489485052551,-0.342031727635589,
-0.524173606837142));
#70071=CARTESIAN_POINT('Ctrl Pts',(0.468671170186871,-0.224396737166155,
-0.516224212817731));
#70072=CARTESIAN_POINT('Ctrl Pts',(0.517668709561212,-0.0450074191167323,
-0.508274818798319));
#70073=CARTESIAN_POINT('Ctrl Pts',(0.48000131258373,0.113829768049986,-0.500325424778908));
#70074=CARTESIAN_POINT('Ctrl Pts',(0.442333915606249,0.272666955216704,
-0.492376030759496));
#70075=CARTESIAN_POINT('Ctrl Pts',(0.318001582276944,0.410952011500721,
-0.484426636740084));
#70076=CARTESIAN_POINT('Ctrl Pts',(0.164049813753438,0.465237719088328,
-0.476477242720673));
#70077=CARTESIAN_POINT('Ctrl Pts',(0.0100980452299302,0.519523426675936,
-0.468527848701261));
#70078=CARTESIAN_POINT('Ctrl Pts',(-0.173473158487775,0.489809785567135,
-0.46057845468185));
#70079=CARTESIAN_POINT('Ctrl Pts',(-0.302438623662206,0.389729850637384,
-0.452629060662438));
#70080=CARTESIAN_POINT('Ctrl Pts',(-0.42003006848778,0.298476396617569,
-0.445380757971745));
#70081=CARTESIAN_POINT('Ctrl Pts',(-0.492222869400628,0.148721136709646,
-0.438132455281051));
#70082=CARTESIAN_POINT('Ctrl Pts',(-0.493153848081098,-0.00025272981683833,
-0.430884152590357));
#70083=CARTESIAN_POINT('Origin',(0.,0.,-1.725));
#70084=CARTESIAN_POINT('',(-0.492748795109349,0.000423665976190507,-0.259115847409639));
#70085=CARTESIAN_POINT('',(-0.492657439364267,0.000439738527351781,-0.280884152590357));
#70086=CARTESIAN_POINT('',(-0.4925,-6.03138548580071E-17,-1.725));
#70087=CARTESIAN_POINT('Ctrl Pts',(-0.492748795109349,0.000423665976190507,
-0.259115847409639));
#70088=CARTESIAN_POINT('Ctrl Pts',(-0.493021314980458,0.0303989720533546,
-0.260571171800541));
#70089=CARTESIAN_POINT('Ctrl Pts',(-0.490521432313287,0.0603288797091717,
-0.262026496191444));
#70090=CARTESIAN_POINT('Ctrl Pts',(-0.485086207269442,0.0897158849497183,
-0.263481820582346));
#70091=CARTESIAN_POINT('Ctrl Pts',(-0.455397468643341,0.250236030951502,
-0.271431214601757));
#70092=CARTESIAN_POINT('Ctrl Pts',(-0.33812827529867,0.394557848344311,
-0.279380608621169));
#70093=CARTESIAN_POINT('Ctrl Pts',(-0.187080149952232,0.456464357226385,
-0.28733000264058));
#70094=CARTESIAN_POINT('Ctrl Pts',(-0.0360320246057905,0.51837086610846,
-0.295279396659992));
#70095=CARTESIAN_POINT('Ctrl Pts',(0.148795032742419,0.497862066479795,
-0.303228790679403));
#70096=CARTESIAN_POINT('Ctrl Pts',(0.282597925207516,0.404347700904736,
-0.311178184698815));
#70097=CARTESIAN_POINT('Ctrl Pts',(0.416400817672612,0.310833335329677,
-0.319127578718226));
#70098=CARTESIAN_POINT('Ctrl Pts',(0.499179545254594,0.144313403808224,
-0.327076972737638));
#70099=CARTESIAN_POINT('Ctrl Pts',(0.492954908135233,-0.0188103011477814,
-0.335026366757049));
#70100=CARTESIAN_POINT('Ctrl Pts',(0.486730271015873,-0.181934006103787,
-0.342975760776461));
#70101=CARTESIAN_POINT('Ctrl Pts',(0.391502269195169,-0.341661484494344,
-0.350925154795873));
#70102=CARTESIAN_POINT('Ctrl Pts',(0.250962442861246,-0.424707418399116,
-0.358874548815284));
#70103=CARTESIAN_POINT('Ctrl Pts',(0.110422616527323,-0.507753352303887,
-0.366823942834696));
#70104=CARTESIAN_POINT('Ctrl Pts',(-0.07542903431982,-0.514117741722873,
-0.374773336854107));
#70105=CARTESIAN_POINT('Ctrl Pts',(-0.221320794217617,-0.440880511665361,
-0.382722730873519));
#70106=CARTESIAN_POINT('Ctrl Pts',(-0.367212554115415,-0.367643281607849,
-0.39067212489293));
#70107=CARTESIAN_POINT('Ctrl Pts',(-0.473144423063867,-0.214804432073841,
-0.398621518912342));
#70108=CARTESIAN_POINT('Ctrl Pts',(-0.490513428213171,-0.0524886754866058,
-0.406570912931754));
#70109=CARTESIAN_POINT('Ctrl Pts',(-0.492366943921122,-0.0351673147122667,
-0.407419224424382));
#70110=CARTESIAN_POINT('Ctrl Pts',(-0.493211916893557,-0.0177380321143359,
-0.40826753591701));
#70111=CARTESIAN_POINT('Ctrl Pts',(-0.493088042785032,-0.000296614551317576,
-0.409115847409638));
#70112=CARTESIAN_POINT('Ctrl Pts',(-0.493153848081098,-0.00025272981683833,
-0.430884152590357));
#70113=CARTESIAN_POINT('Ctrl Pts',(-0.493243896897759,-0.014662211661654,
-0.430183061261639));
#70114=CARTESIAN_POINT('Ctrl Pts',(-0.492667241082679,-0.0290643830200086,
-0.429481969932921));
#70115=CARTESIAN_POINT('Ctrl Pts',(-0.491400476278679,-0.0434055967665068,
-0.428780878604204));
#70116=CARTESIAN_POINT('Ctrl Pts',(-0.477037137089573,-0.206014880489943,
-0.420831484584792));
#70117=CARTESIAN_POINT('Ctrl Pts',(-0.373950732080215,-0.360787219186121,
-0.412882090565381));
#70118=CARTESIAN_POINT('Ctrl Pts',(-0.229438802677289,-0.436710789854924,
-0.40493269654597));
#70119=CARTESIAN_POINT('Ctrl Pts',(-0.0849268732743565,-0.512634360523731,
-0.396983302526558));
#70120=CARTESIAN_POINT('Ctrl Pts',(0.101010580522155,-0.509709163165152,
-0.389033908507146));
#70121=CARTESIAN_POINT('Ctrl Pts',(0.243062685356905,-0.429277315683624,
-0.381084514487734));
#70122=CARTESIAN_POINT('Ctrl Pts',(0.385114790191649,-0.3488454682021,-0.373135120468323));
#70123=CARTESIAN_POINT('Ctrl Pts',(0.483281546064643,-0.190906970597636,
-0.365185726448912));
#70124=CARTESIAN_POINT('Ctrl Pts',(0.492522666606163,-0.027926340012255,
-0.3572363324295));
#70125=CARTESIAN_POINT('Ctrl Pts',(0.501763787147683,0.13505429057313,-0.349286938410089));
#70126=CARTESIAN_POINT('Ctrl Pts',(0.422079272357724,0.303077054139432,
-0.341337544390677));
#70127=CARTESIAN_POINT('Ctrl Pts',(0.290029424374363,0.399050655768452,
-0.333388150371265));
#70128=CARTESIAN_POINT('Ctrl Pts',(0.157979576391001,0.495024257397473,
-0.325438756351854));
#70129=CARTESIAN_POINT('Ctrl Pts',(-0.0264356047857588,0.518948697089211,
-0.317489362332442));
#70130=CARTESIAN_POINT('Ctrl Pts',(-0.178603480069354,0.45984704982415,
-0.309539968313031));
#70131=CARTESIAN_POINT('Ctrl Pts',(-0.330771355352949,0.40074540255909,
-0.301590574293619));
#70132=CARTESIAN_POINT('Ctrl Pts',(-0.450691924743376,0.258617668337232,
-0.293641180274208));
#70133=CARTESIAN_POINT('Ctrl Pts',(-0.48334432902377,0.0986742195455115,
-0.285691786254796));
#70134=CARTESIAN_POINT('Ctrl Pts',(-0.489926834879352,0.0664306922636456,
-0.284089241699983));
#70135=CARTESIAN_POINT('Ctrl Pts',(-0.492962774926304,0.0334631368774868,
-0.28248669714517));
#70136=CARTESIAN_POINT('Ctrl Pts',(-0.492657439364267,0.000439738527351781,
-0.280884152590357));
#70137=CARTESIAN_POINT('Origin',(0.,0.,-1.725));
#70138=CARTESIAN_POINT('',(-0.491761526237315,7.34498668767403E-5,-0.109115847409639));
#70139=CARTESIAN_POINT('',(-0.491698555522654,2.49815306513942E-5,-0.130884152590357));
#70140=CARTESIAN_POINT('',(-0.4925,-6.03138548580071E-17,-1.725));
#70141=CARTESIAN_POINT('Ctrl Pts',(-0.491761526237315,7.34498668767403E-5,
-0.109115847409639));
#70142=CARTESIAN_POINT('Ctrl Pts',(-0.491825690633276,0.0779166216940231,
-0.112874807684072));
#70143=CARTESIAN_POINT('Ctrl Pts',(-0.474387552418018,0.155716209514715,
-0.116633767958505));
#70144=CARTESIAN_POINT('Ctrl Pts',(-0.439245516028347,0.224454403316697,
-0.120392728232938));
#70145=CARTESIAN_POINT('Ctrl Pts',(-0.364927653238976,0.369820926722449,
-0.12834212225235));
#70146=CARTESIAN_POINT('Ctrl Pts',(-0.211432346318084,0.474662023942289,
-0.136291516271761));
#70147=CARTESIAN_POINT('Ctrl Pts',(-0.049019555660165,0.490874829170351,
-0.144240910291172));
#70148=CARTESIAN_POINT('Ctrl Pts',(0.113393234997754,0.507087634398413,
-0.152190304310584));
#70149=CARTESIAN_POINT('Ctrl Pts',(0.284723509392699,0.434672147634697,
-0.160139698329996));
#70150=CARTESIAN_POINT('Ctrl Pts',(0.38627620605837,0.306853825701618,-0.168089092349407));
#70151=CARTESIAN_POINT('Ctrl Pts',(0.48782890272404,0.17903550376854,-0.176038486368819));
#70152=CARTESIAN_POINT('Ctrl Pts',(0.519604021660437,-0.00418565333390042,
-0.18398788038823));
#70153=CARTESIAN_POINT('Ctrl Pts',(0.46706756334537,-0.158745174957354,
-0.191937274407642));
#70154=CARTESIAN_POINT('Ctrl Pts',(0.414531105030304,-0.313304696580808,
-0.199886668427054));
#70155=CARTESIAN_POINT('Ctrl Pts',(0.277683069463775,-0.439202582725276,
-0.207836062446465));
#70156=CARTESIAN_POINT('Ctrl Pts',(0.119287960412537,-0.478674982698152,
-0.215785456465877));
#70157=CARTESIAN_POINT('Ctrl Pts',(-0.039107148638701,-0.518147382671028,
-0.223734850485288));
#70158=CARTESIAN_POINT('Ctrl Pts',(-0.219049331174648,-0.471194296472313,
-0.2316842445047));
#70159=CARTESIAN_POINT('Ctrl Pts',(-0.337966280488859,-0.359358516067573,
-0.239633638524111));
#70160=CARTESIAN_POINT('Ctrl Pts',(-0.435112672650402,-0.267996917544017,
-0.24612770815262));
#70161=CARTESIAN_POINT('Ctrl Pts',(-0.491532734257764,-0.133334639744414,
-0.25262177778113));
#70162=CARTESIAN_POINT('Ctrl Pts',(-0.492748795109349,0.000423665976190507,
-0.259115847409639));
#70163=CARTESIAN_POINT('Ctrl Pts',(-0.492657439364267,0.000439738527351781,
-0.280884152590357));
#70164=CARTESIAN_POINT('Ctrl Pts',(-0.491448163252337,-0.130348848603208,
-0.274537303125758));
#70165=CARTESIAN_POINT('Ctrl Pts',(-0.437829573728453,-0.262013356113694,
-0.26819045366116));
#70166=CARTESIAN_POINT('Ctrl Pts',(-0.344554674086439,-0.353044898970412,
-0.261843604196561));
#70167=CARTESIAN_POINT('Ctrl Pts',(-0.227728375698354,-0.467061405333034,
-0.25389421017715));
#70168=CARTESIAN_POINT('Ctrl Pts',(-0.0486915397518234,-0.517335254696698,
-0.245944816157738));
#70169=CARTESIAN_POINT('Ctrl Pts',(0.110409397431204,-0.480799781899208,
-0.237995422138326));
#70170=CARTESIAN_POINT('Ctrl Pts',(0.269510334614231,-0.444264309101718,
-0.230046028118915));
#70171=CARTESIAN_POINT('Ctrl Pts',(0.408675373033755,-0.320919514143075,
-0.222096634099504));
#70172=CARTESIAN_POINT('Ctrl Pts',(0.46405681172168,-0.167358347485203,
-0.214147240080092));
#70173=CARTESIAN_POINT('Ctrl Pts',(0.519438250409602,-0.0137971808273366,
-0.206197846060681));
#70174=CARTESIAN_POINT('Ctrl Pts',(0.491036089365932,0.169980357529756,
-0.198248452041269));
#70175=CARTESIAN_POINT('Ctrl Pts',(0.391875390863108,0.299655473021211,
-0.190299058021858));
#70176=CARTESIAN_POINT('Ctrl Pts',(0.292714692360281,0.429330588512671,
-0.182349664002446));
#70177=CARTESIAN_POINT('Ctrl Pts',(0.122795456398295,0.50490328113849,-0.174400269983035));
#70178=CARTESIAN_POINT('Ctrl Pts',(-0.0399088460306932,0.491697684968673,
-0.166450875963623));
#70179=CARTESIAN_POINT('Ctrl Pts',(-0.202613148459681,0.478492088798855,
-0.158501481944212));
#70180=CARTESIAN_POINT('Ctrl Pts',(-0.358102517355672,0.376508203833402,
-0.1505520879248));
#70181=CARTESIAN_POINT('Ctrl Pts',(-0.435059219194714,0.232541579850291,
-0.142602693905388));
#70182=CARTESIAN_POINT('Ctrl Pts',(-0.472874273095562,0.161799129670568,
-0.138696513467045));
#70183=CARTESIAN_POINT('Ctrl Pts',(-0.491727206546983,0.0809197290486493,
-0.134790333028701));
#70184=CARTESIAN_POINT('Ctrl Pts',(-0.491698555522654,2.49815306513942E-5,
-0.130884152590357));
#70185=CARTESIAN_POINT('Origin',(0.,0.,-3.73478126690739));
#70186=CARTESIAN_POINT('',(-0.40643965330944,6.07061285855456E-5,-0.0597812669073879));
#70187=CARTESIAN_POINT('',(-0.406892273398771,-0.000115106065058088,-0.0302187330926113));
#70188=CARTESIAN_POINT('',(-0.40705,-1.06687458785308E-14,-3.73478126690739));
#70189=CARTESIAN_POINT('',(-0.0460018146225333,-0.405020972964472,-0.0249999999999997));
#70190=CARTESIAN_POINT('Ctrl Pts',(-0.40643965330944,6.07061285855248E-5,
-0.0597812669073879));
#70191=CARTESIAN_POINT('Ctrl Pts',(-0.406380534337011,-0.0716614422772074,
-0.0555908331624084));
#70192=CARTESIAN_POINT('Ctrl Pts',(-0.356479421834089,-0.270220379709696,
-0.0439970775266123));
#70193=CARTESIAN_POINT('Ctrl Pts',(-0.170735417371495,-0.390082040693776,
-0.0324033218908163));
#70194=CARTESIAN_POINT('Ctrl Pts',(-0.0460018146225332,-0.405020972964472,
-0.0249999999999997));
#70195=CARTESIAN_POINT('',(-0.39736287274916,-0.0882748540669144,-0.0249999999999999));
#70196=CARTESIAN_POINT('Origin',(0.,0.,-0.0249999999999999));
#70197=CARTESIAN_POINT('Ctrl Pts',(-0.406892273398771,-0.000115106065058105,
-0.0302187330926113));
#70198=CARTESIAN_POINT('Ctrl Pts',(-0.406947232354318,-0.029718523814811,
-0.0284791553950742));
#70199=CARTESIAN_POINT('Ctrl Pts',(-0.40379521950949,-0.0593201102248456,
-0.0267395776975371));
#70200=CARTESIAN_POINT('Ctrl Pts',(-0.39736287274916,-0.0882748540669144,
-0.0249999999999999));
#70201=CARTESIAN_POINT('Origin',(0.,0.,-3.73478126690739));
#70202=CARTESIAN_POINT('',(-0.407255628526418,0.000350158854048321,-0.209781266907387));
#70203=CARTESIAN_POINT('',(-0.406387608173597,2.06471716764911E-5,-0.180218733092611));
#70204=CARTESIAN_POINT('',(-0.40705,-1.06687458785308E-14,-3.73478126690739));
#70205=CARTESIAN_POINT('Ctrl Pts',(-0.407255628526418,0.000350158854048318,
-0.209781266907387));
#70206=CARTESIAN_POINT('Ctrl Pts',(-0.406250557319037,-0.110200741335954,
-0.203287197278877));
#70207=CARTESIAN_POINT('Ctrl Pts',(-0.302538442003538,-0.357738749730799,
-0.188843733630956));
#70208=CARTESIAN_POINT('Ctrl Pts',(0.116399798066751,-0.467054103255692,
-0.166450875963623));
#70209=CARTESIAN_POINT('Ctrl Pts',(0.45571346026384,-0.154891253173831,
-0.142602693905389));
#70210=CARTESIAN_POINT('Ctrl Pts',(0.376927294803572,0.299404210776717,
-0.118754511847154));
#70211=CARTESIAN_POINT('Ctrl Pts',(-0.0478848160134567,0.478957858820396,
-0.094906329788919));
#70212=CARTESIAN_POINT('Ctrl Pts',(-0.361600601784404,0.264682205348061,
-0.075248581475664));
#70213=CARTESIAN_POINT('Ctrl Pts',(-0.406492685019843,0.0643978900722083,
-0.0635402271818201));
#70214=CARTESIAN_POINT('Ctrl Pts',(-0.40643965330944,6.07061285855248E-5,
-0.0597812669073879));
#70215=CARTESIAN_POINT('Ctrl Pts',(-0.406387608173597,2.06471716765189E-5,
-0.180218733092611));
#70216=CARTESIAN_POINT('Ctrl Pts',(-0.406363097454078,-0.069184154866318,
-0.176175519511543));
#70217=CARTESIAN_POINT('Ctrl Pts',(-0.356697934417019,-0.27449337105559,
-0.164182911911064));
#70218=CARTESIAN_POINT('Ctrl Pts',(-0.0305910094676718,-0.480372488794092,
-0.144240910291172));
#70219=CARTESIAN_POINT('Ctrl Pts',(0.387186688863383,-0.285728547318658,
-0.120392728232938));
#70220=CARTESIAN_POINT('Ctrl Pts',(0.450204815655376,0.171019861124231,
-0.0965445461747034));
#70221=CARTESIAN_POINT('Ctrl Pts',(0.0990560712614088,0.471004678905531,
-0.0726963641164688));
#70222=CARTESIAN_POINT('Ctrl Pts',(-0.267488470034939,0.360553837565826,
-0.0528228790679404));
#70223=CARTESIAN_POINT('Ctrl Pts',(-0.391916341648465,0.143605734703497,
-0.038663668726654));
#70224=CARTESIAN_POINT('Ctrl Pts',(-0.406821658661013,0.0379212350609192,
-0.0324538524047797));
#70225=CARTESIAN_POINT('Ctrl Pts',(-0.406892273398771,-0.000115106065058105,
-0.0302187330926113));
#70226=CARTESIAN_POINT('Origin',(0.,0.,-3.73478126690739));
#70227=CARTESIAN_POINT('',(-0.407536015869335,-0.000245151173813718,-0.359781266907386));
#70228=CARTESIAN_POINT('',(-0.407180123234974,0.000363442776755235,-0.33021873309261));
#70229=CARTESIAN_POINT('',(-0.40705,-1.06687458785308E-14,-3.73478126690739));
#70230=CARTESIAN_POINT('Ctrl Pts',(-0.407536015869335,-0.000245151173813667,
-0.359781266907386));
#70231=CARTESIAN_POINT('Ctrl Pts',(-0.40763839750563,-0.0146604385220988,
-0.358932955414758));
#70232=CARTESIAN_POINT('Ctrl Pts',(-0.400395732273573,-0.164055109369366,
-0.350135249902717));
#70233=CARTESIAN_POINT('Ctrl Pts',(-0.215947823141546,-0.43017716036811,
-0.333388150371265));
#70234=CARTESIAN_POINT('Ctrl Pts',(0.244869930019852,-0.41439670526355,
-0.309539968313031));
#70235=CARTESIAN_POINT('Ctrl Pts',(0.480987035447976,-0.0183536387932365,
-0.285691786254796));
#70236=CARTESIAN_POINT('Ctrl Pts',(0.275737810703329,0.394531263495945,
-0.261843604196561));
#70237=CARTESIAN_POINT('Ctrl Pts',(-0.182539470678933,0.445382676016845,
-0.237995422138327));
#70238=CARTESIAN_POINT('Ctrl Pts',(-0.394128840463536,0.184982126500309,
-0.220641309708602));
#70239=CARTESIAN_POINT('Ctrl Pts',(-0.407480865508213,0.0251246732473596,
-0.211236591298289));
#70240=CARTESIAN_POINT('Ctrl Pts',(-0.407255628526418,0.000350158854048318,
-0.209781266907387));
#70241=CARTESIAN_POINT('Ctrl Pts',(-0.407180123234974,0.000363442776755221,
-0.33021873309261));
#70242=CARTESIAN_POINT('Ctrl Pts',(-0.406180659597689,-0.10773299253592,
-0.323871883628011));
#70243=CARTESIAN_POINT('Ctrl Pts',(-0.306359951108232,-0.352850302396471,
-0.309575640144001));
#70244=CARTESIAN_POINT('Ctrl Pts',(0.107730056479299,-0.469127483873643,
-0.28733000264058));
#70245=CARTESIAN_POINT('Ctrl Pts',(0.452788709608233,-0.16329500394726,
-0.263481820582346));
#70246=CARTESIAN_POINT('Ctrl Pts',(0.382365767560564,0.292380003087804,
-0.239633638524111));
#70247=CARTESIAN_POINT('Ctrl Pts',(-0.0389476842058911,0.479761919026928,
-0.215785456465877));
#70248=CARTESIAN_POINT('Ctrl Pts',(-0.359118952835858,0.269764862243941,
-0.195980487988709));
#70249=CARTESIAN_POINT('Ctrl Pts',(-0.406411288172487,0.0668799506786837,
-0.184124913530954));
#70250=CARTESIAN_POINT('Ctrl Pts',(-0.406387608173597,2.06471716765189E-5,
-0.180218733092611));
#70251=CARTESIAN_POINT('Origin',(0.,0.,-3.73478126690739));
#70252=CARTESIAN_POINT('',(-0.406495579036522,-0.000218292764554502,-0.509781266907387));
#70253=CARTESIAN_POINT('',(-0.407590403779514,-0.000208880552183932,-0.48021873309261));
#70254=CARTESIAN_POINT('',(-0.40705,-1.06687458785308E-14,-3.73478126690739));
#70255=CARTESIAN_POINT('Ctrl Pts',(-0.406495579036522,-0.000218292764554491,
-0.509781266907387));
#70256=CARTESIAN_POINT('Ctrl Pts',(-0.406757194309198,-0.0541301997109065,
-0.506629319531227));
#70257=CARTESIAN_POINT('Ctrl Pts',(-0.37167061156908,-0.243684261789019,
-0.495527978135656));
#70258=CARTESIAN_POINT('Ctrl Pts',(-0.0841652808768616,-0.473921941809059,
-0.476477242720672));
#70259=CARTESIAN_POINT('Ctrl Pts',(0.352973553690336,-0.327254449368329,
-0.452629060662438));
#70260=CARTESIAN_POINT('Ctrl Pts',(0.466213453793493,0.119711354789871,
-0.428780878604203));
#70261=CARTESIAN_POINT('Ctrl Pts',(0.151642201636973,0.456826497412456,
-0.404932696545969));
#70262=CARTESIAN_POINT('Ctrl Pts',(-0.285940937986012,0.377663980843574,
-0.381932825980363));
#70263=CARTESIAN_POINT('Ctrl Pts',(-0.406678995240854,0.120422959534271,
-0.366882349434169));
#70264=CARTESIAN_POINT('Ctrl Pts',(-0.407536015869335,-0.000245151173813667,
-0.359781266907386));
#70265=CARTESIAN_POINT('Ctrl Pts',(-0.407590403779514,-0.000208880552183977,
-0.48021873309261));
#70266=CARTESIAN_POINT('Ctrl Pts',(-0.407664828897934,-0.0121182807246313,
-0.479517641763892));
#70267=CARTESIAN_POINT('Ctrl Pts',(-0.401784195862354,-0.158989052611827,
-0.470867156415763));
#70268=CARTESIAN_POINT('Ctrl Pts',(-0.223868678851143,-0.426108666062932,
-0.454267277048223));
#70269=CARTESIAN_POINT('Ctrl Pts',(0.23716182206986,-0.418855661485411,
-0.430419094989988));
#70270=CARTESIAN_POINT('Ctrl Pts',(0.48056554579435,-0.0272483592525269,
-0.406570912931754));
#70271=CARTESIAN_POINT('Ctrl Pts',(0.282988398107527,0.389362803648974,
-0.382722730873519));
#70272=CARTESIAN_POINT('Ctrl Pts',(-0.174267639443746,0.448683269698852,
-0.358874548815284));
#70273=CARTESIAN_POINT('Ctrl Pts',(-0.392476459337574,0.190066042342598,
-0.341373216221648));
#70274=CARTESIAN_POINT('Ctrl Pts',(-0.407432482302036,0.0276571976974138,
-0.331821277647423));
#70275=CARTESIAN_POINT('Ctrl Pts',(-0.407180123234974,0.000363442776755221,
-0.33021873309261));
#70276=CARTESIAN_POINT('Origin',(0.,0.,-3.73478126690739));
#70277=CARTESIAN_POINT('',(-0.406736284960564,0.000338103824355545,-0.659781266907385));
#70278=CARTESIAN_POINT('',(-0.406539468648906,-0.000250938292638919,-0.630218733092608));
#70279=CARTESIAN_POINT('',(-0.40705,-1.06687458785308E-14,-3.73478126690739));
#70280=CARTESIAN_POINT('Ctrl Pts',(-0.406736284960564,0.000338103824355524,
-0.659781266907385));
#70281=CARTESIAN_POINT('Ctrl Pts',(-0.406007819042367,-0.0928372021789944,
-0.654325683647695));
#70282=CARTESIAN_POINT('Ctrl Pts',(-0.327910738459151,-0.322882824533624,
-0.640920706368594));
#70283=CARTESIAN_POINT('Ctrl Pts',(0.0546211364799233,-0.47822832672903,
-0.61956633507008));
#70284=CARTESIAN_POINT('Ctrl Pts',(0.431703968907574,-0.212879036894682,
-0.595718153011845));
#70285=CARTESIAN_POINT('Ctrl Pts',(0.412642536941405,0.247814320823537,
-0.571869970953611));
#70286=CARTESIAN_POINT('Ctrl Pts',(0.0149281723354398,0.481105966208734,
-0.548021788895376));
#70287=CARTESIAN_POINT('Ctrl Pts',(-0.342109434348876,0.300435894725022,
-0.527325554213302));
#70288=CARTESIAN_POINT('Ctrl Pts',(-0.406097385424149,0.0818387551948536,
-0.514578713550639));
#70289=CARTESIAN_POINT('Ctrl Pts',(-0.406495579036522,-0.000218292764554491,
-0.509781266907387));
#70290=CARTESIAN_POINT('Ctrl Pts',(-0.406539468648906,-0.000250938292638857,
-0.630218733092608));
#70291=CARTESIAN_POINT('Ctrl Pts',(-0.406828025379177,-0.0516308404303603,
-0.62721400588036));
#70292=CARTESIAN_POINT('Ctrl Pts',(-0.373926460083483,-0.238586974373572,
-0.616259884648701));
#70293=CARTESIAN_POINT('Ctrl Pts',(-0.0929180364960938,-0.472283827945071,
-0.59735636939763));
#70294=CARTESIAN_POINT('Ctrl Pts',(0.346859190705059,-0.333728149797965,
-0.573508187339396));
#70295=CARTESIAN_POINT('Ctrl Pts',(0.468348216506024,0.11106629839706,-0.549660005281161));
#70296=CARTESIAN_POINT('Ctrl Pts',(0.160067142708905,0.453943042521375,
-0.525811823222927));
#70297=CARTESIAN_POINT('Ctrl Pts',(-0.281715318279609,0.382434193485541,
-0.502664732493409));
#70298=CARTESIAN_POINT('Ctrl Pts',(-0.406820952263001,0.122917642025699,
-0.487467035783304));
#70299=CARTESIAN_POINT('Ctrl Pts',(-0.407590403779514,-0.000208880552183977,
-0.48021873309261));
#70300=CARTESIAN_POINT('Origin',(0.,0.,-3.73478126690739));
#70301=CARTESIAN_POINT('',(-0.407711648784268,6.03515928581689E-5,-0.809781266907385));
#70302=CARTESIAN_POINT('',(-0.40667324284948,0.000317666674979761,-0.780218733092609));
#70303=CARTESIAN_POINT('',(-0.40705,-1.06687458785308E-14,-3.73478126690739));
#70304=CARTESIAN_POINT('Ctrl Pts',(-0.407711648784268,6.03515928581763E-5,
-0.809781266907385));
#70305=CARTESIAN_POINT('Ctrl Pts',(-0.407439602143414,-0.131640917466901,
-0.802022047764164));
#70306=CARTESIAN_POINT('Ctrl Pts',(-0.266430554273655,-0.398771500841622,
-0.786313434601533));
#70307=CARTESIAN_POINT('Ctrl Pts',(0.188862140533343,-0.442737950614639,
-0.762655427419487));
#70308=CARTESIAN_POINT('Ctrl Pts',(0.474509248268113,-0.0807884543198489,
-0.738807245361255));
#70309=CARTESIAN_POINT('Ctrl Pts',(0.324732708102262,0.355294904731216,
-0.714959063303019));
#70310=CARTESIAN_POINT('Ctrl Pts',(-0.123028119751846,0.465349205210794,
-0.691110881244784));
#70311=CARTESIAN_POINT('Ctrl Pts',(-0.381289613521448,0.220894998825026,
-0.67271828244624));
#70312=CARTESIAN_POINT('Ctrl Pts',(-0.407069275230974,0.0429296232991591,
-0.662275077667107));
#70313=CARTESIAN_POINT('Ctrl Pts',(-0.406736284960564,0.000338103824355524,
-0.659781266907385));
#70314=CARTESIAN_POINT('Ctrl Pts',(-0.40667324284948,0.000317666674979726,
-0.780218733092608));
#70315=CARTESIAN_POINT('Ctrl Pts',(-0.406014261258321,-0.0903787005689077,
-0.77491036999683));
#70316=CARTESIAN_POINT('Ctrl Pts',(-0.331210705683951,-0.317881053446477,
-0.76165261288164));
#70317=CARTESIAN_POINT('Ctrl Pts',(0.0457649569583762,-0.479156909945254,
-0.740445461747037));
#70318=CARTESIAN_POINT('Ctrl Pts',(0.427691983500448,-0.220828763743674,
-0.716597279688803));
#70319=CARTESIAN_POINT('Ctrl Pts',(0.417156261778369,0.240138353613306,
-0.692749097630569));
#70320=CARTESIAN_POINT('Ctrl Pts',(0.0238256801714527,0.480747451989572,
-0.668900915572333));
#70321=CARTESIAN_POINT('Ctrl Pts',(-0.339056139434653,0.305475237122115,
-0.648057460726347));
#70322=CARTESIAN_POINT('Ctrl Pts',(-0.406064611270727,0.0843013284223252,
-0.635163399899772));
#70323=CARTESIAN_POINT('Ctrl Pts',(-0.406539468648906,-0.000250938292638857,
-0.630218733092608));
#70324=CARTESIAN_POINT('Origin',(0.,0.,-3.73478126690739));
#70325=CARTESIAN_POINT('',(-0.406916788159929,-0.000370586961657899,-0.959781266907386));
#70326=CARTESIAN_POINT('',(-0.407689224696409,0.000105882686618278,-0.930218733092609));
#70327=CARTESIAN_POINT('',(-0.40705,-1.06687458785308E-14,-3.73478126690739));
#70328=CARTESIAN_POINT('Ctrl Pts',(-0.406916788159929,-0.000370586961657902,
-0.959781266907386));
#70329=CARTESIAN_POINT('Ctrl Pts',(-0.407236540481942,-0.0364256157311761,
-0.957667805900046));
#70330=CARTESIAN_POINT('Ctrl Pts',(-0.386314993991867,-0.207730077702373,
-0.947604950873294));
#70331=CARTESIAN_POINT('Ctrl Pts',(-0.145121056613384,-0.458939734572041,
-0.92959270182713));
#70332=CARTESIAN_POINT('Ctrl Pts',(0.307386590221547,-0.370404218649844,
-0.905744519768897));
#70333=CARTESIAN_POINT('Ctrl Pts',(0.477827257505465,0.0580251068631922,
-0.88189633771066));
#70334=CARTESIAN_POINT('Ctrl Pts',(0.209799573991638,0.433208887021656,
-0.858048155652426));
#70335=CARTESIAN_POINT('Ctrl Pts',(-0.250746371636999,0.410867445963362,
-0.834199973594193));
#70336=CARTESIAN_POINT('Ctrl Pts',(-0.406219899087611,0.141439081117942,
-0.818111010679178));
#70337=CARTESIAN_POINT('Ctrl Pts',(-0.407718316521741,0.00328828884727744,
-0.809971441783576));
#70338=CARTESIAN_POINT('Ctrl Pts',(-0.407711648784268,6.03515928581763E-5,
-0.809781266907385));
#70339=CARTESIAN_POINT('Ctrl Pts',(-0.407689224696409,0.000105882686618259,
-0.930218733092609));
#70340=CARTESIAN_POINT('Ctrl Pts',(-0.407240576284007,-0.129115553887518,
-0.9226067341133));
#70341=CARTESIAN_POINT('Ctrl Pts',(-0.270934220145519,-0.394100455809237,
-0.907045341114577));
#70342=CARTESIAN_POINT('Ctrl Pts',(0.180639524384169,-0.446155956886755,
-0.883534554096447));
#70343=CARTESIAN_POINT('Ctrl Pts',(0.472933502380155,-0.0895526546900201,
-0.85968637203821));
#70344=CARTESIAN_POINT('Ctrl Pts',(0.331249783271615,0.34922679839552,-0.835838189979976));
#70345=CARTESIAN_POINT('Ctrl Pts',(-0.114398483465715,0.467545465827366,
-0.811990007921742));
#70346=CARTESIAN_POINT('Ctrl Pts',(-0.379241019134891,0.225992617481762,
-0.793450188959285));
#70347=CARTESIAN_POINT('Ctrl Pts',(-0.407001101123104,0.0454411644897258,
-0.782859764016241));
#70348=CARTESIAN_POINT('Ctrl Pts',(-0.40667324284948,0.000317666674979726,
-0.780218733092608));
#70349=CARTESIAN_POINT('Origin',(0.,0.,-3.73478126690739));
#70350=CARTESIAN_POINT('',(-0.406413319057786,0.000122795012471166,-1.10978126690739));
#70351=CARTESIAN_POINT('',(-0.40699144156463,-0.000374692172387947,-1.08021873309261));
#70352=CARTESIAN_POINT('',(-0.40705,-1.06687458785308E-14,-3.73478126690739));
#70353=CARTESIAN_POINT('Ctrl Pts',(-0.406413319057786,0.000122795012471158,
-1.10978126690739));
#70354=CARTESIAN_POINT('Ctrl Pts',(-0.406209480110007,-0.0754668531410285,
-1.10536417001651));
#70355=CARTESIAN_POINT('Ctrl Pts',(-0.34967754470652,-0.287377509622766,
-1.09299767910623));
#70356=CARTESIAN_POINT('Ctrl Pts',(-0.0080751395090761,-0.481269771711826,
-1.07268179417654));
#70357=CARTESIAN_POINT('Ctrl Pts',(0.400331227942373,-0.26724653220537,
-1.0488336121183));
#70358=CARTESIAN_POINT('Ctrl Pts',(0.441381881521284,0.192009988558863,
-1.02498543006007));
#70359=CARTESIAN_POINT('Ctrl Pts',(0.0774075336531558,0.475072494231541,
-1.00113724800183));
#70360=CARTESIAN_POINT('Ctrl Pts',(-0.319047392123228,0.335742773799606,
-0.97940252695094));
#70361=CARTESIAN_POINT('Ctrl Pts',(-0.406033851060433,0.0991887292104516,
-0.965617199919458));
#70362=CARTESIAN_POINT('Ctrl Pts',(-0.406916788159929,-0.000370586961657902,
-0.959781266907386));
#70363=CARTESIAN_POINT('Ctrl Pts',(-0.40699144156463,-0.000374692172387895,
-1.08021873309261));
#70364=CARTESIAN_POINT('Ctrl Pts',(-0.407296855312001,-0.0339025205290725,
-1.07825249224918));
#70365=CARTESIAN_POINT('Ctrl Pts',(-0.388158661228782,-0.202637347893537,
-1.06833685738634));
#70366=CARTESIAN_POINT('Ctrl Pts',(-0.153586221418629,-0.456176553787775,
-1.05047182850409));
#70367=CARTESIAN_POINT('Ctrl Pts',(0.300481799522643,-0.376027211503337,
-1.02662364644585));
#70368=CARTESIAN_POINT('Ctrl Pts',(0.478818880020692,0.0491757640619698,
-1.00277546438762));
#70369=CARTESIAN_POINT('Ctrl Pts',(0.217777667724211,0.429253611605008,
-0.978927282329384));
#70370=CARTESIAN_POINT('Ctrl Pts',(-0.243102740239076,0.415435715031318,
-0.955079100271148));
#70371=CARTESIAN_POINT('Ctrl Pts',(-0.405001862422473,0.146490969879461,
-0.938842917192225));
#70372=CARTESIAN_POINT('Ctrl Pts',(-0.407709110635635,0.00583350717703751,
-0.930556128132711));
#70373=CARTESIAN_POINT('Ctrl Pts',(-0.407689224696409,0.000105882686618259,
-0.930218733092609));
#70374=CARTESIAN_POINT('Origin',(0.,0.,-3.73478126690739));
#70375=CARTESIAN_POINT('',(-0.407368292334763,0.000320074934392933,-1.25978126690739));
#70376=CARTESIAN_POINT('',(-0.406394339960205,8.27571951184103E-5,-1.23021873309261));
#70377=CARTESIAN_POINT('',(-0.40705,-1.06687458785308E-14,-3.73478126690739));
#70378=CARTESIAN_POINT('Ctrl Pts',(-0.407368292334763,0.000320074934392955,
-1.25978126690739));
#70379=CARTESIAN_POINT('Ctrl Pts',(-0.406381911580918,-0.114007642520982,
-1.25306053413298));
#70380=CARTESIAN_POINT('Ctrl Pts',(-0.296492855911722,-0.36522436272828,
-1.23839040733917));
#70381=CARTESIAN_POINT('Ctrl Pts',(0.129642767060033,-0.463549947676258,
-1.21577088652594));
#70382=CARTESIAN_POINT('Ctrl Pts',(0.459961473100724,-0.141849371886711,
-1.19192270446771));
#70383=CARTESIAN_POINT('Ctrl Pts',(0.368205997786016,0.310016361239286,
-1.16807452240948));
#70384=CARTESIAN_POINT('Ctrl Pts',(-0.0614261349757158,0.477401959551476,
-1.14422634035124));
#70385=CARTESIAN_POINT('Ctrl Pts',(-0.365556557396479,0.256846415827171,
-1.12479525518388));
#70386=CARTESIAN_POINT('Ctrl Pts',(-0.406576326514428,0.0605708910621262,
-1.11331356403593));
#70387=CARTESIAN_POINT('Ctrl Pts',(-0.406413319057786,0.000122795012471158,
-1.10978126690739));
#70388=CARTESIAN_POINT('Ctrl Pts',(-0.406394339960205,8.27571951184519E-5,
-1.23021873309261));
#70389=CARTESIAN_POINT('Ctrl Pts',(-0.406261889000297,-0.0729960169730691,
-1.22594885636565));
#70390=CARTESIAN_POINT('Ctrl Pts',(-0.35248490968645,-0.282310174334548,
-1.21372958561928));
#70391=CARTESIAN_POINT('Ctrl Pts',(-0.0169768509947866,-0.481038004907766,
-1.19356092085349));
#70392=CARTESIAN_POINT('Ctrl Pts',(0.395318859158266,-0.274606582639873,
-1.16971273879526));
#70393=CARTESIAN_POINT('Ctrl Pts',(0.444858352516096,0.183811919722327,
-1.14586455673703));
#70394=CARTESIAN_POINT('Ctrl Pts',(0.0861827323523932,0.473559196172579,
-1.12201637467879));
#70395=CARTESIAN_POINT('Ctrl Pts',(-0.315484200393037,0.34069350414254,
-1.10013443346399));
#70396=CARTESIAN_POINT('Ctrl Pts',(-0.406062085815216,0.101648482346894,
-1.08620188626859));
#70397=CARTESIAN_POINT('Ctrl Pts',(-0.40699144156463,-0.000374692172387895,
-1.08021873309261));
#70398=CARTESIAN_POINT('Origin',(0.,0.,-3.73478126690739));
#70399=CARTESIAN_POINT('',(-0.407440005731881,-0.00029330702205249,-1.40978126690739));
#70400=CARTESIAN_POINT('',(-0.407295941515244,0.000340925431555991,-1.38021873309261));
#70401=CARTESIAN_POINT('',(-0.40705,-1.06687458785308E-14,-3.73478126690739));
#70402=CARTESIAN_POINT('Ctrl Pts',(-0.407440005731881,-0.000293307022052439,
-1.40978126690739));
#70403=CARTESIAN_POINT('Ctrl Pts',(-0.407588524841362,-0.0185715359398175,
-1.40870629226887));
#70404=CARTESIAN_POINT('Ctrl Pts',(-0.39815909867122,-0.171862363193748,
-1.39968192361093));
#70405=CARTESIAN_POINT('Ctrl Pts',(-0.203608890553224,-0.43615274930846,
-1.38270816093359));
#70406=CARTESIAN_POINT('Ctrl Pts',(0.256572182166905,-0.407254854335409,
-1.35885997887535));
#70407=CARTESIAN_POINT('Ctrl Pts',(0.481315071300406,-0.00464792219482722,
-1.33501179681712));
#70408=CARTESIAN_POINT('Ctrl Pts',(0.264389089074653,0.402224080109482,
-1.31116361475888));
#70409=CARTESIAN_POINT('Ctrl Pts',(-0.195148100516391,0.440003431698535,
-1.28731543270065));
#70410=CARTESIAN_POINT('Ctrl Pts',(-0.396573317235439,0.177160896699739,
-1.27018798341682));
#70411=CARTESIAN_POINT('Ctrl Pts',(-0.407548619070813,0.0212210749269621,
-1.2610099281524));
#70412=CARTESIAN_POINT('Ctrl Pts',(-0.407368292334763,0.000320074934392955,
-1.25978126690739));
#70413=CARTESIAN_POINT('Ctrl Pts',(-0.407295941515244,0.000340925431555998,
-1.38021873309261));
#70414=CARTESIAN_POINT('Ctrl Pts',(-0.406292379364719,-0.111533876317919,
-1.37364522048212));
#70415=CARTESIAN_POINT('Ctrl Pts',(-0.300437242591872,-0.360368125454541,
-1.35912231385222));
#70416=CARTESIAN_POINT('Ctrl Pts',(0.121045283258203,-0.465868881807192,
-1.3366500132029));
#70417=CARTESIAN_POINT('Ctrl Pts',(0.457258640884715,-0.150333998056345,
-1.31280183114467));
#70418=CARTESIAN_POINT('Ctrl Pts',(0.373878015523797,0.303151785650903,
-1.28895364908643));
#70419=CARTESIAN_POINT('Ctrl Pts',(-0.0525840776504784,0.478456571083512,
-1.2651054670282));
#70420=CARTESIAN_POINT('Ctrl Pts',(-0.363077306115782,0.261936811360845,
-1.24552716169692));
#70421=CARTESIAN_POINT('Ctrl Pts',(-0.406508478055647,0.0630575525949989,
-1.23389825038506));
#70422=CARTESIAN_POINT('Ctrl Pts',(-0.406394339960205,8.27571951184519E-5,
-1.23021873309261));
#70423=CARTESIAN_POINT('Origin',(0.,0.,-3.73478126690739));
#70424=CARTESIAN_POINT('',(-0.406440918185289,-0.000163016377902653,-1.55978126690739));
#70425=CARTESIAN_POINT('',(-0.407503887525846,-0.000263145742968152,-1.53021873309261));
#70426=CARTESIAN_POINT('',(-0.40705,-1.06687458785308E-14,-3.73478126690739));
#70427=CARTESIAN_POINT('Ctrl Pts',(-0.406440918185289,-0.000163016377902669,
-1.55978126690739));
#70428=CARTESIAN_POINT('Ctrl Pts',(-0.406648703272632,-0.0579712755676122,
-1.55640265638533));
#70429=CARTESIAN_POINT('Ctrl Pts',(-0.368077181138247,-0.251529596840672,
-1.54507465184387));
#70430=CARTESIAN_POINT('Ctrl Pts',(-0.0706340888623429,-0.476126691682194,
-1.525797253283));
#70431=CARTESIAN_POINT('Ctrl Pts',(0.362150411553781,-0.317069204517043,
-1.50194907122476));
#70432=CARTESIAN_POINT('Ctrl Pts',(0.462615038625616,0.132940313972334,
-1.47810088916653));
#70433=CARTESIAN_POINT('Ctrl Pts',(0.138570494539446,0.460959888802416,
-1.45425270710829));
#70434=CARTESIAN_POINT('Ctrl Pts',(-0.292292194285244,0.370269985671315,
-1.43147949968858));
#70435=CARTESIAN_POINT('Ctrl Pts',(-0.406490232027403,0.116595228407491,
-1.41665568628828));
#70436=CARTESIAN_POINT('Ctrl Pts',(-0.407440005731881,-0.000293307022052439,
-1.40978126690739));
#70437=CARTESIAN_POINT('Ctrl Pts',(-0.407503887525846,-0.000263145742968167,
-1.53021873309261));
#70438=CARTESIAN_POINT('Ctrl Pts',(-0.407622154607844,-0.0160316617814609,
-1.529290978618));
#70439=CARTESIAN_POINT('Ctrl Pts',(-0.399625537496969,-0.166790447514566,
-1.52041383012398));
#70440=CARTESIAN_POINT('Ctrl Pts',(-0.211642503026044,-0.432311492500735,
-1.50358728761054));
#70441=CARTESIAN_POINT('Ctrl Pts',(0.24899438347629,-0.411931514493132,
-1.47973910555231));
#70442=CARTESIAN_POINT('Ctrl Pts',(0.481146697435232,-0.0135510583539467,
-1.45589092349407));
#70443=CARTESIAN_POINT('Ctrl Pts',(0.271784644847739,0.397264247649257,
-1.43204274143584));
#70444=CARTESIAN_POINT('Ctrl Pts',(-0.186974994684948,0.443538191137929,
-1.40819455937761));
#70445=CARTESIAN_POINT('Ctrl Pts',(-0.395000964387442,0.182239984207465,
-1.39091988992986));
#70446=CARTESIAN_POINT('Ctrl Pts',(-0.407505993976906,0.0237570910304725,
-1.38159461450153));
#70447=CARTESIAN_POINT('Ctrl Pts',(-0.407295941515244,0.000340925431555998,
-1.38021873309261));
#70448=CARTESIAN_POINT('Origin',(0.,0.,-3.73478126690739));
#70449=CARTESIAN_POINT('',(-0.406841268402119,0.000361155301022391,-1.70978126690739));
#70450=CARTESIAN_POINT('',(-0.406474561616192,-0.000199550871096271,-1.68021873309261));
#70451=CARTESIAN_POINT('',(-0.40705,-1.06687458785308E-14,-3.73478126690739));
#70452=CARTESIAN_POINT('Ctrl Pts',(-0.406841268402119,0.000361155301022383,
-1.70978126690739));
#70453=CARTESIAN_POINT('Ctrl Pts',(-0.406015505560738,-0.0966219857244575,
-1.7040990205018));
#70454=CARTESIAN_POINT('Ctrl Pts',(-0.322687842220291,-0.330557993933317,
-1.69046738007681));
#70455=CARTESIAN_POINT('Ctrl Pts',(0.0682186748769831,-0.476478764940969,
-1.6688863456324));
#70456=CARTESIAN_POINT('Ctrl Pts',(0.437591544119186,-0.200497983922606,
-1.64503816357417));
#70457=CARTESIAN_POINT('Ctrl Pts',(0.405417537039194,0.259465646478908,
-1.62118998151593));
#70458=CARTESIAN_POINT('Ctrl Pts',(0.00122046920282805,0.481335965305491,
-1.5973417994577));
#70459=CARTESIAN_POINT('Ctrl Pts',(-0.346674621281165,0.29266017250168,
-1.57687222792152));
#70460=CARTESIAN_POINT('Ctrl Pts',(-0.406159814269338,0.0780434046909889,
-1.56435205040475));
#70461=CARTESIAN_POINT('Ctrl Pts',(-0.406440918185289,-0.000163016377902669,
-1.55978126690739));
#70462=CARTESIAN_POINT('Ctrl Pts',(-0.406474561616192,-0.000199550871096264,
-1.68021873309261));
#70463=CARTESIAN_POINT('Ctrl Pts',(-0.406718999720409,-0.0554774150689223,
-1.67698734273447));
#70464=CARTESIAN_POINT('Ctrl Pts',(-0.37042783086876,-0.246434376736608,
-1.66580655835692));
#70465=CARTESIAN_POINT('Ctrl Pts',(-0.0794299488178135,-0.474738516307812,
-1.64667637995995));
#70466=CARTESIAN_POINT('Ctrl Pts',(0.356222900192536,-0.323714412737155,
-1.62282819790172));
#70467=CARTESIAN_POINT('Ctrl Pts',(0.464995134691316,0.124359560745234,
-1.59898001584348));
#70468=CARTESIAN_POINT('Ctrl Pts',(0.147074151851645,0.458317542204598,
-1.57513183378525));
#70469=CARTESIAN_POINT('Ctrl Pts',(-0.288188203612822,0.375079119038563,
-1.55221140620162));
#70470=CARTESIAN_POINT('Ctrl Pts',(-0.406608792064132,0.119079674807948,
-1.53724037263741));
#70471=CARTESIAN_POINT('Ctrl Pts',(-0.407503887525846,-0.000263145742968167,
-1.53021873309261));
#70472=CARTESIAN_POINT('Origin',(0.,0.,-3.73478126690739));
#70473=CARTESIAN_POINT('',(-0.40772218496585,-1.16393611243039E-5,-1.85978126690739));
#70474=CARTESIAN_POINT('',(-0.406772054937087,0.00034738140794717,-1.83021873309261));
#70475=CARTESIAN_POINT('',(-0.40705,-1.06687458785308E-14,-3.73478126690739));
#70476=CARTESIAN_POINT('Ctrl Pts',(-0.40772218496585,-1.16393611242892E-5,
-1.85978126690739));
#70477=CARTESIAN_POINT('Ctrl Pts',(-0.407722444052212,-0.000630930684549266,
-1.85974477863768));
#70478=CARTESIAN_POINT('Ctrl Pts',(-0.407440412028103,-0.136169797995048,
-1.85175889634857));
#70479=CARTESIAN_POINT('Ctrl Pts',(-0.258634130007767,-0.405948503922317,
-1.83582362004005));
#70480=CARTESIAN_POINT('Ctrl Pts',(0.20139448024705,-0.437179670579116,
-1.81197543798181));
#70481=CARTESIAN_POINT('Ctrl Pts',(0.476617589713424,-0.0672419081928105,
-1.78812725592358));
#70482=CARTESIAN_POINT('Ctrl Pts',(0.314482375140717,0.364399007637914,
-1.76427907386534));
#70483=CARTESIAN_POINT('Ctrl Pts',(-0.136231120007138,0.461656672196172,
-1.74043089180711));
#70484=CARTESIAN_POINT('Ctrl Pts',(-0.384330302527872,0.213048446444068,
-1.72226495615446));
#70485=CARTESIAN_POINT('Ctrl Pts',(-0.407170737791829,0.0390562559818897,
-1.71204841452121));
#70486=CARTESIAN_POINT('Ctrl Pts',(-0.406841268402119,0.000361155301022383,
-1.70978126690739));
#70487=CARTESIAN_POINT('Ctrl Pts',(-0.406772054937087,0.000347381407947184,
-1.83021873309261));
#70488=CARTESIAN_POINT('Ctrl Pts',(-0.406007973272697,-0.0941637101848716,
-1.82468370685094));
#70489=CARTESIAN_POINT('Ctrl Pts',(-0.32609986428909,-0.325576544298442,
-1.81119928658986));
#70490=CARTESIAN_POINT('Ctrl Pts',(0.0593925331488187,-0.477659190889811,
-1.78976547230936));
#70491=CARTESIAN_POINT('Ctrl Pts',(0.433807590226198,-0.208558745435148,
-1.76591729025113));
#70492=CARTESIAN_POINT('Ctrl Pts',(0.410148038410438,0.251921341341723,
-1.74206910819289));
#70493=CARTESIAN_POINT('Ctrl Pts',(0.0101245785925387,0.481230992916775,
-1.71822092613466));
#70494=CARTESIAN_POINT('Ctrl Pts',(-0.343728093356254,0.297712804988723,
-1.69760413443456));
#70495=CARTESIAN_POINT('Ctrl Pts',(-0.406117668841617,0.0805091029179855,
-1.68493673675388));
#70496=CARTESIAN_POINT('Ctrl Pts',(-0.406474561616192,-0.000199550871096264,
-1.68021873309261));
#70497=CARTESIAN_POINT('Origin',(0.,0.,-3.73478126690739));
#70498=CARTESIAN_POINT('',(-0.40680653690778,-0.000354893438868044,-2.00978126690739));
#70499=CARTESIAN_POINT('',(-0.40771880079626,3.52644710581579E-5,-1.98021873309261));
#70500=CARTESIAN_POINT('',(-0.40705,-1.06687458785308E-14,-3.73478126690739));
#70501=CARTESIAN_POINT('Ctrl Pts',(-0.40680653690778,-0.000354893438868045,
-2.00978126690739));
#70502=CARTESIAN_POINT('Ctrl Pts',(-0.407138596781516,-0.0403041751809355,
-2.00744114275415));
#70503=CARTESIAN_POINT('Ctrl Pts',(-0.383366193393983,-0.215574408747965,
-1.99715162458151));
#70504=CARTESIAN_POINT('Ctrl Pts',(-0.131991827375041,-0.46288655040716,
-1.97891271238946));
#70505=CARTESIAN_POINT('Ctrl Pts',(0.317810826682713,-0.361499764156071,
-1.95506453033122));
#70506=CARTESIAN_POINT('Ctrl Pts',(0.475980915095963,0.0716098422428978,
-1.93121634827299));
#70507=CARTESIAN_POINT('Ctrl Pts',(0.197376910832261,0.439008150393539,
-1.90736816621475));
#70508=CARTESIAN_POINT('Ctrl Pts',(-0.261642567705972,0.403613899628779,
-1.88355647242622));
#70509=CARTESIAN_POINT('Ctrl Pts',(-0.407665999074413,0.134288888284683,
-1.8676941726571));
#70510=CARTESIAN_POINT('Ctrl Pts',(-0.40772218496585,-1.16393611242892E-5,
-1.85978126690739));
#70511=CARTESIAN_POINT('Ctrl Pts',(-0.40771880079626,3.52644710581694E-5,
-1.98021873309261));
#70512=CARTESIAN_POINT('Ctrl Pts',(-0.407554198464361,-0.133008126687299,
-1.97238007096741));
#70513=CARTESIAN_POINT('Ctrl Pts',(-0.263966612793417,-0.401278997996624,
-1.95659201482279));
#70514=CARTESIAN_POINT('Ctrl Pts',(0.193272542416614,-0.440830466260172,
-1.93285456465877));
#70515=CARTESIAN_POINT('Ctrl Pts',(0.475292082851708,-0.0760474300277662,
-1.90900638260053));
#70516=CARTESIAN_POINT('Ctrl Pts',(0.321169623344976,0.358518965573356,
-1.8851582005423));
#70517=CARTESIAN_POINT('Ctrl Pts',(-0.127667532450826,0.464097809511379,
-1.86131001848406));
#70518=CARTESIAN_POINT('Ctrl Pts',(-0.382370862514766,0.218144542773098,
-1.8429968626675));
#70519=CARTESIAN_POINT('Ctrl Pts',(-0.407105345886311,0.0415729373886564,
-1.83263310087035));
#70520=CARTESIAN_POINT('Ctrl Pts',(-0.406772054937087,0.000347381407947184,
-1.83021873309261));
#70521=CARTESIAN_POINT('Origin',(0.,0.,-3.73478126690739));
#70522=CARTESIAN_POINT('',(-0.406456740617355,0.000181399743008865,-2.15978126690739));
#70523=CARTESIAN_POINT('',(-0.406877361306786,-0.000366356398630974,-2.13021873309261));
#70524=CARTESIAN_POINT('',(-0.40705,-1.06687458785308E-14,-3.73478126690739));
#70525=CARTESIAN_POINT('Ctrl Pts',(-0.406456740617355,0.000181399743008834,
-2.15978126690739));
#70526=CARTESIAN_POINT('Ctrl Pts',(-0.4061382297576,-0.0792659267566264,
-2.15513750687062));
#70527=CARTESIAN_POINT('Ctrl Pts',(-0.34522264593974,-0.295165752186438,
-2.14254435281445));
#70528=CARTESIAN_POINT('Ctrl Pts',(0.00563444864094621,-0.481304533564932,
-2.12200180473886));
#70529=CARTESIAN_POINT('Ctrl Pts',(0.407779886717249,-0.255736905882805,
-2.09815362268063));
#70530=CARTESIAN_POINT('Ctrl Pts',(0.435734502464197,0.204502431290978,
-2.07430544062239));
#70531=CARTESIAN_POINT('Ctrl Pts',(0.0638463179520797,0.47708432035187,
-2.05045725856416));
#70532=CARTESIAN_POINT('Ctrl Pts',(-0.324388339227509,0.328090460304887,
-2.02894920065916));
#70533=CARTESIAN_POINT('Ctrl Pts',(-0.406010590487186,0.0954034029496748,
-2.01539053677357));
#70534=CARTESIAN_POINT('Ctrl Pts',(-0.40680653690778,-0.000354893438868045,
-2.00978126690739));
#70535=CARTESIAN_POINT('Ctrl Pts',(-0.406877361306786,-0.00036635639863097,
-2.13021873309261));
#70536=CARTESIAN_POINT('Ctrl Pts',(-0.407202839001211,-0.037785859492885,
-2.12802582910329));
#70537=CARTESIAN_POINT('Ctrl Pts',(-0.385296759883492,-0.210478987110743,
-2.11788353109455));
#70538=CARTESIAN_POINT('Ctrl Pts',(-0.14053225246876,-0.460365573920769,
-2.09979183906641));
#70539=CARTESIAN_POINT('Ctrl Pts',(0.311068976634055,-0.367317121042818,
-2.07594365700817));
#70540=CARTESIAN_POINT('Ctrl Pts',(0.477224160065282,0.0627923298288068,
-2.05209547494994));
#70541=CARTESIAN_POINT('Ctrl Pts',(0.205464412655191,0.435281691284622,
-2.02824729289171));
#70542=CARTESIAN_POINT('Ctrl Pts',(-0.254835525272372,0.408343765342997,
-2.00439911083347));
#70543=CARTESIAN_POINT('Ctrl Pts',(-0.406857244157191,0.138714721617122,
-1.98838959090044));
#70544=CARTESIAN_POINT('Ctrl Pts',(-0.407721126030811,0.00191468553547783,
-1.98032946498682));
#70545=CARTESIAN_POINT('Ctrl Pts',(-0.40771880079626,3.52644710581694E-5,
-1.98021873309261));
#70546=CARTESIAN_POINT('Origin',(0.,0.,-3.73478126690739));
#70547=CARTESIAN_POINT('',(-0.407472342035332,0.0002788890774828,-2.30978126690739));
#70548=CARTESIAN_POINT('',(-0.406426582399692,0.00014382004374669,-2.28021873309261));
#70549=CARTESIAN_POINT('',(-0.40705,-1.06687458785308E-14,-3.73478126690739));
#70550=CARTESIAN_POINT('Ctrl Pts',(-0.407472342035332,0.000278889077482811,
-2.30978126690739));
#70551=CARTESIAN_POINT('Ctrl Pts',(-0.406547165835321,-0.117826010948906,
-2.30283387098709));
#70552=CARTESIAN_POINT('Ctrl Pts',(-0.2902676921825,-0.37265690370858,-2.28793708104738));
#70553=CARTESIAN_POINT('Ctrl Pts',(0.142791842339502,-0.459669762767722,
-2.26509089708827));
#70554=CARTESIAN_POINT('Ctrl Pts',(0.463814698616821,-0.128692371136095,
-2.24124271503003));
#70555=CARTESIAN_POINT('Ctrl Pts',(0.359227540430107,0.3203769268193,-2.2173945329718));
#70556=CARTESIAN_POINT('Ctrl Pts',(-0.0749973785569536,0.475458930141424,
-2.19354635091357));
#70557=CARTESIAN_POINT('Ctrl Pts',(-0.369250167839865,0.249004140055587,
-2.17434192889209));
#70558=CARTESIAN_POINT('Ctrl Pts',(-0.406683470748437,0.0567355240363727,
-2.16308690089003));
#70559=CARTESIAN_POINT('Ctrl Pts',(-0.406456740617355,0.000181399743008834,
-2.15978126690739));
#70560=CARTESIAN_POINT('Ctrl Pts',(-0.406426582399692,0.000143820043746662,
-2.28021873309261));
#70561=CARTESIAN_POINT('Ctrl Pts',(-0.406183098315414,-0.0767990503092323,
-2.27572219321976));
#70562=CARTESIAN_POINT('Ctrl Pts',(-0.348134530504143,-0.290109160327883,
-2.26327625932749));
#70563=CARTESIAN_POINT('Ctrl Pts',(-0.00327025270698847,-0.481326376882232,
-2.24288093141582));
#70564=CARTESIAN_POINT('Ctrl Pts',(0.402979161470327,-0.263236720569178,
-2.21903274935758));
#70565=CARTESIAN_POINT('Ctrl Pts',(0.4394430400586,0.196406695861922,-2.19518456729935));
#70566=CARTESIAN_POINT('Ctrl Pts',(0.0726610551733367,0.47582154921403,
-2.17133638524111));
#70567=CARTESIAN_POINT('Ctrl Pts',(-0.320939240454663,0.33306470369783,
-2.14968110717221));
#70568=CARTESIAN_POINT('Ctrl Pts',(-0.406022964984787,0.0978618366923023,
-2.1359752231227));
#70569=CARTESIAN_POINT('Ctrl Pts',(-0.406877361306786,-0.00036635639863097,
-2.13021873309261));
#70570=CARTESIAN_POINT('Origin',(0.,0.,-3.73478126690739));
#70571=CARTESIAN_POINT('',(-0.40733281339199,-0.000331010205261331,-2.45978126690739));
#70572=CARTESIAN_POINT('',(-0.407405900524309,0.000306859758717713,-2.43021873309261));
#70573=CARTESIAN_POINT('',(-0.40705,-1.06687458785308E-14,-3.73478126690739));
#70574=CARTESIAN_POINT('Ctrl Pts',(-0.40733281339199,-0.000331010205261342,
-2.45978126690739));
#70575=CARTESIAN_POINT('Ctrl Pts',(-0.407528022996003,-0.0224784334219731,
-2.45847962912297));
#70576=CARTESIAN_POINT('Ctrl Pts',(-0.395800475568512,-0.179678172289964,
-2.44922859731915));
#70577=CARTESIAN_POINT('Ctrl Pts',(-0.191104898808961,-0.441774511139857,
-2.43202817149591));
#70578=CARTESIAN_POINT('Ctrl Pts',(0.268066517033437,-0.399782620291585,
-2.40817998943768));
#70579=CARTESIAN_POINT('Ctrl Pts',(0.481252209413066,0.00906156590694945,
-2.38433180737944));
#70580=CARTESIAN_POINT('Ctrl Pts',(0.252826714350878,0.409590592607036,
-2.36048362532121));
#70581=CARTESIAN_POINT('Ctrl Pts',(-0.207600012825493,0.434267239976145,
-2.33663544326297));
#70582=CARTESIAN_POINT('Ctrl Pts',(-0.398892410069302,0.169347774513397,
-2.31973465712503));
#70583=CARTESIAN_POINT('Ctrl Pts',(-0.407605776894147,0.0173127369653136,
-2.3107832650065));
#70584=CARTESIAN_POINT('Ctrl Pts',(-0.407472342035332,0.000278889077482811,
-2.30978126690739));
#70585=CARTESIAN_POINT('Ctrl Pts',(-0.407405900524309,0.00030685975871772,
-2.43021873309261));
#70586=CARTESIAN_POINT('Ctrl Pts',(-0.406435945677901,-0.115344487807178,
-2.42341855733623));
#70587=CARTESIAN_POINT('Ctrl Pts',(-0.294332076638151,-0.367835636378687,
-2.40866898756043));
#70588=CARTESIAN_POINT('Ctrl Pts',(0.134263887909296,-0.462232608151807,
-2.38597002376523));
#70589=CARTESIAN_POINT('Ctrl Pts',(0.461354600469472,-0.137250531004422,
-2.36212184170699));
#70590=CARTESIAN_POINT('Ctrl Pts',(0.365092757010119,0.313676671772215,
-2.33827365964876));
#70591=CARTESIAN_POINT('Ctrl Pts',(-0.0661889425581167,0.476764931091184,
-2.31442547759052));
#70592=CARTESIAN_POINT('Ctrl Pts',(-0.366868044521016,0.254098374107902,
-2.29507383540514));
#70593=CARTESIAN_POINT('Ctrl Pts',(-0.406613551725838,0.0592275858856569,
-2.28367158723917));
#70594=CARTESIAN_POINT('Ctrl Pts',(-0.406426582399692,0.000143820043746662,
-2.28021873309261));
#70595=CARTESIAN_POINT('Origin',(0.,0.,-3.73478126690739));
#70596=CARTESIAN_POINT('',(-0.406402994387456,-0.000103102301948036,-2.60978126690739));
#70597=CARTESIAN_POINT('',(-0.407403472603433,-0.000307765760287793,-2.58021873309261));
#70598=CARTESIAN_POINT('',(-0.40705,-1.06687458785308E-14,-3.73478126690739));
#70599=CARTESIAN_POINT('Ctrl Pts',(-0.406402994387456,-0.000103102301948009,
-2.60978126690739));
#70600=CARTESIAN_POINT('Ctrl Pts',(-0.406542488586396,-0.0618039549847077,
-2.60617599323944));
#70601=CARTESIAN_POINT('Ctrl Pts',(-0.364335566924364,-0.259370083859107,
-2.59462132555209));
#70602=CARTESIAN_POINT('Ctrl Pts',(-0.0570455976290363,-0.477945186012748,
-2.57511726384532));
#70603=CARTESIAN_POINT('Ctrl Pts',(0.371033481116859,-0.306626738775311,
-2.55126908178708));
#70604=CARTESIAN_POINT('Ctrl Pts',(0.458641320517021,0.146061425968784,
-2.52742089972885));
#70605=CARTESIAN_POINT('Ctrl Pts',(0.125386389416043,0.46471932861766,-2.50357271767061));
#70606=CARTESIAN_POINT('Ctrl Pts',(-0.298457773679393,0.362819873754557,
-2.4810261733968));
#70607=CARTESIAN_POINT('Ctrl Pts',(-0.406335834141885,0.112780849746093,
-2.46642902314238));
#70608=CARTESIAN_POINT('Ctrl Pts',(-0.40733281339199,-0.000331010205261342,
-2.45978126690739));
#70609=CARTESIAN_POINT('Ctrl Pts',(-0.407403472603433,-0.000307765760287751,
-2.58021873309261));
#70610=CARTESIAN_POINT('Ctrl Pts',(-0.407568470906435,-0.0199413795938409,
-2.57906431547211));
#70611=CARTESIAN_POINT('Ctrl Pts',(-0.39734641009149,-0.174600768307096,
-2.56996050383219));
#70612=CARTESIAN_POINT('Ctrl Pts',(-0.199244649661891,-0.438163605536162,
-2.55290729817287));
#70613=CARTESIAN_POINT('Ctrl Pts',(0.260624980917576,-0.404673195253975,
-2.52905911611463));
#70614=CARTESIAN_POINT('Ctrl Pts',(0.481337460529596,0.000157245861404591,
-2.5052109340564));
#70615=CARTESIAN_POINT('Ctrl Pts',(0.260360523766897,0.404843393547639,
-2.48136275199817));
#70616=CARTESIAN_POINT('Ctrl Pts',(-0.199530890300541,0.438033331438621,
-2.45751456993993));
#70617=CARTESIAN_POINT('Ctrl Pts',(-0.39740005747315,0.174421513829129,
-2.44046656363808));
#70618=CARTESIAN_POINT('Ctrl Pts',(-0.407569821261616,0.0198517429393876,
-2.43136795135564));
#70619=CARTESIAN_POINT('Ctrl Pts',(-0.407405900524309,0.00030685975871772,
-2.43021873309261));
#70620=CARTESIAN_POINT('Origin',(0.,0.,-3.73478126690739));
#70621=CARTESIAN_POINT('',(-0.406953572106064,0.000373234526637736,-2.75978126690739));
#70622=CARTESIAN_POINT('',(-0.406425648305095,-0.000142458567169629,-2.73021873309261));
#70623=CARTESIAN_POINT('',(-0.40705,-1.06687458785308E-14,-3.73478126690739));
#70624=CARTESIAN_POINT('Ctrl Pts',(-0.406953572106064,0.000373234526637737,
-2.75978126690739));
#70625=CARTESIAN_POINT('Ctrl Pts',(-0.406046513116615,-0.100407864961081,
-2.75387235735591));
#70626=CARTESIAN_POINT('Ctrl Pts',(-0.317290461654102,-0.338198853077946,
-2.74001405378502));
#70627=CARTESIAN_POINT('Ctrl Pts',(0.0817608711451184,-0.474342661995509,
-2.71820635619473));
#70628=CARTESIAN_POINT('Ctrl Pts',(0.443124125342135,-0.187954277905899,
-2.69435817413649));
#70629=CARTESIAN_POINT('Ctrl Pts',(0.397863643893962,0.270906481850664,
-2.67050999207826));
#70630=CARTESIAN_POINT('Ctrl Pts',(-0.0124882236963727,0.481175482864919,
-2.64666181002002));
#70631=CARTESIAN_POINT('Ctrl Pts',(-0.351077571508608,0.284866454272714,
-2.62641890162973));
#70632=CARTESIAN_POINT('Ctrl Pts',(-0.406234912947782,0.0742424133312181,
-2.61412538725885));
#70633=CARTESIAN_POINT('Ctrl Pts',(-0.406402994387456,-0.000103102301948009,
-2.60978126690739));
#70634=CARTESIAN_POINT('Ctrl Pts',(-0.406425648305095,-0.000142458567169636,
-2.73021873309261));
#70635=CARTESIAN_POINT('Ctrl Pts',(-0.406611102354183,-0.0593155331541186,
-2.72676067958858));
#70636=CARTESIAN_POINT('Ctrl Pts',(-0.366782770719768,-0.254278247849184,
-2.71535323206513));
#70637=CARTESIAN_POINT('Ctrl Pts',(-0.0658774242972122,-0.476808075228433,
-2.69599639052228));
#70638=CARTESIAN_POINT('Ctrl Pts',(0.365297626161182,-0.313438063988078,
-2.67214820846404));
#70639=CARTESIAN_POINT('Ctrl Pts',(0.461264826549058,0.137551937187166,
-2.64830002640581));
#70640=CARTESIAN_POINT('Ctrl Pts',(0.133961850108581,0.462320233551161,
-2.62445184434757));
#70641=CARTESIAN_POINT('Ctrl Pts',(-0.294474187986566,0.367664936403977,
-2.60175807990984));
#70642=CARTESIAN_POINT('Ctrl Pts',(-0.406432281974628,0.115256948650598,
-2.58701370949152));
#70643=CARTESIAN_POINT('Ctrl Pts',(-0.407403472603433,-0.000307765760287751,
-2.58021873309261));
#70644=CARTESIAN_POINT('Origin',(0.,0.,-3.73478126690739));
#70645=CARTESIAN_POINT('',(-0.40770196810232,-8.31109565067826E-5,-2.90978126690739));
#70646=CARTESIAN_POINT('',(-0.406879917492779,0.000366675793932125,-2.88021873309261));
#70647=CARTESIAN_POINT('',(-0.40705,-1.06687458785308E-14,-3.73478126690739));
#70648=CARTESIAN_POINT('Ctrl Pts',(-0.407701968102319,-8.31109565068242E-5,
-2.90978126690739));
#70649=CARTESIAN_POINT('Ctrl Pts',(-0.407714401779122,-0.00455000157151528,
-2.90951811549179));
#70650=CARTESIAN_POINT('Ctrl Pts',(-0.405622145279423,-0.143942763391086,
-2.90130557005679));
#70651=CARTESIAN_POINT('Ctrl Pts',(-0.246968019692694,-0.413149607648352,
-2.88514363060237));
#70652=CARTESIAN_POINT('Ctrl Pts',(0.213763439489368,-0.431266730500215,
-2.86129544854413));
#70653=CARTESIAN_POINT('Ctrl Pts',(0.478339277460365,-0.053640812432835,
-2.8374472664859));
#70654=CARTESIAN_POINT('Ctrl Pts',(0.303976919789322,0.373207493590096,
-2.81359908442767));
#70655=CARTESIAN_POINT('Ctrl Pts',(-0.149323603380172,0.457589622365882,
-2.78975090236943));
#70656=CARTESIAN_POINT('Ctrl Pts',(-0.387235890803543,0.205205383146445,
-2.77181162986267));
#70657=CARTESIAN_POINT('Ctrl Pts',(-0.407266800759058,0.0351753018750611,
-2.76182175137532));
#70658=CARTESIAN_POINT('Ctrl Pts',(-0.406953572106064,0.000373234526637737,
-2.75978126690739));
#70659=CARTESIAN_POINT('Ctrl Pts',(-0.406879917492779,0.000366675793932139,
-2.88021873309261));
#70660=CARTESIAN_POINT('Ctrl Pts',(-0.406023584688337,-0.0979486711077955,
-2.87445704370505));
#70661=CARTESIAN_POINT('Ctrl Pts',(-0.320816081720589,-0.333240111186755,
-2.86074596029807));
#70662=CARTESIAN_POINT('Ctrl Pts',(0.0729719274013494,-0.475773973046388,
-2.83908548287168));
#70663=CARTESIAN_POINT('Ctrl Pts',(0.439571272608378,-0.196119534836683,
-2.81523730081345));
#70664=CARTESIAN_POINT('Ctrl Pts',(0.402807084347494,0.263499959076195,
-2.79138911875521));
#70665=CARTESIAN_POINT('Ctrl Pts',(-0.00358473645388183,0.481324137455872,
-2.76754093669698));
#70666=CARTESIAN_POINT('Ctrl Pts',(-0.348236120974117,0.289930441795519,
-2.74715080814278));
#70667=CARTESIAN_POINT('Ctrl Pts',(-0.406184779480063,0.0767118836232727,
-2.73471007360799));
#70668=CARTESIAN_POINT('Ctrl Pts',(-0.406425648305095,-0.000142458567169636,
-2.73021873309261));
#70669=CARTESIAN_POINT('Origin',(0.,0.,-3.73478126690739));
#70670=CARTESIAN_POINT('',(-0.406704477435532,-0.000328489605546852,-3.05978126690739));
#70671=CARTESIAN_POINT('',(-0.407718443135198,-3.6913074990319E-5,-3.03021873309261));
#70672=CARTESIAN_POINT('',(-0.40705,-1.06687458785308E-14,-3.73478126690739));
#70673=CARTESIAN_POINT('Ctrl Pts',(-0.406704477435532,-0.000328489605546836,
-3.05978126690739));
#70674=CARTESIAN_POINT('Ctrl Pts',(-0.407035682029235,-0.0441750126328872,
-3.05721447960826));
#70675=CARTESIAN_POINT('Ctrl Pts',(-0.380281467477358,-0.223421781283086,
-3.04669829828972));
#70676=CARTESIAN_POINT('Ctrl Pts',(-0.118755506361991,-0.466457860652117,
-3.02823272295178));
#70677=CARTESIAN_POINT('Ctrl Pts',(0.3279772332983,-0.35230204001918,-3.00438454089354));
#70678=CARTESIAN_POINT('Ctrl Pts',(0.473748439217363,0.0851364820465625,
-2.9805363588353));
#70679=CARTESIAN_POINT('Ctrl Pts',(0.184794124598751,0.44445127173508,-2.95668817677707));
#70680=CARTESIAN_POINT('Ctrl Pts',(-0.26867312063451,0.396459958744006,
-2.93310314613443));
#70681=CARTESIAN_POINT('Ctrl Pts',(-0.407338799786674,0.130387800150095,
-2.9174675095112));
#70682=CARTESIAN_POINT('Ctrl Pts',(-0.407701968102319,-8.31109565068242E-5,
-2.90978126690739));
#70683=CARTESIAN_POINT('Ctrl Pts',(-0.407718443135198,-3.69130749903674E-5,
-3.03021873309261));
#70684=CARTESIAN_POINT('Ctrl Pts',(-0.407720987214861,-0.00200458601030759,
-3.03010280184093));
#70685=CARTESIAN_POINT('Ctrl Pts',(-0.406815955677249,-0.138892984777138,
-3.02203747656983));
#70686=CARTESIAN_POINT('Ctrl Pts',(-0.2545686693589,-0.408510181769555,
-3.00602275727932));
#70687=CARTESIAN_POINT('Ctrl Pts',(0.205748768093235,-0.435147353171444,
-2.98217457522109));
#70688=CARTESIAN_POINT('Ctrl Pts',(0.477265085335348,-0.0624805126738404,
-2.95832639316285));
#70689=CARTESIAN_POINT('Ctrl Pts',(0.310828915823958,0.367520286150906,
-2.93447821110462));
#70690=CARTESIAN_POINT('Ctrl Pts',(-0.140833011620641,0.460273655915389,
-2.91063002904639));
#70691=CARTESIAN_POINT('Ctrl Pts',(-0.385363902673548,0.210299061331091,
-2.89254353637572));
#70692=CARTESIAN_POINT('Ctrl Pts',(-0.40720506574647,0.0376968623643481,
-2.88240643772446));
#70693=CARTESIAN_POINT('Ctrl Pts',(-0.406879917492779,0.000366675793932139,
-2.88021873309261));
#70694=CARTESIAN_POINT('Origin',(0.,0.,-3.73478126690739));
#70695=CARTESIAN_POINT('',(-0.406515871833776,0.000234398840525714,-3.20978126690739));
#70696=CARTESIAN_POINT('',(-0.406769660729406,-0.000346827701298791,-3.18021873309261));
#70697=CARTESIAN_POINT('',(-0.40705,-1.06687458785308E-14,-3.73478126690739));
#70698=CARTESIAN_POINT('Ctrl Pts',(-0.406515871833776,0.000234398840525681,
-3.20978126690739));
#70699=CARTESIAN_POINT('Ctrl Pts',(-0.40607992506813,-0.0830599315404157,
-3.20491084372473));
#70700=CARTESIAN_POINT('Ctrl Pts',(-0.340605751677683,-0.302934358736486,
-3.19209102652267));
#70701=CARTESIAN_POINT('Ctrl Pts',(0.0193401667723502,-0.480949286387233,
-3.17132181530118));
#70702=CARTESIAN_POINT('Ctrl Pts',(0.414897370773675,-0.244019581286168,
-3.14747363324295));
#70703=CARTESIAN_POINT('Ctrl Pts',(0.429733826132711,0.216828851028994,
-3.12362545118471));
#70704=CARTESIAN_POINT('Ctrl Pts',(0.0502332080755313,0.478709177297012,
-3.09977726912648));
#70705=CARTESIAN_POINT('Ctrl Pts',(-0.329555527927946,0.32040500537278,
-3.07849587436737));
#70706=CARTESIAN_POINT('Ctrl Pts',(-0.406009934466403,0.091618587422811,
-3.06516387362767));
#70707=CARTESIAN_POINT('Ctrl Pts',(-0.406704477435532,-0.000328489605546836,
-3.05978126690739));
#70708=CARTESIAN_POINT('Ctrl Pts',(-0.406769660729406,-0.000346827701298773,
-3.18021873309261));
#70709=CARTESIAN_POINT('Ctrl Pts',(-0.407103008418297,-0.0416617513481845,
-3.1777991659574));
#70710=CARTESIAN_POINT('Ctrl Pts',(-0.382300719991004,-0.218324446081393,
-3.16743020480277));
#70711=CARTESIAN_POINT('Ctrl Pts',(-0.12736418971267,-0.464181203311474,
-3.14911184962874));
#70712=CARTESIAN_POINT('Ctrl Pts',(0.321403754809788,-0.358309005302331,
-3.12526366757049));
#70713=CARTESIAN_POINT('Ctrl Pts',(0.475242318068355,0.0763579342497911,
-3.10141548551227));
#70714=CARTESIAN_POINT('Ctrl Pts',(0.192984463138943,0.440956661874455,
-3.07756730345403));
#70715=CARTESIAN_POINT('Ctrl Pts',(-0.264128587748445,0.401115167263869,
-3.05383505264748));
#70716=CARTESIAN_POINT('Ctrl Pts',(-0.407546539933712,0.132918545043735,
-3.03805219586034));
#70717=CARTESIAN_POINT('Ctrl Pts',(-0.407718443135198,-3.69130749903674E-5,
-3.03021873309261));
#70718=CARTESIAN_POINT('Origin',(0.,0.,-3.73478126690739));
#70719=CARTESIAN_POINT('',(-0.407524236888043,0.000202371512057609,-3.35978126690739));
#70720=CARTESIAN_POINT('',(-0.406471795258815,0.000197138416556913,-3.33021873309261));
#70721=CARTESIAN_POINT('',(-0.40705,-1.06687458785308E-14,-3.73478126690739));
#70722=CARTESIAN_POINT('Ctrl Pts',(-0.407524236888043,0.000202371512057618,
-3.35978126690739));
#70723=CARTESIAN_POINT('Ctrl Pts',(-0.406696015914146,-0.121691487438068,
-3.3526072078412));
#70724=CARTESIAN_POINT('Ctrl Pts',(-0.283920138602621,-0.379991082756219,
-3.3374837547556));
#70725=CARTESIAN_POINT('Ctrl Pts',(0.155860105948259,-0.455439012791576,
-3.31441090765059));
#70726=CARTESIAN_POINT('Ctrl Pts',(0.467273406510021,-0.115419330027175,
-3.29056272559236));
#70727=CARTESIAN_POINT('Ctrl Pts',(0.349967170548287,0.330471523578635,
-3.26671454353412));
#70728=CARTESIAN_POINT('Ctrl Pts',(-0.0885127355860925,0.473133346833339,
-3.24286636147589));
#70729=CARTESIAN_POINT('Ctrl Pts',(-0.372795421348288,0.241157012369009,
-3.22388860260031));
#70730=CARTESIAN_POINT('Ctrl Pts',(-0.406791467470431,0.0528911813195563,
-3.21286023774414));
#70731=CARTESIAN_POINT('Ctrl Pts',(-0.406515871833776,0.000234398840525681,
-3.20978126690739));
#70732=CARTESIAN_POINT('Ctrl Pts',(-0.406471795258815,0.00019713841655692,
-3.33021873309261));
#70733=CARTESIAN_POINT('Ctrl Pts',(-0.406113950682387,-0.0805982389011809,
-3.32549553007387));
#70734=CARTESIAN_POINT('Ctrl Pts',(-0.343629442042593,-0.297885115520438,
-3.31282293303571));
#70735=CARTESIAN_POINT('Ctrl Pts',(0.0104433754015671,-0.481228201914669,
-3.29220094197814));
#70736=CARTESIAN_POINT('Ctrl Pts',(0.410310267884784,-0.251651262526424,
-3.26835275991991));
#70737=CARTESIAN_POINT('Ctrl Pts',(0.433672420198296,0.208841071520909,
-3.24450457786167));
#70738=CARTESIAN_POINT('Ctrl Pts',(0.0590798125780674,0.477698450045499,
-3.22065639580344));
#70739=CARTESIAN_POINT('Ctrl Pts',(-0.326218801964724,0.325400159805307,
-3.19922778088042));
#70740=CARTESIAN_POINT('Ctrl Pts',(-0.406007807509882,0.0940768285701207,
-3.18574855997681));
#70741=CARTESIAN_POINT('Ctrl Pts',(-0.406769660729406,-0.000346827701298773,
-3.18021873309261));
#70742=CARTESIAN_POINT('Origin',(4.52129938221115E-17,0.,-0.0249999999999999));
#70743=CARTESIAN_POINT('',(0.457029747534529,0.183521279061925,-0.0249999999999995));
#70744=CARTESIAN_POINT('Ctrl Pts',(-0.0460018146225333,-0.405020972964472,
-0.0249999999999997));
#70745=CARTESIAN_POINT('Ctrl Pts',(-0.0368688609768173,-0.407072845965971,
-0.0249999999999997));
#70746=CARTESIAN_POINT('Ctrl Pts',(-0.0276790887507462,-0.408785206362994,
-0.0249999999999986));
#70747=CARTESIAN_POINT('Ctrl Pts',(-0.0184481190379368,-0.410148694579132,
-0.0249999999999989));
#70748=CARTESIAN_POINT('Ctrl Pts',(-0.000736091208704569,-0.412764903057811,
-0.0249999999999994));
#70749=CARTESIAN_POINT('Ctrl Pts',(0.0171271945392099,-0.414098204546599,
-0.0250000000000001));
#70750=CARTESIAN_POINT('Ctrl Pts',(0.0350370752015178,-0.414220086012056,
-0.025));
#70751=CARTESIAN_POINT('Ctrl Pts',(0.0427871578566146,-0.414272827370261,
-0.0249999999999999));
#70752=CARTESIAN_POINT('Ctrl Pts',(0.0505460648098107,-0.414098441504754,
-0.0249999999999998));
#70753=CARTESIAN_POINT('Ctrl Pts',(0.058305636297932,-0.413701440723197,
-0.0249999999999998));
#70754=CARTESIAN_POINT('Ctrl Pts',(0.065639227935195,-0.413326234229375,
-0.0249999999999999));
#70755=CARTESIAN_POINT('Ctrl Pts',(0.0729656785645081,-0.412752439508174,
-0.0250000000000003));
#70756=CARTESIAN_POINT('Ctrl Pts',(0.0802705309395109,-0.411985704296353,
-0.0250000000000002));
#70757=CARTESIAN_POINT('Ctrl Pts',(0.0959965992620539,-0.410335057615571,
-0.0249999999999999));
#70758=CARTESIAN_POINT('Ctrl Pts',(0.111633086246646,-0.407790477600622,
-0.0250000000000002));
#70759=CARTESIAN_POINT('Ctrl Pts',(0.12711142996823,-0.404395753004662,
-0.0250000000000004));
#70760=CARTESIAN_POINT('Ctrl Pts',(0.137179327745643,-0.402187652394586,
-0.0250000000000005));
#70761=CARTESIAN_POINT('Ctrl Pts',(0.147180389015943,-0.399619615326678,
-0.0249999999999996));
#70762=CARTESIAN_POINT('Ctrl Pts',(0.15709598249321,-0.39670101471998,-0.0249999999999997));
#70763=CARTESIAN_POINT('Ctrl Pts',(0.16522061739264,-0.394309572956958,
-0.0249999999999997));
#70764=CARTESIAN_POINT('Ctrl Pts',(0.173292434393707,-0.391680787125226,
-0.0249999999999981));
#70765=CARTESIAN_POINT('Ctrl Pts',(0.18127262697246,-0.388829912162784,
-0.0249999999999984));
#70766=CARTESIAN_POINT('Ctrl Pts',(0.20372446637048,-0.380809129936173,
-0.0249999999999991));
#70767=CARTESIAN_POINT('Ctrl Pts',(0.22549026171249,-0.371025032773971,
-0.0250000000000013));
#70768=CARTESIAN_POINT('Ctrl Pts',(0.246351583123323,-0.35961031708094,
-0.0250000000000009));
#70769=CARTESIAN_POINT('Ctrl Pts',(0.259270215793116,-0.35254161245939,
-0.0250000000000007));
#70770=CARTESIAN_POINT('Ctrl Pts',(0.271842146168147,-0.344846493770231,
-0.0249999999999993));
#70771=CARTESIAN_POINT('Ctrl Pts',(0.284013996361614,-0.336546617664755,
-0.0249999999999994));
#70772=CARTESIAN_POINT('Ctrl Pts',(0.293911077818581,-0.32979788607564,
-0.0249999999999996));
#70773=CARTESIAN_POINT('Ctrl Pts',(0.303543649983073,-0.322649170726144,
-0.0249999999999999));
#70774=CARTESIAN_POINT('Ctrl Pts',(0.312881312926065,-0.315108752373828,
-0.025));
#70775=CARTESIAN_POINT('Ctrl Pts',(0.317290196363017,-0.311548458349062,
-0.025));
#70776=CARTESIAN_POINT('Ctrl Pts',(0.321632703673732,-0.307901054442145,
-0.0249999999999991));
#70777=CARTESIAN_POINT('Ctrl Pts',(0.325895512535387,-0.304176694866598,
-0.0249999999999992));
#70778=CARTESIAN_POINT('Ctrl Pts',(0.341087497923146,-0.290903658686291,
-0.0249999999999993));
#70779=CARTESIAN_POINT('Ctrl Pts',(0.355302925077213,-0.276627230860661,
-0.0250000000000004));
#70780=CARTESIAN_POINT('Ctrl Pts',(0.368414610711014,-0.261411535021156,
-0.0250000000000003));
#70781=CARTESIAN_POINT('Ctrl Pts',(0.38096744800188,-0.246844364981002,
-0.0250000000000003));
#70782=CARTESIAN_POINT('Ctrl Pts',(0.392509163584889,-0.231416085721514,
-0.0250000000000002));
#70783=CARTESIAN_POINT('Ctrl Pts',(0.403021877045189,-0.215260169684606,
-0.0250000000000003));
#70784=CARTESIAN_POINT('Ctrl Pts',(0.41029062462888,-0.204089573615468,
-0.0250000000000003));
#70785=CARTESIAN_POINT('Ctrl Pts',(0.417067159241788,-0.192570686603153,
-0.0249999999999998));
#70786=CARTESIAN_POINT('Ctrl Pts',(0.423341039846872,-0.180743491987121,
-0.0249999999999996));
#70787=CARTESIAN_POINT('Ctrl Pts',(0.426046091107006,-0.175644069522175,
-0.0249999999999995));
#70788=CARTESIAN_POINT('Ctrl Pts',(0.428657339542585,-0.170487505211596,
-0.0249999999999992));
#70789=CARTESIAN_POINT('Ctrl Pts',(0.431168090704968,-0.165289798304669,
-0.0249999999999992));
#70790=CARTESIAN_POINT('Ctrl Pts',(0.441952230009222,-0.142964688518082,
-0.0249999999999993));
#70791=CARTESIAN_POINT('Ctrl Pts',(0.450916595356233,-0.119826320055446,
-0.0249999999999978));
#70792=CARTESIAN_POINT('Ctrl Pts',(0.458031178347495,-0.0961506920430363,
-0.0249999999999986));
#70793=CARTESIAN_POINT('Ctrl Pts',(0.462087263293214,-0.0826530129127887,
-0.0249999999999991));
#70794=CARTESIAN_POINT('Ctrl Pts',(0.465541456021857,-0.0689799331539447,
-0.0249999999999998));
#70795=CARTESIAN_POINT('Ctrl Pts',(0.468382162239584,-0.0551781242986939,
-0.0249999999999996));
#70796=CARTESIAN_POINT('Ctrl Pts',(0.471104443522198,-0.0419516928999102,
-0.0249999999999995));
#70797=CARTESIAN_POINT('Ctrl Pts',(0.473263317184127,-0.0286069608577007,
-0.0249999999999989));
#70798=CARTESIAN_POINT('Ctrl Pts',(0.474858192805233,-0.0151757738305842,
-0.024999999999999));
#70799=CARTESIAN_POINT('Ctrl Pts',(0.475856795922803,-0.00676607400168343,
-0.0249999999999991));
#70800=CARTESIAN_POINT('Ctrl Pts',(0.476634321335288,0.0016835602057796,
-0.0250000000000001));
#70801=CARTESIAN_POINT('Ctrl Pts',(0.477188356191574,0.0101317298598468,
-0.0250000000000001));
#70802=CARTESIAN_POINT('Ctrl Pts',(0.478859492768636,0.0356139628961899,
-0.0250000000000002));
#70803=CARTESIAN_POINT('Ctrl Pts',(0.478509242868913,0.0611272410931792,
-0.0250000000000001));
#70804=CARTESIAN_POINT('Ctrl Pts',(0.476172029705562,0.0864508239821215,
-0.0249999999999998));
#70805=CARTESIAN_POINT('Ctrl Pts',(0.473839980058189,0.111718460444394,
-0.0249999999999995));
#70806=CARTESIAN_POINT('Ctrl Pts',(0.469529905743689,0.136798534533325,
-0.025));
#70807=CARTESIAN_POINT('Ctrl Pts',(0.46322590299162,0.161480326316489,-0.0250000000000002));
#70808=CARTESIAN_POINT('Ctrl Pts',(0.461339801487617,0.168864898696068,
-0.0250000000000003));
#70809=CARTESIAN_POINT('Ctrl Pts',(0.459274862212137,0.17621380430208,-0.0249999999999995));
#70810=CARTESIAN_POINT('Ctrl Pts',(0.457029747534529,0.183521279061925,
-0.0249999999999995));
#70811=CARTESIAN_POINT('',(-0.4925,-6.03138548580071E-17,-0.0249999999999999));
#70812=CARTESIAN_POINT('Origin',(0.,0.,-0.0249999999999999));
#70813=CARTESIAN_POINT('',(0.134559949224566,0.474484556402355,-0.0249999999999999));
#70814=CARTESIAN_POINT('Origin',(0.,0.,-0.0249999999999999));
#70815=CARTESIAN_POINT('Ctrl Pts',(0.134559949224566,0.474484556402355,
-0.0249999999999999));
#70816=CARTESIAN_POINT('Ctrl Pts',(0.123555094791079,0.476693790868335,
-0.025));
#70817=CARTESIAN_POINT('Ctrl Pts',(0.112488500107867,0.478496855056247,
-0.0250000000000006));
#70818=CARTESIAN_POINT('Ctrl Pts',(0.101375304595012,0.479878948430273,
-0.0250000000000004));
#70819=CARTESIAN_POINT('Ctrl Pts',(0.0820161039435544,0.482286556837401,
-0.0250000000000001));
#70820=CARTESIAN_POINT('Ctrl Pts',(0.0625152503388465,0.483417645176772,
-0.0249999999999985));
#70821=CARTESIAN_POINT('Ctrl Pts',(0.0429779460829366,0.483316943501375,
-0.0249999999999985));
#70822=CARTESIAN_POINT('Ctrl Pts',(0.0325576452803804,0.483263233852632,
-0.0249999999999985));
#70823=CARTESIAN_POINT('Ctrl Pts',(0.0221270158330046,0.482858819240042,
-0.0249999999999989));
#70824=CARTESIAN_POINT('Ctrl Pts',(0.0117026104786621,0.482108568565393,
-0.0249999999999988));
#70825=CARTESIAN_POINT('Ctrl Pts',(0.00498825037415073,0.481625332061534,
-0.0249999999999987));
#70826=CARTESIAN_POINT('Ctrl Pts',(-0.0017201083185829,0.480998723263594,
-0.0249999999999994));
#70827=CARTESIAN_POINT('Ctrl Pts',(-0.00840971123782733,0.480231503030802,
-0.0249999999999995));
#70828=CARTESIAN_POINT('Ctrl Pts',(-0.03375204596074,0.47732502977965,-0.0249999999999997));
#70829=CARTESIAN_POINT('Ctrl Pts',(-0.0588627694554139,0.472401938366701,
-0.0249999999999997));
#70830=CARTESIAN_POINT('Ctrl Pts',(-0.0835002259753155,0.465549384270615,
-0.0250000000000004));
#70831=CARTESIAN_POINT('Ctrl Pts',(-0.0924179898816985,0.463069036531178,
-0.0250000000000006));
#70832=CARTESIAN_POINT('Ctrl Pts',(-0.101273541185288,0.460335451608263,
-0.0250000000000007));
#70833=CARTESIAN_POINT('Ctrl Pts',(-0.110054517088707,0.457351333110056,
-0.0250000000000009));
#70834=CARTESIAN_POINT('Ctrl Pts',(-0.115349721097155,0.455551816016833,
-0.0250000000000009));
#70835=CARTESIAN_POINT('Ctrl Pts',(-0.120616282206451,0.453661581487259,
-0.0249999999999976));
#70836=CARTESIAN_POINT('Ctrl Pts',(-0.12584278956843,0.451684861751622,
-0.0249999999999977));
#70837=CARTESIAN_POINT('Ctrl Pts',(-0.149125860671454,0.442878960799412,
-0.0249999999999981));
#70838=CARTESIAN_POINT('Ctrl Pts',(-0.171665873862567,0.432343672613944,
-0.0249999999999992));
#70839=CARTESIAN_POINT('Ctrl Pts',(-0.193238606369979,0.42015887610055,
-0.0249999999999992));
#70840=CARTESIAN_POINT('Ctrl Pts',(-0.21426277833423,0.40828391973334,-0.0249999999999992));
#70841=CARTESIAN_POINT('Ctrl Pts',(-0.234369248412146,0.394841501860522,
-0.0249999999999994));
#70842=CARTESIAN_POINT('Ctrl Pts',(-0.253316286172159,0.379871074180984,
-0.0249999999999996));
#70843=CARTESIAN_POINT('Ctrl Pts',(-0.258074354348964,0.376111630808495,
-0.0249999999999996));
#70844=CARTESIAN_POINT('Ctrl Pts',(-0.262759091303972,0.372255683264206,
-0.0249999999999996));
#70845=CARTESIAN_POINT('Ctrl Pts',(-0.267366205423779,0.368303587897705,
-0.0249999999999997));
#70846=CARTESIAN_POINT('Ctrl Pts',(-0.272131127547925,0.364216120958777,
-0.0249999999999997));
#70847=CARTESIAN_POINT('Ctrl Pts',(-0.276807128535211,0.36003072093939,
-0.0249999999999994));
#70848=CARTESIAN_POINT('Ctrl Pts',(-0.281384804472264,0.35575357543162,
-0.0249999999999993));
#70849=CARTESIAN_POINT('Ctrl Pts',(-0.294787805690782,0.343230498822286,
-0.0249999999999992));
#70850=CARTESIAN_POINT('Ctrl Pts',(-0.307364443444733,0.329908587482838,
-0.0249999999999991));
#70851=CARTESIAN_POINT('Ctrl Pts',(-0.319013982928522,0.31581173345222,
-0.0249999999999992));
#70852=CARTESIAN_POINT('Ctrl Pts',(-0.332336765116745,0.299690124864134,
-0.0249999999999993));
#70853=CARTESIAN_POINT('Ctrl Pts',(-0.344447706547327,0.282554571833339,
-0.0249999999999993));
#70854=CARTESIAN_POINT('Ctrl Pts',(-0.355285026905852,0.264573570396947,
-0.024999999999999));
#70855=CARTESIAN_POINT('Ctrl Pts',(-0.36027217617748,0.256299021407897,
-0.0249999999999989));
#70856=CARTESIAN_POINT('Ctrl Pts',(-0.364989210369154,0.247845308384308,
-0.0250000000000001));
#70857=CARTESIAN_POINT('Ctrl Pts',(-0.369427973343093,0.239228558655422,
-0.0250000000000002));
#70858=CARTESIAN_POINT('Ctrl Pts',(-0.372691078878274,0.23289405422239,
-0.0250000000000002));
#70859=CARTESIAN_POINT('Ctrl Pts',(-0.375804878242441,0.226468396851928,
-0.0250000000000003));
#70860=CARTESIAN_POINT('Ctrl Pts',(-0.378755924034929,0.219981221274517,
-0.0250000000000002));
#70861=CARTESIAN_POINT('Ctrl Pts',(-0.388473620732812,0.198619165542392,
-0.0249999999999998));
#70862=CARTESIAN_POINT('Ctrl Pts',(-0.396457052544794,0.176542967218711,
-0.0250000000000005));
#70863=CARTESIAN_POINT('Ctrl Pts',(-0.402628366384551,0.153995847400014,
-0.025));
#70864=CARTESIAN_POINT('Ctrl Pts',(-0.405848553416808,0.142230776826689,
-0.0249999999999998));
#70865=CARTESIAN_POINT('Ctrl Pts',(-0.40857451584816,0.130337276741726,
-0.0249999999999988));
#70866=CARTESIAN_POINT('Ctrl Pts',(-0.410789527386875,0.118349752967864,
-0.0249999999999986));
#70867=CARTESIAN_POINT('Ctrl Pts',(-0.413173307917742,0.105448860450609,
-0.0249999999999984));
#70868=CARTESIAN_POINT('Ctrl Pts',(-0.414965336322946,0.0924389960516608,
-0.0249999999999991));
#70869=CARTESIAN_POINT('Ctrl Pts',(-0.416156410828275,0.0793583313213072,
-0.0249999999999989));
#70870=CARTESIAN_POINT('Ctrl Pts',(-0.41678540546089,0.0724505620175296,
-0.0249999999999988));
#70871=CARTESIAN_POINT('Ctrl Pts',(-0.417246607084851,0.0655199159985511,
-0.0250000000000001));
#70872=CARTESIAN_POINT('Ctrl Pts',(-0.417537811172664,0.0585969702267026,
-0.025));
#70873=CARTESIAN_POINT('Ctrl Pts',(-0.418493406177842,0.0358791146829457,
-0.0249999999999998));
#70874=CARTESIAN_POINT('Ctrl Pts',(-0.41762892133668,0.0131899923548943,
-0.0249999999999987));
#70875=CARTESIAN_POINT('Ctrl Pts',(-0.414931126870213,-0.00927360260191209,
-0.024999999999999));
#70876=CARTESIAN_POINT('Ctrl Pts',(-0.412300309655844,-0.0311795013067703,
-0.0249999999999994));
#70877=CARTESIAN_POINT('Ctrl Pts',(-0.407925720268869,-0.0528720434064392,
-0.0250000000000002));
#70878=CARTESIAN_POINT('Ctrl Pts',(-0.401749711262537,-0.0741500679289064,
-0.0250000000000002));
#70879=CARTESIAN_POINT('Ctrl Pts',(-0.400376913363202,-0.0788797286752727,
-0.0250000000000002));
#70880=CARTESIAN_POINT('Ctrl Pts',(-0.39891494101082,-0.0835887978684164,
-0.0249999999999999));
#70881=CARTESIAN_POINT('Ctrl Pts',(-0.39736287274916,-0.0882748540669144,
-0.0249999999999999));
#70882=CARTESIAN_POINT('Ctrl Pts',(-0.179217368492187,0.365473442716069,
-3.50683458050225));
#70883=CARTESIAN_POINT('Ctrl Pts',(-0.240065670223399,0.33563523495891,
-3.50285988349255));
#70884=CARTESIAN_POINT('Ctrl Pts',(-0.345646884548746,0.244990880907642,
-3.49491048947314));
#70885=CARTESIAN_POINT('Ctrl Pts',(-0.448647636125016,-0.0162619182297498,
-3.47901170143431));
#70886=CARTESIAN_POINT('Ctrl Pts',(-0.305996566448462,-0.371515294606295,
-3.45913821638579));
#70887=CARTESIAN_POINT('Ctrl Pts',(0.147593574246178,-0.458419355808066,
-3.43529003432755));
#70888=CARTESIAN_POINT('Ctrl Pts',(0.464962259161517,-0.123953347438615,
-3.41144185226931));
#70889=CARTESIAN_POINT('Ctrl Pts',(0.356070675898753,0.323893827689701,
-3.38759367021108));
#70890=CARTESIAN_POINT('Ctrl Pts',(-0.0797710380057583,0.474714264786181,
-3.36374548815284));
#70891=CARTESIAN_POINT('Ctrl Pts',(-0.44230355372976,0.189825171767689,
-3.33989730609462));
#70892=CARTESIAN_POINT('Ctrl Pts',(-0.399022082550972,-0.269202152090369,
-3.31604912403637));
#70893=CARTESIAN_POINT('Ctrl Pts',(0.0104433754015671,-0.481228201914669,
-3.29220094197814));
#70894=CARTESIAN_POINT('Ctrl Pts',(0.410310267884784,-0.251651262526424,
-3.26835275991991));
#70895=CARTESIAN_POINT('Ctrl Pts',(0.433672420198296,0.208841071520909,
-3.24450457786167));
#70896=CARTESIAN_POINT('Ctrl Pts',(0.0590798125780674,0.477698450045499,
-3.22065639580344));
#70897=CARTESIAN_POINT('Ctrl Pts',(-0.369723987360064,0.30820371761162,
-3.1968082137452));
#70898=CARTESIAN_POINT('Ctrl Pts',(-0.459259315099757,-0.144106794284832,
-3.17296003168697));
#70899=CARTESIAN_POINT('Ctrl Pts',(-0.12736418971267,-0.464181203311474,
-3.14911184962874));
#70900=CARTESIAN_POINT('Ctrl Pts',(0.321403754809788,-0.358309005302331,
-3.12526366757049));
#70901=CARTESIAN_POINT('Ctrl Pts',(0.475242318068355,0.0763579342497911,
-3.10141548551227));
#70902=CARTESIAN_POINT('Ctrl Pts',(0.192984463138943,0.440956661874455,
-3.07756730345403));
#70903=CARTESIAN_POINT('Ctrl Pts',(-0.266361569718098,0.400920542894828,
-3.0537191213958));
#70904=CARTESIAN_POINT('Ctrl Pts',(-0.481286411713864,-0.00701204226000944,
-3.02987093933756));
#70905=CARTESIAN_POINT('Ctrl Pts',(-0.2545686693589,-0.408510181769555,
-3.00602275727932));
#70906=CARTESIAN_POINT('Ctrl Pts',(0.205748768093235,-0.435147353171444,
-2.98217457522109));
#70907=CARTESIAN_POINT('Ctrl Pts',(0.477265085335348,-0.0624805126738404,
-2.95832639316285));
#70908=CARTESIAN_POINT('Ctrl Pts',(0.310828915823958,0.367520286150906,
-2.93447821110462));
#70909=CARTESIAN_POINT('Ctrl Pts',(-0.140833011620641,0.460273655915389,
-2.91063002904639));
#70910=CARTESIAN_POINT('Ctrl Pts',(-0.463262424270052,0.130666376597655,
-2.88678184698815));
#70911=CARTESIAN_POINT('Ctrl Pts',(-0.360588605408013,-0.318844214750719,
-2.86293366492992));
#70912=CARTESIAN_POINT('Ctrl Pts',(0.0729719274013494,-0.475773973046388,
-2.83908548287168));
#70913=CARTESIAN_POINT('Ctrl Pts',(0.439571272608378,-0.196119534836683,
-2.81523730081345));
#70914=CARTESIAN_POINT('Ctrl Pts',(0.402807084347494,0.263499959076195,
-2.79138911875521));
#70915=CARTESIAN_POINT('Ctrl Pts',(-0.00358473645388183,0.481324137455872,
-2.76754093669698));
#70916=CARTESIAN_POINT('Ctrl Pts',(-0.406687097619119,0.257471125113484,
-2.74369275463875));
#70917=CARTESIAN_POINT('Ctrl Pts',(-0.436601411880274,-0.202644967317561,
-2.71984457258051));
#70918=CARTESIAN_POINT('Ctrl Pts',(-0.0658774242972122,-0.476808075228433,
-2.69599639052228));
#70919=CARTESIAN_POINT('Ctrl Pts',(0.365297626161182,-0.313438063988078,
-2.67214820846404));
#70920=CARTESIAN_POINT('Ctrl Pts',(0.461264826549058,0.137551937187166,
-2.64830002640581));
#70921=CARTESIAN_POINT('Ctrl Pts',(0.133961850108581,0.462320233551161,
-2.62445184434757));
#70922=CARTESIAN_POINT('Ctrl Pts',(-0.316268461607078,0.362849880567804,
-2.60060366228934));
#70923=CARTESIAN_POINT('Ctrl Pts',(-0.47628152725319,-0.0695821991079605,
-2.5767554802311));
#70924=CARTESIAN_POINT('Ctrl Pts',(-0.199244649661891,-0.438163605536162,
-2.55290729817287));
#70925=CARTESIAN_POINT('Ctrl Pts',(0.260624980917576,-0.404673195253975,
-2.52905911611463));
#70926=CARTESIAN_POINT('Ctrl Pts',(0.481337460529596,0.000157245861404591,
-2.5052109340564));
#70927=CARTESIAN_POINT('Ctrl Pts',(0.260360523766897,0.404843393547639,
-2.48136275199817));
#70928=CARTESIAN_POINT('Ctrl Pts',(-0.199530890300541,0.438033331438621,
-2.45751456993993));
#70929=CARTESIAN_POINT('Ctrl Pts',(-0.476326888547635,0.0692709959641985,
-2.4336663878817));
#70930=CARTESIAN_POINT('Ctrl Pts',(-0.3160313186988,-0.363056443596366,
-2.40981820582346));
#70931=CARTESIAN_POINT('Ctrl Pts',(0.134263887909296,-0.462232608151807,
-2.38597002376523));
#70932=CARTESIAN_POINT('Ctrl Pts',(0.461354600469472,-0.137250531004422,
-2.36212184170699));
#70933=CARTESIAN_POINT('Ctrl Pts',(0.365092757010119,0.313676671772215,
-2.33827365964876));
#70934=CARTESIAN_POINT('Ctrl Pts',(-0.0661889425581167,0.476764931091184,
-2.31442547759052));
#70935=CARTESIAN_POINT('Ctrl Pts',(-0.436733720930171,0.202359661587554,
-2.29057729553229));
#70936=CARTESIAN_POINT('Ctrl Pts',(-0.40651878677836,-0.257736787501498,
-2.26672911347405));
#70937=CARTESIAN_POINT('Ctrl Pts',(-0.00327025270698847,-0.481326376882232,
-2.24288093141582));
#70938=CARTESIAN_POINT('Ctrl Pts',(0.402979161470327,-0.263236720569178,
-2.21903274935758));
#70939=CARTESIAN_POINT('Ctrl Pts',(0.4394430400586,0.196406695861922,-2.19518456729935));
#70940=CARTESIAN_POINT('Ctrl Pts',(0.0726610551733367,0.47582154921403,
-2.17133638524111));
#70941=CARTESIAN_POINT('Ctrl Pts',(-0.3607968518755,0.318608548711537,-2.14748820318288));
#70942=CARTESIAN_POINT('Ctrl Pts',(-0.463176951767192,-0.13096903064082,
-2.12364002112464));
#70943=CARTESIAN_POINT('Ctrl Pts',(-0.14053225246876,-0.460365573920769,
-2.09979183906641));
#70944=CARTESIAN_POINT('Ctrl Pts',(0.311068976634055,-0.367317121042818,
-2.07594365700817));
#70945=CARTESIAN_POINT('Ctrl Pts',(0.477224160065282,0.0627923298288068,
-2.05209547494994));
#70946=CARTESIAN_POINT('Ctrl Pts',(0.205464412655191,0.435281691284622,
-2.02824729289171));
#70947=CARTESIAN_POINT('Ctrl Pts',(-0.254835525272372,0.408343765342997,
-2.00439911083347));
#70948=CARTESIAN_POINT('Ctrl Pts',(-0.481290887078107,0.00669758545379794,
-1.98055092877524));
#70949=CARTESIAN_POINT('Ctrl Pts',(-0.266099569678556,-0.401094495913658,
-1.956702746717));
#70950=CARTESIAN_POINT('Ctrl Pts',(0.193272542416614,-0.440830466260172,
-1.93285456465877));
#70951=CARTESIAN_POINT('Ctrl Pts',(0.475292082851708,-0.0760474300277662,
-1.90900638260053));
#70952=CARTESIAN_POINT('Ctrl Pts',(0.321169623344976,0.358518965573356,
-1.8851582005423));
#70953=CARTESIAN_POINT('Ctrl Pts',(-0.127667532450826,0.464097809511379,
-1.86131001848406));
#70954=CARTESIAN_POINT('Ctrl Pts',(-0.459353204054721,0.143806848098432,
-1.83746183642583));
#70955=CARTESIAN_POINT('Ctrl Pts',(-0.369522859877177,-0.308445508418479,
-1.8136136543676));
#70956=CARTESIAN_POINT('Ctrl Pts',(0.0593925331488187,-0.477659190889811,
-1.78976547230936));
#70957=CARTESIAN_POINT('Ctrl Pts',(0.433807590226198,-0.208558745435148,
-1.76591729025113));
#70958=CARTESIAN_POINT('Ctrl Pts',(0.410148038410438,0.251921341341723,
-1.74206910819289));
#70959=CARTESIAN_POINT('Ctrl Pts',(0.0101245785925387,0.481230992916775,
-1.71822092613466));
#70960=CARTESIAN_POINT('Ctrl Pts',(-0.39918949244157,0.268948925931271,
-1.69437274407642));
#70961=CARTESIAN_POINT('Ctrl Pts',(-0.442195539692441,-0.190128588885139,
-1.67052456201819));
#70962=CARTESIAN_POINT('Ctrl Pts',(-0.0794299488178135,-0.474738516307812,
-1.64667637995995));
#70963=CARTESIAN_POINT('Ctrl Pts',(0.356222900192536,-0.323714412737155,
-1.62282819790172));
#70964=CARTESIAN_POINT('Ctrl Pts',(0.464995134691316,0.124359560745234,
-1.59898001584348));
#70965=CARTESIAN_POINT('Ctrl Pts',(0.147074151851645,0.458317542204598,
-1.57513183378525));
#70966=CARTESIAN_POINT('Ctrl Pts',(-0.305806400151182,0.371709861668907,
-1.55128365172701));
#70967=CARTESIAN_POINT('Ctrl Pts',(-0.478070001506081,-0.0559897249083942,
-1.52743546966878));
#70968=CARTESIAN_POINT('Ctrl Pts',(-0.211642503026044,-0.432311492500735,
-1.50358728761054));
#70969=CARTESIAN_POINT('Ctrl Pts',(0.24899438347629,-0.411931514493132,
-1.47973910555231));
#70970=CARTESIAN_POINT('Ctrl Pts',(0.481146697435232,-0.0135510583539467,
-1.45589092349407));
#70971=CARTESIAN_POINT('Ctrl Pts',(0.271784644847739,0.397264247649257,
-1.43204274143584));
#70972=CARTESIAN_POINT('Ctrl Pts',(-0.186974994684948,0.443538191137929,
-1.40819455937761));
#70973=CARTESIAN_POINT('Ctrl Pts',(-0.474160877651511,0.0828084400293316,
-1.38434637731937));
#70974=CARTESIAN_POINT('Ctrl Pts',(-0.32624278785187,-0.353908772157435,
-1.36049819526114));
#70975=CARTESIAN_POINT('Ctrl Pts',(0.121045283258203,-0.465868881807192,
-1.3366500132029));
#70976=CARTESIAN_POINT('Ctrl Pts',(0.457258640884715,-0.150333998056345,
-1.31280183114467));
#70977=CARTESIAN_POINT('Ctrl Pts',(0.373878015523797,0.303151785650903,
-1.28895364908643));
#70978=CARTESIAN_POINT('Ctrl Pts',(-0.0525840776504784,0.478456571083512,
-1.2651054670282));
#70979=CARTESIAN_POINT('Ctrl Pts',(-0.430793473969433,0.214715529062733,
-1.24125728496997));
#70980=CARTESIAN_POINT('Ctrl Pts',(-0.413694103158059,-0.246054800090533,
-1.21740910291173));
#70981=CARTESIAN_POINT('Ctrl Pts',(-0.0169768509947866,-0.481038004907766,
-1.19356092085349));
#70982=CARTESIAN_POINT('Ctrl Pts',(0.395318859158266,-0.274606582639873,
-1.16971273879526));
#70983=CARTESIAN_POINT('Ctrl Pts',(0.444858352516096,0.183811919722327,
-1.14586455673703));
#70984=CARTESIAN_POINT('Ctrl Pts',(0.0861827323523932,0.473559196172579,
-1.12201637467879));
#70985=CARTESIAN_POINT('Ctrl Pts',(-0.35157669880833,0.328754620485218,
-1.09816819262056));
#70986=CARTESIAN_POINT('Ctrl Pts',(-0.466719006554749,-0.117724868043632,
-1.07432001056232));
#70987=CARTESIAN_POINT('Ctrl Pts',(-0.153586221418629,-0.456176553787775,
-1.05047182850409));
#70988=CARTESIAN_POINT('Ctrl Pts',(0.300481799522643,-0.376027211503337,
-1.02662364644585));
#70989=CARTESIAN_POINT('Ctrl Pts',(0.478818880020692,0.0491757640619698,
-1.00277546438762));
#70990=CARTESIAN_POINT('Ctrl Pts',(0.217777667724211,0.429253611605008,
-0.978927282329384));
#70991=CARTESIAN_POINT('Ctrl Pts',(-0.243102740239076,0.415435715031318,
-0.955079100271148));
#70992=CARTESIAN_POINT('Ctrl Pts',(-0.480904920845782,0.0204017828066685,
-0.931230918212915));
#70993=CARTESIAN_POINT('Ctrl Pts',(-0.277414596218298,-0.393353425611565,
-0.907382736154679));
#70994=CARTESIAN_POINT('Ctrl Pts',(0.180639524384169,-0.446155956886755,
-0.883534554096447));
#70995=CARTESIAN_POINT('Ctrl Pts',(0.472933502380155,-0.0895526546900201,
-0.85968637203821));
#70996=CARTESIAN_POINT('Ctrl Pts',(0.331249783271615,0.34922679839552,-0.835838189979976));
#70997=CARTESIAN_POINT('Ctrl Pts',(-0.114398483465715,0.467545465827366,
-0.811990007921742));
#70998=CARTESIAN_POINT('Ctrl Pts',(-0.455071335783922,0.15683065703141,
-0.788141825863506));
#70999=CARTESIAN_POINT('Ctrl Pts',(-0.378157340626862,-0.29779657715142,
-0.764293643805273));
#71000=CARTESIAN_POINT('Ctrl Pts',(0.0457649569583762,-0.479156909945254,
-0.740445461747037));
#71001=CARTESIAN_POINT('Ctrl Pts',(0.427691983500448,-0.220828763743674,
-0.716597279688803));
#71002=CARTESIAN_POINT('Ctrl Pts',(0.417156261778369,0.240138353613306,
-0.692749097630569));
#71003=CARTESIAN_POINT('Ctrl Pts',(0.0238256801714527,0.480747451989572,
-0.668900915572333));
#71004=CARTESIAN_POINT('Ctrl Pts',(-0.391368046757949,0.28020854321486,
-0.6450527335141));
#71005=CARTESIAN_POINT('Ctrl Pts',(-0.447430938281907,-0.177457969559079,
-0.621204551455864));
#71006=CARTESIAN_POINT('Ctrl Pts',(-0.0929180364960938,-0.472283827945071,
-0.59735636939763));
#71007=CARTESIAN_POINT('Ctrl Pts',(0.346859190705059,-0.333728149797965,
-0.573508187339396));
#71008=CARTESIAN_POINT('Ctrl Pts',(0.468348216506024,0.11106629839706,-0.549660005281161));
#71009=CARTESIAN_POINT('Ctrl Pts',(0.160067142708905,0.453943042521375,
-0.525811823222927));
#71010=CARTESIAN_POINT('Ctrl Pts',(-0.29509625915887,0.380268295638099,
-0.501963641164692));
#71011=CARTESIAN_POINT('Ctrl Pts',(-0.479470635149994,-0.0423518307353366,
-0.478115459106457));
#71012=CARTESIAN_POINT('Ctrl Pts',(-0.223868678851143,-0.426108666062932,
-0.454267277048223));
#71013=CARTESIAN_POINT('Ctrl Pts',(0.23716182206986,-0.418855661485411,
-0.430419094989988));
#71014=CARTESIAN_POINT('Ctrl Pts',(0.48056554579435,-0.0272483592525269,
-0.406570912931754));
#71015=CARTESIAN_POINT('Ctrl Pts',(0.282988398107527,0.389362803648974,
-0.382722730873519));
#71016=CARTESIAN_POINT('Ctrl Pts',(-0.174267639443746,0.448683269698852,
-0.358874548815284));
#71017=CARTESIAN_POINT('Ctrl Pts',(-0.471609778146528,0.0962786348866224,
-0.33502636675705));
#71018=CARTESIAN_POINT('Ctrl Pts',(-0.336190415025481,-0.34447385717225,
-0.311178184698814));
#71019=CARTESIAN_POINT('Ctrl Pts',(0.107730056479299,-0.469127483873643,
-0.28733000264058));
#71020=CARTESIAN_POINT('Ctrl Pts',(0.452788709608233,-0.16329500394726,
-0.263481820582346));
#71021=CARTESIAN_POINT('Ctrl Pts',(0.382365767560564,0.292380003087804,
-0.239633638524111));
#71022=CARTESIAN_POINT('Ctrl Pts',(-0.0389476842058911,0.479761919026928,
-0.215785456465877));
#71023=CARTESIAN_POINT('Ctrl Pts',(-0.424482390454294,0.226893652782127,
-0.191937274407642));
#71024=CARTESIAN_POINT('Ctrl Pts',(-0.42057479669623,-0.234166376920184,
-0.168089092349408));
#71025=CARTESIAN_POINT('Ctrl Pts',(-0.0305910094676718,-0.480372488794092,
-0.144240910291172));
#71026=CARTESIAN_POINT('Ctrl Pts',(0.387186688863383,-0.285728547318658,
-0.120392728232938));
#71027=CARTESIAN_POINT('Ctrl Pts',(0.450204815655376,0.171019861124231,
-0.0965445461747034));
#71028=CARTESIAN_POINT('Ctrl Pts',(0.0990560712614088,0.471004678905531,
-0.0726963641164688));
#71029=CARTESIAN_POINT('Ctrl Pts',(-0.267488470034939,0.360553837565826,
-0.0528228790679404));
#71030=CARTESIAN_POINT('Ctrl Pts',(-0.407203348846865,0.116951841430801,
-0.0369240910291168));
#71031=CARTESIAN_POINT('Ctrl Pts',(-0.412059904948337,-0.022117226311166,
-0.0289746970097056));
#71032=CARTESIAN_POINT('Ctrl Pts',(-0.39736287274916,-0.0882748540669144,
-0.0249999999999999));
#71033=CARTESIAN_POINT('Ctrl Pts',(-0.191758108071809,0.391047455474607,
-3.49038972033484));
#71034=CARTESIAN_POINT('Ctrl Pts',(-0.256864271149238,0.359121318427148,
-3.48641502332513));
#71035=CARTESIAN_POINT('Ctrl Pts',(-0.36983353343274,0.262134123567069,
-3.47846562930572));
#71036=CARTESIAN_POINT('Ctrl Pts',(-0.480041765025547,-0.0173998463407366,
-3.46256684126689));
#71037=CARTESIAN_POINT('Ctrl Pts',(-0.327408683389887,-0.397512086093095,
-3.44269335621837));
#71038=CARTESIAN_POINT('Ctrl Pts',(0.157921438078905,-0.490497261023478,
-3.41884517416013));
#71039=CARTESIAN_POINT('Ctrl Pts',(0.497498004193129,-0.132626985843913,
-3.39499699210189));
#71040=CARTESIAN_POINT('Ctrl Pts',(0.380986729827876,0.346558305907843,
-3.37114881004367));
#71041=CARTESIAN_POINT('Ctrl Pts',(-0.0853530182682902,0.507932406640973,
-3.34730062798542));
#71042=CARTESIAN_POINT('Ctrl Pts',(-0.473253755315321,0.20310819263126,
-3.3234524459272));
#71043=CARTESIAN_POINT('Ctrl Pts',(-0.426943662171806,-0.288039579020821,
-3.29960426386895));
#71044=CARTESIAN_POINT('Ctrl Pts',(0.0111741508411632,-0.514902156673387,
-3.27575608181073));
#71045=CARTESIAN_POINT('Ctrl Pts',(0.439021738540113,-0.269260565546433,
-3.25190789975249));
#71046=CARTESIAN_POINT('Ctrl Pts',(0.464018658011788,0.223454730417408,
-3.22805971769425));
#71047=CARTESIAN_POINT('Ctrl Pts',(0.0632139238541575,0.51112541033407,
-3.20421153563602));
#71048=CARTESIAN_POINT('Ctrl Pts',(-0.395595432080138,0.329770280007651,
-3.18036335357778));
#71049=CARTESIAN_POINT('Ctrl Pts',(-0.491395996486379,-0.154190670607673,
-3.15651517151955));
#71050=CARTESIAN_POINT('Ctrl Pts',(-0.136276501886399,-0.496662293941589,
-3.13266698946132));
#71051=CARTESIAN_POINT('Ctrl Pts',(0.343893990119533,-0.383381686384168,
-3.10881880740308));
#71052=CARTESIAN_POINT('Ctrl Pts',(0.508497410464,0.0817010824966437,-3.08497062534485));
#71053=CARTESIAN_POINT('Ctrl Pts',(0.206488555490598,0.47181261467073,-3.06112244328661));
#71054=CARTESIAN_POINT('Ctrl Pts',(-0.285000226830173,0.428974967322919,
-3.03727426122838));
#71055=CARTESIAN_POINT('Ctrl Pts',(-0.514964439704652,-0.00750271008224029,
-3.01342607917014));
#71056=CARTESIAN_POINT('Ctrl Pts',(-0.272382117990696,-0.437095691356589,
-2.98957789711191));
#71057=CARTESIAN_POINT('Ctrl Pts',(0.22014604298458,-0.465596799454457,
-2.96572971505367));
#71058=CARTESIAN_POINT('Ctrl Pts',(0.510661720918123,-0.0668525880191949,
-2.94188153299544));
#71059=CARTESIAN_POINT('Ctrl Pts',(0.332579176526704,0.393237526826984,
-2.9180333509372));
#71060=CARTESIAN_POINT('Ctrl Pts',(-0.150687804924479,0.492481315824468,
-2.89418516887897));
#71061=CARTESIAN_POINT('Ctrl Pts',(-0.495679223315113,0.139809759376405,
-2.87033698682074));
#71062=CARTESIAN_POINT('Ctrl Pts',(-0.385820801560915,-0.34115534618457,
-2.8464888047625));
#71063=CARTESIAN_POINT('Ctrl Pts',(0.0780781397392639,-0.509066268011637,
-2.82264062270427));
#71064=CARTESIAN_POINT('Ctrl Pts',(0.470330282758143,-0.209843003904197,
-2.79879244064603));
#71065=CARTESIAN_POINT('Ctrl Pts',(0.430993519558152,0.281938374916232,
-2.7749442585878));
#71066=CARTESIAN_POINT('Ctrl Pts',(-0.00383557847163829,0.515004805306344,
-2.75109607652956));
#71067=CARTESIAN_POINT('Ctrl Pts',(-0.435145036849806,0.275487673155042,
-2.72724789447133));
#71068=CARTESIAN_POINT('Ctrl Pts',(-0.46715260595567,-0.216825053676554,
-2.70339971241309));
#71069=CARTESIAN_POINT('Ctrl Pts',(-0.0704871986133876,-0.510172731518216,
-2.67955153035486));
#71070=CARTESIAN_POINT('Ctrl Pts',(0.390859336152151,-0.335370899895037,
-2.65570334829662));
#71071=CARTESIAN_POINT('Ctrl Pts',(0.493541843646563,0.147177137230274,
-2.63185516623839));
#71072=CARTESIAN_POINT('Ctrl Pts',(0.143335833723845,0.494671102778485,
-2.60800698418016));
#71073=CARTESIAN_POINT('Ctrl Pts',(-0.338399354654062,0.38824030950325,
-2.58415880212192));
#71074=CARTESIAN_POINT('Ctrl Pts',(-0.509609338336009,-0.0744512151287393,
-2.56031062006369));
#71075=CARTESIAN_POINT('Ctrl Pts',(-0.213186798712875,-0.468824114149408,
-2.53646243800545));
#71076=CARTESIAN_POINT('Ctrl Pts',(0.278862220093275,-0.432990211619247,
-2.51261425594722));
#71077=CARTESIAN_POINT('Ctrl Pts',(0.515019060662466,0.000168249144257329,
-2.48876607388898));
#71078=CARTESIAN_POINT('Ctrl Pts',(0.278579257547253,0.433172319542517,
-2.46491789183075));
#71079=CARTESIAN_POINT('Ctrl Pts',(-0.213493069046952,0.468684724118824,
-2.44106970977251));
#71080=CARTESIAN_POINT('Ctrl Pts',(-0.509657873788101,0.0741182355376679,
-2.41722152771428));
#71081=CARTESIAN_POINT('Ctrl Pts',(-0.338145617665194,-0.388461326784597,
-2.39337334565604));
#71082=CARTESIAN_POINT('Ctrl Pts',(0.143659006626774,-0.494577345789749,
-2.36952516359781));
#71083=CARTESIAN_POINT('Ctrl Pts',(0.49363789949917,-0.146854640142799,
-2.34567698153957));
#71084=CARTESIAN_POINT('Ctrl Pts',(0.39064013127742,0.335626204264484,-2.32182879948134));
#71085=CARTESIAN_POINT('Ctrl Pts',(-0.0708205153719315,0.510126568368949,
-2.2979806174231));
#71086=CARTESIAN_POINT('Ctrl Pts',(-0.467294173334448,0.216519783671375,
-2.27413243536487));
#71087=CARTESIAN_POINT('Ctrl Pts',(-0.434964948454003,-0.27577192527491,
-2.25028425330663));
#71088=CARTESIAN_POINT('Ctrl Pts',(-0.00349908871715384,-0.515007201436616,
-2.2264360712484));
#71089=CARTESIAN_POINT('Ctrl Pts',(0.431177637781705,-0.28165671628849,
-2.20258788919016));
#71090=CARTESIAN_POINT('Ctrl Pts',(0.470193077132676,0.210150259028937,
-2.17873970713193));
#71091=CARTESIAN_POINT('Ctrl Pts',(0.0777455142197789,0.50911717332273,
-2.15489152507369));
#71092=CARTESIAN_POINT('Ctrl Pts',(-0.386043620079866,0.340903189408749,
-2.13104334301546));
#71093=CARTESIAN_POINT('Ctrl Pts',(-0.495587769871853,-0.140133591643364,
-2.10719516095723));
#71094=CARTESIAN_POINT('Ctrl Pts',(-0.150366000143867,-0.492579665794437,
-2.08334697889899));
#71095=CARTESIAN_POINT('Ctrl Pts',(0.332836035597638,-0.393020145235676,
-2.05949879684076));
#71096=CARTESIAN_POINT('Ctrl Pts',(0.51061793190132,0.0671862245869203,
-2.03565061478253));
#71097=CARTESIAN_POINT('Ctrl Pts',(0.219841789768066,0.465740537880266,
-2.01180243272429));
#71098=CARTESIAN_POINT('Ctrl Pts',(-0.272667647152995,0.436917629936666,
-1.98795425066605));
#71099=CARTESIAN_POINT('Ctrl Pts',(-0.514969228232612,0.00716624915361177,
-1.96410606860782));
#71100=CARTESIAN_POINT('Ctrl Pts',(-0.284719893331698,-0.429161092708335,
-1.94025788654958));
#71101=CARTESIAN_POINT('Ctrl Pts',(0.206796793122505,-0.471677588515368,
-1.91640970449135));
#71102=CARTESIAN_POINT('Ctrl Pts',(0.508550657539238,-0.0813688507343729,
-1.89256152243311));
#71103=CARTESIAN_POINT('Ctrl Pts',(0.34364347529996,0.383606338630098,-1.86871334037488));
#71104=CARTESIAN_POINT('Ctrl Pts',(-0.136601071039797,0.49657306465837,
-1.84486515831665));
#71105=CARTESIAN_POINT('Ctrl Pts',(-0.491496455323177,0.15386973567982,
-1.82101697625841));
#71106=CARTESIAN_POINT('Ctrl Pts',(-0.395380230696901,-0.330028990131912,
-1.79716879420018));
#71107=CARTESIAN_POINT('Ctrl Pts',(0.0635485270542077,-0.511083404018038,
-1.77332061214195));
#71108=CARTESIAN_POINT('Ctrl Pts',(0.464163286565573,-0.223152648557151,
-1.74947243008371));
#71109=CARTESIAN_POINT('Ctrl Pts',(0.438848157054481,0.269549543133189,
-1.72562424802547));
#71110=CARTESIAN_POINT('Ctrl Pts',(0.0108330462179193,0.514905142975932,
-1.70177606596724));
#71111=CARTESIAN_POINT('Ctrl Pts',(-0.427122786573439,0.287768633355279,
-1.677927883909));
#71112=CARTESIAN_POINT('Ctrl Pts',(-0.473138182993198,-0.203432841368646,
-1.65407970185077));
#71113=CARTESIAN_POINT('Ctrl Pts',(-0.0849880613563904,-0.507958355163401,
-1.63023151979254));
#71114=CARTESIAN_POINT('Ctrl Pts',(0.381149606020199,-0.346366336389769,
-1.6063833377343));
#71115=CARTESIAN_POINT('Ctrl Pts',(0.497533180188899,0.133061623936225,
-1.58253515567607));
#71116=CARTESIAN_POINT('Ctrl Pts',(0.157365669090087,0.490388323010709,
-1.55868697361783));
#71117=CARTESIAN_POINT('Ctrl Pts',(-0.327205210201477,0.397720267990497,
-1.53483879155959));
#71118=CARTESIAN_POINT('Ctrl Pts',(-0.511522961116853,-0.0599076072270458,
-1.51099060950136));
#71119=CARTESIAN_POINT('Ctrl Pts',(-0.226452192158073,-0.462562499366548,
-1.48714242744313));
#71120=CARTESIAN_POINT('Ctrl Pts',(0.266417771322213,-0.44075643191805,
-1.46329424538489));
#71121=CARTESIAN_POINT('Ctrl Pts',(0.514814948916082,-0.0144992939813027,
-1.43944606332666));
#71122=CARTESIAN_POINT('Ctrl Pts',(0.29080278176969,0.425062822731458,-1.41559788126842));
#71123=CARTESIAN_POINT('Ctrl Pts',(-0.200058574340051,0.474574786505194,
-1.39174969921019));
#71124=CARTESIAN_POINT('Ctrl Pts',(-0.507340296228526,0.0886029625699759,
-1.36790151715195));
#71125=CARTESIAN_POINT('Ctrl Pts',(-0.349071634612663,-0.37867354682136,
-1.34405333509372));
#71126=CARTESIAN_POINT('Ctrl Pts',(0.12951542980401,-0.49846806777978,-1.32020515303549));
#71127=CARTESIAN_POINT('Ctrl Pts',(0.489255325046037,-0.160853623109709,
-1.29635697097725));
#71128=CARTESIAN_POINT('Ctrl Pts',(0.400040138462428,0.324364838989042,
-1.27250878891902));
#71129=CARTESIAN_POINT('Ctrl Pts',(-0.0562636497220763,0.511936580909566,
-1.24866060686078));
#71130=CARTESIAN_POINT('Ctrl Pts',(-0.460938257452779,0.229740253264028,
-1.22481242480255));
#71131=CARTESIAN_POINT('Ctrl Pts',(-0.442642357766302,-0.263272490519829,
-1.20096424274431));
#71132=CARTESIAN_POINT('Ctrl Pts',(-0.0181648065428401,-0.514698650626448,
-1.17711606068608));
#71133=CARTESIAN_POINT('Ctrl Pts',(0.422981305635007,-0.293822184725266,
-1.15326787862784));
#71134=CARTESIAN_POINT('Ctrl Pts',(0.47598732620688,0.196674163132451,-1.12941969656961));
#71135=CARTESIAN_POINT('Ctrl Pts',(0.0922133710777856,0.50669651207394,
-1.10557151451137));
#71136=CARTESIAN_POINT('Ctrl Pts',(-0.376178286584747,0.351759232793667,
-1.08172333245314));
#71137=CARTESIAN_POINT('Ctrl Pts',(-0.499377680026562,-0.125962668456626,
-1.0578751503949));
#71138=CARTESIAN_POINT('Ctrl Pts',(-0.164333420878337,-0.488097518879012,
-1.03402696833667));
#71139=CARTESIAN_POINT('Ctrl Pts',(0.321508020518597,-0.402339724481236,
-1.01017878627844));
#71140=CARTESIAN_POINT('Ctrl Pts',(0.512324242423155,0.052616839309969,
-0.9863306042202));
#71141=CARTESIAN_POINT('Ctrl Pts',(0.233016665150436,0.459290643183149,
-0.962482422161966));
#71142=CARTESIAN_POINT('Ctrl Pts',(-0.260113860210765,0.444505838971396,
-0.938634240103731));
#71143=CARTESIAN_POINT('Ctrl Pts',(-0.514556254004094,0.0218293980388927,
-0.914786058045497));
#71144=CARTESIAN_POINT('Ctrl Pts',(-0.296826689119951,-0.420878340829603,
-0.890937875987262));
#71145=CARTESIAN_POINT('Ctrl Pts',(0.193279779355815,-0.477375730473926,
-0.867089693929028));
#71146=CARTESIAN_POINT('Ctrl Pts',(0.50602703534366,-0.0958191038103274,
-0.843241511870793));
#71147=CARTESIAN_POINT('Ctrl Pts',(0.354428994654787,0.373663951835225,
-0.819393329812559));
#71148=CARTESIAN_POINT('Ctrl Pts',(-0.122403520039554,0.500261970806237,
-0.795545147754323));
#71149=CARTESIAN_POINT('Ctrl Pts',(-0.48691496321932,0.167804885949508,
-0.77169696569609));
#71150=CARTESIAN_POINT('Ctrl Pts',(-0.40461890944033,-0.318634899648728,
-0.747848783637854));
#71151=CARTESIAN_POINT('Ctrl Pts',(0.0489673608989993,-0.512685925999647,
-0.72400060157962));
#71152=CARTESIAN_POINT('Ctrl Pts',(0.457619740115207,-0.236281261685694,
-0.700152419521385));
#71153=CARTESIAN_POINT('Ctrl Pts',(0.44634678101758,0.256942040561066,-0.67630423746315));
#71154=CARTESIAN_POINT('Ctrl Pts',(0.0254928827023883,0.514387766260962,
-0.652456055404916));
#71155=CARTESIAN_POINT('Ctrl Pts',(-0.418754035043963,0.299816142623377,
-0.628607873346681));
#71156=CARTESIAN_POINT('Ctrl Pts',(-0.478739928722221,-0.189875595156935,
-0.604759691288448));
#71157=CARTESIAN_POINT('Ctrl Pts',(-0.0994199782875138,-0.505331899924686,
-0.580911509230211));
#71158=CARTESIAN_POINT('Ctrl Pts',(0.371130670740883,-0.357080784937167,
-0.557063327171978));
#71159=CARTESIAN_POINT('Ctrl Pts',(0.501120893982533,0.11883816524227,-0.533215145113743));
#71160=CARTESIAN_POINT('Ctrl Pts',(0.171267844788483,0.485707717609162,
-0.509366963055509));
#71161=CARTESIAN_POINT('Ctrl Pts',(-0.315745626841075,0.406877578578177,
-0.485518780997274));
#71162=CARTESIAN_POINT('Ctrl Pts',(-0.513021604132975,-0.0453154010881461,
-0.461670598939039));
#71163=CARTESIAN_POINT('Ctrl Pts',(-0.239533894924378,-0.455925630002724,
-0.437822416880805));
#71164=CARTESIAN_POINT('Ctrl Pts',(0.253757226152789,-0.448165096259132,
-0.41397423482257));
#71165=CARTESIAN_POINT('Ctrl Pts',(0.514193131175447,-0.0291550638327419,
-0.390126052764336));
#71166=CARTESIAN_POINT('Ctrl Pts',(0.302790517927606,0.416608475001228,
-0.366277870706101));
#71167=CARTESIAN_POINT('Ctrl Pts',(-0.186462021616671,0.480079892059551,
-0.342429688647866));
#71168=CARTESIAN_POINT('Ctrl Pts',(-0.50461068347562,0.103015734629539,
-0.318581506589632));
#71169=CARTESIAN_POINT('Ctrl Pts',(-0.359715347231949,-0.368578423437957,
-0.294733324531397));
#71170=CARTESIAN_POINT('Ctrl Pts',(0.115268469717766,-0.501954690602548,
-0.270885142473162));
#71171=CARTESIAN_POINT('Ctrl Pts',(0.484472610223246,-0.174721575692987,
-0.247036960414928));
#71172=CARTESIAN_POINT('Ctrl Pts',(0.409121821147799,0.312839300687487,
-0.223188778356693));
#71173=CARTESIAN_POINT('Ctrl Pts',(-0.0416730493251578,0.513333270606055,
-0.199340596298459));
#71174=CARTESIAN_POINT('Ctrl Pts',(-0.454185555720083,0.242770541477401,
-0.175492414240224));
#71175=CARTESIAN_POINT('Ctrl Pts',(-0.450004527996802,-0.250552174658241,
-0.15164423218199));
#71176=CARTESIAN_POINT('Ctrl Pts',(-0.0327316160753884,-0.513986565007051,
-0.127796050123755));
#71177=CARTESIAN_POINT('Ctrl Pts',(0.414280086532281,-0.305722409144298,
-0.10394786806552));
#71178=CARTESIAN_POINT('Ctrl Pts',(0.481707908230206,0.182986979932784,
-0.0800996860072855));
#71179=CARTESIAN_POINT('Ctrl Pts',(0.105987522180041,0.503963242400988,
-0.0562515039490512));
#71180=CARTESIAN_POINT('Ctrl Pts',(-0.286205982023216,0.385783600838152,
-0.0363780189005224));
#71181=CARTESIAN_POINT('Ctrl Pts',(-0.435697412769368,0.125135549288363,
-0.020479230861699));
#71182=CARTESIAN_POINT('Ctrl Pts',(-0.44089380649838,-0.0236648797430034,
-0.0125298368422878));
#71183=CARTESIAN_POINT('Ctrl Pts',(-0.425168349125048,-0.0944518890585346,
-0.00855513983258212));
#71184=CARTESIAN_POINT('Ctrl Pts',(-0.204298847651432,0.416621468233145,
-3.47394486016742));
#71185=CARTESIAN_POINT('Ctrl Pts',(-0.273662872075077,0.382607401895386,
-3.46997016315771));
#71186=CARTESIAN_POINT('Ctrl Pts',(-0.394020182316735,0.279277366226496,
-3.4620207691383));
#71187=CARTESIAN_POINT('Ctrl Pts',(-0.511435893926076,-0.0185377744517229,
-3.44612198109947));
#71188=CARTESIAN_POINT('Ctrl Pts',(-0.348820800331314,-0.423508877579897,
-3.42624849605095));
#71189=CARTESIAN_POINT('Ctrl Pts',(0.168249301911632,-0.522575166238889,
-3.40240031399271));
#71190=CARTESIAN_POINT('Ctrl Pts',(0.530033749224739,-0.141300624249212,
-3.37855213193448));
#71191=CARTESIAN_POINT('Ctrl Pts',(0.405902783757,0.369222784125986,-3.35470394987624));
#71192=CARTESIAN_POINT('Ctrl Pts',(-0.0909349985308223,0.541150548495764,
-3.33085576781801));
#71193=CARTESIAN_POINT('Ctrl Pts',(-0.504203956900882,0.216391213494833,
-3.30700758575977));
#71194=CARTESIAN_POINT('Ctrl Pts',(-0.45486524179264,-0.306877005951273,
-3.28315940370154));
#71195=CARTESIAN_POINT('Ctrl Pts',(0.0119049262807596,-0.548576111432104,
-3.25931122164331));
#71196=CARTESIAN_POINT('Ctrl Pts',(0.467733209195441,-0.286869868566442,
-3.23546303958507));
#71197=CARTESIAN_POINT('Ctrl Pts',(0.494364895825279,0.238068389313909,
-3.21161485752684));
#71198=CARTESIAN_POINT('Ctrl Pts',(0.067348035130247,0.54455237062264,-3.1877666754686));
#71199=CARTESIAN_POINT('Ctrl Pts',(-0.42146687680021,0.351336842403683,
-3.16391849341037));
#71200=CARTESIAN_POINT('Ctrl Pts',(-0.523532677873002,-0.164274546930515,
-3.14007031135213));
#71201=CARTESIAN_POINT('Ctrl Pts',(-0.145188814060127,-0.529143384571705,
-3.1162221292939));
#71202=CARTESIAN_POINT('Ctrl Pts',(0.366384225429279,-0.408454367466004,
-3.09237394723566));
#71203=CARTESIAN_POINT('Ctrl Pts',(0.541752502859644,0.0870442307434959,
-3.06852576517743));
#71204=CARTESIAN_POINT('Ctrl Pts',(0.219992647842253,0.502668567467005,
-3.04467758311919));
#71205=CARTESIAN_POINT('Ctrl Pts',(-0.303638883942248,0.457029391751011,
-3.02082940106096));
#71206=CARTESIAN_POINT('Ctrl Pts',(-0.548642467695438,-0.00799337790447078,
-2.99698121900273));
#71207=CARTESIAN_POINT('Ctrl Pts',(-0.290195566622494,-0.465681200943625,
-2.97313303694449));
#71208=CARTESIAN_POINT('Ctrl Pts',(0.234543317875925,-0.496046245737469,
-2.94928485488626));
#71209=CARTESIAN_POINT('Ctrl Pts',(0.544058356500897,-0.0712246633645508,
-2.92543667282802));
#71210=CARTESIAN_POINT('Ctrl Pts',(0.35432943722945,0.418954767503064,-2.90158849076979));
#71211=CARTESIAN_POINT('Ctrl Pts',(-0.160542598228318,0.524688975733545,
-2.87774030871155));
#71212=CARTESIAN_POINT('Ctrl Pts',(-0.528096022360174,0.148953142155155,
-2.85389212665332));
#71213=CARTESIAN_POINT('Ctrl Pts',(-0.411052997713816,-0.363466477618423,
-2.83004394459508));
#71214=CARTESIAN_POINT('Ctrl Pts',(0.0831843520771779,-0.542358562976886,
-2.80619576253685));
#71215=CARTESIAN_POINT('Ctrl Pts',(0.501089292907908,-0.223566472971712,
-2.78234758047861));
#71216=CARTESIAN_POINT('Ctrl Pts',(0.459179954768808,0.300376790756268,
-2.75849939842038));
#71217=CARTESIAN_POINT('Ctrl Pts',(-0.00408642048939399,0.548685473156816,
-2.73465121636214));
#71218=CARTESIAN_POINT('Ctrl Pts',(-0.463602976080494,0.2935042211966,-2.71080303430391));
#71219=CARTESIAN_POINT('Ctrl Pts',(-0.497703800031065,-0.231005140035548,
-2.68695485224567));
#71220=CARTESIAN_POINT('Ctrl Pts',(-0.0750969729295639,-0.543537387808,
-2.66310667018744));
#71221=CARTESIAN_POINT('Ctrl Pts',(0.416421046143122,-0.357303735801995,
-2.63925848812921));
#71222=CARTESIAN_POINT('Ctrl Pts',(0.525818860744067,0.156802337273383,
-2.61541030607097));
#71223=CARTESIAN_POINT('Ctrl Pts',(0.152709817339109,0.527021972005809,
-2.59156212401274));
#71224=CARTESIAN_POINT('Ctrl Pts',(-0.360530247701046,0.413630738438696,
-2.5677139419545));
#71225=CARTESIAN_POINT('Ctrl Pts',(-0.542937149418829,-0.0793202311495182,
-2.54386575989627));
#71226=CARTESIAN_POINT('Ctrl Pts',(-0.227128947763859,-0.499484622762653,
-2.52001757783803));
#71227=CARTESIAN_POINT('Ctrl Pts',(0.297099459268975,-0.46130722798452,
-2.4961693957798));
#71228=CARTESIAN_POINT('Ctrl Pts',(0.548700660795336,0.000179252427110567,
-2.47232121372157));
#71229=CARTESIAN_POINT('Ctrl Pts',(0.296797991327609,0.461501245537395,
-2.44847303166333));
#71230=CARTESIAN_POINT('Ctrl Pts',(-0.227455247793364,0.499336116799028,
-2.4246248496051));
#71231=CARTESIAN_POINT('Ctrl Pts',(-0.542988859028567,0.078965475111137,
-2.40077666754686));
#71232=CARTESIAN_POINT('Ctrl Pts',(-0.36025991663159,-0.413866209972829,
-2.37692848548863));
#71233=CARTESIAN_POINT('Ctrl Pts',(0.153054125344252,-0.52692208342769,
-2.35308030343039));
#71234=CARTESIAN_POINT('Ctrl Pts',(0.525921198528869,-0.156458749281175,
-2.32923212137215));
#71235=CARTESIAN_POINT('Ctrl Pts',(0.416187505544722,0.357575736756754,
-2.30538393931392));
#71236=CARTESIAN_POINT('Ctrl Pts',(-0.0754520881857466,0.543488205646713,
-2.28153575725568));
#71237=CARTESIAN_POINT('Ctrl Pts',(-0.497854625738724,0.230679905755195,
-2.25768757519746));
#71238=CARTESIAN_POINT('Ctrl Pts',(-0.463411110129646,-0.293807063048322,
-2.23383939313921));
#71239=CARTESIAN_POINT('Ctrl Pts',(-0.0037279247273187,-0.548688025991,
-2.20999121108099));
#71240=CARTESIAN_POINT('Ctrl Pts',(0.459376114093082,-0.300076712007801,
-2.18614302902275));
#71241=CARTESIAN_POINT('Ctrl Pts',(0.500943114206752,0.223893822195952,
-2.16229484696451));
#71242=CARTESIAN_POINT('Ctrl Pts',(0.0828299732662211,0.542412797431429,
-2.13844666490628));
#71243=CARTESIAN_POINT('Ctrl Pts',(-0.411290388284232,0.363197830105963,
-2.11459848284804));
#71244=CARTESIAN_POINT('Ctrl Pts',(-0.527998587976513,-0.149298152645908,
-2.09075030078981));
#71245=CARTESIAN_POINT('Ctrl Pts',(-0.160199747818974,-0.524793757668104,
-2.06690211873158));
#71246=CARTESIAN_POINT('Ctrl Pts',(0.354603094561221,-0.418723169428535,
-2.04305393667334));
#71247=CARTESIAN_POINT('Ctrl Pts',(0.544011703737359,0.0715801193450341,
-2.01920575461511));
#71248=CARTESIAN_POINT('Ctrl Pts',(0.234219166880941,0.496199384475909,
-1.99535757255687));
#71249=CARTESIAN_POINT('Ctrl Pts',(-0.290499769033619,0.465491494530337,
-1.97150939049864));
#71250=CARTESIAN_POINT('Ctrl Pts',(-0.548647569387118,0.00763491285342533,
-1.9476612084404));
#71251=CARTESIAN_POINT('Ctrl Pts',(-0.303340216984838,-0.457227689503013,
-1.92381302638217));
#71252=CARTESIAN_POINT('Ctrl Pts',(0.220321043828396,-0.502524710770565,
-1.89996484432393));
#71253=CARTESIAN_POINT('Ctrl Pts',(0.54180923222677,-0.0866902714409802,
-1.8761166622657));
#71254=CARTESIAN_POINT('Ctrl Pts',(0.366117327254944,0.408693711686842,
-1.85226848020746));
#71255=CARTESIAN_POINT('Ctrl Pts',(-0.145534609628768,0.529048319805361,
-1.82842029814923));
#71256=CARTESIAN_POINT('Ctrl Pts',(-0.523639706591634,0.163932623261208,
-1.804572116091));
#71257=CARTESIAN_POINT('Ctrl Pts',(-0.421237601516625,-0.351612471845344,
-1.78072393403276));
#71258=CARTESIAN_POINT('Ctrl Pts',(0.0677045209595963,-0.544507617146265,
-1.75687575197453));
#71259=CARTESIAN_POINT('Ctrl Pts',(0.494518982904948,-0.237746551679154,
-1.73302756991629));
#71260=CARTESIAN_POINT('Ctrl Pts',(0.467548275698523,0.287177744924656,
-1.70917938785805));
#71261=CARTESIAN_POINT('Ctrl Pts',(0.0115415138432998,0.548579293035088,
-1.68533120579982));
#71262=CARTESIAN_POINT('Ctrl Pts',(-0.455056080705307,0.306588340779288,
-1.66148302374159));
#71263=CARTESIAN_POINT('Ctrl Pts',(-0.504080826293955,-0.216737093852153,
-1.63763484168335));
#71264=CARTESIAN_POINT('Ctrl Pts',(-0.0905461738949672,-0.541178194018989,
-1.61378665962512));
#71265=CARTESIAN_POINT('Ctrl Pts',(0.406076311847863,-0.369018260042385,
-1.58993847756688));
#71266=CARTESIAN_POINT('Ctrl Pts',(0.530071225686482,0.141763687127217,
-1.56609029550865));
#71267=CARTESIAN_POINT('Ctrl Pts',(0.167657186328529,0.522459103816819,
-1.54224211345041));
#71268=CARTESIAN_POINT('Ctrl Pts',(-0.348604020251771,0.423730674312086,
-1.51839393139218));
#71269=CARTESIAN_POINT('Ctrl Pts',(-0.544975920727627,-0.0638254895456974,
-1.49454574933394));
#71270=CARTESIAN_POINT('Ctrl Pts',(-0.241261881290101,-0.49281350623236,
-1.47069756727571));
#71271=CARTESIAN_POINT('Ctrl Pts',(0.283841159168135,-0.469581349342968,
-1.44684938521748));
#71272=CARTESIAN_POINT('Ctrl Pts',(0.548483200396933,-0.0154475296086586,
-1.42300120315924));
#71273=CARTESIAN_POINT('Ctrl Pts',(0.309820918691641,0.452861397813657,
-1.39915302110101));
#71274=CARTESIAN_POINT('Ctrl Pts',(-0.213142153995152,0.50561138187246,
-1.37530483904277));
#71275=CARTESIAN_POINT('Ctrl Pts',(-0.540519714805541,0.0943974851106201,
-1.35145665698454));
#71276=CARTESIAN_POINT('Ctrl Pts',(-0.371900481373456,-0.403438321485286,
-1.3276084749263));
#71277=CARTESIAN_POINT('Ctrl Pts',(0.137985576349817,-0.531067253752366,
-1.30376029286807));
#71278=CARTESIAN_POINT('Ctrl Pts',(0.521252009207359,-0.171373248163074,
-1.27991211080983));
#71279=CARTESIAN_POINT('Ctrl Pts',(0.426202261401058,0.345577892327182,
-1.2560639287516));
#71280=CARTESIAN_POINT('Ctrl Pts',(-0.0599432217936751,0.54541659073562,
-1.23221574669336));
#71281=CARTESIAN_POINT('Ctrl Pts',(-0.491083040936125,0.244764977465323,
-1.20836756463513));
#71282=CARTESIAN_POINT('Ctrl Pts',(-0.471590612374546,-0.280490180949125,
-1.18451938257689));
#71283=CARTESIAN_POINT('Ctrl Pts',(-0.0193527620908934,-0.54835929634513,
-1.16067120051866));
#71284=CARTESIAN_POINT('Ctrl Pts',(0.450643752111749,-0.31303778681066,
-1.13682301846043));
#71285=CARTESIAN_POINT('Ctrl Pts',(0.507116299897664,0.209536406542574,
-1.11297483640219));
#71286=CARTESIAN_POINT('Ctrl Pts',(0.0982440098031782,0.539833827975301,
-1.08912665434396));
#71287=CARTESIAN_POINT('Ctrl Pts',(-0.400779874361163,0.374763845102116,
-1.06527847228572));
#71288=CARTESIAN_POINT('Ctrl Pts',(-0.532036353498374,-0.134200468869619,
-1.04143029022749));
#71289=CARTESIAN_POINT('Ctrl Pts',(-0.175080620338046,-0.52001848397025,
-1.01758210816925));
#71290=CARTESIAN_POINT('Ctrl Pts',(0.342534241514551,-0.428652237459134,
-0.993733926111017));
#71291=CARTESIAN_POINT('Ctrl Pts',(0.545829604825618,0.056057914557968,
-0.969885744052783));
#71292=CARTESIAN_POINT('Ctrl Pts',(0.248255662576661,0.489327674761291,
-0.946037561994548));
#71293=CARTESIAN_POINT('Ctrl Pts',(-0.277124980182455,0.473575962911475,
-0.922189379936314));
#71294=CARTESIAN_POINT('Ctrl Pts',(-0.548207587162405,0.023257013271117,
-0.898341197878079));
#71295=CARTESIAN_POINT('Ctrl Pts',(-0.316238782021605,-0.448403256047641,
-0.874493015819845));
#71296=CARTESIAN_POINT('Ctrl Pts',(0.205920034327462,-0.508595504061096,
-0.850644833761609));
#71297=CARTESIAN_POINT('Ctrl Pts',(0.539120568307165,-0.102085552930635,
-0.826796651703376));
#71298=CARTESIAN_POINT('Ctrl Pts',(0.377608206037959,0.398101105274931,
-0.80294846964514));
#71299=CARTESIAN_POINT('Ctrl Pts',(-0.130408556613393,0.532978475785109,
-0.779100287586906));
#71300=CARTESIAN_POINT('Ctrl Pts',(-0.518758590654718,0.178779114867606,
-0.755252105528672));
#71301=CARTESIAN_POINT('Ctrl Pts',(-0.431080478253797,-0.339473222146037,
-0.731403923470437));
#71302=CARTESIAN_POINT('Ctrl Pts',(0.0521697648396222,-0.54621494205404,
-0.707555741412202));
#71303=CARTESIAN_POINT('Ctrl Pts',(0.487547496729966,-0.251733759627714,
-0.683707559353968));
#71304=CARTESIAN_POINT('Ctrl Pts',(0.47553730025679,0.273745727508825,-0.659859377295733));
#71305=CARTESIAN_POINT('Ctrl Pts',(0.027160085233324,0.548028080532353,
-0.636011195237498));
#71306=CARTESIAN_POINT('Ctrl Pts',(-0.446140023329977,0.319423742031895,
-0.612163013179265));
#71307=CARTESIAN_POINT('Ctrl Pts',(-0.510048919162534,-0.202293220754791,
-0.588314831121028));
#71308=CARTESIAN_POINT('Ctrl Pts',(-0.105921920078934,-0.5383799719043,
-0.564466649062795));
#71309=CARTESIAN_POINT('Ctrl Pts',(0.395402150776707,-0.38043342007637,
-0.540618467004559));
#71310=CARTESIAN_POINT('Ctrl Pts',(0.533893571459043,0.126610032087479,
-0.516770284946326));
#71311=CARTESIAN_POINT('Ctrl Pts',(0.182468546868062,0.51747239269695,-0.492922102888091));
#71312=CARTESIAN_POINT('Ctrl Pts',(-0.336394994523279,0.433486861518255,
-0.469073920829856));
#71313=CARTESIAN_POINT('Ctrl Pts',(-0.546572573115956,-0.048278971440956,
-0.445225738771622));
#71314=CARTESIAN_POINT('Ctrl Pts',(-0.255199110997613,-0.485742593942516,
-0.421377556713387));
#71315=CARTESIAN_POINT('Ctrl Pts',(0.270352630235717,-0.477474531032853,
-0.397529374655153));
#71316=CARTESIAN_POINT('Ctrl Pts',(0.547820716556546,-0.0310617684129566,
-0.373681192596918));
#71317=CARTESIAN_POINT('Ctrl Pts',(0.322592637747684,0.443854146353481,
-0.349833010538683));
#71318=CARTESIAN_POINT('Ctrl Pts',(-0.198656403789595,0.51147651442025,
-0.325984828480449));
#71319=CARTESIAN_POINT('Ctrl Pts',(-0.537611588804712,0.109752834372456,
-0.302136646422214));
#71320=CARTESIAN_POINT('Ctrl Pts',(-0.383240279438416,-0.392682989703664,
-0.278288464363979));
#71321=CARTESIAN_POINT('Ctrl Pts',(0.122806882956234,-0.534781897331454,
-0.254440282305745));
#71322=CARTESIAN_POINT('Ctrl Pts',(0.516156510838259,-0.186148147438714,
-0.23059210024751));
#71323=CARTESIAN_POINT('Ctrl Pts',(0.435877874735032,0.333298598287169,
-0.206743918189276));
#71324=CARTESIAN_POINT('Ctrl Pts',(-0.0443984144444239,0.546904622185182,
-0.182895736131041));
#71325=CARTESIAN_POINT('Ctrl Pts',(-0.483888720985873,0.258647430172675,
-0.159047554072806));
#71326=CARTESIAN_POINT('Ctrl Pts',(-0.479434259297373,-0.266937972396299,
-0.135199372014572));
#71327=CARTESIAN_POINT('Ctrl Pts',(-0.0348722226831059,-0.54760064122001,
-0.111351189956337));
#71328=CARTESIAN_POINT('Ctrl Pts',(0.441373484201181,-0.325716270969938,
-0.0875030078981022));
#71329=CARTESIAN_POINT('Ctrl Pts',(0.513211000805034,0.194954098741337,
-0.0636548258398677));
#71330=CARTESIAN_POINT('Ctrl Pts',(0.112918973098675,0.536921805896445,
-0.0398066437816333));
#71331=CARTESIAN_POINT('Ctrl Pts',(-0.304923494011494,0.411013364110478,
-0.0199331587331047));
#71332=CARTESIAN_POINT('Ctrl Pts',(-0.464191476691871,0.133319257145926,
-0.00403437069428121));
#71333=CARTESIAN_POINT('Ctrl Pts',(-0.469727708048424,-0.0252125331748408,
0.00391502332512999));
#71334=CARTESIAN_POINT('Ctrl Pts',(-0.452973825500936,-0.100628924050155,
0.00788972033483567));
#71335=CARTESIAN_POINT('Ctrl Pts',(-0.216839587231055,0.442195480991683,
-3.4575));
#71336=CARTESIAN_POINT('Ctrl Pts',(-0.290461473000917,0.406093485363625,
-3.45352530299029));
#71337=CARTESIAN_POINT('Ctrl Pts',(-0.418206831200729,0.296420608885922,
-3.44557590897088));
#71338=CARTESIAN_POINT('Ctrl Pts',(-0.542830022826607,-0.0196757025627097,
-3.42967712093206));
#71339=CARTESIAN_POINT('Ctrl Pts',(-0.370232917272739,-0.449505669066697,
-3.40980363588353));
#71340=CARTESIAN_POINT('Ctrl Pts',(0.178577165744359,-0.554653071454301,
-3.3859554538253));
#71341=CARTESIAN_POINT('Ctrl Pts',(0.56256949425635,-0.149974262654511,
-3.36210727176706));
#71342=CARTESIAN_POINT('Ctrl Pts',(0.430818837686123,0.391887262344127,
-3.33825908970883));
#71343=CARTESIAN_POINT('Ctrl Pts',(-0.0965169787933541,0.574368690350557,
-3.31441090765059));
#71344=CARTESIAN_POINT('Ctrl Pts',(-0.535154158486442,0.229674234358403,
-3.29056272559236));
#71345=CARTESIAN_POINT('Ctrl Pts',(-0.482786821413474,-0.325714432881724,
-3.26671454353412));
#71346=CARTESIAN_POINT('Ctrl Pts',(0.012635701720356,-0.582250066190823,
-3.24286636147589));
#71347=CARTESIAN_POINT('Ctrl Pts',(0.496444679850769,-0.30447917158645,
-3.21901817941765));
#71348=CARTESIAN_POINT('Ctrl Pts',(0.524711133638771,0.252682048210408,
-3.19516999735942));
#71349=CARTESIAN_POINT('Ctrl Pts',(0.0714821464063366,0.577979330911211,
-3.17132181530119));
#71350=CARTESIAN_POINT('Ctrl Pts',(-0.447338321520283,0.372903404799714,
-3.14747363324295));
#71351=CARTESIAN_POINT('Ctrl Pts',(-0.555669359259625,-0.174358423253356,
-3.12362545118472));
#71352=CARTESIAN_POINT('Ctrl Pts',(-0.154101126233856,-0.56162447520182,
-3.09977726912648));
#71353=CARTESIAN_POINT('Ctrl Pts',(0.388874460739024,-0.43352704854784,
-3.07592908706825));
#71354=CARTESIAN_POINT('Ctrl Pts',(0.575007595255289,0.0923873789903477,
-3.05208090501001));
#71355=CARTESIAN_POINT('Ctrl Pts',(0.233496740193908,0.533524520263281,
-3.02823272295177));
#71356=CARTESIAN_POINT('Ctrl Pts',(-0.322277541054323,0.485083816179102,
-3.00438454089354));
#71357=CARTESIAN_POINT('Ctrl Pts',(-0.582320495686226,-0.00848404572670107,
-2.9805363588353));
#71358=CARTESIAN_POINT('Ctrl Pts',(-0.308009015254291,-0.49426671053066,
-2.95668817677707));
#71359=CARTESIAN_POINT('Ctrl Pts',(0.24894059276727,-0.526495692020481,
-2.93283999471884));
#71360=CARTESIAN_POINT('Ctrl Pts',(0.577454992083672,-0.0755967387099062,
-2.9089918126606));
#71361=CARTESIAN_POINT('Ctrl Pts',(0.376079697932196,0.444672008179143,
-2.88514363060237));
#71362=CARTESIAN_POINT('Ctrl Pts',(-0.170397391532157,0.556896635642623,
-2.86129544854414));
#71363=CARTESIAN_POINT('Ctrl Pts',(-0.560512821405234,0.158096524933905,
-2.8374472664859));
#71364=CARTESIAN_POINT('Ctrl Pts',(-0.436285193866717,-0.385777609052274,
-2.81359908442767));
#71365=CARTESIAN_POINT('Ctrl Pts',(0.0882905644150925,-0.575650857942135,
-2.78975090236943));
#71366=CARTESIAN_POINT('Ctrl Pts',(0.531848303057673,-0.237289942039227,
-2.76590272031119));
#71367=CARTESIAN_POINT('Ctrl Pts',(0.487366389979465,0.318815206596304,
-2.74205453825296));
#71368=CARTESIAN_POINT('Ctrl Pts',(-0.00433726250715015,0.582366141007289,
-2.71820635619472));
#71369=CARTESIAN_POINT('Ctrl Pts',(-0.492060915311181,0.311520769238158,
-2.69435817413649));
#71370=CARTESIAN_POINT('Ctrl Pts',(-0.528254994106461,-0.245185226394541,
-2.67050999207826));
#71371=CARTESIAN_POINT('Ctrl Pts',(-0.0797067472457391,-0.576902044097784,
-2.64666181002002));
#71372=CARTESIAN_POINT('Ctrl Pts',(0.44198275613409,-0.379236571708953,
-2.62281362796179));
#71373=CARTESIAN_POINT('Ctrl Pts',(0.558095877841571,0.166427537316492,
-2.59896544590355));
#71374=CARTESIAN_POINT('Ctrl Pts',(0.162083800954373,0.559372841233132,
-2.57511726384532));
#71375=CARTESIAN_POINT('Ctrl Pts',(-0.382661140748029,0.439021167374142,
-2.55126908178708));
#71376=CARTESIAN_POINT('Ctrl Pts',(-0.576264960501648,-0.0841892471702974,
-2.52742089972885));
#71377=CARTESIAN_POINT('Ctrl Pts',(-0.241071096814844,-0.530145131375898,
-2.50357271767062));
#71378=CARTESIAN_POINT('Ctrl Pts',(0.315336698444676,-0.489624244349793,
-2.47972453561237));
#71379=CARTESIAN_POINT('Ctrl Pts',(0.582382260928205,0.000190255709963338,
-2.45587635355415));
#71380=CARTESIAN_POINT('Ctrl Pts',(0.315016725107966,0.489830171532273,
-2.43202817149591));
#71381=CARTESIAN_POINT('Ctrl Pts',(-0.241417426539775,0.529987509479231,
-2.40817998943768));
#71382=CARTESIAN_POINT('Ctrl Pts',(-0.576319844269034,0.0838127146846064,
-2.38433180737944));
#71383=CARTESIAN_POINT('Ctrl Pts',(-0.382374215597984,-0.439271093161061,
-2.36048362532121));
#71384=CARTESIAN_POINT('Ctrl Pts',(0.16244924406173,-0.559266821065631,
-2.33663544326297));
#71385=CARTESIAN_POINT('Ctrl Pts',(0.558204497558567,-0.166062858419552,
-2.31278726120474));
#71386=CARTESIAN_POINT('Ctrl Pts',(0.441734879812023,0.379525269249024,
-2.2889390791465));
#71387=CARTESIAN_POINT('Ctrl Pts',(-0.0800836609995613,0.576849842924477,
-2.26509089708827));
#71388=CARTESIAN_POINT('Ctrl Pts',(-0.528415078143001,0.244840027839016,
-2.24124271503004));
#71389=CARTESIAN_POINT('Ctrl Pts',(-0.491857271805289,-0.311842200821734,
-2.2173945329718));
#71390=CARTESIAN_POINT('Ctrl Pts',(-0.00395676073748407,-0.582368850545385,
-2.19354635091357));
#71391=CARTESIAN_POINT('Ctrl Pts',(0.48757459040446,-0.318496707727113,
-2.16969816885533));
#71392=CARTESIAN_POINT('Ctrl Pts',(0.531693151280828,0.237637385362967,
-2.1458499867971));
#71393=CARTESIAN_POINT('Ctrl Pts',(0.0879144323126632,0.575708421540129,
-2.12200180473886));
#71394=CARTESIAN_POINT('Ctrl Pts',(-0.436537156488597,0.385492470803176,
-2.09815362268063));
#71395=CARTESIAN_POINT('Ctrl Pts',(-0.560409406081175,-0.158462713648453,
-2.07430544062239));
#71396=CARTESIAN_POINT('Ctrl Pts',(-0.17003349549408,-0.557007849541772,
-2.05045725856416));
#71397=CARTESIAN_POINT('Ctrl Pts',(0.376370153524803,-0.444426193621394,
-2.02660907650592));
#71398=CARTESIAN_POINT('Ctrl Pts',(0.577405475573398,0.0759740141031477,
-2.00276089444769));
#71399=CARTESIAN_POINT('Ctrl Pts',(0.248596543993815,0.526658231071553,
-1.97891271238945));
#71400=CARTESIAN_POINT('Ctrl Pts',(-0.308331890914242,0.494065359124006,
-1.95506453033122));
#71401=CARTESIAN_POINT('Ctrl Pts',(-0.582325910541624,0.00810357655323996,
-1.93121634827298));
#71402=CARTESIAN_POINT('Ctrl Pts',(-0.321960540637979,-0.485294286297692,
-1.90736816621475));
#71403=CARTESIAN_POINT('Ctrl Pts',(0.233845294534286,-0.53337183302576,
-1.88351998415651));
#71404=CARTESIAN_POINT('Ctrl Pts',(0.5750678069143,-0.0920116921475879,
-1.85967180209828));
#71405=CARTESIAN_POINT('Ctrl Pts',(0.388591179209928,0.433781084743586,
-1.83582362004004));
#71406=CARTESIAN_POINT('Ctrl Pts',(-0.154468148217739,0.561523574952351,
-1.81197543798181));
#71407=CARTESIAN_POINT('Ctrl Pts',(-0.55578295786009,0.173995510842596,
-1.78812725592357));
#71408=CARTESIAN_POINT('Ctrl Pts',(-0.447094972336349,-0.373195953558777,
-1.76427907386534));
#71409=CARTESIAN_POINT('Ctrl Pts',(0.0718605148649851,-0.577931830274492,
-1.74043089180711));
#71410=CARTESIAN_POINT('Ctrl Pts',(0.524874679244323,-0.252340454801157,
-1.71658270974887));
#71411=CARTESIAN_POINT('Ctrl Pts',(0.496248394342566,0.304805946716122,
-1.69273452769064));
#71412=CARTESIAN_POINT('Ctrl Pts',(0.0122499814686803,0.582253443094244,
-1.6688863456324));
#71413=CARTESIAN_POINT('Ctrl Pts',(-0.482989374837176,0.325408048203296,
-1.64503816357417));
#71414=CARTESIAN_POINT('Ctrl Pts',(-0.535023469594712,-0.230041346335659,
-1.62118998151593));
#71415=CARTESIAN_POINT('Ctrl Pts',(-0.0961042864335442,-0.574398032874579,
-1.5973417994577));
#71416=CARTESIAN_POINT('Ctrl Pts',(0.431003017675527,-0.391670183695,-1.57349361739947));
#71417=CARTESIAN_POINT('Ctrl Pts',(0.562609271184064,0.150465750318208,
-1.54964543534123));
#71418=CARTESIAN_POINT('Ctrl Pts',(0.177948703566972,0.55452988462293,-1.525797253283));
#71419=CARTESIAN_POINT('Ctrl Pts',(-0.370002830302066,0.449741080633676,
-1.50194907122476));
#71420=CARTESIAN_POINT('Ctrl Pts',(-0.578428880338399,-0.0677433718643487,
-1.47810088916653));
#71421=CARTESIAN_POINT('Ctrl Pts',(-0.256071570422129,-0.523064513098173,
-1.45425270710829));
#71422=CARTESIAN_POINT('Ctrl Pts',(0.301264547014057,-0.498406266767886,
-1.43040452505006));
#71423=CARTESIAN_POINT('Ctrl Pts',(0.582151451877784,-0.0163957652360146,
-1.40655634299182));
#71424=CARTESIAN_POINT('Ctrl Pts',(0.328839055613591,0.480659972895857,
-1.38270816093359));
#71425=CARTESIAN_POINT('Ctrl Pts',(-0.226225733650254,0.536647977239726,
-1.35885997887535));
#71426=CARTESIAN_POINT('Ctrl Pts',(-0.573699133382556,0.100192007651264,
-1.33501179681712));
#71427=CARTESIAN_POINT('Ctrl Pts',(-0.39472932813425,-0.42820309614921,
-1.31116361475888));
#71428=CARTESIAN_POINT('Ctrl Pts',(0.146455722895625,-0.563666439724954,
-1.28731543270065));
#71429=CARTESIAN_POINT('Ctrl Pts',(0.553248693368682,-0.181892873216438,
-1.26346725064242));
#71430=CARTESIAN_POINT('Ctrl Pts',(0.452364384339689,0.366790945665321,
-1.23961906858418));
#71431=CARTESIAN_POINT('Ctrl Pts',(-0.0636227938652733,0.578896600561675,
-1.21577088652595));
#71432=CARTESIAN_POINT('Ctrl Pts',(-0.52122782441947,0.259789701666618,
-1.19192270446771));
#71433=CARTESIAN_POINT('Ctrl Pts',(-0.500538866982789,-0.297707871378421,
-1.16807452240948));
#71434=CARTESIAN_POINT('Ctrl Pts',(-0.0205407176389471,-0.582019942063812,
-1.14422634035124));
#71435=CARTESIAN_POINT('Ctrl Pts',(0.478306198588491,-0.332253388896053,
-1.12037815829301));
#71436=CARTESIAN_POINT('Ctrl Pts',(0.538245273588447,0.222398649952697,
-1.09652997623477));
#71437=CARTESIAN_POINT('Ctrl Pts',(0.104274648528571,0.572971143876661,
-1.07268179417654));
#71438=CARTESIAN_POINT('Ctrl Pts',(-0.42538146213758,0.397768457410565,
-1.0488336121183));
#71439=CARTESIAN_POINT('Ctrl Pts',(-0.564695026970186,-0.142438269282613,
-1.02498543006007));
#71440=CARTESIAN_POINT('Ctrl Pts',(-0.185827819797754,-0.551939449061487,
-1.00113724800184));
#71441=CARTESIAN_POINT('Ctrl Pts',(0.363560462510505,-0.454964750437033,
-0.977289065943598));
#71442=CARTESIAN_POINT('Ctrl Pts',(0.579334967228081,0.0594989898059677,
-0.953440883885366));
#71443=CARTESIAN_POINT('Ctrl Pts',(0.263494660002887,0.519364706339432,
-0.92959270182713));
#71444=CARTESIAN_POINT('Ctrl Pts',(-0.294136100154144,0.502646086851553,
-0.905744519768896));
#71445=CARTESIAN_POINT('Ctrl Pts',(-0.581858920320716,0.0246846285033414,
-0.881896337710661));
#71446=CARTESIAN_POINT('Ctrl Pts',(-0.335650874923259,-0.47592817126568,
-0.858048155652427));
#71447=CARTESIAN_POINT('Ctrl Pts',(0.218560289299109,-0.539815277648267,
-0.834199973594192));
#71448=CARTESIAN_POINT('Ctrl Pts',(0.572214101270669,-0.108352002050942,
-0.810351791535958));
#71449=CARTESIAN_POINT('Ctrl Pts',(0.400787417421131,0.422538258714637,
-0.786503609477722));
#71450=CARTESIAN_POINT('Ctrl Pts',(-0.138413593187233,0.56569498076398,
-0.762655427419489));
#71451=CARTESIAN_POINT('Ctrl Pts',(-0.550602218090115,0.189753343785704,
-0.738807245361253));
#71452=CARTESIAN_POINT('Ctrl Pts',(-0.457542047067265,-0.360311544643345,
-0.714959063303019));
#71453=CARTESIAN_POINT('Ctrl Pts',(0.055372168780246,-0.579743958108433,
-0.691110881244784));
#71454=CARTESIAN_POINT('Ctrl Pts',(0.517475253344724,-0.267186257569734,
-0.66726269918655));
#71455=CARTESIAN_POINT('Ctrl Pts',(0.504727819496001,0.290549414456584,
-0.643414517128314));
#71456=CARTESIAN_POINT('Ctrl Pts',(0.0288272877642591,0.581668394803744,
-0.619566335070081));
#71457=CARTESIAN_POINT('Ctrl Pts',(-0.473526011615991,0.339031341440412,
-0.595718153011845));
#71458=CARTESIAN_POINT('Ctrl Pts',(-0.541357909602848,-0.214710846352648,
-0.571869970953612));
#71459=CARTESIAN_POINT('Ctrl Pts',(-0.112423861870353,-0.571428043883915,
-0.548021788895377));
#71460=CARTESIAN_POINT('Ctrl Pts',(0.419673630812531,-0.403786055215572,
-0.524173606837142));
#71461=CARTESIAN_POINT('Ctrl Pts',(0.566666248935553,0.134381898932689,
-0.500325424778908));
#71462=CARTESIAN_POINT('Ctrl Pts',(0.19366924894764,0.549237067784737,-0.476477242720673));
#71463=CARTESIAN_POINT('Ctrl Pts',(-0.357044362205485,0.460096144458333,
-0.452629060662439));
#71464=CARTESIAN_POINT('Ctrl Pts',(-0.580123542098937,-0.0512425417937655,
-0.428780878604203));
#71465=CARTESIAN_POINT('Ctrl Pts',(-0.270864327070848,-0.515559557882308,
-0.404932696545969));
#71466=CARTESIAN_POINT('Ctrl Pts',(0.286948034318646,-0.506783965806573,
-0.381084514487735));
#71467=CARTESIAN_POINT('Ctrl Pts',(0.581448301937643,-0.0329684729931716,
-0.3572363324295));
#71468=CARTESIAN_POINT('Ctrl Pts',(0.342394757567763,0.471099817705734,
-0.333388150371265));
#71469=CARTESIAN_POINT('Ctrl Pts',(-0.21085078596252,0.542873136780949,
-0.309539968313031));
#71470=CARTESIAN_POINT('Ctrl Pts',(-0.570612494133804,0.116489934115373,
-0.285691786254796));
#71471=CARTESIAN_POINT('Ctrl Pts',(-0.406765211644884,-0.416787555969371,
-0.261843604196561));
#71472=CARTESIAN_POINT('Ctrl Pts',(0.130345296194702,-0.56760910406036,
-0.237995422138327));
#71473=CARTESIAN_POINT('Ctrl Pts',(0.547840411453272,-0.197574719184441,
-0.214147240080093));
#71474=CARTESIAN_POINT('Ctrl Pts',(0.462633928322266,0.353757895886852,
-0.190299058021858));
#71475=CARTESIAN_POINT('Ctrl Pts',(-0.0471237795636909,0.580475973764309,
-0.166450875963623));
#71476=CARTESIAN_POINT('Ctrl Pts',(-0.513591886251662,0.274524318867949,
-0.142602693905388));
#71477=CARTESIAN_POINT('Ctrl Pts',(-0.508863990597946,-0.283323770134356,
-0.118754511847154));
#71478=CARTESIAN_POINT('Ctrl Pts',(-0.0370128292908223,-0.581214717432969,
-0.0949063297889191));
#71479=CARTESIAN_POINT('Ctrl Pts',(0.468466881870079,-0.345710132795577,
-0.0710581477306844));
#71480=CARTESIAN_POINT('Ctrl Pts',(0.544714093379863,0.20692121754989,-0.0472099656724499));
#71481=CARTESIAN_POINT('Ctrl Pts',(0.119850424017307,0.569880369391903,
-0.0233617836142156));
#71482=CARTESIAN_POINT('Ctrl Pts',(-0.32364100599977,0.436243127382803,
-0.00348829856568689));
#71483=CARTESIAN_POINT('Ctrl Pts',(-0.492685540614374,0.141502965003489,
0.0124104894731366));
#71484=CARTESIAN_POINT('Ctrl Pts',(-0.498561609598467,-0.0267601866066781,
0.0203598834925478));
#71485=CARTESIAN_POINT('Ctrl Pts',(-0.480779301876824,-0.106805959041775,
0.0243345805022535));
#71486=CARTESIAN_POINT('Ctrl Pts',(-0.491698555522654,2.49815306513942E-5,
-0.130884152590357));
#71487=CARTESIAN_POINT('Ctrl Pts',(-0.49166889938861,-0.0837076434631148,
-0.12684093900929));
#71488=CARTESIAN_POINT('Ctrl Pts',(-0.471409647654858,-0.167456711012418,
-0.122797725428222));
#71489=CARTESIAN_POINT('Ctrl Pts',(-0.431010112989045,-0.239997579850407,
-0.118754511847154));
#71490=CARTESIAN_POINT('Ctrl Pts',(-0.351580270162238,-0.382620752567228,
-0.110805117827742));
#71491=CARTESIAN_POINT('Ctrl Pts',(-0.194296549726532,-0.481917735000098,
-0.102855723808331));
#71492=CARTESIAN_POINT('Ctrl Pts',(-0.0314080709818594,-0.492315462110302,
-0.0949063297889192));
#71493=CARTESIAN_POINT('Ctrl Pts',(0.131480407762813,-0.502713189220506,
-0.0869569357695075));
#71494=CARTESIAN_POINT('Ctrl Pts',(0.299973644816456,-0.424211661008035,
-0.0790075417500954));
#71495=CARTESIAN_POINT('Ctrl Pts',(0.396928131928234,-0.292855671844219,
-0.0710581477306837));
#71496=CARTESIAN_POINT('Ctrl Pts',(0.49388261904001,-0.161499682680408,
-0.0631087537112723));
#71497=CARTESIAN_POINT('Ctrl Pts',(0.519298356209934,0.0227107674347409,
-0.0551593596918611));
#71498=CARTESIAN_POINT('Ctrl Pts',(0.461195613234472,0.175309184465985,
-0.0472099656724497));
#71499=CARTESIAN_POINT('Ctrl Pts',(0.407084154180315,0.317425073872489,
-0.0398066437816331));
#71500=CARTESIAN_POINT('Ctrl Pts',(0.280534470088716,0.432122845008194,
-0.0324033218908166));
#71501=CARTESIAN_POINT('Ctrl Pts',(0.134559949224566,0.474484556402355,
-0.0249999999999999));
#71502=CARTESIAN_POINT('',(-0.236230756092323,-0.331488661006752,-3.4575));
#71503=CARTESIAN_POINT('Ctrl Pts',(-0.236825839292543,-0.331770464644072,
-3.4575));
#71504=CARTESIAN_POINT('Ctrl Pts',(-0.24498592505692,-0.327184164044185,
-3.4575));
#71505=CARTESIAN_POINT('Ctrl Pts',(-0.252961058460668,-0.322307537184471,
-3.4575));
#71506=CARTESIAN_POINT('Ctrl Pts',(-0.2607333681375,-0.317144081077849,
-3.4575));
#71507=CARTESIAN_POINT('Ctrl Pts',(-0.275646574082145,-0.307236642040296,
-3.4575));
#71508=CARTESIAN_POINT('Ctrl Pts',(-0.289813760355341,-0.296274605501924,
-3.4575));
#71509=CARTESIAN_POINT('Ctrl Pts',(-0.303204978700601,-0.284381130110945,
-3.4575));
#71510=CARTESIAN_POINT('Ctrl Pts',(-0.30899969474596,-0.279234525007043,
-3.4575));
#71511=CARTESIAN_POINT('Ctrl Pts',(-0.314648992460393,-0.273913228093762,
-3.4575));
#71512=CARTESIAN_POINT('Ctrl Pts',(-0.320149827110806,-0.268426052542454,
-3.4575));
#71513=CARTESIAN_POINT('Ctrl Pts',(-0.325348715088508,-0.26324007390136,
-3.4575));
#71514=CARTESIAN_POINT('Ctrl Pts',(-0.330409414487503,-0.257911292679725,
-3.4575));
#71515=CARTESIAN_POINT('Ctrl Pts',(-0.335324960153577,-0.252453580040169,
-3.4575));
#71516=CARTESIAN_POINT('Ctrl Pts',(-0.345907619881657,-0.240703691079382,
-3.4575));
#71517=CARTESIAN_POINT('Ctrl Pts',(-0.355825502531319,-0.228349378127429,
-3.4575));
#71518=CARTESIAN_POINT('Ctrl Pts',(-0.365056952902446,-0.215469067942917,
-3.4575));
#71519=CARTESIAN_POINT('Ctrl Pts',(-0.371061713935393,-0.207090841166103,
-3.4575));
#71520=CARTESIAN_POINT('Ctrl Pts',(-0.376775924245827,-0.198489825135662,
-3.4575));
#71521=CARTESIAN_POINT('Ctrl Pts',(-0.382192007793225,-0.189685455619147,
-3.4575));
#71522=CARTESIAN_POINT('Ctrl Pts',(-0.386628891731828,-0.182472870112388,
-3.4575));
#71523=CARTESIAN_POINT('Ctrl Pts',(-0.39086776775683,-0.175119290841785,
-3.4575));
#71524=CARTESIAN_POINT('Ctrl Pts',(-0.394890010680429,-0.16766200827966,
-3.4575));
#71525=CARTESIAN_POINT('Ctrl Pts',(-0.40620807148356,-0.146678199228982,
-3.4575));
#71526=CARTESIAN_POINT('Ctrl Pts',(-0.415836408714529,-0.124843045338353,
-3.4575));
#71527=CARTESIAN_POINT('Ctrl Pts',(-0.423701483345752,-0.10240131787515,
-3.4575));
#71528=CARTESIAN_POINT('Ctrl Pts',(-0.428572017874585,-0.088504029721993,
-3.4575));
#71529=CARTESIAN_POINT('Ctrl Pts',(-0.432765748438528,-0.0743732157083639,
-3.4575));
#71530=CARTESIAN_POINT('Ctrl Pts',(-0.436257497594041,-0.0600606864200386,
-3.4575));
#71531=CARTESIAN_POINT('Ctrl Pts',(-0.439096686594963,-0.0484229730789673,
-3.4575));
#71532=CARTESIAN_POINT('Ctrl Pts',(-0.441471662517333,-0.0366650055184638,
-3.4575));
#71533=CARTESIAN_POINT('Ctrl Pts',(-0.443365374066457,-0.0248132790866735,
-3.4575));
#71534=CARTESIAN_POINT('Ctrl Pts',(-0.444259517728958,-0.0192173127508425,
-3.4575));
#71535=CARTESIAN_POINT('Ctrl Pts',(-0.44504604416487,-0.0136010248224324,
-3.4575));
#71536=CARTESIAN_POINT('Ctrl Pts',(-0.445721847253133,-0.00798087641735873,
-3.4575));
#71537=CARTESIAN_POINT('Ctrl Pts',(-0.448130298890454,0.0120484129766512,
-3.4575));
#71538=CARTESIAN_POINT('Ctrl Pts',(-0.449141601140773,0.0321699224781787,
-3.4575));
#71539=CARTESIAN_POINT('Ctrl Pts',(-0.448704141806069,0.0522508947148586,
-3.4575));
#71540=CARTESIAN_POINT('Ctrl Pts',(-0.448285329643317,0.0714758940357306,
-3.4575));
#71541=CARTESIAN_POINT('Ctrl Pts',(-0.446538897531985,0.0906642480359715,
-3.4575));
#71542=CARTESIAN_POINT('Ctrl Pts',(-0.443540878719968,0.109704804163937,
-3.4575));
#71543=CARTESIAN_POINT('Ctrl Pts',(-0.441467971943461,0.122869930969648,
-3.4575));
#71544=CARTESIAN_POINT('Ctrl Pts',(-0.438796223272655,0.135964533139785,
-3.4575));
#71545=CARTESIAN_POINT('Ctrl Pts',(-0.435544631086097,0.14895191104839,
-3.4575));
#71546=CARTESIAN_POINT('Ctrl Pts',(-0.434142676634257,0.154551540778085,
-3.4575));
#71547=CARTESIAN_POINT('Ctrl Pts',(-0.432632778326946,0.160130868848963,
-3.4575));
#71548=CARTESIAN_POINT('Ctrl Pts',(-0.43102066709347,0.165673526206262,
-3.4575));
#71549=CARTESIAN_POINT('Ctrl Pts',(-0.424096345244513,0.189480285096999,
-3.4575));
#71550=CARTESIAN_POINT('Ctrl Pts',(-0.415275503745151,0.212673748338969,
-3.4575));
#71551=CARTESIAN_POINT('Ctrl Pts',(-0.404720542116381,0.235028731869538,
-3.4575));
#71552=CARTESIAN_POINT('Ctrl Pts',(-0.398703059276772,0.247773518113789,
-3.4575));
#71553=CARTESIAN_POINT('Ctrl Pts',(-0.392120926506971,0.260245908659614,
-3.4575));
#71554=CARTESIAN_POINT('Ctrl Pts',(-0.384996760852124,0.272403462043344,
-3.4575));
#71555=CARTESIAN_POINT('Ctrl Pts',(-0.378169594196076,0.284054179769713,
-3.4575));
#71556=CARTESIAN_POINT('Ctrl Pts',(-0.370844587868519,0.295415819953137,
-3.4575));
#71557=CARTESIAN_POINT('Ctrl Pts',(-0.36304260791885,0.306464321135028,
-3.4575));
#71558=CARTESIAN_POINT('Ctrl Pts',(-0.358157538916131,0.313382140842121,
-3.4575));
#71559=CARTESIAN_POINT('Ctrl Pts',(-0.353081459306764,0.320181708144073,
-3.4575));
#71560=CARTESIAN_POINT('Ctrl Pts',(-0.347840276198119,0.326830643032922,
-3.4575));
#71561=CARTESIAN_POINT('Ctrl Pts',(-0.332031181725627,0.346885969782693,
-3.4575));
#71562=CARTESIAN_POINT('Ctrl Pts',(-0.314699132938717,0.36561178190024,
-3.4575));
#71563=CARTESIAN_POINT('Ctrl Pts',(-0.296017391187458,0.382867065282375,
-3.4575));
#71564=CARTESIAN_POINT('Ctrl Pts',(-0.277377076349629,0.400084084934052,
-3.4575));
#71565=CARTESIAN_POINT('Ctrl Pts',(-0.257392306372362,0.415838166281252,
-3.4575));
#71566=CARTESIAN_POINT('Ctrl Pts',(-0.236192234025625,0.429962070234951,
-3.4575));
#71567=CARTESIAN_POINT('Ctrl Pts',(-0.229849434346378,0.434187767770413,
-3.4575));
#71568=CARTESIAN_POINT('Ctrl Pts',(-0.223397598075027,0.438267297508737,
-3.4575));
#71569=CARTESIAN_POINT('Ctrl Pts',(-0.216839587231055,0.442195480991683,
-3.4575));
#71570=CARTESIAN_POINT('Ctrl Pts',(-0.236825839292548,-0.331770464644068,
-3.4575));
#71571=CARTESIAN_POINT('Ctrl Pts',(-0.134134507353825,-0.404131753741505,
-3.45009667810918));
#71572=CARTESIAN_POINT('Ctrl Pts',(0.154860635227925,-0.45076080285477,
-3.43474396219895));
#71573=CARTESIAN_POINT('Ctrl Pts',(0.464962259161517,-0.123953347438615,
-3.41144185226931));
#71574=CARTESIAN_POINT('Ctrl Pts',(0.356070675898753,0.323893827689701,
-3.38759367021108));
#71575=CARTESIAN_POINT('Ctrl Pts',(-0.0797710380057583,0.474714264786181,
-3.36374548815284));
#71576=CARTESIAN_POINT('Ctrl Pts',(-0.370502916327729,0.246248299571174,
-3.34462050911336));
#71577=CARTESIAN_POINT('Ctrl Pts',(-0.406716221540625,0.0553845436928955,
-3.33344492409328));
#71578=CARTESIAN_POINT('Ctrl Pts',(-0.406471795258815,0.00019713841655692,
-3.33021873309261));
#71579=CARTESIAN_POINT('Origin',(-4.52129938221115E-17,0.,-3.4575));
#71580=CARTESIAN_POINT('',(-0.4925,-6.03138548580071E-17,-3.4575));
#71581=CARTESIAN_POINT('Origin',(0.,0.,-3.4575));
#71582=CARTESIAN_POINT('Origin',(0.,0.,-3.4575));
#71583=CARTESIAN_POINT('',(0.23623075609233,-0.331488661006747,-3.4575));
#71584=CARTESIAN_POINT('Ctrl Pts',(0.217494704229604,0.442648936192906,
-3.4575));
#71585=CARTESIAN_POINT('Ctrl Pts',(0.227151161842225,0.436927031618297,
-3.4575));
#71586=CARTESIAN_POINT('Ctrl Pts',(0.236581718719849,0.430861971334928,
-3.4575));
#71587=CARTESIAN_POINT('Ctrl Pts',(0.245765220410661,0.424452886643136,
-3.4575));
#71588=CARTESIAN_POINT('Ctrl Pts',(0.261762891981356,0.41328825299684,-3.4575));
#71589=CARTESIAN_POINT('Ctrl Pts',(0.277011667809708,0.401080195483046,
-3.4575));
#71590=CARTESIAN_POINT('Ctrl Pts',(0.291463300048419,0.38793234921563,-3.4575));
#71591=CARTESIAN_POINT('Ctrl Pts',(0.299171148542744,0.380919881323978,
-3.4575));
#71592=CARTESIAN_POINT('Ctrl Pts',(0.306652003669299,0.373639876799799,
-3.4575));
#71593=CARTESIAN_POINT('Ctrl Pts',(0.313896822610377,0.366107029970977,
-3.4575));
#71594=CARTESIAN_POINT('Ctrl Pts',(0.318563214856714,0.361255118788553,
-3.4575));
#71595=CARTESIAN_POINT('Ctrl Pts',(0.323129211638469,0.35630067653166,-3.4575));
#71596=CARTESIAN_POINT('Ctrl Pts',(0.327587182139254,0.351254289248762,
-3.4575));
#71597=CARTESIAN_POINT('Ctrl Pts',(0.344475362309805,0.332137003113971,
-3.4575));
#71598=CARTESIAN_POINT('Ctrl Pts',(0.35984203627762,0.311676053598004,-3.4575));
#71599=CARTESIAN_POINT('Ctrl Pts',(0.37356594240373,0.290097909978538,-3.4575));
#71600=CARTESIAN_POINT('Ctrl Pts',(0.378533439188415,0.282287498127555,
-3.4575));
#71601=CARTESIAN_POINT('Ctrl Pts',(0.383285254569069,0.274330522722929,
-3.4575));
#71602=CARTESIAN_POINT('Ctrl Pts',(0.387814010524765,0.266237265287823,
-3.4575));
#71603=CARTESIAN_POINT('Ctrl Pts',(0.390544998544752,0.261356766246991,
-3.4575));
#71604=CARTESIAN_POINT('Ctrl Pts',(0.39319399866812,0.25642801685015,-3.4575));
#71605=CARTESIAN_POINT('Ctrl Pts',(0.395755363081162,0.251461797430097,
-3.4575));
#71606=CARTESIAN_POINT('Ctrl Pts',(0.407165733601745,0.229338274755702,
-3.4575));
#71607=CARTESIAN_POINT('Ctrl Pts',(0.416866719135654,0.20642676787138,-3.4575));
#71608=CARTESIAN_POINT('Ctrl Pts',(0.424745143572822,0.182936674070674,
-3.4575));
#71609=CARTESIAN_POINT('Ctrl Pts',(0.432423237211658,0.160043881073128,
-3.4575));
#71610=CARTESIAN_POINT('Ctrl Pts',(0.438370511455948,0.13660029841765,-3.4575));
#71611=CARTESIAN_POINT('Ctrl Pts',(0.442433727764424,0.112796995411841,
-3.4575));
#71612=CARTESIAN_POINT('Ctrl Pts',(0.443454271781346,0.106818401947623,
-3.4575));
#71613=CARTESIAN_POINT('Ctrl Pts',(0.444355706852267,0.100817152549543,
-3.4575));
#71614=CARTESIAN_POINT('Ctrl Pts',(0.445135080697175,0.0947963852933782,
-3.4575));
#71615=CARTESIAN_POINT('Ctrl Pts',(0.445940883140782,0.088571453575303,
-3.4575));
#71616=CARTESIAN_POINT('Ctrl Pts',(0.44661511688423,0.0823332556971779,
-3.4575));
#71617=CARTESIAN_POINT('Ctrl Pts',(0.447154936518576,0.0760926679104064,
-3.4575));
#71618=CARTESIAN_POINT('Ctrl Pts',(0.448735717878663,0.0578180364934373,
-3.4575));
#71619=CARTESIAN_POINT('Ctrl Pts',(0.449167900960623,0.0395027025829728,
-3.4575));
#71620=CARTESIAN_POINT('Ctrl Pts',(0.448392616133184,0.021231823691261,
-3.4575));
#71621=CARTESIAN_POINT('Ctrl Pts',(0.447505993275466,0.000337078582567013,
-3.4575));
#71622=CARTESIAN_POINT('Ctrl Pts',(0.445040447967601,-0.020500296725011,
-3.4575));
#71623=CARTESIAN_POINT('Ctrl Pts',(0.4410627946643,-0.0411137620726926,
-3.4575));
#71624=CARTESIAN_POINT('Ctrl Pts',(0.439232335579409,-0.0505997836134454,
-3.4575));
#71625=CARTESIAN_POINT('Ctrl Pts',(0.437081273421581,-0.06003821102663,
-3.4575));
#71626=CARTESIAN_POINT('Ctrl Pts',(0.434614336619626,-0.069411603243447,
-3.4575));
#71627=CARTESIAN_POINT('Ctrl Pts',(0.432800575766688,-0.0763031830555531,
-3.4575));
#71628=CARTESIAN_POINT('Ctrl Pts',(0.430814830929698,-0.0831625935919254,
-3.4575));
#71629=CARTESIAN_POINT('Ctrl Pts',(0.428666939775117,-0.0899588063351191,
-3.4575));
#71630=CARTESIAN_POINT('Ctrl Pts',(0.421594724438486,-0.112336234488735,
-3.4575));
#71631=CARTESIAN_POINT('Ctrl Pts',(0.412755846768818,-0.13408393119108,
-3.4575));
#71632=CARTESIAN_POINT('Ctrl Pts',(0.402255176200046,-0.154969058094331,
-3.4575));
#71633=CARTESIAN_POINT('Ctrl Pts',(0.396775801082079,-0.165867166357014,
-3.4575));
#71634=CARTESIAN_POINT('Ctrl Pts',(0.390843182289698,-0.176530007122764,
-3.4575));
#71635=CARTESIAN_POINT('Ctrl Pts',(0.384467909415291,-0.186920817753301,
-3.4575));
#71636=CARTESIAN_POINT('Ctrl Pts',(0.377607033364656,-0.198103094215212,
-3.4575));
#71637=CARTESIAN_POINT('Ctrl Pts',(0.37023347161565,-0.208970394721843,
-3.4575));
#71638=CARTESIAN_POINT('Ctrl Pts',(0.362365932264957,-0.21948819497612,
-3.4575));
#71639=CARTESIAN_POINT('Ctrl Pts',(0.358211148066264,-0.225042560623827,
-3.4575));
#71640=CARTESIAN_POINT('Ctrl Pts',(0.353916358841732,-0.230501651312997,
-3.4575));
#71641=CARTESIAN_POINT('Ctrl Pts',(0.349500387143519,-0.235841268640749,
-3.4575));
#71642=CARTESIAN_POINT('Ctrl Pts',(0.335009267560686,-0.253363354041415,
-3.4575));
#71643=CARTESIAN_POINT('Ctrl Pts',(0.319184772663791,-0.26964621528388,
-3.4575));
#71644=CARTESIAN_POINT('Ctrl Pts',(0.302148777404973,-0.284534751709626,
-3.4575));
#71645=CARTESIAN_POINT('Ctrl Pts',(0.285535708385829,-0.299053673526473,
-3.4575));
#71646=CARTESIAN_POINT('Ctrl Pts',(0.267769531136388,-0.312247224204637,
-3.4575));
#71647=CARTESIAN_POINT('Ctrl Pts',(0.248942033157039,-0.323927335938675,
-3.4575));
#71648=CARTESIAN_POINT('Ctrl Pts',(0.24475711745839,-0.326523553609836,
-3.4575));
#71649=CARTESIAN_POINT('Ctrl Pts',(0.240519713189094,-0.329044800635418,
-3.4575));
#71650=CARTESIAN_POINT('Ctrl Pts',(0.236230756092332,-0.331488661006746,
-3.4575));
#71651=CARTESIAN_POINT('Origin',(0.,0.,-3.4575));
#71652=CARTESIAN_POINT('Origin',(0.,0.,-3.73478126690739));
#71653=CARTESIAN_POINT('Ctrl Pts',(0.236230756092329,-0.331488661006748,
-3.4575));
#71654=CARTESIAN_POINT('Ctrl Pts',(0.291420873096492,-0.292158196341315,
-3.45352530299029));
#71655=CARTESIAN_POINT('Ctrl Pts',(0.380867829859202,-0.185560026793827,
-3.44557590897088));
#71656=CARTESIAN_POINT('Ctrl Pts',(0.440039431000898,0.0889589528409691,
-3.42967712093207));
#71657=CARTESIAN_POINT('Ctrl Pts',(0.241551031548769,0.416306162933455,
-3.40980363588352));
#71658=CARTESIAN_POINT('Ctrl Pts',(-0.22013291818294,0.428338358383622,
-3.3859554538253));
#71659=CARTESIAN_POINT('Ctrl Pts',(-0.401074963635459,0.16153375529599,
-3.36928133083325));
#71660=CARTESIAN_POINT('Ctrl Pts',(-0.407613746698895,0.0133760251655175,
-3.36055660186061));
#71661=CARTESIAN_POINT('Ctrl Pts',(-0.407524236888043,0.000202371512057618,
-3.35978126690739));
#71662=CARTESIAN_POINT('Ctrl Pts',(0.285821514250022,-0.401076441581682,
-3.50683458050225));
#71663=CARTESIAN_POINT('Ctrl Pts',(0.35259742046437,-0.353489526343442,
-3.50285988349255));
#71664=CARTESIAN_POINT('Ctrl Pts',(0.460821535943143,-0.224513728524654,
-3.49491048947313));
#71665=CARTESIAN_POINT('Ctrl Pts',(0.532414739633811,0.10763366729929,-3.47901170143431));
#71666=CARTESIAN_POINT('Ctrl Pts',(0.292258648907431,0.503699263591024,
-3.45913821638578));
#71667=CARTESIAN_POINT('Ctrl Pts',(-0.266344336580512,0.518257318520905,
-3.43529003432755));
#71668=CARTESIAN_POINT('Ctrl Pts',(-0.579463933371572,0.0565528565653229,
-3.41144185226931));
#71669=CARTESIAN_POINT('Ctrl Pts',(-0.36140270524706,-0.456693171189222,
-3.38759367021108));
#71670=CARTESIAN_POINT('Ctrl Pts',(0.188579049697867,-0.551047079719571,
-3.36374548815284));
#71671=CARTESIAN_POINT('Ctrl Pts',(0.565365809375224,-0.139648741035217,
-3.33989730609461));
#71672=CARTESIAN_POINT('Ctrl Pts',(0.42343405354387,0.39984578150713,-3.31604912403638));
#71673=CARTESIAN_POINT('Ctrl Pts',(-0.107093777855668,0.572455898084804,
-3.29220094197814));
#71674=CARTESIAN_POINT('Ctrl Pts',(-0.539328090055823,0.219750171019256,
-3.26835275991991));
#71675=CARTESIAN_POINT('Ctrl Pts',(-0.476670081241653,-0.334597761312887,
-3.24450457786167));
#71676=CARTESIAN_POINT('Ctrl Pts',(0.0234001526480324,-0.58191259930159,
-3.22065639580343));
#71677=CARTESIAN_POINT('Ctrl Pts',(0.501994730637598,-0.295245409122807,
-3.19680821374521));
#71678=CARTESIAN_POINT('Ctrl Pts',(0.519945729935783,0.262346662895907,
-3.17296003168696));
#71679=CARTESIAN_POINT('Ctrl Pts',(0.0607784178287687,0.579202235152385,
-3.14911184962874));
#71680=CARTESIAN_POINT('Ctrl Pts',(-0.454160536196269,0.364564524813034,
-3.1252636675705));
#71681=CARTESIAN_POINT('Ctrl Pts',(-0.552348639443532,-0.184608179799961,
-3.10141548551227));
#71682=CARTESIAN_POINT('Ctrl Pts',(-0.143685264422752,-0.564379059995498,
-3.07756730345403));
#71683=CARTESIAN_POINT('Ctrl Pts',(0.396827877163523,-0.426259070653351,
-3.0537191213958));
#71684=CARTESIAN_POINT('Ctrl Pts',(0.573200113780989,0.103008764053386,
-3.02987093933756));
#71685=CARTESIAN_POINT('Ctrl Pts',(0.223587044257181,0.537752736345724,
-3.00602275727933));
#71686=CARTESIAN_POINT('Ctrl Pts',(-0.331196067315227,0.479038969850997,
-2.98217457522109));
#71687=CARTESIAN_POINT('Ctrl Pts',(-0.582063927005535,-0.0192550475321526,
-2.95832639316286));
#71688=CARTESIAN_POINT('Ctrl Pts',(-0.298812798670071,-0.499880068214747,
-2.93447821110462));
#71689=CARTESIAN_POINT('Ctrl Pts',(0.258637744622312,-0.521800429360905,
-2.91063002904639));
#71690=CARTESIAN_POINT('Ctrl Pts',(0.578754684066404,-0.0649013637714588,
-2.88678184698815));
#71691=CARTESIAN_POINT('Ctrl Pts',(0.367789296146031,0.451553103041694,
-2.86293366492992));
#71692=CARTESIAN_POINT('Ctrl Pts',(-0.1806703713665,0.553649156160662,-2.83908548287168));
#71693=CARTESIAN_POINT('Ctrl Pts',(-0.563341590261651,0.147700453392908,
-2.81523730081345));
#71694=CARTESIAN_POINT('Ctrl Pts',(-0.429073990452302,-0.393782531289495,
-2.79138911875521));
#71695=CARTESIAN_POINT('Ctrl Pts',(0.0989245277950369,-0.573919078817807,
-2.76754093669698));
#71696=CARTESIAN_POINT('Ctrl Pts',(0.536146988652502,-0.227410592970535,
-2.74369275463874));
#71697=CARTESIAN_POINT('Ctrl Pts',(0.48138519743957,0.327776544187327,-2.71984457258051));
#71698=CARTESIAN_POINT('Ctrl Pts',(-0.0151098149378764,0.582186280090831,
-2.69599639052227));
#71699=CARTESIAN_POINT('Ctrl Pts',(-0.497739616547707,0.302364755474486,
-2.67214820846404));
#71700=CARTESIAN_POINT('Ctrl Pts',(-0.523628900812201,-0.254915565370088,
-2.6483000264058));
#71701=CARTESIAN_POINT('Ctrl Pts',(-0.0690208987404531,-0.578277862943811,
-2.62445184434757));
#71702=CARTESIAN_POINT('Ctrl Pts',(0.448922710846462,-0.370995378569811,
-2.60060366228934));
#71703=CARTESIAN_POINT('Ctrl Pts',(0.55492163212046,0.176723381131619,-2.5767554802311));
#71704=CARTESIAN_POINT('Ctrl Pts',(0.151708136070267,0.562275566500915,
-2.55290729817287));
#71705=CARTESIAN_POINT('Ctrl Pts',(-0.390717209409772,0.431867147980593,
-2.52905911611463));
#71706=CARTESIAN_POINT('Ctrl Pts',(-0.574608947300046,-0.0948352725338707,
-2.5052109340564));
#71707=CARTESIAN_POINT('Ctrl Pts',(-0.231222608189202,-0.534514056593488,
-2.48136275199816));
#71708=CARTESIAN_POINT('Ctrl Pts',(0.324340399555256,-0.483707015093002,
-2.45751456993993));
#71709=CARTESIAN_POINT('Ctrl Pts',(0.582279113465016,0.010963815769983,
-2.43366638788169));
#71710=CARTESIAN_POINT('Ctrl Pts',(0.305901380218176,0.495573926689509,
-2.40981820582346));
#71711=CARTESIAN_POINT('Ctrl Pts',(-0.251180460180701,0.525430821000496,
-2.38597002376523));
#71712=CARTESIAN_POINT('Ctrl Pts',(-0.577771719730372,0.0731369339913324,
-2.36212184170699));
#71713=CARTESIAN_POINT('Ctrl Pts',(-0.374182649237275,-0.446269555586775,
-2.33827365964876));
#71714=CARTESIAN_POINT('Ctrl Pts',(0.172767429928028,-0.556165970183279,
-2.31442547759052));
#71715=CARTESIAN_POINT('Ctrl Pts',(0.561181031983256,-0.155708126236403,
-2.29057729553229));
#71716=CARTESIAN_POINT('Ctrl Pts',(0.434638407227192,0.387632075810108,
-2.26672911347405));
#71717=CARTESIAN_POINT('Ctrl Pts',(-0.0907412085475953,0.575269679633096,
-2.24288093141582));
#71718=CARTESIAN_POINT('Ctrl Pts',(-0.5328540214427,0.235022899025148,-2.21903274935759));
#71719=CARTESIAN_POINT('Ctrl Pts',(-0.486004305875971,-0.320887808905013,
-2.19518456729935));
#71720=CARTESIAN_POINT('Ctrl Pts',(0.00681726066985583,-0.582342421768158,
-2.17133638524111));
#71721=CARTESIAN_POINT('Ctrl Pts',(0.493383108237918,-0.30942249391299,
-2.14748820318288));
#71722=CARTESIAN_POINT('Ctrl Pts',(0.527206098669985,0.24743261862377,-2.12364002112464));
#71723=CARTESIAN_POINT('Ctrl Pts',(0.0772492607576471,0.57723627999827,
-2.09979183906641));
#71724=CARTESIAN_POINT('Ctrl Pts',(-0.443593771763116,0.377350946582644,
-2.07594365700817));
#71725=CARTESIAN_POINT('Ctrl Pts',(-0.557382107269562,-0.168802718371432,
-2.05209547494994));
#71726=CARTESIAN_POINT('Ctrl Pts',(-0.159700221059351,-0.560058042195126,
-2.02824729289171));
#71727=CARTESIAN_POINT('Ctrl Pts',(0.384527286921104,-0.437387627679315,
-2.00439911083347));
#71728=CARTESIAN_POINT('Ctrl Pts',(0.575901242316084,0.0866425434335488,
-1.98055092877524));
#71729=CARTESIAN_POINT('Ctrl Pts',(0.238811272779486,0.53116696737211,-1.956702746717));
#71730=CARTESIAN_POINT('Ctrl Pts',(-0.317418947303206,0.488276953302907,
-1.93285456465877));
#71731=CARTESIAN_POINT('Ctrl Pts',(-0.58237620179046,-0.00267035989340219,
-1.90900638260054));
#71732=CARTESIAN_POINT('Ctrl Pts',(-0.312927918017016,-0.491167272280409,
-1.8851582005423));
#71733=CARTESIAN_POINT('Ctrl Pts',(0.243672230737431,-0.528954643803501,
-1.86131001848407));
#71734=CARTESIAN_POINT('Ctrl Pts',(0.576671570897583,-0.0813576705194944,
-1.83746183642583));
#71735=CARTESIAN_POINT('Ctrl Pts',(0.380500109954069,0.440895495053855,
-1.8136136543676));
#71736=CARTESIAN_POINT('Ctrl Pts',(-0.164829447496658,0.558569981713831,
-1.78976547230936));
#71737=CARTESIAN_POINT('Ctrl Pts',(-0.558906654078905,0.163684218115762,
-1.76591729025113));
#71738=CARTESIAN_POINT('Ctrl Pts',(-0.44011466993486,-0.381403000174322,
-1.74206910819289));
#71739=CARTESIAN_POINT('Ctrl Pts',(0.0825394850188265,-0.576503603324966,
-1.71822092613466));
#71740=CARTESIAN_POINT('Ctrl Pts',(0.529452979925558,-0.242587537358763,
-1.69437274407642));
#71741=CARTESIAN_POINT('Ctrl Pts',(0.490524842136848,0.313933990642086,
-1.67052456201819));
#71742=CARTESIAN_POINT('Ctrl Pts',(0.00147667628643591,0.582380451819074,
-1.64667637995995));
#71743=CARTESIAN_POINT('Ctrl Pts',(-0.488926531173269,0.316417474784054,
-1.62282819790172));
#71744=CARTESIAN_POINT('Ctrl Pts',(-0.530676367739226,-0.239899487196084,
-1.59898001584349));
#71745=CARTESIAN_POINT('Ctrl Pts',(-0.0854619549556686,-0.576077621062474,
-1.57513183378525));
#71746=CARTESIAN_POINT('Ctrl Pts',(0.438174862277943,-0.383629979669929,
-1.55128365172701));
#71747=CARTESIAN_POINT('Ctrl Pts',(0.559729533283666,0.160847818772567,
-1.52743546966878));
#71748=CARTESIAN_POINT('Ctrl Pts',(0.167659915392895,0.557726926016926,
-1.50358728761054));
#71749=CARTESIAN_POINT('Ctrl Pts',(-0.378259373989984,0.442819395716301,
-1.47973910555231));
#71750=CARTESIAN_POINT('Ctrl Pts',(-0.5770767321164,-0.0784322413532939,
-1.45589092349408));
#71751=CARTESIAN_POINT('Ctrl Pts',(-0.246351501283537,-0.527712146012568,
-1.43204274143584));
#71752=CARTESIAN_POINT('Ctrl Pts',(0.310433115630021,-0.49274785839624,
-1.40819455937761));
#71753=CARTESIAN_POINT('Ctrl Pts',(0.582355171638496,-0.00562363758986257,
-1.38434637731937));
#71754=CARTESIAN_POINT('Ctrl Pts',(0.319890987272491,0.486660998535609,
-1.36049819526114));
#71755=CARTESIAN_POINT('Ctrl Pts',(-0.23611457930063,0.532371183175357,
-1.3366500132029));
#71756=CARTESIAN_POINT('Ctrl Pts',(-0.575454460609791,0.0895619059541361,
-1.31280183114467));
#71757=CARTESIAN_POINT('Ctrl Pts',(-0.386740397026913,-0.435432011387898,
-1.28895364908643));
#71758=CARTESIAN_POINT('Ctrl Pts',(0.156858034091794,-0.560860703182797,
-1.2651054670282));
#71759=CARTESIAN_POINT('Ctrl Pts',(0.556518917828539,-0.171627111298872,
-1.24125728496997));
#71760=CARTESIAN_POINT('Ctrl Pts',(0.445501667877689,0.375096567768941,
-1.21740910291173));
#71761=CARTESIAN_POINT('Ctrl Pts',(-0.0743210206990269,0.577620599629289,
-1.1935609208535));
#71762=CARTESIAN_POINT('Ctrl Pts',(-0.52594455390394,0.250102973698091,
-1.16971273879526));
#71763=CARTESIAN_POINT('Ctrl Pts',(-0.494945889360727,-0.306916499782533,
-1.14586455673702));
#71764=CARTESIAN_POINT('Ctrl Pts',(-0.00977031374086975,-0.582300362530584,
-1.12201637467879));
#71765=CARTESIAN_POINT('Ctrl Pts',(0.484370789243626,-0.323348279354245,
-1.09816819262055));
#71766=CARTESIAN_POINT('Ctrl Pts',(0.534039004174506,0.232317698968773,
-1.07432001056233));
#71767=CARTESIAN_POINT('Ctrl Pts',(0.0936573156226028,0.574802121137536,
-1.05047182850409));
#71768=CARTESIAN_POINT('Ctrl Pts',(-0.432667081462839,0.389831204308058,
-1.02662364644585));
#71769=CARTESIAN_POINT('Ctrl Pts',(-0.561963434054077,-0.15286029576054,
-1.00277546438762));
#71770=CARTESIAN_POINT('Ctrl Pts',(-0.175585604672873,-0.555282690767055,
-0.978927282329385));
#71771=CARTESIAN_POINT('Ctrl Pts',(0.371914741884562,-0.448161350411617,
-0.955079100271149));
#71772=CARTESIAN_POINT('Ctrl Pts',(0.578135178286308,0.0702060315197663,
-0.931230918212915));
#71773=CARTESIAN_POINT('Ctrl Pts',(0.253841764380009,0.524150293227283,
-0.90738273615468));
#71774=CARTESIAN_POINT('Ctrl Pts',(-0.303384321413146,0.497118823576847,
-0.883534554096446));
#71775=CARTESIAN_POINT('Ctrl Pts',(-0.582216027274799,0.0139164944779112,
-0.859686372038211));
#71776=CARTESIAN_POINT('Ctrl Pts',(-0.326789175723116,-0.48205601942478,
-0.835838189979976));
#71777=CARTESIAN_POINT('Ctrl Pts',(0.228509038724162,-0.535679746168062,
-0.811990007921742));
#71778=CARTESIAN_POINT('Ctrl Pts',(0.574120635725452,-0.0977479762990466,
-0.788141825863507));
#71779=CARTESIAN_POINT('Ctrl Pts',(0.39290224478655,0.429880212701446,-0.764293643805274));
#71780=CARTESIAN_POINT('Ctrl Pts',(-0.148854806480243,0.563037669982351,
-0.740445461747037));
#71781=CARTESIAN_POINT('Ctrl Pts',(-0.554018307532132,0.179535194795418,
-0.716597279688804));
#71782=CARTESIAN_POINT('Ctrl Pts',(-0.450798308426413,-0.368714057674789,
-0.692749097630568));
#71783=CARTESIAN_POINT('Ctrl Pts',(0.0660874824133674,-0.578620441994957,
-0.668900915572334));
#71784=CARTESIAN_POINT('Ctrl Pts',(0.522329455071808,-0.257567683750478,
-0.645052733514099));
#71785=CARTESIAN_POINT('Ctrl Pts',(0.499266550653832,0.299836759625578,
-0.621204551455865));
#71786=CARTESIAN_POINT('Ctrl Pts',(0.0180619699673387,0.582102170145686,
-0.597356369397629));
#71787=CARTESIAN_POINT('Ctrl Pts',(-0.479716807224914,0.330213501908238,
-0.573508187339396));
#71788=CARTESIAN_POINT('Ctrl Pts',(-0.537293324476905,-0.224688791695386,
-0.549660005281161));
#71789=CARTESIAN_POINT('Ctrl Pts',(-0.101833683409545,-0.5734100389165,
-0.525811823222927));
#71790=CARTESIAN_POINT('Ctrl Pts',(0.427071551879351,-0.395953362766007,
-0.501963641164691));
#71791=CARTESIAN_POINT('Ctrl Pts',(0.564083346009815,0.144841769399363,
-0.478115459106457));
#71792=CARTESIAN_POINT('Ctrl Pts',(0.183475701526128,0.552725832147485,
-0.454267277048223));
#71793=CARTESIAN_POINT('Ctrl Pts',(-0.365494716062787,0.453412408381549,
-0.430419094989988));
#71794=CARTESIAN_POINT('Ctrl Pts',(-0.579076292012319,-0.0619655825398327,
-0.406570912931754));
#71795=CARTESIAN_POINT('Ctrl Pts',(-0.261280685166963,-0.520482131141858,
-0.382722730873519));
#71796=CARTESIAN_POINT('Ctrl Pts',(0.296274267374466,-0.501388962884901,
-0.358874548815284));
#71797=CARTESIAN_POINT('Ctrl Pts',(0.581958272836576,-0.0222065277132291,
-0.335026366757049));
#71798=CARTESIAN_POINT('Ctrl Pts',(0.333622090090629,0.477353266851129,
-0.311178184698815));
#71799=CARTESIAN_POINT('Ctrl Pts',(-0.220859081953995,0.538879665737125,
-0.28733000264058));
#71800=CARTESIAN_POINT('Ctrl Pts',(-0.572666661988016,0.105914213558689,
-0.263481820582346));
#71801=CARTESIAN_POINT('Ctrl Pts',(-0.398991513710596,-0.424241210273597,
-0.239633638524111));
#71802=CARTESIAN_POINT('Ctrl Pts',(0.140835033897246,-0.565100468869743,
-0.215785456465876));
#71803=CARTESIAN_POINT('Ctrl Pts',(0.551379140596833,-0.187406810436341,
-0.191937274407642));
#71804=CARTESIAN_POINT('Ctrl Pts',(0.456053783787644,0.36225666087098,-0.168089092349407));
#71805=CARTESIAN_POINT('Ctrl Pts',(-0.0579370393971914,0.57950312116213,
-0.144240910291172));
#71806=CARTESIAN_POINT('Ctrl Pts',(-0.518422960159868,0.264979829502608,
-0.120392728232938));
#71807=CARTESIAN_POINT('Ctrl Pts',(-0.503844216133415,-0.292696019272375,
-0.0965445461747031));
#71808=CARTESIAN_POINT('Ctrl Pts',(-0.0256409405766145,-0.581782268696529,
-0.0726963641164688));
#71809=CARTESIAN_POINT('Ctrl Pts',(0.390234871038739,-0.377845479979599,
-0.0528228790679399));
#71810=CARTESIAN_POINT('Ctrl Pts',(0.509133042526885,-0.0595520553159744,
-0.0369240910291169));
#71811=CARTESIAN_POINT('Ctrl Pts',(0.487584520760919,0.107429610755057,
-0.0289746970097051));
#71812=CARTESIAN_POINT('Ctrl Pts',(0.457029747534529,0.183521279061925,
-0.0249999999999995));
#71813=CARTESIAN_POINT('Ctrl Pts',(0.269291261530791,-0.377880514723371,
-3.49038972033484));
#71814=CARTESIAN_POINT('Ctrl Pts',(0.332205238008411,-0.333045749676066,
-3.48641502332513));
#71815=CARTESIAN_POINT('Ctrl Pts',(0.434170300581829,-0.211529161281045,
-3.47846562930572));
#71816=CARTESIAN_POINT('Ctrl Pts',(0.501622970089507,0.10140876247985,-3.46256684126689));
#71817=CARTESIAN_POINT('Ctrl Pts',(0.275356109787877,0.474568230038501,
-3.44269335621837));
#71818=CARTESIAN_POINT('Ctrl Pts',(-0.250940530447988,0.488284331808477,
-3.41884517416013));
#71819=CARTESIAN_POINT('Ctrl Pts',(-0.545951112318035,0.0532821685155709,
-3.3949969921019));
#71820=CARTESIAN_POINT('Ctrl Pts',(-0.340501276371688,-0.430280696415537,
-3.37114881004366));
#71821=CARTESIAN_POINT('Ctrl Pts',(0.177672735114664,-0.519177724076906,
-3.34730062798543));
#71822=CARTESIAN_POINT('Ctrl Pts',(0.53266834175349,-0.131572270699203,
-3.32345244592719));
#71823=CARTESIAN_POINT('Ctrl Pts',(0.398945092545343,0.376721028864299,
-3.29960426386896));
#71824=CARTESIAN_POINT('Ctrl Pts',(-0.100900097099143,0.539348381000982,
-3.27575608181072));
#71825=CARTESIAN_POINT('Ctrl Pts',(-0.508136492563255,0.207041100214791,
-3.25190789975249));
#71826=CARTESIAN_POINT('Ctrl Pts',(-0.449102258268996,-0.31524657437266,
-3.22805971769425));
#71827=CARTESIAN_POINT('Ctrl Pts',(0.0220468240228047,-0.548258161663471,
-3.20421153563602));
#71828=CARTESIAN_POINT('Ctrl Pts',(0.472962277349624,-0.278170133177261,
-3.18036335357779));
#71829=CARTESIAN_POINT('Ctrl Pts',(0.489875095334758,0.247174058940269,
-3.15651517151955));
#71830=CARTESIAN_POINT('Ctrl Pts',(0.0572633479110232,0.545704549200595,
-3.13266698946132));
#71831=CARTESIAN_POINT('Ctrl Pts',(-0.427894534289014,0.343480234697789,
-3.10881880740308));
#71832=CARTESIAN_POINT('Ctrl Pts',(-0.520404009162348,-0.173931517218637,
-3.08497062534485));
#71833=CARTESIAN_POINT('Ctrl Pts',(-0.135375345069165,-0.531738660214371,
-3.06112244328661));
#71834=CARTESIAN_POINT('Ctrl Pts',(0.373877662541782,-0.401606727108627,
-3.03727426122838));
#71835=CARTESIAN_POINT('Ctrl Pts',(0.540049555593113,0.097051336717778,
-3.01342607917014));
#71836=CARTESIAN_POINT('Ctrl Pts',(0.210656071037705,0.506652248142177,
-2.98957789711191));
#71837=CARTESIAN_POINT('Ctrl Pts',(-0.312041614555778,0.45133414414963,
-2.96572971505367));
#71838=CARTESIAN_POINT('Ctrl Pts',(-0.548400737453845,-0.0181414476596504,
-2.94188153299544));
#71839=CARTESIAN_POINT('Ctrl Pts',(-0.281531205677612,-0.470969914692616,
-2.9180333509372));
#71840=CARTESIAN_POINT('Ctrl Pts',(0.243679642911331,-0.491622529740674,
-2.89418516887897));
#71841=CARTESIAN_POINT('Ctrl Pts',(0.545282881864391,-0.0611478466585844,
-2.87033698682073));
#71842=CARTESIAN_POINT('Ctrl Pts',(0.346518504027128,0.425437899891161,
-2.8464888047625));
#71843=CARTESIAN_POINT('Ctrl Pts',(-0.170221448704391,0.521629311562401,
-2.82264062270426));
#71844=CARTESIAN_POINT('Ctrl Pts',(-0.530761191691188,0.139158318880268,
-2.79879244064603));
#71845=CARTESIAN_POINT('Ctrl Pts',(-0.404258848331051,-0.371008441747237,
-2.77494425858779));
#71846=CARTESIAN_POINT('Ctrl Pts',(0.0932033089117306,-0.540726939877041,
-2.75109607652956));
#71847=CARTESIAN_POINT('Ctrl Pts',(0.505139367549047,-0.21425848794899,
-2.72724789447133));
#71848=CARTESIAN_POINT('Ctrl Pts',(0.453544679591033,0.308819856741773,
-2.70339971241309));
#71849=CARTESIAN_POINT('Ctrl Pts',(-0.0142359511907082,0.54851601434886,
-2.67955153035486));
#71850=CARTESIAN_POINT('Ctrl Pts',(-0.468953254291192,0.284877737975132,
-2.65570334829662));
#71851=CARTESIAN_POINT('Ctrl Pts',(-0.493345253046107,-0.240172732841578,
-2.63185516623839));
#71852=CARTESIAN_POINT('Ctrl Pts',(-0.0650291317033143,-0.544833637300124,
-2.60800698418015));
#71853=CARTESIAN_POINT('Ctrl Pts',(0.422959634269928,-0.349539165304978,
-2.58415880212192));
#71854=CARTESIAN_POINT('Ctrl Pts',(0.522828194919314,0.166502729410674,
-2.56031062006369));
#71855=CARTESIAN_POINT('Ctrl Pts',(0.142934220518859,0.52975682053983,-2.53646243800545));
#71856=CARTESIAN_POINT('Ctrl Pts',(-0.368120400242892,0.406890465885877,
-2.51261425594722));
#71857=CARTESIAN_POINT('Ctrl Pts',(-0.541376910381746,-0.0893505523727755,
-2.48876607388898));
#71858=CARTESIAN_POINT('Ctrl Pts',(-0.217850038395788,-0.503600874775611,
-2.46491789183075));
#71859=CARTESIAN_POINT('Ctrl Pts',(0.305582438714649,-0.455732216825863,
-2.44106970977251));
#71860=CARTESIAN_POINT('Ctrl Pts',(0.548603478781033,0.0103297324823055,
-2.41722152771428));
#71861=CARTESIAN_POINT('Ctrl Pts',(0.288209824929076,0.466912815328684,
-2.39337334565605));
#71862=CARTESIAN_POINT('Ctrl Pts',(-0.236653644395632,0.495042960659046,
-2.36952516359781));
#71863=CARTESIAN_POINT('Ctrl Pts',(-0.54435676646407,0.0689071194332546,
-2.34567698153958));
#71864=CARTESIAN_POINT('Ctrl Pts',(-0.352542102789,-0.420459922067392,-2.32182879948134));
#71865=CARTESIAN_POINT('Ctrl Pts',(0.16277556739852,-0.524000567711426,
-2.29798061742311));
#71866=CARTESIAN_POINT('Ctrl Pts',(0.528725587527778,-0.146702874536301,
-2.27413243536486));
#71867=CARTESIAN_POINT('Ctrl Pts',(0.409501451628164,0.365213692813172,
-2.25028425330664));
#71868=CARTESIAN_POINT('Ctrl Pts',(-0.085493265217381,0.541999429802538,
-2.2264360712484));
#71869=CARTESIAN_POINT('Ctrl Pts',(-0.502036846395473,0.22143054252992,
-2.20258788919017));
#71870=CARTESIAN_POINT('Ctrl Pts',(-0.457896645681655,-0.302329525811319,
-2.17873970713193));
#71871=CARTESIAN_POINT('Ctrl Pts',(0.00642298999355273,-0.548663125700416,
-2.1548915250737));
#71872=CARTESIAN_POINT('Ctrl Pts',(0.464848701064361,-0.291527297902928,
-2.13104334301546));
#71873=CARTESIAN_POINT('Ctrl Pts',(0.49671556660139,0.233122556179506,-2.10719516095723));
#71874=CARTESIAN_POINT('Ctrl Pts',(0.0727816131557911,0.54385229344947,
-2.08334697889899));
#71875=CARTESIAN_POINT('Ctrl Pts',(-0.41793889000531,0.355527164257441,
-2.05949879684076));
#71876=CARTESIAN_POINT('Ctrl Pts',(-0.525146370507339,-0.159040151681187,
-2.03565061478253));
#71877=CARTESIAN_POINT('Ctrl Pts',(-0.150464089831247,-0.52766754493247,
-2.01180243272429));
#71878=CARTESIAN_POINT('Ctrl Pts',(0.36228846684164,-0.412091673171567,
-1.98795425066605));
#71879=CARTESIAN_POINT('Ctrl Pts',(0.542594466576044,0.081631643036665,
-1.96410606860782));
#71880=CARTESIAN_POINT('Ctrl Pts',(0.224999818797078,0.500447361712587,
-1.94025788654959));
#71881=CARTESIAN_POINT('Ctrl Pts',(-0.299061282973556,0.460037856409686,
-1.91640970449135));
#71882=CARTESIAN_POINT('Ctrl Pts',(-0.548694952082849,-0.00251592182037977,
-1.89256152243312));
#71883=CARTESIAN_POINT('Ctrl Pts',(-0.2948299886806,-0.462761016161045,
-1.86871334037488));
#71884=CARTESIAN_POINT('Ctrl Pts',(0.229579647240638,-0.49836298606204,
-1.84486515831665));
#71885=CARTESIAN_POINT('Ctrl Pts',(0.543320243836196,-0.0766524164105996,
-1.82101697625841));
#71886=CARTESIAN_POINT('Ctrl Pts',(0.358494198349619,0.415396665915208,
-1.79716879420018));
#71887=CARTESIAN_POINT('Ctrl Pts',(-0.155296671666819,0.526265545207944,
-1.77332061214194));
#71888=CARTESIAN_POINT('Ctrl Pts',(-0.526582746403072,0.15421767568734,
-1.74947243008371));
#71889=CARTESIAN_POINT('Ctrl Pts',(-0.41466099917619,-0.359344870654934,
-1.72562424802547));
#71890=CARTESIAN_POINT('Ctrl Pts',(0.077765881638212,-0.5431619905303,-1.70177606596724));
#71891=CARTESIAN_POINT('Ctrl Pts',(0.498832501323434,-0.228557686213378,
-1.677927883909));
#71892=CARTESIAN_POINT('Ctrl Pts',(0.46215574043763,0.295777875921027,-1.65407970185077));
#71893=CARTESIAN_POINT('Ctrl Pts',(0.00139127392523328,0.548698956314547,
-1.63023151979253));
#71894=CARTESIAN_POINT('Ctrl Pts',(-0.460649866476988,0.298117729795697,
-1.6063833377343));
#71895=CARTESIAN_POINT('Ctrl Pts',(-0.499985135506862,-0.226025097225929,
-1.58253515567606));
#71896=CARTESIAN_POINT('Ctrl Pts',(-0.08051933292456,-0.54276064460238,
-1.55868697361783));
#71897=CARTESIAN_POINT('Ctrl Pts',(0.412833378703222,-0.361443054618967,
-1.5348387915596));
#71898=CARTESIAN_POINT('Ctrl Pts',(0.527358035064316,0.151545317172489,
-1.51099060950136));
#71899=CARTESIAN_POINT('Ctrl Pts',(0.157963441775079,0.525471246945423,
-1.48714242744312));
#71900=CARTESIAN_POINT('Ctrl Pts',(-0.356383053511173,0.417209299361676,
-1.46329424538489));
#71901=CARTESIAN_POINT('Ctrl Pts',(-0.543701972888415,-0.0738961770394953,
-1.43944606332666));
#71902=CARTESIAN_POINT('Ctrl Pts',(-0.232103964373433,-0.497192347111199,
-1.41559788126843));
#71903=CARTESIAN_POINT('Ctrl Pts',(0.292479471142316,-0.464250190375963,
-1.39174969921019));
#71904=CARTESIAN_POINT('Ctrl Pts',(0.548675138192466,-0.00529839912485062,
-1.36790151715196));
#71905=CARTESIAN_POINT('Ctrl Pts',(0.301390354539878,0.458515359060233,
-1.34405333509372));
#71906=CARTESIAN_POINT('Ctrl Pts',(-0.22245908637255,0.501581932683083,
-1.32020515303549));
#71907=CARTESIAN_POINT('Ctrl Pts',(-0.542173524123086,0.084382166621627,
-1.29635697097725));
#71908=CARTESIAN_POINT('Ctrl Pts',(-0.364373583540652,-0.410249158343502,
-1.27250878891902));
#71909=CARTESIAN_POINT('Ctrl Pts',(0.14778627841454,-0.528423784680618,
-1.24866060686078));
#71910=CARTESIAN_POINT('Ctrl Pts',(0.524333102919268,-0.161701198161485,
-1.22481242480255));
#71911=CARTESIAN_POINT('Ctrl Pts',(0.419736444513797,0.35340316559239,-1.20096424274431));
#71912=CARTESIAN_POINT('Ctrl Pts',(-0.0700227254579231,0.544214386270018,
-1.17711606068608));
#71913=CARTESIAN_POINT('Ctrl Pts',(-0.495526982241611,0.235638473459511,
-1.15326787862784));
#71914=CARTESIAN_POINT('Ctrl Pts',(-0.466321100023418,-0.289166235886481,
-1.12941969656961));
#71915=CARTESIAN_POINT('Ctrl Pts',(-0.00920525566360501,-0.548623498924331,
-1.10557151451137));
#71916=CARTESIAN_POINT('Ctrl Pts',(0.456357602143208,-0.304647696971287,
-1.08172333245314));
#71917=CARTESIAN_POINT('Ctrl Pts',(0.503153296623432,0.218881795498803,
-1.05787515039491));
#71918=CARTESIAN_POINT('Ctrl Pts',(0.088240721632787,0.541558912168871,
-1.03402696833667));
#71919=CARTESIAN_POINT('Ctrl Pts',(-0.407644135871638,0.367285636519142,
-1.01017878627844));
#71920=CARTESIAN_POINT('Ctrl Pts',(-0.529462740016906,-0.144019745998958,
-0.986330604220201));
#71921=CARTESIAN_POINT('Ctrl Pts',(-0.16543075531971,-0.523168372035383,
-0.962482422161966));
#71922=CARTESIAN_POINT('Ctrl Pts',(0.35040535799689,-0.422242306491027,
-0.938634240103732));
#71923=CARTESIAN_POINT('Ctrl Pts',(0.544699204692694,0.0661457233009084,
-0.914786058045497));
#71924=CARTESIAN_POINT('Ctrl Pts',(0.239161034250552,0.49383649115874,-0.890937875987262));
#71925=CARTESIAN_POINT('Ctrl Pts',(-0.28583833815443,0.468368364372352,
-0.867089693929028));
#71926=CARTESIAN_POINT('Ctrl Pts',(-0.548544041128856,0.0131116454402537,
-0.843241511870794));
#71927=CARTESIAN_POINT('Ctrl Pts',(-0.307889591922411,-0.454176705137236,
-0.819393329812559));
#71928=CARTESIAN_POINT('Ctrl Pts',(0.215293405993889,-0.504699147650254,
-0.795545147754323));
#71929=CARTESIAN_POINT('Ctrl Pts',(0.540916839906339,-0.092094802305981,
-0.77169696569609));
#71930=CARTESIAN_POINT('Ctrl Pts',(0.370179065891787,0.405018443378037,
-0.747848783637855));
#71931=CARTESIAN_POINT('Ctrl Pts',(-0.140245910904111,0.530474848391832,
-0.724000601579619));
#71932=CARTESIAN_POINT('Ctrl Pts',(-0.521977113367245,0.169151924138721,
-0.700152419521386));
#71933=CARTESIAN_POINT('Ctrl Pts',(-0.424726758203037,-0.347389782731771,
-0.67630423746315));
#71934=CARTESIAN_POINT('Ctrl Pts',(0.0622653671022191,-0.545156403572981,
-0.652456055404916));
#71935=CARTESIAN_POINT('Ctrl Pts',(0.49212095968373,-0.242671468131879,
-0.628607873346681));
#71936=CARTESIAN_POINT('Ctrl Pts',(0.470391879416357,0.282495946691564,
-0.604759691288447));
#71937=CARTESIAN_POINT('Ctrl Pts',(0.0170173707567055,0.548436768833369,
-0.580911509230212));
#71938=CARTESIAN_POINT('Ctrl Pts',(-0.451972779355291,0.311115875012766,
-0.557063327171978));
#71939=CARTESIAN_POINT('Ctrl Pts',(-0.506219405981777,-0.211694099816963,
-0.533215145113743));
#71940=CARTESIAN_POINT('Ctrl Pts',(-0.0959442158986505,-0.540247339880686,
-0.509366963055509));
#71941=CARTESIAN_POINT('Ctrl Pts',(0.402372219149679,-0.373053724966781,
-0.485518780997274));
#71942=CARTESIAN_POINT('Ctrl Pts',(0.531460048604374,0.136464964529532,
-0.461670598939039));
#71943=CARTESIAN_POINT('Ctrl Pts',(0.17286453489641,0.520759387235809,-0.437822416880805));
#71944=CARTESIAN_POINT('Ctrl Pts',(-0.344356629099969,0.42718967383251,
-0.41397423482257));
#71945=CARTESIAN_POINT('Ctrl Pts',(-0.545585889878679,-0.0583818539252621,
-0.390126052764335));
#71946=CARTESIAN_POINT('Ctrl Pts',(-0.24616973115849,-0.490380474217275,
-0.366277870706102));
#71947=CARTESIAN_POINT('Ctrl Pts',(0.279139488256261,-0.472391543677784,
-0.342429688647865));
#71948=CARTESIAN_POINT('Ctrl Pts',(0.548301193707043,-0.020922231406565,
-0.318581506589632));
#71949=CARTESIAN_POINT('Ctrl Pts',(0.314327330294862,0.449745932399401,
-0.294733324531397));
#71950=CARTESIAN_POINT('Ctrl Pts',(-0.208085878195641,0.507714002497032,
-0.270885142473163));
#71951=CARTESIAN_POINT('Ctrl Pts',(-0.539546955546815,0.0997887519352769,
-0.247036960414928));
#71952=CARTESIAN_POINT('Ctrl Pts',(-0.375916166944726,-0.399705568027995,
-0.223188778356693));
#71953=CARTESIAN_POINT('Ctrl Pts',(0.132689955287081,-0.532418346998393,
-0.199340596298459));
#71954=CARTESIAN_POINT('Ctrl Pts',(0.519490580485835,-0.176568291348837,
-0.175492414240224));
#71955=CARTESIAN_POINT('Ctrl Pts',(0.42967828745962,0.341305844172893,-0.151644232181989));
#71956=CARTESIAN_POINT('Ctrl Pts',(-0.0545862982692795,0.545988033714885,
-0.127796050123755));
#71957=CARTESIAN_POINT('Ctrl Pts',(-0.488440393699185,0.249654938517161,
-0.10394786806552));
#71958=CARTESIAN_POINT('Ctrl Pts',(-0.474704799369555,-0.275768185196691,
-0.0800996860072854));
#71959=CARTESIAN_POINT('Ctrl Pts',(-0.0241580178204238,-0.548135368621999,
-0.056251503949051));
#71960=CARTESIAN_POINT('Ctrl Pts',(0.367665957515721,-0.355993096721218,
-0.036378018900522));
#71961=CARTESIAN_POINT('Ctrl Pts',(0.479687750828799,-0.0561079110677501,
-0.0204792308616991));
#71962=CARTESIAN_POINT('Ctrl Pts',(0.459385470135524,0.101216507378395,
-0.0125298368422873));
#71963=CARTESIAN_POINT('Ctrl Pts',(0.430597807144122,0.172907476492828,
-0.00855513983258168));
#71964=CARTESIAN_POINT('Ctrl Pts',(0.25276100881156,-0.354684587865059,
-3.47394486016742));
#71965=CARTESIAN_POINT('Ctrl Pts',(0.311813055552452,-0.312601973008691,
-3.46997016315771));
#71966=CARTESIAN_POINT('Ctrl Pts',(0.407519065220516,-0.198544594037436,
-3.4620207691383));
#71967=CARTESIAN_POINT('Ctrl Pts',(0.470831200545202,0.0951838576604093,
-3.44612198109948));
#71968=CARTESIAN_POINT('Ctrl Pts',(0.258453570668323,0.445437196485978,
-3.42624849605095));
#71969=CARTESIAN_POINT('Ctrl Pts',(-0.235536724315465,0.458311345096049,
-3.40240031399271));
#71970=CARTESIAN_POINT('Ctrl Pts',(-0.512438291264498,0.0500114804658197,
-3.37855213193448));
#71971=CARTESIAN_POINT('Ctrl Pts',(-0.319599847496316,-0.403868221641854,
-3.35470394987625));
#71972=CARTESIAN_POINT('Ctrl Pts',(0.166766420531462,-0.487308368434241,
-3.33085576781801));
#71973=CARTESIAN_POINT('Ctrl Pts',(0.499970874131756,-0.123495800363189,
-3.30700758575978));
#71974=CARTESIAN_POINT('Ctrl Pts',(0.374456131546814,0.353596276221467,
-3.28315940370154));
#71975=CARTESIAN_POINT('Ctrl Pts',(-0.0947064163426174,0.506240863917161,
-3.25931122164331));
#71976=CARTESIAN_POINT('Ctrl Pts',(-0.476944895070687,0.194332029410326,
-3.23546303958507));
#71977=CARTESIAN_POINT('Ctrl Pts',(-0.421534435296339,-0.295895387432433,
-3.21161485752684));
#71978=CARTESIAN_POINT('Ctrl Pts',(0.0206934953975774,-0.514603724025353,
-3.1877666754686));
#71979=CARTESIAN_POINT('Ctrl Pts',(0.443929824061649,-0.261094857231714,
-3.16391849341037));
#71980=CARTESIAN_POINT('Ctrl Pts',(0.459804460733734,0.232001454984632,
-3.14007031135213));
#71981=CARTESIAN_POINT('Ctrl Pts',(0.0537482779932776,0.512206863248803,
-3.1162221292939));
#71982=CARTESIAN_POINT('Ctrl Pts',(-0.401628532381758,0.322395944582544,
-3.09237394723566));
#71983=CARTESIAN_POINT('Ctrl Pts',(-0.488459378881163,-0.163254854637313,
-3.06852576517743));
#71984=CARTESIAN_POINT('Ctrl Pts',(-0.127065425715578,-0.499098260433244,
-3.04467758311919));
#71985=CARTESIAN_POINT('Ctrl Pts',(0.350927447920041,-0.376954383563904,
-3.02082940106096));
#71986=CARTESIAN_POINT('Ctrl Pts',(0.506898997405238,0.0910939093821704,
-2.99698121900272));
#71987=CARTESIAN_POINT('Ctrl Pts',(0.197725097818228,0.475551759938628,
-2.97313303694449));
#71988=CARTESIAN_POINT('Ctrl Pts',(-0.29288716179633,0.423629318448265,
-2.94928485488626));
#71989=CARTESIAN_POINT('Ctrl Pts',(-0.514737547902153,-0.0170278477871493,
-2.92543667282802));
#71990=CARTESIAN_POINT('Ctrl Pts',(-0.264249612685154,-0.442059761170484,
-2.90158849076979));
#71991=CARTESIAN_POINT('Ctrl Pts',(0.228721541200349,-0.461444630120445,
-2.87774030871155));
#71992=CARTESIAN_POINT('Ctrl Pts',(0.511811079662378,-0.0573943295457097,
-2.85389212665332));
#71993=CARTESIAN_POINT('Ctrl Pts',(0.325247711908225,0.399322696740629,
-2.83004394459509));
#71994=CARTESIAN_POINT('Ctrl Pts',(-0.159772526042282,0.489609466964142,
-2.80619576253684));
#71995=CARTESIAN_POINT('Ctrl Pts',(-0.498180793120726,0.130616184367629,
-2.78234758047862));
#71996=CARTESIAN_POINT('Ctrl Pts',(-0.379443706209799,-0.348234352204978,
-2.75849939842038));
#71997=CARTESIAN_POINT('Ctrl Pts',(0.0874820900284247,-0.507534800936275,
-2.73465121636214));
#71998=CARTESIAN_POINT('Ctrl Pts',(0.474131746445591,-0.201106382927444,
-2.71080303430391));
#71999=CARTESIAN_POINT('Ctrl Pts',(0.425704161742498,0.289863169296219,
-2.68695485224568));
#72000=CARTESIAN_POINT('Ctrl Pts',(-0.0133620874435406,0.51484574860689,
-2.66310667018744));
#72001=CARTESIAN_POINT('Ctrl Pts',(-0.440166892034677,0.267390720475778,
-2.63925848812921));
#72002=CARTESIAN_POINT('Ctrl Pts',(-0.463061605280014,-0.225429900313069,
-2.61541030607097));
#72003=CARTESIAN_POINT('Ctrl Pts',(-0.0610373646661749,-0.511389411656436,
-2.59156212401274));
#72004=CARTESIAN_POINT('Ctrl Pts',(0.396996557693393,-0.328082952040145,
-2.5677139419545));
#72005=CARTESIAN_POINT('Ctrl Pts',(0.490734757718168,0.156282077689729,
-2.54386575989627));
#72006=CARTESIAN_POINT('Ctrl Pts',(0.13416030496745,0.497238074578745,-2.52001757783803));
#72007=CARTESIAN_POINT('Ctrl Pts',(-0.345523591076013,0.381913783791161,
-2.4961693957798));
#72008=CARTESIAN_POINT('Ctrl Pts',(-0.508144873463445,-0.0838658322116802,
-2.47232121372156));
#72009=CARTESIAN_POINT('Ctrl Pts',(-0.204477468602375,-0.472687692957734,
-2.44847303166333));
#72010=CARTESIAN_POINT('Ctrl Pts',(0.286824477874043,-0.427757418558724,
-2.4246248496051));
#72011=CARTESIAN_POINT('Ctrl Pts',(0.514927844097049,0.00969564919462744,
-2.40077666754686));
#72012=CARTESIAN_POINT('Ctrl Pts',(0.270518269639977,0.43825170396786,-2.37692848548863));
#72013=CARTESIAN_POINT('Ctrl Pts',(-0.222126828610562,0.464655100317595,
-2.35308030343039));
#72014=CARTESIAN_POINT('Ctrl Pts',(-0.510941813197769,0.0646773048751767,
-2.32923212137215));
#72015=CARTESIAN_POINT('Ctrl Pts',(-0.330901556340725,-0.394650288548008,
-2.30538393931392));
#72016=CARTESIAN_POINT('Ctrl Pts',(0.15278370486901,-0.491835165239574,
-2.28153575725568));
#72017=CARTESIAN_POINT('Ctrl Pts',(0.4962701430723,-0.137697622836198,-2.25768757519746));
#72018=CARTESIAN_POINT('Ctrl Pts',(0.384364496029135,0.342795309816236,
-2.23383939313921));
#72019=CARTESIAN_POINT('Ctrl Pts',(-0.0802453218871671,0.508729179971981,
-2.20999121108098));
#72020=CARTESIAN_POINT('Ctrl Pts',(-0.471219671348245,0.207838186034692,
-2.18614302902275));
#72021=CARTESIAN_POINT('Ctrl Pts',(-0.429788985487338,-0.283771242717626,
-2.16229484696452));
#72022=CARTESIAN_POINT('Ctrl Pts',(0.0060287193172493,-0.514983829632674,
-2.13844666490628));
#72023=CARTESIAN_POINT('Ctrl Pts',(0.436314293890805,-0.273632101892866,
-2.11459848284804));
#72024=CARTESIAN_POINT('Ctrl Pts',(0.466225034532793,0.218812493735242,
-2.09075030078981));
#72025=CARTESIAN_POINT('Ctrl Pts',(0.0683139655539354,0.510468306900671,
-2.06690211873158));
#72026=CARTESIAN_POINT('Ctrl Pts',(-0.392284008247505,0.333703381932237,
-2.04305393667334));
#72027=CARTESIAN_POINT('Ctrl Pts',(-0.492910633745116,-0.149277584990941,
-2.01920575461511));
#72028=CARTESIAN_POINT('Ctrl Pts',(-0.141227958603144,-0.495277047669815,
-1.99535757255687));
#72029=CARTESIAN_POINT('Ctrl Pts',(0.340049646762177,-0.386795718663819,
-1.97150939049864));
#72030=CARTESIAN_POINT('Ctrl Pts',(0.509287690836003,0.0766207426397812,
-1.9476612084404));
#72031=CARTESIAN_POINT('Ctrl Pts',(0.211188364814669,0.469727756053063,
-1.92381302638217));
#72032=CARTESIAN_POINT('Ctrl Pts',(-0.280703618643906,0.431798759516465,
-1.89996484432393));
#72033=CARTESIAN_POINT('Ctrl Pts',(-0.515013702375239,-0.00236148374735782,
-1.8761166622657));
#72034=CARTESIAN_POINT('Ctrl Pts',(-0.276732059344184,-0.434354760041681,
-1.85226848020746));
#72035=CARTESIAN_POINT('Ctrl Pts',(0.215487063743844,-0.467771328320578,
-1.82842029814923));
#72036=CARTESIAN_POINT('Ctrl Pts',(0.50996891677481,-0.071947162301705,
-1.80457211609099));
#72037=CARTESIAN_POINT('Ctrl Pts',(0.336488286745168,0.389897836776561,
-1.78072393403276));
#72038=CARTESIAN_POINT('Ctrl Pts',(-0.145763895836979,0.493961108702058,
-1.75687575197452));
#72039=CARTESIAN_POINT('Ctrl Pts',(-0.49425883872724,0.144751133258919,
-1.73302756991629));
#72040=CARTESIAN_POINT('Ctrl Pts',(-0.38920732841752,-0.337286741135547,
-1.70917938785805));
#72041=CARTESIAN_POINT('Ctrl Pts',(0.0729922782575974,-0.509820377735635,
-1.68533120579982));
#72042=CARTESIAN_POINT('Ctrl Pts',(0.46821202272131,-0.214527835067992,
-1.66148302374158));
#72043=CARTESIAN_POINT('Ctrl Pts',(0.433786638738412,0.277621761199967,
-1.63763484168335));
#72044=CARTESIAN_POINT('Ctrl Pts',(0.00130587156403045,0.515017460810019,
-1.61378665962512));
#72045=CARTESIAN_POINT('Ctrl Pts',(-0.432373201780706,0.279817984807339,
-1.58993847756689));
#72046=CARTESIAN_POINT('Ctrl Pts',(-0.469293903274499,-0.212150707255774,
-1.56609029550865));
#72047=CARTESIAN_POINT('Ctrl Pts',(-0.0755767108934513,-0.509443668142287,
-1.54224211345042));
#72048=CARTESIAN_POINT('Ctrl Pts',(0.387491895128502,-0.339256129568005,
-1.51839393139218));
#72049=CARTESIAN_POINT('Ctrl Pts',(0.494986536844966,0.142242815572411,
-1.49454574933395));
#72050=CARTESIAN_POINT('Ctrl Pts',(0.148266968157262,0.49321556787392,-1.47069756727571));
#72051=CARTESIAN_POINT('Ctrl Pts',(-0.334506733032362,0.39159920300705,
-1.44684938521747));
#72052=CARTESIAN_POINT('Ctrl Pts',(-0.510327213660431,-0.069360112725696,
-1.42300120315924));
#72053=CARTESIAN_POINT('Ctrl Pts',(-0.217856427463329,-0.466672548209829,
-1.39915302110101));
#72054=CARTESIAN_POINT('Ctrl Pts',(0.274525826654611,-0.435752522355686,
-1.37530483904277));
#72055=CARTESIAN_POINT('Ctrl Pts',(0.514995104746436,-0.004973160659839,
-1.35145665698454));
#72056=CARTESIAN_POINT('Ctrl Pts',(0.282889721807265,0.430369719584858,
-1.3276084749263));
#72057=CARTESIAN_POINT('Ctrl Pts',(-0.208803593444471,0.470792682190809,
-1.30376029286807));
#72058=CARTESIAN_POINT('Ctrl Pts',(-0.508892587636381,0.0792024272891182,
-1.27991211080983));
#72059=CARTESIAN_POINT('Ctrl Pts',(-0.342006770054391,-0.385066305299106,
-1.2560639287516));
#72060=CARTESIAN_POINT('Ctrl Pts',(0.138714522737286,-0.495986866178438,
-1.23221574669336));
#72061=CARTESIAN_POINT('Ctrl Pts',(0.492147288009996,-0.151775285024098,
-1.20836756463513));
#72062=CARTESIAN_POINT('Ctrl Pts',(0.393971221149906,0.331709763415838,
-1.18451938257689));
#72063=CARTESIAN_POINT('Ctrl Pts',(-0.0657244302168194,0.510808172910747,
-1.16067120051866));
#72064=CARTESIAN_POINT('Ctrl Pts',(-0.465109410579282,0.22117397322093,
-1.13682301846043));
#72065=CARTESIAN_POINT('Ctrl Pts',(-0.437696310686108,-0.271415971990429,
-1.11297483640219));
#72066=CARTESIAN_POINT('Ctrl Pts',(-0.00864019758634064,-0.514946635318078,
-1.08912665434395));
#72067=CARTESIAN_POINT('Ctrl Pts',(0.42834441504279,-0.285947114588328,
-1.06527847228572));
#72068=CARTESIAN_POINT('Ctrl Pts',(0.472267589072358,0.205445892028833,
-1.04143029022749));
#72069=CARTESIAN_POINT('Ctrl Pts',(0.0828241276429715,0.508315703200206,
-1.01758210816925));
#72070=CARTESIAN_POINT('Ctrl Pts',(-0.382621190280438,0.344740068730225,
-0.993733926111018));
#72071=CARTESIAN_POINT('Ctrl Pts',(-0.496962045979734,-0.135179196237376,
-0.969885744052783));
#72072=CARTESIAN_POINT('Ctrl Pts',(-0.155275905966547,-0.491054053303712,
-0.946037561994549));
#72073=CARTESIAN_POINT('Ctrl Pts',(0.328895974109219,-0.396323262570435,
-0.922189379936314));
#72074=CARTESIAN_POINT('Ctrl Pts',(0.511263231099079,0.06208541508205,-0.89834119787808));
#72075=CARTESIAN_POINT('Ctrl Pts',(0.224480304121095,0.463522689090198,
-0.874493015819844));
#72076=CARTESIAN_POINT('Ctrl Pts',(-0.268292354895715,0.439617905167857,
-0.850644833761611));
#72077=CARTESIAN_POINT('Ctrl Pts',(-0.514872054982912,0.0123067964025964,
-0.826796651703375));
#72078=CARTESIAN_POINT('Ctrl Pts',(-0.288990008121707,-0.426297390849691,
-0.802948469645141));
#72079=CARTESIAN_POINT('Ctrl Pts',(0.202077773263616,-0.473718549132447,
-0.779100287586905));
#72080=CARTESIAN_POINT('Ctrl Pts',(0.507713044087226,-0.0864416283129147,
-0.755252105528672));
#72081=CARTESIAN_POINT('Ctrl Pts',(0.347455886997024,0.380156674054626,
-0.731403923470436));
#72082=CARTESIAN_POINT('Ctrl Pts',(-0.131637015327978,0.497912026801313,
-0.707555741412202));
#72083=CARTESIAN_POINT('Ctrl Pts',(-0.489935919202359,0.158768653482024,
-0.683707559353968));
#72084=CARTESIAN_POINT('Ctrl Pts',(-0.398655207979661,-0.326065507788752,
-0.659859377295733));
#72085=CARTESIAN_POINT('Ctrl Pts',(0.058443251791071,-0.511692365151006,
-0.636011195237498));
#72086=CARTESIAN_POINT('Ctrl Pts',(0.461912464295652,-0.227775252513281,
-0.612163013179264));
#72087=CARTESIAN_POINT('Ctrl Pts',(0.441517208178881,0.265155133757551,
-0.588314831121029));
#72088=CARTESIAN_POINT('Ctrl Pts',(0.0159727715460726,0.514771367521052,
-0.564466649062794));
#72089=CARTESIAN_POINT('Ctrl Pts',(-0.424228751485667,0.292018248117294,
-0.54061846700456));
#72090=CARTESIAN_POINT('Ctrl Pts',(-0.475145487486649,-0.19869940793854,
-0.516770284946325));
#72091=CARTESIAN_POINT('Ctrl Pts',(-0.0900547483877555,-0.507084640844872,
-0.492922102888091));
#72092=CARTESIAN_POINT('Ctrl Pts',(0.377672886420007,-0.350154087167556,
-0.469073920829856));
#72093=CARTESIAN_POINT('Ctrl Pts',(0.498836751198934,0.128088159659702,
-0.445225738771621));
#72094=CARTESIAN_POINT('Ctrl Pts',(0.162253368266692,0.488792942324132,
-0.421377556713388));
#72095=CARTESIAN_POINT('Ctrl Pts',(-0.323218542137151,0.400966939283472,
-0.397529374655152));
#72096=CARTESIAN_POINT('Ctrl Pts',(-0.512095487745039,-0.0547981253106918,
-0.373681192596918));
#72097=CARTESIAN_POINT('Ctrl Pts',(-0.231058777150018,-0.460278817292692,
-0.349833010538684));
#72098=CARTESIAN_POINT('Ctrl Pts',(0.262004709138057,-0.443394124470668,
-0.325984828480448));
#72099=CARTESIAN_POINT('Ctrl Pts',(0.51464411457751,-0.0196379350999004,
-0.302136646422214));
#72100=CARTESIAN_POINT('Ctrl Pts',(0.295032570499096,0.422138597947673,
-0.278288464363979));
#72101=CARTESIAN_POINT('Ctrl Pts',(-0.195312674437287,0.476548339256938,
-0.254440282305745));
#72102=CARTESIAN_POINT('Ctrl Pts',(-0.506427249105613,0.0936632903118652,
-0.23059210024751));
#72103=CARTESIAN_POINT('Ctrl Pts',(-0.352840820178858,-0.375169925782392,
-0.206743918189276));
#72104=CARTESIAN_POINT('Ctrl Pts',(0.124544876676916,-0.499736225127042,
-0.182895736131041));
#72105=CARTESIAN_POINT('Ctrl Pts',(0.487602020374838,-0.165729772261334,
-0.159047554072806));
#72106=CARTESIAN_POINT('Ctrl Pts',(0.403302791131596,0.320355027474805,
-0.135199372014571));
#72107=CARTESIAN_POINT('Ctrl Pts',(-0.0512355571413682,0.512472946267641,
-0.111351189956337));
#72108=CARTESIAN_POINT('Ctrl Pts',(-0.458457827238502,0.234330047531713,
-0.0875030078981023));
#72109=CARTESIAN_POINT('Ctrl Pts',(-0.445565382605697,-0.258840351121007,
-0.0636548258398675));
#72110=CARTESIAN_POINT('Ctrl Pts',(-0.0226750950642322,-0.514488468547469,
-0.0398066437816332));
#72111=CARTESIAN_POINT('Ctrl Pts',(0.345097043992702,-0.334140713462838,
-0.0199331587331043));
#72112=CARTESIAN_POINT('Ctrl Pts',(0.450242459130713,-0.0526637668195261,
-0.00403437069428129));
#72113=CARTESIAN_POINT('Ctrl Pts',(0.43118641951013,0.0950034040017324,
0.00391502332513044));
#72114=CARTESIAN_POINT('Ctrl Pts',(0.404165866753715,0.162293673923731,
0.00788972033483611));
#72115=CARTESIAN_POINT('Ctrl Pts',(0.236230756092329,-0.331488661006748,
-3.4575));
#72116=CARTESIAN_POINT('Ctrl Pts',(0.291420873096492,-0.292158196341315,
-3.45352530299029));
#72117=CARTESIAN_POINT('Ctrl Pts',(0.380867829859202,-0.185560026793827,
-3.44557590897088));
#72118=CARTESIAN_POINT('Ctrl Pts',(0.440039431000898,0.0889589528409691,
-3.42967712093207));
#72119=CARTESIAN_POINT('Ctrl Pts',(0.241551031548769,0.416306162933455,
-3.40980363588352));
#72120=CARTESIAN_POINT('Ctrl Pts',(-0.22013291818294,0.428338358383622,
-3.3859554538253));
#72121=CARTESIAN_POINT('Ctrl Pts',(-0.478925470210962,0.0467407924160679,
-3.36210727176706));
#72122=CARTESIAN_POINT('Ctrl Pts',(-0.298698418620944,-0.377455746868169,
-3.33825908970883));
#72123=CARTESIAN_POINT('Ctrl Pts',(0.155860105948259,-0.455439012791576,
-3.31441090765059));
#72124=CARTESIAN_POINT('Ctrl Pts',(0.467273406510021,-0.115419330027175,
-3.29056272559236));
#72125=CARTESIAN_POINT('Ctrl Pts',(0.349967170548287,0.330471523578635,
-3.26671454353412));
#72126=CARTESIAN_POINT('Ctrl Pts',(-0.0885127355860925,0.473133346833339,
-3.24286636147589));
#72127=CARTESIAN_POINT('Ctrl Pts',(-0.445753297578119,0.181622958605862,
-3.21901817941765));
#72128=CARTESIAN_POINT('Ctrl Pts',(-0.393966612323683,-0.276544200492206,
-3.19516999735943));
#72129=CARTESIAN_POINT('Ctrl Pts',(0.0193401667723502,-0.480949286387233,
-3.17132181530118));
#72130=CARTESIAN_POINT('Ctrl Pts',(0.414897370773675,-0.244019581286168,
-3.14747363324295));
#72131=CARTESIAN_POINT('Ctrl Pts',(0.429733826132711,0.216828851028994,
-3.12362545118471));
#72132=CARTESIAN_POINT('Ctrl Pts',(0.0502332080755313,0.478709177297012,
-3.09977726912648));
#72133=CARTESIAN_POINT('Ctrl Pts',(-0.375362530474502,0.301311654467299,
-3.07592908706825));
#72134=CARTESIAN_POINT('Ctrl Pts',(-0.456514748599978,-0.15257819205599,
-3.05208090501001));
#72135=CARTESIAN_POINT('Ctrl Pts',(-0.118755506361991,-0.466457860652117,
-3.02823272295178));
#72136=CARTESIAN_POINT('Ctrl Pts',(0.3279772332983,-0.35230204001918,-3.00438454089354));
#72137=CARTESIAN_POINT('Ctrl Pts',(0.473748439217363,0.0851364820465625,
-2.9805363588353));
#72138=CARTESIAN_POINT('Ctrl Pts',(0.184794124598751,0.44445127173508,-2.95668817677707));
#72139=CARTESIAN_POINT('Ctrl Pts',(-0.273732709036882,0.395924492746899,
-2.93283999471884));
#72140=CARTESIAN_POINT('Ctrl Pts',(-0.481074358350462,-0.0159142479146477,
-2.9089918126606));
#72141=CARTESIAN_POINT('Ctrl Pts',(-0.246968019692694,-0.413149607648352,
-2.88514363060237));
#72142=CARTESIAN_POINT('Ctrl Pts',(0.213763439489368,-0.431266730500215,
-2.86129544854413));
#72143=CARTESIAN_POINT('Ctrl Pts',(0.478339277460365,-0.053640812432835,
-2.8374472664859));
#72144=CARTESIAN_POINT('Ctrl Pts',(0.303976919789322,0.373207493590096,
-2.81359908442767));
#72145=CARTESIAN_POINT('Ctrl Pts',(-0.149323603380172,0.457589622365882,
-2.78975090236943));
#72146=CARTESIAN_POINT('Ctrl Pts',(-0.465600394550264,0.122074049854989,
-2.7659027203112));
#72147=CARTESIAN_POINT('Ctrl Pts',(-0.354628564088546,-0.32546026266272,
-2.74205453825296));
#72148=CARTESIAN_POINT('Ctrl Pts',(0.0817608711451184,-0.474342661995509,
-2.71820635619473));
#72149=CARTESIAN_POINT('Ctrl Pts',(0.443124125342135,-0.187954277905899,
-2.69435817413649));
#72150=CARTESIAN_POINT('Ctrl Pts',(0.397863643893962,0.270906481850664,
-2.67050999207826));
#72151=CARTESIAN_POINT('Ctrl Pts',(-0.0124882236963727,0.481175482864919,
-2.64666181002002));
#72152=CARTESIAN_POINT('Ctrl Pts',(-0.411380529778162,0.249903702976424,
-2.62281362796179));
#72153=CARTESIAN_POINT('Ctrl Pts',(-0.432777957513921,-0.210687067784559,
-2.59896544590356));
#72154=CARTESIAN_POINT('Ctrl Pts',(-0.0570455976290363,-0.477945186012748,
-2.57511726384532));
#72155=CARTESIAN_POINT('Ctrl Pts',(0.371033481116859,-0.306626738775311,
-2.55126908178708));
#72156=CARTESIAN_POINT('Ctrl Pts',(0.458641320517021,0.146061425968784,
-2.52742089972885));
#72157=CARTESIAN_POINT('Ctrl Pts',(0.125386389416043,0.46471932861766,-2.50357271767061));
#72158=CARTESIAN_POINT('Ctrl Pts',(-0.322926781909134,0.356937101696446,
-2.47972453561238));
#72159=CARTESIAN_POINT('Ctrl Pts',(-0.474912836545144,-0.078381112050585,
-2.45587635355414));
#72160=CARTESIAN_POINT('Ctrl Pts',(-0.191104898808961,-0.441774511139857,
-2.43202817149591));
#72161=CARTESIAN_POINT('Ctrl Pts',(0.268066517033437,-0.399782620291585,
-2.40817998943768));
#72162=CARTESIAN_POINT('Ctrl Pts',(0.481252209413066,0.00906156590694945,
-2.38433180737944));
#72163=CARTESIAN_POINT('Ctrl Pts',(0.252826714350878,0.409590592607036,
-2.36048362532121));
#72164=CARTESIAN_POINT('Ctrl Pts',(-0.207600012825493,0.434267239976145,
-2.33663544326297));
#72165=CARTESIAN_POINT('Ctrl Pts',(-0.477526859931467,0.0604474903170984,
-2.31278726120474));
#72166=CARTESIAN_POINT('Ctrl Pts',(-0.309261009892451,-0.368840655028625,
-2.2889390791465));
#72167=CARTESIAN_POINT('Ctrl Pts',(0.142791842339502,-0.459669762767722,
-2.26509089708827));
#72168=CARTESIAN_POINT('Ctrl Pts',(0.463814698616821,-0.128692371136095,
-2.24124271503003));
#72169=CARTESIAN_POINT('Ctrl Pts',(0.359227540430107,0.3203769268193,-2.2173945329718));
#72170=CARTESIAN_POINT('Ctrl Pts',(-0.0749973785569536,0.475458930141424,
-2.19354635091357));
#72171=CARTESIAN_POINT('Ctrl Pts',(-0.440402496301018,0.194245829539463,
-2.16969816885533));
#72172=CARTESIAN_POINT('Ctrl Pts',(-0.401681325293022,-0.265212959623932,
-2.1458499867971));
#72173=CARTESIAN_POINT('Ctrl Pts',(0.00563444864094621,-0.481304533564932,
-2.12200180473886));
#72174=CARTESIAN_POINT('Ctrl Pts',(0.407779886717249,-0.255736905882805,
-2.09815362268063));
#72175=CARTESIAN_POINT('Ctrl Pts',(0.435734502464197,0.204502431290978,
-2.07430544062239));
#72176=CARTESIAN_POINT('Ctrl Pts',(0.0638463179520797,0.47708432035187,
-2.05045725856416));
#72177=CARTESIAN_POINT('Ctrl Pts',(-0.366629126489699,0.311879599607034,
-2.02660907650592));
#72178=CARTESIAN_POINT('Ctrl Pts',(-0.460674896982894,-0.139515018300695,
-2.00276089444769));
#72179=CARTESIAN_POINT('Ctrl Pts',(-0.131991827375041,-0.46288655040716,
-1.97891271238946));
#72180=CARTESIAN_POINT('Ctrl Pts',(0.317810826682713,-0.361499764156071,
-1.95506453033122));
#72181=CARTESIAN_POINT('Ctrl Pts',(0.475980915095963,0.0716098422428978,
-1.93121634827299));
#72182=CARTESIAN_POINT('Ctrl Pts',(0.197376910832261,0.439008150393539,
-1.90736816621475));
#72183=CARTESIAN_POINT('Ctrl Pts',(-0.262345954314256,0.403559662623244,
-1.88351998415652));
#72184=CARTESIAN_POINT('Ctrl Pts',(-0.481332452667628,-0.00220704567433563,
-1.85967180209828));
#72185=CARTESIAN_POINT('Ctrl Pts',(-0.258634130007767,-0.405948503922317,
-1.83582362004005));
#72186=CARTESIAN_POINT('Ctrl Pts',(0.20139448024705,-0.437179670579116,
-1.81197543798181));
#72187=CARTESIAN_POINT('Ctrl Pts',(0.476617589713424,-0.0672419081928105,
-1.78812725592358));
#72188=CARTESIAN_POINT('Ctrl Pts',(0.314482375140717,0.364399007637914,
-1.76427907386534));
#72189=CARTESIAN_POINT('Ctrl Pts',(-0.136231120007138,0.461656672196172,
-1.74043089180711));
#72190=CARTESIAN_POINT('Ctrl Pts',(-0.461934931051408,0.135284590830497,
-1.71658270974887));
#72191=CARTESIAN_POINT('Ctrl Pts',(-0.363753657658851,-0.31522861161616,
-1.69273452769064));
#72192=CARTESIAN_POINT('Ctrl Pts',(0.0682186748769831,-0.476478764940969,
-1.6688863456324));
#72193=CARTESIAN_POINT('Ctrl Pts',(0.437591544119186,-0.200497983922606,
-1.64503816357417));
#72194=CARTESIAN_POINT('Ctrl Pts',(0.405417537039194,0.259465646478908,
-1.62118998151593));
#72195=CARTESIAN_POINT('Ctrl Pts',(0.00122046920282805,0.481335965305491,
-1.5973417994577));
#72196=CARTESIAN_POINT('Ctrl Pts',(-0.404096537084426,0.261518239818982,
-1.57349361739947));
#72197=CARTESIAN_POINT('Ctrl Pts',(-0.438602671042135,-0.198276317285618,
-1.54964543534123));
#72198=CARTESIAN_POINT('Ctrl Pts',(-0.0706340888623429,-0.476126691682194,
-1.525797253283));
#72199=CARTESIAN_POINT('Ctrl Pts',(0.362150411553781,-0.317069204517043,
-1.50194907122476));
#72200=CARTESIAN_POINT('Ctrl Pts',(0.462615038625616,0.132940313972334,
-1.47810088916653));
#72201=CARTESIAN_POINT('Ctrl Pts',(0.138570494539446,0.460959888802416,
-1.45425270710829));
#72202=CARTESIAN_POINT('Ctrl Pts',(-0.312630412553551,0.365989106652426,
-1.43040452505006));
#72203=CARTESIAN_POINT('Ctrl Pts',(-0.476952454432448,-0.0648240484118974,
-1.40655634299182));
#72204=CARTESIAN_POINT('Ctrl Pts',(-0.203608890553224,-0.43615274930846,
-1.38270816093359));
#72205=CARTESIAN_POINT('Ctrl Pts',(0.256572182166905,-0.407254854335409,
-1.35885997887535));
#72206=CARTESIAN_POINT('Ctrl Pts',(0.481315071300406,-0.00464792219482722,
-1.33501179681712));
#72207=CARTESIAN_POINT('Ctrl Pts',(0.264389089074653,0.402224080109482,
-1.31116361475888));
#72208=CARTESIAN_POINT('Ctrl Pts',(-0.195148100516391,0.440003431698535,
-1.28731543270065));
#72209=CARTESIAN_POINT('Ctrl Pts',(-0.475611651149676,0.0740226879566094,
-1.26346725064241));
#72210=CARTESIAN_POINT('Ctrl Pts',(-0.31963995656813,-0.35988345225471,
-1.23961906858418));
#72211=CARTESIAN_POINT('Ctrl Pts',(0.129642767060033,-0.463549947676258,
-1.21577088652594));
#72212=CARTESIAN_POINT('Ctrl Pts',(0.459961473100724,-0.141849371886711,
-1.19192270446771));
#72213=CARTESIAN_POINT('Ctrl Pts',(0.368205997786016,0.310016361239286,
-1.16807452240948));
#72214=CARTESIAN_POINT('Ctrl Pts',(-0.0614261349757158,0.477401959551476,
-1.14422634035124));
#72215=CARTESIAN_POINT('Ctrl Pts',(-0.434691838916953,0.206709472982349,
-1.12037815829301));
#72216=CARTESIAN_POINT('Ctrl Pts',(-0.409071521348799,-0.253665708094378,
-1.09652997623477));
#72217=CARTESIAN_POINT('Ctrl Pts',(-0.0080751395090761,-0.481269771711826,
-1.07268179417654));
#72218=CARTESIAN_POINT('Ctrl Pts',(0.400331227942373,-0.26724653220537,
-1.0488336121183));
#72219=CARTESIAN_POINT('Ctrl Pts',(0.441381881521284,0.192009988558863,
-1.02498543006007));
#72220=CARTESIAN_POINT('Ctrl Pts',(0.0774075336531558,0.475072494231541,
-1.00113724800183));
#72221=CARTESIAN_POINT('Ctrl Pts',(-0.357598244689237,0.322194500941308,
-0.9772890659436));
#72222=CARTESIAN_POINT('Ctrl Pts',(-0.464461351942563,-0.126338646475794,
-0.953440883885366));
#72223=CARTESIAN_POINT('Ctrl Pts',(-0.145121056613384,-0.458939734572041,
-0.92959270182713));
#72224=CARTESIAN_POINT('Ctrl Pts',(0.307386590221547,-0.370404218649844,
-0.905744519768897));
#72225=CARTESIAN_POINT('Ctrl Pts',(0.477827257505465,0.0580251068631922,
-0.88189633771066));
#72226=CARTESIAN_POINT('Ctrl Pts',(0.209799573991638,0.433208887021656,
-0.858048155652426));
#72227=CARTESIAN_POINT('Ctrl Pts',(-0.250746371636999,0.410867445963362,
-0.834199973594193));
#72228=CARTESIAN_POINT('Ctrl Pts',(-0.481200068836968,0.0115019473649387,
-0.810351791535957));
#72229=CARTESIAN_POINT('Ctrl Pts',(-0.270090424321002,-0.398418076562146,
-0.786503609477724));
#72230=CARTESIAN_POINT('Ctrl Pts',(0.188862140533343,-0.442737950614639,
-0.762655427419487));
#72231=CARTESIAN_POINT('Ctrl Pts',(0.474509248268113,-0.0807884543198489,
-0.738807245361255));
#72232=CARTESIAN_POINT('Ctrl Pts',(0.324732708102262,0.355294904731216,
-0.714959063303019));
#72233=CARTESIAN_POINT('Ctrl Pts',(-0.123028119751846,0.465349205210794,
-0.691110881244784));
#72234=CARTESIAN_POINT('Ctrl Pts',(-0.457894725037471,0.148385382825327,
-0.66726269918655));
#72235=CARTESIAN_POINT('Ctrl Pts',(-0.372583657756285,-0.304741232845733,
-0.643414517128315));
#72236=CARTESIAN_POINT('Ctrl Pts',(0.0546211364799233,-0.47822832672903,
-0.61956633507008));
#72237=CARTESIAN_POINT('Ctrl Pts',(0.431703968907574,-0.212879036894682,
-0.595718153011845));
#72238=CARTESIAN_POINT('Ctrl Pts',(0.412642536941405,0.247814320823537,
-0.571869970953611));
#72239=CARTESIAN_POINT('Ctrl Pts',(0.0149281723354398,0.481105966208734,
-0.548021788895376));
#72240=CARTESIAN_POINT('Ctrl Pts',(-0.396484723616044,0.272920621221822,
-0.524173606837142));
#72241=CARTESIAN_POINT('Ctrl Pts',(-0.44407156899152,-0.185704716060117,
-0.500325424778908));
#72242=CARTESIAN_POINT('Ctrl Pts',(-0.0841652808768616,-0.473921941809059,
-0.476477242720672));
#72243=CARTESIAN_POINT('Ctrl Pts',(0.352973553690336,-0.327254449368329,
-0.452629060662438));
#72244=CARTESIAN_POINT('Ctrl Pts',(0.466213453793493,0.119711354789871,
-0.428780878604203));
#72245=CARTESIAN_POINT('Ctrl Pts',(0.151642201636973,0.456826497412456,
-0.404932696545969));
#72246=CARTESIAN_POINT('Ctrl Pts',(-0.302080455174332,0.374744204734433,
-0.381084514487734));
#72247=CARTESIAN_POINT('Ctrl Pts',(-0.4786050856114,-0.051214396696121,
-0.3572363324295));
#72248=CARTESIAN_POINT('Ctrl Pts',(-0.215947823141546,-0.43017716036811,
-0.333388150371265));
#72249=CARTESIAN_POINT('Ctrl Pts',(0.244869930019852,-0.41439670526355,
-0.309539968313031));
#72250=CARTESIAN_POINT('Ctrl Pts',(0.480987035447976,-0.0183536387932365,
-0.285691786254796));
#72251=CARTESIAN_POINT('Ctrl Pts',(0.275737810703329,0.394531263495945,
-0.261843604196561));
#72252=CARTESIAN_POINT('Ctrl Pts',(-0.182539470678933,0.445382676016845,
-0.237995422138327));
#72253=CARTESIAN_POINT('Ctrl Pts',(-0.473307542664411,0.0875378286884531,
-0.214147240080092));
#72254=CARTESIAN_POINT('Ctrl Pts',(-0.329765473412989,-0.350634283536789,
-0.190299058021858));
#72255=CARTESIAN_POINT('Ctrl Pts',(0.116399798066751,-0.467054103255692,
-0.166450875963623));
#72256=CARTESIAN_POINT('Ctrl Pts',(0.45571346026384,-0.154891253173831,
-0.142602693905389));
#72257=CARTESIAN_POINT('Ctrl Pts',(0.376927294803572,0.299404210776717,
-0.118754511847154));
#72258=CARTESIAN_POINT('Ctrl Pts',(-0.0478848160134567,0.478957858820396,
-0.094906329788919));
#72259=CARTESIAN_POINT('Ctrl Pts',(-0.428475260777818,0.219005156546266,
-0.0710581477306846));
#72260=CARTESIAN_POINT('Ctrl Pts',(-0.416425965841839,-0.241912517045322,
-0.0472099656724497));
#72261=CARTESIAN_POINT('Ctrl Pts',(-0.0211921723080409,-0.480841568472938,
-0.0233617836142155));
#72262=CARTESIAN_POINT('Ctrl Pts',(0.322528130469684,-0.312288330204457,
-0.00348829856568646));
#72263=CARTESIAN_POINT('Ctrl Pts',(0.420797167432627,-0.0492196225713022,
0.0124104894731365));
#72264=CARTESIAN_POINT('Ctrl Pts',(0.402987368884735,0.08879030062507,0.0203598834925482));
#72265=CARTESIAN_POINT('Ctrl Pts',(0.377733926363309,0.151679871354634,
0.0243345805022539));
#72266=CARTESIAN_POINT('Ctrl Pts',(0.457029747534529,0.183521279061925,
-0.0249999999999995));
#72267=CARTESIAN_POINT('Ctrl Pts',(0.487584520760919,0.107429610755057,
-0.0289746970097051));
#72268=CARTESIAN_POINT('Ctrl Pts',(0.498358781643902,0.0239387777195438,
-0.0329493940194109));
#72269=CARTESIAN_POINT('Ctrl Pts',(0.488883640649376,-0.0575933168811649,
-0.0369240910291166));
#72270=CARTESIAN_POINT('Ctrl Pts',(0.47940849965485,-0.139125411481874,
-0.0408987880388223));
#72271=CARTESIAN_POINT('Ctrl Pts',(0.449683956782815,-0.218698767647778,
-0.0448734850485279));
#72272=CARTESIAN_POINT('Ctrl Pts',(0.402142540760437,-0.285343457672843,
-0.0488481820582336));
#72273=CARTESIAN_POINT('Ctrl Pts',(0.307059708715675,-0.418632837722982,
-0.0567975760776454));
#72274=CARTESIAN_POINT('Ctrl Pts',(0.140709384069528,-0.500207553209759,
-0.0647469700970572));
#72275=CARTESIAN_POINT('Ctrl Pts',(-0.0221663241796822,-0.492813869382451,
-0.072696364116469));
#72276=CARTESIAN_POINT('Ctrl Pts',(-0.185042032428883,-0.485420185555144,
-0.0806457581358803));
#72277=CARTESIAN_POINT('Ctrl Pts',(-0.344443124281146,-0.389058102413761,
-0.0885951521552916));
#72278=CARTESIAN_POINT('Ctrl Pts',(-0.426573460878355,-0.247931086047241,
-0.096544546174703));
#72279=CARTESIAN_POINT('Ctrl Pts',(-0.469867545071818,-0.173537564947853,
-0.100734979919682));
#72280=CARTESIAN_POINT('Ctrl Pts',(-0.491689996710417,-0.0867049756087339,
-0.104925413664661));
#72281=CARTESIAN_POINT('Ctrl Pts',(-0.491761526237315,7.34498668767403E-5,
-0.109115847409639));
#72282=CARTESIAN_POINT('Origin',(0.,0.,-0.0249999999999999));
#72283=CARTESIAN_POINT('',(-0.5175,6.33754718558755E-17,0.));
#72284=CARTESIAN_POINT('Origin',(-0.5175,-6.33754718558755E-17,-0.0249999999999999));
#72285=CARTESIAN_POINT('Origin',(0.,0.,0.));
#72286=CARTESIAN_POINT('Origin',(0.,0.,-0.0249999999999999));
#72287=CARTESIAN_POINT('Origin',(0.,0.,-1.725));
#72288=CARTESIAN_POINT('Origin',(0.77,0.,0.));
#72289=CARTESIAN_POINT('',(-0.77,-9.42978035343462E-17,8.67361737988404E-18));
#72290=CARTESIAN_POINT('Origin',(0.,0.,0.));
#72291=CARTESIAN_POINT('Origin',(0.,0.,0.4));
#72292=CARTESIAN_POINT('',(0.23094010767585,0.4,0.4));
#72293=CARTESIAN_POINT('',(0.461880215351701,0.,0.4));
#72294=CARTESIAN_POINT('',(0.461880215351701,0.,0.4));
#72295=CARTESIAN_POINT('Origin',(0.,0.,0.4));
#72296=CARTESIAN_POINT('Origin',(0.,0.,0.4));
#72297=CARTESIAN_POINT('',(0.23094010767585,-0.4,0.4));
#72298=CARTESIAN_POINT('',(0.23094010767585,-0.4,0.4));
#72299=CARTESIAN_POINT('Origin',(0.,0.,0.4));
#72300=CARTESIAN_POINT('Origin',(0.,0.,0.4));
#72301=CARTESIAN_POINT('',(-0.230940107675851,-0.4,0.4));
#72302=CARTESIAN_POINT('',(-0.230940107675851,-0.4,0.4));
#72303=CARTESIAN_POINT('Origin',(0.,0.,0.4));
#72304=CARTESIAN_POINT('Origin',(0.,0.,0.4));
#72305=CARTESIAN_POINT('',(-0.461880215351701,5.55111512312578E-17,0.4));
#72306=CARTESIAN_POINT('',(-0.461880215351701,5.6564012731995E-17,0.4));
#72307=CARTESIAN_POINT('Origin',(0.,0.,0.4));
#72308=CARTESIAN_POINT('Origin',(0.,0.,0.4));
#72309=CARTESIAN_POINT('',(-0.23094010767585,0.4,0.4));
#72310=CARTESIAN_POINT('',(-0.23094010767585,0.4,0.4));
#72311=CARTESIAN_POINT('Origin',(0.,0.,0.4));
#72312=CARTESIAN_POINT('Origin',(0.,0.,0.4));
#72313=CARTESIAN_POINT('',(0.23094010767585,0.4,0.4));
#72314=CARTESIAN_POINT('Origin',(0.,0.,0.4));
#72315=CARTESIAN_POINT('Origin',(0.,0.,0.26143593539449));
#72316=CARTESIAN_POINT('',(0.,0.,0.12287187078898));
#72317=CARTESIAN_POINT('',(-0.23094010767585,-2.82820063659975E-17,0.26143593539449));
#72318=CARTESIAN_POINT('Origin',(0.23094010767585,0.4,1.));
#72319=CARTESIAN_POINT('',(0.23094010767585,0.4,1.));
#72320=CARTESIAN_POINT('',(0.461880215351701,0.,1.));
#72321=CARTESIAN_POINT('',(0.288675134594813,0.3,1.));
#72322=CARTESIAN_POINT('',(0.23094010767585,0.4,1.));
#72323=CARTESIAN_POINT('',(0.461880215351701,0.,1.));
#72324=CARTESIAN_POINT('Origin',(-0.23094010767585,0.4,1.));
#72325=CARTESIAN_POINT('',(-0.23094010767585,0.4,1.));
#72326=CARTESIAN_POINT('',(-0.115470053837925,0.4,1.));
#72327=CARTESIAN_POINT('',(-0.23094010767585,0.4,1.));
#72328=CARTESIAN_POINT('Origin',(-0.461880215351701,5.55111512312578E-17,
1.));
#72329=CARTESIAN_POINT('',(-0.461880215351701,5.6564012731995E-17,1.));
#72330=CARTESIAN_POINT('',(-0.404145188432738,0.1,1.));
#72331=CARTESIAN_POINT('',(-0.461880215351701,5.6564012731995E-17,1.));
#72332=CARTESIAN_POINT('Origin',(-0.230940107675851,-0.4,1.));
#72333=CARTESIAN_POINT('',(-0.230940107675851,-0.4,1.));
#72334=CARTESIAN_POINT('',(-0.288675134594813,-0.3,1.));
#72335=CARTESIAN_POINT('',(-0.230940107675851,-0.4,1.));
#72336=CARTESIAN_POINT('Origin',(0.23094010767585,-0.4,1.));
#72337=CARTESIAN_POINT('',(0.23094010767585,-0.4,1.));
#72338=CARTESIAN_POINT('',(0.115470053837925,-0.4,1.));
#72339=CARTESIAN_POINT('',(0.23094010767585,-0.4,1.));
#72340=CARTESIAN_POINT('Origin',(0.461880215351701,0.,1.));
#72341=CARTESIAN_POINT('',(0.404145188432738,-0.1,1.));
#72342=CARTESIAN_POINT('Origin',(0.77322407690005,-0.32821414793099,0.95));
#72343=CARTESIAN_POINT('',(0.746549912099409,-0.28751213669055,0.0499999999999999));
#72344=CARTESIAN_POINT('',(0.746549912099409,-0.28751213669055,0.95));
#72345=CARTESIAN_POINT('',(0.746549912099409,-0.28751213669055,0.49));
#72346=CARTESIAN_POINT('',(0.732960244213009,-0.266775711794021,0.0499999999999999));
#72347=CARTESIAN_POINT('',(0.77322407690005,-0.32821414793099,0.0499999999999999));
#72348=CARTESIAN_POINT('',(0.732960244213009,-0.266775711794021,0.95));
#72349=CARTESIAN_POINT('',(0.732960244213009,-0.266775711794021,0.95));
#72350=CARTESIAN_POINT('',(0.77322407690005,-0.32821414793099,0.95));
#72351=CARTESIAN_POINT('Origin',(0.768128119610979,-0.286903189949045,0.95));
#72352=CARTESIAN_POINT('',(0.756699650773902,-0.259625958869015,0.95));
#72353=CARTESIAN_POINT('Origin',(0.,0.,0.95));
#72354=CARTESIAN_POINT('',(0.732960244213009,-0.266775711794021,0.95));
#72355=CARTESIAN_POINT('Origin',(0.732960244213009,-0.266775711794021,0.95));
#72356=CARTESIAN_POINT('',(0.756699650773902,-0.259625958869015,0.0499999999999999));
#72357=CARTESIAN_POINT('',(0.756699650773902,-0.259625958869015,0.49));
#72358=CARTESIAN_POINT('',(0.732960244213009,-0.266775711794021,0.0499999999999999));
#72359=CARTESIAN_POINT('Origin',(0.768128119610979,-0.286903189949045,0.0499999999999999));
#72360=CARTESIAN_POINT('Origin',(0.,0.,0.0499999999999999));
#72361=CARTESIAN_POINT('Origin',(0.614337109360103,-0.572878622452499,0.95));
#72362=CARTESIAN_POINT('',(0.603192501249412,-0.525508141170504,0.0499999999999999));
#72363=CARTESIAN_POINT('',(0.603192501249412,-0.525508141170504,0.95));
#72364=CARTESIAN_POINT('',(0.603192501249412,-0.525508141170504,0.49));
#72365=CARTESIAN_POINT('',(0.597514665632803,-0.501374335555501,0.0499999999999999));
#72366=CARTESIAN_POINT('',(0.614337109360103,-0.572878622452499,0.0499999999999999));
#72367=CARTESIAN_POINT('',(0.597514665632803,-0.501374335555501,0.95));
#72368=CARTESIAN_POINT('',(0.597514665632803,-0.501374335555501,0.95));
#72369=CARTESIAN_POINT('',(0.614337109360103,-0.572878622452499,0.95));
#72370=CARTESIAN_POINT('Origin',(0.634184247036264,-0.537126479004,0.95));
#72371=CARTESIAN_POINT('',(0.622267770320064,-0.502775120725853,0.95));
#72372=CARTESIAN_POINT('Origin',(0.,0.,0.95));
#72373=CARTESIAN_POINT('',(0.597514665632803,-0.501374335555501,0.95));
#72374=CARTESIAN_POINT('Origin',(0.597514665632803,-0.501374335555501,0.95));
#72375=CARTESIAN_POINT('',(0.622267770320064,-0.502775120725853,0.0499999999999999));
#72376=CARTESIAN_POINT('',(0.622267770320064,-0.502775120725853,0.49));
#72377=CARTESIAN_POINT('',(0.597514665632803,-0.501374335555501,0.0499999999999999));
#72378=CARTESIAN_POINT('Origin',(0.634184247036264,-0.537126479004,0.0499999999999999));
#72379=CARTESIAN_POINT('Origin',(0.,0.,0.0499999999999999));
#72380=CARTESIAN_POINT('Origin',(0.381352019781219,-0.748445480318229,0.95));
#72381=CARTESIAN_POINT('',(0.387081172575526,-0.700120108151134,0.0499999999999999));
#72382=CARTESIAN_POINT('',(0.387081172575526,-0.700120108151134,0.95));
#72383=CARTESIAN_POINT('',(0.387081172575525,-0.700120108151135,0.49));
#72384=CARTESIAN_POINT('',(0.39,-0.675499814951862,0.0499999999999999));
#72385=CARTESIAN_POINT('',(0.381352019781219,-0.748445480318229,0.0499999999999999));
#72386=CARTESIAN_POINT('',(0.39,-0.675499814951862,0.95));
#72387=CARTESIAN_POINT('',(0.39,-0.675499814951862,0.95));
#72388=CARTESIAN_POINT('',(0.381352019781219,-0.748445480318229,0.95));
#72389=CARTESIAN_POINT('Origin',(0.419424404596921,-0.711972647635046,0.95));
#72390=CARTESIAN_POINT('',(0.412781213071428,-0.685282182852641,0.95));
#72391=CARTESIAN_POINT('Origin',(0.,0.,0.95));
#72392=CARTESIAN_POINT('',(0.39,-0.675499814951862,0.95));
#72393=CARTESIAN_POINT('Origin',(0.39,-0.675499814951862,0.95));
#72394=CARTESIAN_POINT('',(0.412781213071428,-0.685282182852641,0.0499999999999999));
#72395=CARTESIAN_POINT('',(0.412781213071428,-0.685282182852641,0.49));
#72396=CARTESIAN_POINT('',(0.39,-0.675499814951862,0.0499999999999999));
#72397=CARTESIAN_POINT('Origin',(0.419424404596921,-0.711972647635046,0.0499999999999999));
#72398=CARTESIAN_POINT('Origin',(0.,0.,0.0499999999999999));
#72399=CARTESIAN_POINT('Origin',(0.102370248460324,-0.833738767378711,0.95));
#72400=CARTESIAN_POINT('',(0.124282141779344,-0.790287257416402,0.0499999999999999));
#72401=CARTESIAN_POINT('',(0.124282141779344,-0.790287257416402,0.95));
#72402=CARTESIAN_POINT('',(0.124282141779344,-0.790287257416402,0.49));
#72403=CARTESIAN_POINT('',(0.135445578580205,-0.768150047349522,0.0499999999999999));
#72404=CARTESIAN_POINT('',(0.102370248460324,-0.833738767378711,0.0499999999999999));
#72405=CARTESIAN_POINT('',(0.135445578580205,-0.768150047349522,0.95));
#72406=CARTESIAN_POINT('',(0.135445578580205,-0.768150047349522,0.95));
#72407=CARTESIAN_POINT('',(0.102370248460324,-0.833738767378711,0.95));
#72408=CARTESIAN_POINT('Origin',(0.145664567054585,-0.800944407364116,0.95));
#72409=CARTESIAN_POINT('',(0.15350714952449,-0.785134100039519,0.95));
#72410=CARTESIAN_POINT('Origin',(0.,0.,0.95));
#72411=CARTESIAN_POINT('',(0.135445578580205,-0.768150047349522,0.95));
#72412=CARTESIAN_POINT('Origin',(0.135445578580205,-0.768150047349522,0.95));
#72413=CARTESIAN_POINT('',(0.15350714952449,-0.785134100039519,0.0499999999999999));
#72414=CARTESIAN_POINT('',(0.15350714952449,-0.785134100039519,0.49));
#72415=CARTESIAN_POINT('',(0.135445578580205,-0.768150047349522,0.0499999999999999));
#72416=CARTESIAN_POINT('Origin',(0.145664567054585,-0.800944407364116,0.0499999999999999));
#72417=CARTESIAN_POINT('Origin',(0.,0.,0.0499999999999999));
#72418=CARTESIAN_POINT('Origin',(-0.188958885648847,-0.818470854419598,
0.95));
#72419=CARTESIAN_POINT('',(-0.15350714952449,-0.785134100039519,0.0499999999999999));
#72420=CARTESIAN_POINT('',(-0.15350714952449,-0.785134100039519,0.95));
#72421=CARTESIAN_POINT('',(-0.15350714952449,-0.785134100039519,0.49));
#72422=CARTESIAN_POINT('',(-0.135445578580206,-0.768150047349522,0.0499999999999999));
#72423=CARTESIAN_POINT('',(-0.188958885648847,-0.818470854419598,0.0499999999999999));
#72424=CARTESIAN_POINT('',(-0.135445578580206,-0.768150047349522,0.95));
#72425=CARTESIAN_POINT('',(-0.135445578580206,-0.768150047349522,0.95));
#72426=CARTESIAN_POINT('',(-0.188958885648847,-0.818470854419598,0.95));
#72427=CARTESIAN_POINT('Origin',(-0.145664567054585,-0.800944407364116,
0.95));
#72428=CARTESIAN_POINT('',(-0.124282141779344,-0.790287257416402,0.95));
#72429=CARTESIAN_POINT('Origin',(0.,0.,0.95));
#72430=CARTESIAN_POINT('',(-0.135445578580206,-0.768150047349522,0.95));
#72431=CARTESIAN_POINT('Origin',(-0.135445578580206,-0.768150047349522,
0.95));
#72432=CARTESIAN_POINT('',(-0.124282141779344,-0.790287257416402,0.0499999999999999));
#72433=CARTESIAN_POINT('',(-0.124282141779344,-0.790287257416402,0.49));
#72434=CARTESIAN_POINT('',(-0.135445578580206,-0.768150047349522,0.0499999999999999));
#72435=CARTESIAN_POINT('Origin',(-0.145664567054585,-0.800944407364116,
0.0499999999999999));
#72436=CARTESIAN_POINT('Origin',(0.,0.,0.0499999999999999));
#72437=CARTESIAN_POINT('Origin',(-0.457496789412623,-0.704483277074156,
0.95));
#72438=CARTESIAN_POINT('',(-0.412781213071429,-0.685282182852641,0.0499999999999999));
#72439=CARTESIAN_POINT('',(-0.412781213071429,-0.685282182852641,0.95));
#72440=CARTESIAN_POINT('',(-0.412781213071429,-0.685282182852641,0.49));
#72441=CARTESIAN_POINT('',(-0.39,-0.675499814951862,0.0499999999999999));
#72442=CARTESIAN_POINT('',(-0.457496789412623,-0.704483277074156,0.0499999999999999));
#72443=CARTESIAN_POINT('',(-0.39,-0.675499814951862,0.95));
#72444=CARTESIAN_POINT('',(-0.39,-0.675499814951862,0.95));
#72445=CARTESIAN_POINT('',(-0.457496789412623,-0.704483277074156,0.95));
#72446=CARTESIAN_POINT('Origin',(-0.419424404596921,-0.711972647635045,
0.95));
#72447=CARTESIAN_POINT('',(-0.387081172575526,-0.700120108151134,0.95));
#72448=CARTESIAN_POINT('Origin',(0.,0.,0.95));
#72449=CARTESIAN_POINT('',(-0.39,-0.675499814951862,0.95));
#72450=CARTESIAN_POINT('Origin',(-0.39,-0.675499814951862,0.95));
#72451=CARTESIAN_POINT('',(-0.387081172575526,-0.700120108151134,0.0499999999999999));
#72452=CARTESIAN_POINT('',(-0.387081172575526,-0.700120108151134,0.49));
#72453=CARTESIAN_POINT('',(-0.39,-0.675499814951862,0.0499999999999999));
#72454=CARTESIAN_POINT('Origin',(-0.419424404596921,-0.711972647635045,
0.0499999999999999));
#72455=CARTESIAN_POINT('Origin',(0.,0.,0.0499999999999999));
#72456=CARTESIAN_POINT('Origin',(-0.670853828439726,-0.505524619447721,
0.95));
#72457=CARTESIAN_POINT('',(-0.622267770320064,-0.502775120725853,0.0499999999999999));
#72458=CARTESIAN_POINT('',(-0.622267770320064,-0.502775120725853,0.95));
#72459=CARTESIAN_POINT('',(-0.622267770320064,-0.502775120725853,0.49));
#72460=CARTESIAN_POINT('',(-0.597514665632803,-0.501374335555501,0.0499999999999999));
#72461=CARTESIAN_POINT('',(-0.670853828439726,-0.505524619447721,0.0499999999999999));
#72462=CARTESIAN_POINT('',(-0.597514665632803,-0.501374335555501,0.95));
#72463=CARTESIAN_POINT('',(-0.597514665632803,-0.501374335555501,0.95));
#72464=CARTESIAN_POINT('',(-0.670853828439726,-0.505524619447721,0.95));
#72465=CARTESIAN_POINT('Origin',(-0.634184247036264,-0.537126479004,0.95));
#72466=CARTESIAN_POINT('',(-0.603192501249412,-0.525508141170504,0.95));
#72467=CARTESIAN_POINT('Origin',(0.,0.,0.95));
#72468=CARTESIAN_POINT('',(-0.597514665632803,-0.501374335555501,0.95));
#72469=CARTESIAN_POINT('Origin',(-0.597514665632803,-0.501374335555501,
0.95));
#72470=CARTESIAN_POINT('',(-0.603192501249412,-0.525508141170504,0.0499999999999999));
#72471=CARTESIAN_POINT('',(-0.603192501249412,-0.525508141170504,0.49));
#72472=CARTESIAN_POINT('',(-0.597514665632803,-0.501374335555501,0.0499999999999999));
#72473=CARTESIAN_POINT('Origin',(-0.634184247036264,-0.537126479004,0.0499999999999999));
#72474=CARTESIAN_POINT('Origin',(0.,0.,0.0499999999999999));
#72475=CARTESIAN_POINT('Origin',(-0.80329599500895,-0.245592231967099,0.95));
#72476=CARTESIAN_POINT('',(-0.756699650773902,-0.259625958869015,0.0499999999999999));
#72477=CARTESIAN_POINT('',(-0.756699650773902,-0.259625958869015,0.95));
#72478=CARTESIAN_POINT('',(-0.756699650773902,-0.259625958869015,0.49));
#72479=CARTESIAN_POINT('',(-0.732960244213009,-0.266775711794022,0.0499999999999999));
#72480=CARTESIAN_POINT('',(-0.80329599500895,-0.245592231967099,0.0499999999999999));
#72481=CARTESIAN_POINT('',(-0.732960244213009,-0.266775711794022,0.95));
#72482=CARTESIAN_POINT('',(-0.732960244213009,-0.266775711794022,0.95));
#72483=CARTESIAN_POINT('',(-0.80329599500895,-0.245592231967099,0.95));
#72484=CARTESIAN_POINT('Origin',(-0.768128119610979,-0.286903189949044,
0.95));
#72485=CARTESIAN_POINT('',(-0.746549912099409,-0.287512136690549,0.95));
#72486=CARTESIAN_POINT('Origin',(0.,0.,0.95));
#72487=CARTESIAN_POINT('',(-0.732960244213009,-0.266775711794022,0.95));
#72488=CARTESIAN_POINT('Origin',(-0.732960244213009,-0.266775711794022,
0.95));
#72489=CARTESIAN_POINT('',(-0.746549912099409,-0.287512136690549,0.0499999999999999));
#72490=CARTESIAN_POINT('',(-0.746549912099409,-0.287512136690549,0.49));
#72491=CARTESIAN_POINT('',(-0.732960244213009,-0.266775711794022,0.0499999999999999));
#72492=CARTESIAN_POINT('Origin',(-0.768128119610979,-0.286903189949044,
0.0499999999999999));
#72493=CARTESIAN_POINT('Origin',(0.,0.,0.0499999999999999));
#72494=CARTESIAN_POINT('Origin',(-0.838848809193842,0.0439622032440728,
0.95));
#72495=CARTESIAN_POINT('',(-0.799862385646954,0.0148379252984938,0.0499999999999999));
#72496=CARTESIAN_POINT('',(-0.799862385646954,0.0148379252984938,0.95));
#72497=CARTESIAN_POINT('',(-0.799862385646954,0.0148379252984938,0.49));
#72498=CARTESIAN_POINT('',(-0.78,9.55224503334935E-17,0.0499999999999999));
#72499=CARTESIAN_POINT('',(-0.838848809193842,0.0439622032440728,0.0499999999999999));
#72500=CARTESIAN_POINT('',(-0.78,9.55224503334935E-17,0.95));
#72501=CARTESIAN_POINT('',(-0.78,9.55224503334935E-17,0.95));
#72502=CARTESIAN_POINT('',(-0.838848809193842,0.0439622032440728,0.95));
#72503=CARTESIAN_POINT('Origin',(-0.809424404596921,1.04083408558608E-16,
0.95));
#72504=CARTESIAN_POINT('',(-0.8,-9.79717439317883E-17,0.95));
#72505=CARTESIAN_POINT('Origin',(0.,0.,0.95));
#72506=CARTESIAN_POINT('',(-0.799862385646954,-0.0148379252984938,0.95));
#72507=CARTESIAN_POINT('',(-0.78,9.55224503334935E-17,0.95));
#72508=CARTESIAN_POINT('Origin',(0.,0.,0.95));
#72509=CARTESIAN_POINT('Origin',(-0.78,9.55224503334935E-17,0.95));
#72510=CARTESIAN_POINT('',(-0.799862385646954,-0.0148379252984938,0.0499999999999999));
#72511=CARTESIAN_POINT('',(-0.799862385646954,-0.0148379252984938,0.49));
#72512=CARTESIAN_POINT('',(-0.78,9.55224503334935E-17,0.0499999999999999));
#72513=CARTESIAN_POINT('Origin',(-0.809424404596921,1.04083408558608E-16,
0.0499999999999999));
#72514=CARTESIAN_POINT('',(-0.8,-9.79717439317883E-17,0.0499999999999999));
#72515=CARTESIAN_POINT('Origin',(0.,0.,0.0499999999999999));
#72516=CARTESIAN_POINT('Origin',(0.,0.,0.0499999999999999));
#72517=CARTESIAN_POINT('Origin',(-0.818470854419598,0.188958885648847,0.95));
#72518=CARTESIAN_POINT('',(-0.785134100039519,0.15350714952449,0.0499999999999999));
#72519=CARTESIAN_POINT('',(-0.785134100039519,0.15350714952449,0.95));
#72520=CARTESIAN_POINT('',(-0.785134100039519,0.15350714952449,0.49));
#72521=CARTESIAN_POINT('',(-0.768150047349522,0.135445578580206,0.0499999999999999));
#72522=CARTESIAN_POINT('',(-0.818470854419598,0.188958885648847,0.0499999999999999));
#72523=CARTESIAN_POINT('',(-0.768150047349522,0.135445578580206,0.95));
#72524=CARTESIAN_POINT('',(-0.768150047349522,0.135445578580206,0.95));
#72525=CARTESIAN_POINT('',(-0.818470854419598,0.188958885648847,0.95));
#72526=CARTESIAN_POINT('Origin',(-0.800944407364116,0.145664567054585,0.95));
#72527=CARTESIAN_POINT('',(-0.790287257416402,0.124282141779344,0.95));
#72528=CARTESIAN_POINT('Origin',(0.,0.,0.95));
#72529=CARTESIAN_POINT('',(-0.768150047349522,0.135445578580206,0.95));
#72530=CARTESIAN_POINT('Origin',(-0.768150047349522,0.135445578580206,0.95));
#72531=CARTESIAN_POINT('',(-0.790287257416402,0.124282141779344,0.0499999999999999));
#72532=CARTESIAN_POINT('',(-0.790287257416402,0.124282141779344,0.49));
#72533=CARTESIAN_POINT('',(-0.768150047349522,0.135445578580206,0.0499999999999999));
#72534=CARTESIAN_POINT('Origin',(-0.800944407364116,0.145664567054585,0.0499999999999999));
#72535=CARTESIAN_POINT('Origin',(0.,0.,0.0499999999999999));
#72536=CARTESIAN_POINT('Origin',(-0.704483277074156,0.457496789412623,0.95));
#72537=CARTESIAN_POINT('',(-0.685282182852641,0.412781213071428,0.0499999999999999));
#72538=CARTESIAN_POINT('',(-0.685282182852641,0.412781213071428,0.95));
#72539=CARTESIAN_POINT('',(-0.685282182852641,0.412781213071428,0.49));
#72540=CARTESIAN_POINT('',(-0.675499814951862,0.39,0.0499999999999999));
#72541=CARTESIAN_POINT('',(-0.704483277074156,0.457496789412623,0.0499999999999999));
#72542=CARTESIAN_POINT('',(-0.675499814951862,0.39,0.95));
#72543=CARTESIAN_POINT('',(-0.675499814951862,0.39,0.95));
#72544=CARTESIAN_POINT('',(-0.704483277074156,0.457496789412623,0.95));
#72545=CARTESIAN_POINT('Origin',(-0.711972647635046,0.419424404596921,0.95));
#72546=CARTESIAN_POINT('',(-0.700120108151135,0.387081172575525,0.95));
#72547=CARTESIAN_POINT('Origin',(0.,0.,0.95));
#72548=CARTESIAN_POINT('',(-0.675499814951862,0.39,0.95));
#72549=CARTESIAN_POINT('Origin',(-0.675499814951862,0.39,0.95));
#72550=CARTESIAN_POINT('',(-0.700120108151135,0.387081172575525,0.0499999999999999));
#72551=CARTESIAN_POINT('',(-0.700120108151135,0.387081172575525,0.49));
#72552=CARTESIAN_POINT('',(-0.675499814951862,0.39,0.0499999999999999));
#72553=CARTESIAN_POINT('Origin',(-0.711972647635046,0.419424404596921,0.0499999999999999));
#72554=CARTESIAN_POINT('Origin',(0.,0.,0.0499999999999999));
#72555=CARTESIAN_POINT('Origin',(-0.505524619447721,0.670853828439726,0.95));
#72556=CARTESIAN_POINT('',(-0.502775120725853,0.622267770320064,0.0499999999999999));
#72557=CARTESIAN_POINT('',(-0.502775120725853,0.622267770320064,0.95));
#72558=CARTESIAN_POINT('',(-0.502775120725853,0.622267770320064,0.49));
#72559=CARTESIAN_POINT('',(-0.501374335555501,0.597514665632803,0.0499999999999999));
#72560=CARTESIAN_POINT('',(-0.505524619447721,0.670853828439726,0.0499999999999999));
#72561=CARTESIAN_POINT('',(-0.501374335555501,0.597514665632803,0.95));
#72562=CARTESIAN_POINT('',(-0.501374335555501,0.597514665632803,0.95));
#72563=CARTESIAN_POINT('',(-0.505524619447721,0.670853828439726,0.95));
#72564=CARTESIAN_POINT('Origin',(-0.537126479004,0.634184247036264,0.95));
#72565=CARTESIAN_POINT('',(-0.525508141170504,0.603192501249412,0.95));
#72566=CARTESIAN_POINT('Origin',(0.,0.,0.95));
#72567=CARTESIAN_POINT('',(-0.501374335555501,0.597514665632803,0.95));
#72568=CARTESIAN_POINT('Origin',(-0.501374335555501,0.597514665632803,0.95));
#72569=CARTESIAN_POINT('',(-0.525508141170504,0.603192501249412,0.0499999999999999));
#72570=CARTESIAN_POINT('',(-0.525508141170504,0.603192501249412,0.49));
#72571=CARTESIAN_POINT('',(-0.501374335555501,0.597514665632803,0.0499999999999999));
#72572=CARTESIAN_POINT('Origin',(-0.537126479004,0.634184247036264,0.0499999999999999));
#72573=CARTESIAN_POINT('Origin',(0.,0.,0.0499999999999999));
#72574=CARTESIAN_POINT('Origin',(-0.245592231967099,0.80329599500895,0.95));
#72575=CARTESIAN_POINT('',(-0.259625958869015,0.756699650773901,0.0499999999999999));
#72576=CARTESIAN_POINT('',(-0.259625958869015,0.756699650773901,0.95));
#72577=CARTESIAN_POINT('',(-0.259625958869015,0.756699650773901,0.49));
#72578=CARTESIAN_POINT('',(-0.266775711794022,0.732960244213009,0.0499999999999999));
#72579=CARTESIAN_POINT('',(-0.245592231967099,0.80329599500895,0.0499999999999999));
#72580=CARTESIAN_POINT('',(-0.266775711794022,0.732960244213009,0.95));
#72581=CARTESIAN_POINT('',(-0.266775711794022,0.732960244213009,0.95));
#72582=CARTESIAN_POINT('',(-0.245592231967099,0.80329599500895,0.95));
#72583=CARTESIAN_POINT('Origin',(-0.286903189949044,0.768128119610979,0.95));
#72584=CARTESIAN_POINT('',(-0.28751213669055,0.746549912099409,0.95));
#72585=CARTESIAN_POINT('Origin',(0.,0.,0.95));
#72586=CARTESIAN_POINT('',(-0.266775711794022,0.732960244213009,0.95));
#72587=CARTESIAN_POINT('Origin',(-0.266775711794022,0.732960244213009,0.95));
#72588=CARTESIAN_POINT('',(-0.28751213669055,0.746549912099409,0.0499999999999999));
#72589=CARTESIAN_POINT('',(-0.28751213669055,0.746549912099409,0.49));
#72590=CARTESIAN_POINT('',(-0.266775711794022,0.732960244213009,0.0499999999999999));
#72591=CARTESIAN_POINT('Origin',(-0.286903189949044,0.768128119610979,0.0499999999999999));
#72592=CARTESIAN_POINT('Origin',(0.,0.,0.0499999999999999));
#72593=CARTESIAN_POINT('Origin',(0.0439622032440729,0.838848809193842,0.95));
#72594=CARTESIAN_POINT('',(0.0148379252984938,0.799862385646954,0.0499999999999999));
#72595=CARTESIAN_POINT('',(0.0148379252984938,0.799862385646954,0.95));
#72596=CARTESIAN_POINT('',(0.0148379252984938,0.799862385646954,0.49));
#72597=CARTESIAN_POINT('',(4.77612251667468E-17,0.78,0.0499999999999999));
#72598=CARTESIAN_POINT('',(0.0439622032440729,0.838848809193842,0.0499999999999999));
#72599=CARTESIAN_POINT('',(4.77612251667468E-17,0.78,0.95));
#72600=CARTESIAN_POINT('',(4.77612251667468E-17,0.78,0.95));
#72601=CARTESIAN_POINT('',(0.0439622032440729,0.838848809193842,0.95));
#72602=CARTESIAN_POINT('Origin',(4.85722573273506E-17,0.809424404596921,
0.95));
#72603=CARTESIAN_POINT('',(-0.0148379252984937,0.799862385646954,0.95));
#72604=CARTESIAN_POINT('Origin',(0.,0.,0.95));
#72605=CARTESIAN_POINT('',(4.77612251667468E-17,0.78,0.95));
#72606=CARTESIAN_POINT('Origin',(4.77612251667468E-17,0.78,0.95));
#72607=CARTESIAN_POINT('',(-0.0148379252984937,0.799862385646954,0.0499999999999999));
#72608=CARTESIAN_POINT('',(-0.0148379252984937,0.799862385646954,0.49));
#72609=CARTESIAN_POINT('',(4.77612251667468E-17,0.78,0.0499999999999999));
#72610=CARTESIAN_POINT('Origin',(4.85722573273506E-17,0.809424404596921,
0.0499999999999999));
#72611=CARTESIAN_POINT('Origin',(0.,0.,0.0499999999999999));
#72612=CARTESIAN_POINT('Origin',(0.32821414793099,0.77322407690005,0.95));
#72613=CARTESIAN_POINT('',(0.28751213669055,0.746549912099409,0.0499999999999999));
#72614=CARTESIAN_POINT('',(0.28751213669055,0.746549912099409,0.95));
#72615=CARTESIAN_POINT('',(0.28751213669055,0.746549912099409,0.49));
#72616=CARTESIAN_POINT('',(0.266775711794022,0.732960244213009,0.0499999999999999));
#72617=CARTESIAN_POINT('',(0.32821414793099,0.77322407690005,0.0499999999999999));
#72618=CARTESIAN_POINT('',(0.266775711794022,0.732960244213009,0.95));
#72619=CARTESIAN_POINT('',(0.266775711794022,0.732960244213009,0.95));
#72620=CARTESIAN_POINT('',(0.32821414793099,0.77322407690005,0.95));
#72621=CARTESIAN_POINT('Origin',(0.286903189949044,0.768128119610979,0.95));
#72622=CARTESIAN_POINT('',(0.259625958869015,0.756699650773901,0.95));
#72623=CARTESIAN_POINT('Origin',(0.,0.,0.95));
#72624=CARTESIAN_POINT('',(0.266775711794022,0.732960244213009,0.95));
#72625=CARTESIAN_POINT('Origin',(0.266775711794022,0.732960244213009,0.95));
#72626=CARTESIAN_POINT('',(0.259625958869015,0.756699650773901,0.0499999999999999));
#72627=CARTESIAN_POINT('',(0.259625958869015,0.756699650773901,0.49));
#72628=CARTESIAN_POINT('',(0.266775711794022,0.732960244213009,0.0499999999999999));
#72629=CARTESIAN_POINT('Origin',(0.286903189949044,0.768128119610979,0.0499999999999999));
#72630=CARTESIAN_POINT('Origin',(0.,0.,0.0499999999999999));
#72631=CARTESIAN_POINT('Origin',(0.572878622452499,0.614337109360103,0.95));
#72632=CARTESIAN_POINT('',(0.525508141170504,0.603192501249412,0.0499999999999999));
#72633=CARTESIAN_POINT('',(0.525508141170504,0.603192501249412,0.95));
#72634=CARTESIAN_POINT('',(0.525508141170504,0.603192501249412,0.49));
#72635=CARTESIAN_POINT('',(0.501374335555501,0.597514665632803,0.0499999999999999));
#72636=CARTESIAN_POINT('',(0.572878622452499,0.614337109360103,0.0499999999999999));
#72637=CARTESIAN_POINT('',(0.501374335555501,0.597514665632803,0.95));
#72638=CARTESIAN_POINT('',(0.501374335555501,0.597514665632803,0.95));
#72639=CARTESIAN_POINT('',(0.572878622452499,0.614337109360103,0.95));
#72640=CARTESIAN_POINT('Origin',(0.537126479004,0.634184247036264,0.95));
#72641=CARTESIAN_POINT('',(0.502775120725853,0.622267770320064,0.95));
#72642=CARTESIAN_POINT('Origin',(0.,0.,0.95));
#72643=CARTESIAN_POINT('',(0.501374335555501,0.597514665632803,0.95));
#72644=CARTESIAN_POINT('Origin',(0.501374335555501,0.597514665632803,0.95));
#72645=CARTESIAN_POINT('',(0.502775120725853,0.622267770320064,0.0499999999999999));
#72646=CARTESIAN_POINT('',(0.502775120725853,0.622267770320064,0.49));
#72647=CARTESIAN_POINT('',(0.501374335555501,0.597514665632803,0.0499999999999999));
#72648=CARTESIAN_POINT('Origin',(0.537126479004,0.634184247036264,0.0499999999999999));
#72649=CARTESIAN_POINT('Origin',(0.,0.,0.0499999999999999));
#72650=CARTESIAN_POINT('Origin',(0.748445480318229,0.381352019781219,0.95));
#72651=CARTESIAN_POINT('',(0.700120108151135,0.387081172575526,0.0499999999999999));
#72652=CARTESIAN_POINT('',(0.700120108151135,0.387081172575526,0.95));
#72653=CARTESIAN_POINT('',(0.700120108151135,0.387081172575526,0.49));
#72654=CARTESIAN_POINT('',(0.675499814951862,0.39,0.0499999999999999));
#72655=CARTESIAN_POINT('',(0.748445480318229,0.381352019781219,0.0499999999999999));
#72656=CARTESIAN_POINT('',(0.675499814951862,0.39,0.95));
#72657=CARTESIAN_POINT('',(0.675499814951862,0.39,0.95));
#72658=CARTESIAN_POINT('',(0.748445480318229,0.381352019781219,0.95));
#72659=CARTESIAN_POINT('Origin',(0.711972647635046,0.419424404596921,0.95));
#72660=CARTESIAN_POINT('',(0.685282182852641,0.412781213071428,0.95));
#72661=CARTESIAN_POINT('Origin',(0.,0.,0.95));
#72662=CARTESIAN_POINT('',(0.675499814951862,0.39,0.95));
#72663=CARTESIAN_POINT('Origin',(0.675499814951862,0.39,0.95));
#72664=CARTESIAN_POINT('',(0.685282182852641,0.412781213071428,0.0499999999999999));
#72665=CARTESIAN_POINT('',(0.685282182852641,0.412781213071428,0.49));
#72666=CARTESIAN_POINT('',(0.675499814951862,0.39,0.0499999999999999));
#72667=CARTESIAN_POINT('Origin',(0.711972647635046,0.419424404596921,0.0499999999999999));
#72668=CARTESIAN_POINT('Origin',(0.,0.,0.0499999999999999));
#72669=CARTESIAN_POINT('Origin',(0.833738767378711,0.102370248460324,0.95));
#72670=CARTESIAN_POINT('',(0.790287257416402,0.124282141779344,0.0499999999999999));
#72671=CARTESIAN_POINT('',(0.790287257416402,0.124282141779344,0.95));
#72672=CARTESIAN_POINT('',(0.790287257416402,0.124282141779344,0.49));
#72673=CARTESIAN_POINT('',(0.768150047349522,0.135445578580206,0.0499999999999999));
#72674=CARTESIAN_POINT('',(0.833738767378711,0.102370248460324,0.0499999999999999));
#72675=CARTESIAN_POINT('',(0.768150047349522,0.135445578580206,0.95));
#72676=CARTESIAN_POINT('',(0.768150047349522,0.135445578580206,0.95));
#72677=CARTESIAN_POINT('',(0.833738767378711,0.102370248460324,0.95));
#72678=CARTESIAN_POINT('Origin',(0.800944407364116,0.145664567054585,0.95));
#72679=CARTESIAN_POINT('',(0.785134100039519,0.15350714952449,0.95));
#72680=CARTESIAN_POINT('Origin',(0.,0.,0.95));
#72681=CARTESIAN_POINT('',(0.768150047349522,0.135445578580206,0.95));
#72682=CARTESIAN_POINT('Origin',(0.768150047349522,0.135445578580206,0.95));
#72683=CARTESIAN_POINT('',(0.785134100039519,0.15350714952449,0.0499999999999999));
#72684=CARTESIAN_POINT('',(0.785134100039519,0.15350714952449,0.49));
#72685=CARTESIAN_POINT('',(0.768150047349522,0.135445578580206,0.0499999999999999));
#72686=CARTESIAN_POINT('Origin',(0.800944407364116,0.145664567054585,0.0499999999999999));
#72687=CARTESIAN_POINT('Origin',(0.,0.,0.0499999999999999));
#72688=CARTESIAN_POINT('Origin',(0.80329599500895,0.245592231967099,0.95));
#72689=CARTESIAN_POINT('',(0.756699650773901,0.259625958869015,0.0499999999999999));
#72690=CARTESIAN_POINT('',(0.756699650773901,0.259625958869015,0.95));
#72691=CARTESIAN_POINT('',(0.756699650773902,0.259625958869015,0.49));
#72692=CARTESIAN_POINT('',(0.732960244213009,0.266775711794022,0.0499999999999999));
#72693=CARTESIAN_POINT('',(0.80329599500895,0.245592231967099,0.0499999999999999));
#72694=CARTESIAN_POINT('',(0.732960244213009,0.266775711794022,0.95));
#72695=CARTESIAN_POINT('',(0.732960244213009,0.266775711794022,0.95));
#72696=CARTESIAN_POINT('',(0.80329599500895,0.245592231967099,0.95));
#72697=CARTESIAN_POINT('Origin',(0.768128119610979,0.286903189949044,0.95));
#72698=CARTESIAN_POINT('',(0.746549912099409,0.28751213669055,0.95));
#72699=CARTESIAN_POINT('Origin',(0.,0.,0.95));
#72700=CARTESIAN_POINT('',(0.732960244213009,0.266775711794022,0.95));
#72701=CARTESIAN_POINT('Origin',(0.732960244213009,0.266775711794022,0.95));
#72702=CARTESIAN_POINT('',(0.746549912099409,0.28751213669055,0.0499999999999999));
#72703=CARTESIAN_POINT('',(0.746549912099409,0.28751213669055,0.49));
#72704=CARTESIAN_POINT('',(0.732960244213009,0.266775711794022,0.0499999999999999));
#72705=CARTESIAN_POINT('Origin',(0.768128119610979,0.286903189949044,0.0499999999999999));
#72706=CARTESIAN_POINT('Origin',(0.,0.,0.0499999999999999));
#72707=CARTESIAN_POINT('Origin',(0.670853828439726,0.505524619447721,0.95));
#72708=CARTESIAN_POINT('',(0.622267770320064,0.502775120725853,0.0499999999999999));
#72709=CARTESIAN_POINT('',(0.622267770320064,0.502775120725853,0.95));
#72710=CARTESIAN_POINT('',(0.622267770320064,0.502775120725853,0.49));
#72711=CARTESIAN_POINT('',(0.597514665632803,0.501374335555501,0.0499999999999999));
#72712=CARTESIAN_POINT('',(0.670853828439726,0.505524619447721,0.0499999999999999));
#72713=CARTESIAN_POINT('',(0.597514665632803,0.501374335555501,0.95));
#72714=CARTESIAN_POINT('',(0.597514665632803,0.501374335555501,0.95));
#72715=CARTESIAN_POINT('',(0.670853828439726,0.505524619447721,0.95));
#72716=CARTESIAN_POINT('Origin',(0.634184247036264,0.537126479004,0.95));
#72717=CARTESIAN_POINT('',(0.603192501249412,0.525508141170504,0.95));
#72718=CARTESIAN_POINT('Origin',(0.,0.,0.95));
#72719=CARTESIAN_POINT('',(0.597514665632803,0.501374335555501,0.95));
#72720=CARTESIAN_POINT('Origin',(0.597514665632803,0.501374335555501,0.95));
#72721=CARTESIAN_POINT('',(0.603192501249412,0.525508141170504,0.0499999999999999));
#72722=CARTESIAN_POINT('',(0.603192501249412,0.525508141170504,0.49));
#72723=CARTESIAN_POINT('',(0.597514665632803,0.501374335555501,0.0499999999999999));
#72724=CARTESIAN_POINT('Origin',(0.634184247036264,0.537126479004,0.0499999999999999));
#72725=CARTESIAN_POINT('Origin',(0.,0.,0.0499999999999999));
#72726=CARTESIAN_POINT('Origin',(0.457496789412623,0.704483277074156,0.95));
#72727=CARTESIAN_POINT('',(0.412781213071428,0.685282182852641,0.0499999999999999));
#72728=CARTESIAN_POINT('',(0.412781213071428,0.685282182852641,0.95));
#72729=CARTESIAN_POINT('',(0.412781213071428,0.685282182852641,0.49));
#72730=CARTESIAN_POINT('',(0.39,0.675499814951862,0.0499999999999999));
#72731=CARTESIAN_POINT('',(0.457496789412623,0.704483277074156,0.0499999999999999));
#72732=CARTESIAN_POINT('',(0.39,0.675499814951862,0.95));
#72733=CARTESIAN_POINT('',(0.39,0.675499814951862,0.95));
#72734=CARTESIAN_POINT('',(0.457496789412623,0.704483277074156,0.95));
#72735=CARTESIAN_POINT('Origin',(0.419424404596921,0.711972647635046,0.95));
#72736=CARTESIAN_POINT('',(0.387081172575526,0.700120108151134,0.95));
#72737=CARTESIAN_POINT('Origin',(0.,0.,0.95));
#72738=CARTESIAN_POINT('',(0.39,0.675499814951862,0.95));
#72739=CARTESIAN_POINT('Origin',(0.39,0.675499814951862,0.95));
#72740=CARTESIAN_POINT('',(0.387081172575526,0.700120108151134,0.0499999999999999));
#72741=CARTESIAN_POINT('',(0.387081172575526,0.700120108151134,0.49));
#72742=CARTESIAN_POINT('',(0.39,0.675499814951862,0.0499999999999999));
#72743=CARTESIAN_POINT('Origin',(0.419424404596921,0.711972647635046,0.0499999999999999));
#72744=CARTESIAN_POINT('Origin',(0.,0.,0.0499999999999999));
#72745=CARTESIAN_POINT('Origin',(0.188958885648847,0.818470854419598,0.95));
#72746=CARTESIAN_POINT('',(0.15350714952449,0.785134100039519,0.0499999999999999));
#72747=CARTESIAN_POINT('',(0.15350714952449,0.785134100039519,0.95));
#72748=CARTESIAN_POINT('',(0.15350714952449,0.785134100039519,0.49));
#72749=CARTESIAN_POINT('',(0.135445578580206,0.768150047349522,0.0499999999999999));
#72750=CARTESIAN_POINT('',(0.188958885648847,0.818470854419598,0.0499999999999999));
#72751=CARTESIAN_POINT('',(0.135445578580206,0.768150047349522,0.95));
#72752=CARTESIAN_POINT('',(0.135445578580206,0.768150047349522,0.95));
#72753=CARTESIAN_POINT('',(0.188958885648847,0.818470854419598,0.95));
#72754=CARTESIAN_POINT('Origin',(0.145664567054585,0.800944407364116,0.95));
#72755=CARTESIAN_POINT('',(0.124282141779344,0.790287257416402,0.95));
#72756=CARTESIAN_POINT('Origin',(0.,0.,0.95));
#72757=CARTESIAN_POINT('',(0.135445578580206,0.768150047349522,0.95));
#72758=CARTESIAN_POINT('Origin',(0.135445578580206,0.768150047349522,0.95));
#72759=CARTESIAN_POINT('',(0.124282141779344,0.790287257416402,0.0499999999999999));
#72760=CARTESIAN_POINT('',(0.124282141779344,0.790287257416402,0.49));
#72761=CARTESIAN_POINT('',(0.135445578580206,0.768150047349522,0.0499999999999999));
#72762=CARTESIAN_POINT('Origin',(0.145664567054585,0.800944407364116,0.0499999999999999));
#72763=CARTESIAN_POINT('Origin',(0.,0.,0.0499999999999999));
#72764=CARTESIAN_POINT('Origin',(-0.102370248460324,0.833738767378711,0.95));
#72765=CARTESIAN_POINT('',(-0.124282141779344,0.790287257416403,0.0499999999999999));
#72766=CARTESIAN_POINT('',(-0.124282141779344,0.790287257416403,0.95));
#72767=CARTESIAN_POINT('',(-0.124282141779344,0.790287257416403,0.49));
#72768=CARTESIAN_POINT('',(-0.135445578580206,0.768150047349522,0.0499999999999999));
#72769=CARTESIAN_POINT('',(-0.102370248460324,0.833738767378711,0.0499999999999999));
#72770=CARTESIAN_POINT('',(-0.135445578580206,0.768150047349522,0.95));
#72771=CARTESIAN_POINT('',(-0.135445578580206,0.768150047349522,0.95));
#72772=CARTESIAN_POINT('',(-0.102370248460324,0.833738767378711,0.95));
#72773=CARTESIAN_POINT('Origin',(-0.145664567054585,0.800944407364116,0.95));
#72774=CARTESIAN_POINT('',(-0.15350714952449,0.785134100039519,0.95));
#72775=CARTESIAN_POINT('Origin',(0.,0.,0.95));
#72776=CARTESIAN_POINT('',(-0.135445578580206,0.768150047349522,0.95));
#72777=CARTESIAN_POINT('Origin',(-0.135445578580206,0.768150047349522,0.95));
#72778=CARTESIAN_POINT('',(-0.15350714952449,0.785134100039519,0.0499999999999999));
#72779=CARTESIAN_POINT('',(-0.15350714952449,0.785134100039519,0.49));
#72780=CARTESIAN_POINT('',(-0.135445578580206,0.768150047349522,0.0499999999999999));
#72781=CARTESIAN_POINT('Origin',(-0.145664567054585,0.800944407364116,0.0499999999999999));
#72782=CARTESIAN_POINT('Origin',(0.,0.,0.0499999999999999));
#72783=CARTESIAN_POINT('Origin',(-0.381352019781219,0.748445480318229,0.95));
#72784=CARTESIAN_POINT('',(-0.387081172575525,0.700120108151135,0.0499999999999999));
#72785=CARTESIAN_POINT('',(-0.387081172575525,0.700120108151135,0.95));
#72786=CARTESIAN_POINT('',(-0.387081172575525,0.700120108151135,0.49));
#72787=CARTESIAN_POINT('',(-0.39,0.675499814951862,0.0499999999999999));
#72788=CARTESIAN_POINT('',(-0.381352019781219,0.748445480318229,0.0499999999999999));
#72789=CARTESIAN_POINT('',(-0.39,0.675499814951862,0.95));
#72790=CARTESIAN_POINT('',(-0.39,0.675499814951862,0.95));
#72791=CARTESIAN_POINT('',(-0.381352019781219,0.748445480318229,0.95));
#72792=CARTESIAN_POINT('Origin',(-0.419424404596921,0.711972647635046,0.95));
#72793=CARTESIAN_POINT('',(-0.412781213071428,0.685282182852641,0.95));
#72794=CARTESIAN_POINT('Origin',(0.,0.,0.95));
#72795=CARTESIAN_POINT('',(-0.39,0.675499814951862,0.95));
#72796=CARTESIAN_POINT('Origin',(-0.39,0.675499814951862,0.95));
#72797=CARTESIAN_POINT('',(-0.412781213071428,0.685282182852641,0.0499999999999999));
#72798=CARTESIAN_POINT('',(-0.412781213071428,0.685282182852641,0.49));
#72799=CARTESIAN_POINT('',(-0.39,0.675499814951862,0.0499999999999999));
#72800=CARTESIAN_POINT('Origin',(-0.419424404596921,0.711972647635046,0.0499999999999999));
#72801=CARTESIAN_POINT('Origin',(0.,0.,0.0499999999999999));
#72802=CARTESIAN_POINT('Origin',(-0.614337109360103,0.572878622452499,0.95));
#72803=CARTESIAN_POINT('',(-0.603192501249412,0.525508141170504,0.0499999999999999));
#72804=CARTESIAN_POINT('',(-0.603192501249412,0.525508141170504,0.95));
#72805=CARTESIAN_POINT('',(-0.603192501249412,0.525508141170504,0.49));
#72806=CARTESIAN_POINT('',(-0.597514665632803,0.501374335555501,0.0499999999999999));
#72807=CARTESIAN_POINT('',(-0.614337109360103,0.572878622452499,0.0499999999999999));
#72808=CARTESIAN_POINT('',(-0.597514665632803,0.501374335555501,0.95));
#72809=CARTESIAN_POINT('',(-0.597514665632803,0.501374335555501,0.95));
#72810=CARTESIAN_POINT('',(-0.614337109360103,0.572878622452499,0.95));
#72811=CARTESIAN_POINT('Origin',(-0.634184247036264,0.537126479004,0.95));
#72812=CARTESIAN_POINT('',(-0.622267770320064,0.502775120725853,0.95));
#72813=CARTESIAN_POINT('Origin',(0.,0.,0.95));
#72814=CARTESIAN_POINT('',(-0.597514665632803,0.501374335555501,0.95));
#72815=CARTESIAN_POINT('Origin',(-0.597514665632803,0.501374335555501,0.95));
#72816=CARTESIAN_POINT('',(-0.622267770320064,0.502775120725853,0.0499999999999999));
#72817=CARTESIAN_POINT('',(-0.622267770320064,0.502775120725853,0.49));
#72818=CARTESIAN_POINT('',(-0.597514665632803,0.501374335555501,0.0499999999999999));
#72819=CARTESIAN_POINT('Origin',(-0.634184247036264,0.537126479004,0.0499999999999999));
#72820=CARTESIAN_POINT('Origin',(0.,0.,0.0499999999999999));
#72821=CARTESIAN_POINT('Origin',(-0.77322407690005,0.32821414793099,0.95));
#72822=CARTESIAN_POINT('',(-0.746549912099409,0.28751213669055,0.0499999999999999));
#72823=CARTESIAN_POINT('',(-0.746549912099409,0.28751213669055,0.95));
#72824=CARTESIAN_POINT('',(-0.746549912099409,0.28751213669055,0.49));
#72825=CARTESIAN_POINT('',(-0.732960244213009,0.266775711794022,0.0499999999999999));
#72826=CARTESIAN_POINT('',(-0.77322407690005,0.32821414793099,0.0499999999999999));
#72827=CARTESIAN_POINT('',(-0.732960244213009,0.266775711794022,0.95));
#72828=CARTESIAN_POINT('',(-0.732960244213009,0.266775711794022,0.95));
#72829=CARTESIAN_POINT('',(-0.77322407690005,0.32821414793099,0.95));
#72830=CARTESIAN_POINT('Origin',(-0.768128119610979,0.286903189949044,0.95));
#72831=CARTESIAN_POINT('',(-0.756699650773901,0.259625958869015,0.95));
#72832=CARTESIAN_POINT('Origin',(0.,0.,0.95));
#72833=CARTESIAN_POINT('',(-0.732960244213009,0.266775711794022,0.95));
#72834=CARTESIAN_POINT('Origin',(-0.732960244213009,0.266775711794022,0.95));
#72835=CARTESIAN_POINT('',(-0.756699650773901,0.259625958869015,0.0499999999999999));
#72836=CARTESIAN_POINT('',(-0.756699650773901,0.259625958869015,0.49));
#72837=CARTESIAN_POINT('',(-0.732960244213009,0.266775711794022,0.0499999999999999));
#72838=CARTESIAN_POINT('Origin',(-0.768128119610979,0.286903189949044,0.0499999999999999));
#72839=CARTESIAN_POINT('Origin',(0.,0.,0.0499999999999999));
#72840=CARTESIAN_POINT('Origin',(0.809424404596921,0.,0.95));
#72841=CARTESIAN_POINT('',(0.799862385646954,-0.0148379252984939,0.95));
#72842=CARTESIAN_POINT('',(0.799862385646954,0.0148379252984938,0.95));
#72843=CARTESIAN_POINT('Origin',(0.,0.,0.95));
#72844=CARTESIAN_POINT('',(0.78,0.,0.95));
#72845=CARTESIAN_POINT('',(0.838848809193842,-0.0439622032440728,0.95));
#72846=CARTESIAN_POINT('',(0.78,0.,0.95));
#72847=CARTESIAN_POINT('Origin',(0.838848809193842,-0.0439622032440728,
0.95));
#72848=CARTESIAN_POINT('',(0.799862385646954,-0.0148379252984939,0.0499999999999999));
#72849=CARTESIAN_POINT('',(0.799862385646954,-0.0148379252984938,0.49));
#72850=CARTESIAN_POINT('',(0.78,0.,0.0499999999999999));
#72851=CARTESIAN_POINT('',(0.838848809193842,-0.0439622032440728,0.0499999999999999));
#72852=CARTESIAN_POINT('',(0.78,0.,0.95));
#72853=CARTESIAN_POINT('Origin',(0.78,0.,0.95));
#72854=CARTESIAN_POINT('',(0.799862385646954,0.0148379252984938,0.0499999999999999));
#72855=CARTESIAN_POINT('',(0.799862385646954,0.0148379252984938,0.49));
#72856=CARTESIAN_POINT('',(0.78,0.,0.0499999999999999));
#72857=CARTESIAN_POINT('Origin',(0.809424404596921,0.,0.0499999999999999));
#72858=CARTESIAN_POINT('Origin',(0.,0.,0.0499999999999999));
#72859=CARTESIAN_POINT('Origin',(-0.833738767378711,-0.102370248460324,
0.95));
#72860=CARTESIAN_POINT('',(-0.790287257416402,-0.124282141779344,0.0499999999999999));
#72861=CARTESIAN_POINT('',(-0.790287257416402,-0.124282141779344,0.95));
#72862=CARTESIAN_POINT('',(-0.790287257416402,-0.124282141779344,0.49));
#72863=CARTESIAN_POINT('',(-0.768150047349522,-0.135445578580206,0.0499999999999999));
#72864=CARTESIAN_POINT('',(-0.833738767378711,-0.102370248460324,0.0499999999999999));
#72865=CARTESIAN_POINT('',(-0.768150047349522,-0.135445578580206,0.95));
#72866=CARTESIAN_POINT('',(-0.768150047349522,-0.135445578580206,0.95));
#72867=CARTESIAN_POINT('',(-0.833738767378711,-0.102370248460324,0.95));
#72868=CARTESIAN_POINT('Origin',(-0.800944407364116,-0.145664567054585,
0.95));
#72869=CARTESIAN_POINT('',(-0.785134100039519,-0.15350714952449,0.95));
#72870=CARTESIAN_POINT('Origin',(0.,0.,0.95));
#72871=CARTESIAN_POINT('',(-0.768150047349522,-0.135445578580206,0.95));
#72872=CARTESIAN_POINT('Origin',(-0.768150047349522,-0.135445578580206,
0.95));
#72873=CARTESIAN_POINT('',(-0.785134100039519,-0.15350714952449,0.0499999999999999));
#72874=CARTESIAN_POINT('',(-0.785134100039519,-0.15350714952449,0.49));
#72875=CARTESIAN_POINT('',(-0.768150047349522,-0.135445578580206,0.0499999999999999));
#72876=CARTESIAN_POINT('Origin',(-0.800944407364116,-0.145664567054585,
0.0499999999999999));
#72877=CARTESIAN_POINT('Origin',(0.,0.,0.0499999999999999));
#72878=CARTESIAN_POINT('Origin',(-0.748445480318229,-0.381352019781219,
0.95));
#72879=CARTESIAN_POINT('',(-0.700120108151134,-0.387081172575526,0.0499999999999999));
#72880=CARTESIAN_POINT('',(-0.700120108151134,-0.387081172575526,0.95));
#72881=CARTESIAN_POINT('',(-0.700120108151134,-0.387081172575526,0.49));
#72882=CARTESIAN_POINT('',(-0.675499814951862,-0.39,0.0499999999999999));
#72883=CARTESIAN_POINT('',(-0.748445480318229,-0.381352019781219,0.0499999999999999));
#72884=CARTESIAN_POINT('',(-0.675499814951862,-0.39,0.95));
#72885=CARTESIAN_POINT('',(-0.675499814951862,-0.39,0.95));
#72886=CARTESIAN_POINT('',(-0.748445480318229,-0.381352019781219,0.95));
#72887=CARTESIAN_POINT('Origin',(-0.711972647635046,-0.419424404596921,
0.95));
#72888=CARTESIAN_POINT('',(-0.685282182852641,-0.412781213071428,0.95));
#72889=CARTESIAN_POINT('Origin',(0.,0.,0.95));
#72890=CARTESIAN_POINT('',(-0.675499814951862,-0.39,0.95));
#72891=CARTESIAN_POINT('Origin',(-0.675499814951862,-0.39,0.95));
#72892=CARTESIAN_POINT('',(-0.685282182852641,-0.412781213071428,0.0499999999999999));
#72893=CARTESIAN_POINT('',(-0.685282182852641,-0.412781213071428,0.49));
#72894=CARTESIAN_POINT('',(-0.675499814951862,-0.39,0.0499999999999999));
#72895=CARTESIAN_POINT('Origin',(-0.711972647635046,-0.419424404596921,
0.0499999999999999));
#72896=CARTESIAN_POINT('Origin',(0.,0.,0.0499999999999999));
#72897=CARTESIAN_POINT('Origin',(-0.572878622452499,-0.614337109360103,
0.95));
#72898=CARTESIAN_POINT('',(-0.525508141170504,-0.603192501249412,0.0499999999999999));
#72899=CARTESIAN_POINT('',(-0.525508141170504,-0.603192501249412,0.95));
#72900=CARTESIAN_POINT('',(-0.525508141170504,-0.603192501249412,0.49));
#72901=CARTESIAN_POINT('',(-0.501374335555501,-0.597514665632803,0.0499999999999999));
#72902=CARTESIAN_POINT('',(-0.572878622452499,-0.614337109360103,0.0499999999999999));
#72903=CARTESIAN_POINT('',(-0.501374335555501,-0.597514665632803,0.95));
#72904=CARTESIAN_POINT('',(-0.501374335555501,-0.597514665632803,0.95));
#72905=CARTESIAN_POINT('',(-0.572878622452499,-0.614337109360103,0.95));
#72906=CARTESIAN_POINT('Origin',(-0.537126479004,-0.634184247036264,0.95));
#72907=CARTESIAN_POINT('',(-0.502775120725853,-0.622267770320064,0.95));
#72908=CARTESIAN_POINT('Origin',(0.,0.,0.95));
#72909=CARTESIAN_POINT('',(-0.501374335555501,-0.597514665632803,0.95));
#72910=CARTESIAN_POINT('Origin',(-0.501374335555501,-0.597514665632803,
0.95));
#72911=CARTESIAN_POINT('',(-0.502775120725853,-0.622267770320064,0.0499999999999999));
#72912=CARTESIAN_POINT('',(-0.502775120725853,-0.622267770320064,0.49));
#72913=CARTESIAN_POINT('',(-0.501374335555501,-0.597514665632803,0.0499999999999999));
#72914=CARTESIAN_POINT('Origin',(-0.537126479004,-0.634184247036264,0.0499999999999999));
#72915=CARTESIAN_POINT('Origin',(0.,0.,0.0499999999999999));
#72916=CARTESIAN_POINT('Origin',(-0.32821414793099,-0.77322407690005,0.95));
#72917=CARTESIAN_POINT('',(-0.28751213669055,-0.746549912099409,0.0499999999999999));
#72918=CARTESIAN_POINT('',(-0.28751213669055,-0.746549912099409,0.95));
#72919=CARTESIAN_POINT('',(-0.28751213669055,-0.746549912099409,0.49));
#72920=CARTESIAN_POINT('',(-0.266775711794021,-0.732960244213009,0.0499999999999999));
#72921=CARTESIAN_POINT('',(-0.32821414793099,-0.77322407690005,0.0499999999999999));
#72922=CARTESIAN_POINT('',(-0.266775711794021,-0.732960244213009,0.95));
#72923=CARTESIAN_POINT('',(-0.266775711794021,-0.732960244213009,0.95));
#72924=CARTESIAN_POINT('',(-0.32821414793099,-0.77322407690005,0.95));
#72925=CARTESIAN_POINT('Origin',(-0.286903189949045,-0.768128119610979,
0.95));
#72926=CARTESIAN_POINT('',(-0.259625958869015,-0.756699650773902,0.95));
#72927=CARTESIAN_POINT('Origin',(0.,0.,0.95));
#72928=CARTESIAN_POINT('',(-0.266775711794021,-0.732960244213009,0.95));
#72929=CARTESIAN_POINT('Origin',(-0.266775711794021,-0.732960244213009,
0.95));
#72930=CARTESIAN_POINT('',(-0.259625958869015,-0.756699650773902,0.0499999999999999));
#72931=CARTESIAN_POINT('',(-0.259625958869015,-0.756699650773902,0.49));
#72932=CARTESIAN_POINT('',(-0.266775711794021,-0.732960244213009,0.0499999999999999));
#72933=CARTESIAN_POINT('Origin',(-0.286903189949045,-0.768128119610979,
0.0499999999999999));
#72934=CARTESIAN_POINT('Origin',(0.,0.,0.0499999999999999));
#72935=CARTESIAN_POINT('Origin',(-0.0439622032440732,-0.838848809193842,
0.95));
#72936=CARTESIAN_POINT('',(-0.014837925298494,-0.799862385646954,0.0499999999999999));
#72937=CARTESIAN_POINT('',(-0.014837925298494,-0.799862385646954,0.95));
#72938=CARTESIAN_POINT('',(-0.0148379252984941,-0.799862385646954,0.49));
#72939=CARTESIAN_POINT('',(-1.4328367550024E-16,-0.78,0.0499999999999999));
#72940=CARTESIAN_POINT('',(-0.0439622032440732,-0.838848809193842,0.0499999999999999));
#72941=CARTESIAN_POINT('',(-1.4328367550024E-16,-0.78,0.95));
#72942=CARTESIAN_POINT('',(-1.4328367550024E-16,-0.78,0.95));
#72943=CARTESIAN_POINT('',(-0.0439622032440732,-0.838848809193842,0.95));
#72944=CARTESIAN_POINT('Origin',(-1.52655665885959E-16,-0.809424404596921,
0.95));
#72945=CARTESIAN_POINT('',(0.0148379252984936,-0.799862385646954,0.95));
#72946=CARTESIAN_POINT('Origin',(0.,0.,0.95));
#72947=CARTESIAN_POINT('',(-1.4328367550024E-16,-0.78,0.95));
#72948=CARTESIAN_POINT('Origin',(-1.4328367550024E-16,-0.78,0.95));
#72949=CARTESIAN_POINT('',(0.0148379252984936,-0.799862385646954,0.0499999999999999));
#72950=CARTESIAN_POINT('',(0.0148379252984936,-0.799862385646954,0.49));
#72951=CARTESIAN_POINT('',(-1.4328367550024E-16,-0.78,0.0499999999999999));
#72952=CARTESIAN_POINT('Origin',(-1.52655665885959E-16,-0.809424404596921,
0.0499999999999999));
#72953=CARTESIAN_POINT('Origin',(0.,0.,0.0499999999999999));
#72954=CARTESIAN_POINT('Origin',(0.245592231967099,-0.80329599500895,0.95));
#72955=CARTESIAN_POINT('',(0.259625958869016,-0.756699650773901,0.0499999999999999));
#72956=CARTESIAN_POINT('',(0.259625958869016,-0.756699650773901,0.95));
#72957=CARTESIAN_POINT('',(0.259625958869016,-0.756699650773901,0.49));
#72958=CARTESIAN_POINT('',(0.266775711794022,-0.732960244213009,0.0499999999999999));
#72959=CARTESIAN_POINT('',(0.245592231967099,-0.80329599500895,0.0499999999999999));
#72960=CARTESIAN_POINT('',(0.266775711794022,-0.732960244213009,0.95));
#72961=CARTESIAN_POINT('',(0.266775711794022,-0.732960244213009,0.95));
#72962=CARTESIAN_POINT('',(0.245592231967099,-0.80329599500895,0.95));
#72963=CARTESIAN_POINT('Origin',(0.286903189949044,-0.768128119610979,0.95));
#72964=CARTESIAN_POINT('',(0.28751213669055,-0.746549912099409,0.95));
#72965=CARTESIAN_POINT('Origin',(0.,0.,0.95));
#72966=CARTESIAN_POINT('',(0.266775711794022,-0.732960244213009,0.95));
#72967=CARTESIAN_POINT('Origin',(0.266775711794022,-0.732960244213009,0.95));
#72968=CARTESIAN_POINT('',(0.28751213669055,-0.746549912099409,0.0499999999999999));
#72969=CARTESIAN_POINT('',(0.28751213669055,-0.746549912099409,0.49));
#72970=CARTESIAN_POINT('',(0.266775711794022,-0.732960244213009,0.0499999999999999));
#72971=CARTESIAN_POINT('Origin',(0.286903189949044,-0.768128119610979,0.0499999999999999));
#72972=CARTESIAN_POINT('Origin',(0.,0.,0.0499999999999999));
#72973=CARTESIAN_POINT('Origin',(0.50552461944772,-0.670853828439726,0.95));
#72974=CARTESIAN_POINT('',(0.502775120725853,-0.622267770320064,0.0499999999999999));
#72975=CARTESIAN_POINT('',(0.502775120725853,-0.622267770320064,0.95));
#72976=CARTESIAN_POINT('',(0.502775120725853,-0.622267770320064,0.49));
#72977=CARTESIAN_POINT('',(0.501374335555501,-0.597514665632803,0.0499999999999999));
#72978=CARTESIAN_POINT('',(0.50552461944772,-0.670853828439726,0.0499999999999999));
#72979=CARTESIAN_POINT('',(0.501374335555501,-0.597514665632803,0.95));
#72980=CARTESIAN_POINT('',(0.501374335555501,-0.597514665632803,0.95));
#72981=CARTESIAN_POINT('',(0.50552461944772,-0.670853828439726,0.95));
#72982=CARTESIAN_POINT('Origin',(0.537126479004,-0.634184247036265,0.95));
#72983=CARTESIAN_POINT('',(0.525508141170504,-0.603192501249412,0.95));
#72984=CARTESIAN_POINT('Origin',(0.,0.,0.95));
#72985=CARTESIAN_POINT('',(0.501374335555501,-0.597514665632803,0.95));
#72986=CARTESIAN_POINT('Origin',(0.501374335555501,-0.597514665632803,0.95));
#72987=CARTESIAN_POINT('',(0.525508141170504,-0.603192501249412,0.0499999999999999));
#72988=CARTESIAN_POINT('',(0.525508141170504,-0.603192501249412,0.49));
#72989=CARTESIAN_POINT('',(0.501374335555501,-0.597514665632803,0.0499999999999999));
#72990=CARTESIAN_POINT('Origin',(0.537126479004,-0.634184247036265,0.0499999999999999));
#72991=CARTESIAN_POINT('Origin',(0.,0.,0.0499999999999999));
#72992=CARTESIAN_POINT('Origin',(0.704483277074156,-0.457496789412623,0.95));
#72993=CARTESIAN_POINT('',(0.685282182852641,-0.412781213071429,0.0499999999999999));
#72994=CARTESIAN_POINT('',(0.685282182852641,-0.412781213071429,0.95));
#72995=CARTESIAN_POINT('',(0.685282182852641,-0.412781213071429,0.49));
#72996=CARTESIAN_POINT('',(0.675499814951862,-0.39,0.0499999999999999));
#72997=CARTESIAN_POINT('',(0.704483277074156,-0.457496789412623,0.0499999999999999));
#72998=CARTESIAN_POINT('',(0.675499814951862,-0.39,0.95));
#72999=CARTESIAN_POINT('',(0.675499814951862,-0.39,0.95));
#73000=CARTESIAN_POINT('',(0.704483277074156,-0.457496789412623,0.95));
#73001=CARTESIAN_POINT('Origin',(0.711972647635045,-0.419424404596921,0.95));
#73002=CARTESIAN_POINT('',(0.700120108151134,-0.387081172575526,0.95));
#73003=CARTESIAN_POINT('Origin',(0.,0.,0.95));
#73004=CARTESIAN_POINT('',(0.675499814951862,-0.39,0.95));
#73005=CARTESIAN_POINT('Origin',(0.675499814951862,-0.39,0.95));
#73006=CARTESIAN_POINT('',(0.700120108151134,-0.387081172575526,0.0499999999999999));
#73007=CARTESIAN_POINT('',(0.700120108151134,-0.387081172575526,0.49));
#73008=CARTESIAN_POINT('',(0.675499814951862,-0.39,0.0499999999999999));
#73009=CARTESIAN_POINT('Origin',(0.711972647635045,-0.419424404596921,0.0499999999999999));
#73010=CARTESIAN_POINT('Origin',(0.,0.,0.0499999999999999));
#73011=CARTESIAN_POINT('Origin',(0.818470854419598,-0.188958885648847,0.95));
#73012=CARTESIAN_POINT('',(0.785134100039519,-0.15350714952449,0.0499999999999999));
#73013=CARTESIAN_POINT('',(0.785134100039519,-0.15350714952449,0.95));
#73014=CARTESIAN_POINT('',(0.785134100039519,-0.15350714952449,0.49));
#73015=CARTESIAN_POINT('',(0.768150047349522,-0.135445578580206,0.0499999999999999));
#73016=CARTESIAN_POINT('',(0.818470854419598,-0.188958885648847,0.0499999999999999));
#73017=CARTESIAN_POINT('',(0.768150047349522,-0.135445578580206,0.95));
#73018=CARTESIAN_POINT('',(0.768150047349522,-0.135445578580206,0.95));
#73019=CARTESIAN_POINT('',(0.818470854419598,-0.188958885648847,0.95));
#73020=CARTESIAN_POINT('Origin',(0.800944407364116,-0.145664567054585,0.95));
#73021=CARTESIAN_POINT('',(0.790287257416402,-0.124282141779344,0.95));
#73022=CARTESIAN_POINT('Origin',(0.,0.,0.95));
#73023=CARTESIAN_POINT('',(0.768150047349522,-0.135445578580206,0.95));
#73024=CARTESIAN_POINT('Origin',(0.768150047349522,-0.135445578580206,0.95));
#73025=CARTESIAN_POINT('',(0.790287257416402,-0.124282141779344,0.0499999999999999));
#73026=CARTESIAN_POINT('',(0.790287257416402,-0.124282141779344,0.49));
#73027=CARTESIAN_POINT('',(0.768150047349522,-0.135445578580206,0.0499999999999999));
#73028=CARTESIAN_POINT('Origin',(0.800944407364116,-0.145664567054585,0.0499999999999999));
#73029=CARTESIAN_POINT('Origin',(0.,0.,0.0499999999999999));
#73030=CARTESIAN_POINT('Origin',(0.45,0.,-3.5));
#73031=CARTESIAN_POINT('',(-0.45,-5.51091059616309E-17,-3.5));
#73032=CARTESIAN_POINT('Origin',(0.,0.,-3.5));
#73033=CARTESIAN_POINT('Origin',(0.,0.,-3.475));
#73034=CARTESIAN_POINT('',(-0.475,-5.81707229594993E-17,-3.475));
#73035=CARTESIAN_POINT('Origin',(0.,0.,0.015));
#73036=CARTESIAN_POINT('',(-0.8,-9.79717439317883E-17,0.03));
#73037=CARTESIAN_POINT('Origin',(0.,0.,0.03));
#73038=CARTESIAN_POINT('',(-0.785,-9.61347737330672E-17,0.015));
#73039=CARTESIAN_POINT('Origin',(0.,0.,0.49));
#73040=CARTESIAN_POINT('Origin',(0.,0.,0.95));
#73041=CARTESIAN_POINT('Origin',(0.,0.,0.95));
#73042=CARTESIAN_POINT('Origin',(0.,0.,0.95));
#73043=CARTESIAN_POINT('Origin',(0.,0.,0.95));
#73044=CARTESIAN_POINT('Origin',(0.,0.,0.95));
#73045=CARTESIAN_POINT('Origin',(0.,0.,0.95));
#73046=CARTESIAN_POINT('Origin',(0.,0.,0.95));
#73047=CARTESIAN_POINT('Origin',(0.,0.,0.95));
#73048=CARTESIAN_POINT('Origin',(0.,0.,0.95));
#73049=CARTESIAN_POINT('Origin',(0.,0.,0.95));
#73050=CARTESIAN_POINT('Origin',(0.,0.,0.95));
#73051=CARTESIAN_POINT('Origin',(0.,0.,0.95));
#73052=CARTESIAN_POINT('Origin',(0.,0.,0.95));
#73053=CARTESIAN_POINT('Origin',(0.,0.,0.95));
#73054=CARTESIAN_POINT('Origin',(0.,0.,0.95));
#73055=CARTESIAN_POINT('Origin',(0.,0.,0.95));
#73056=CARTESIAN_POINT('',(-0.8,-9.79717439317883E-17,0.49));
#73057=CARTESIAN_POINT('Origin',(0.,0.,0.95));
#73058=CARTESIAN_POINT('Origin',(0.,0.,0.95));
#73059=CARTESIAN_POINT('Origin',(0.,0.,0.95));
#73060=CARTESIAN_POINT('Origin',(0.,0.,0.95));
#73061=CARTESIAN_POINT('Origin',(0.,0.,0.95));
#73062=CARTESIAN_POINT('Origin',(0.,0.,0.95));
#73063=CARTESIAN_POINT('Origin',(0.,0.,0.95));
#73064=CARTESIAN_POINT('Origin',(0.,0.,0.95));
#73065=CARTESIAN_POINT('Origin',(0.,0.,0.95));
#73066=CARTESIAN_POINT('Origin',(0.,0.,0.95));
#73067=CARTESIAN_POINT('Origin',(0.,0.,0.95));
#73068=CARTESIAN_POINT('Origin',(0.,0.,0.95));
#73069=CARTESIAN_POINT('Origin',(0.,0.,0.95));
#73070=CARTESIAN_POINT('Origin',(0.,0.,0.95));
#73071=CARTESIAN_POINT('Origin',(0.,0.,0.95));
#73072=CARTESIAN_POINT('Origin',(0.,0.,0.95));
#73073=CARTESIAN_POINT('Origin',(0.,0.,0.95));
#73074=CARTESIAN_POINT('Origin',(0.,0.,0.95));
#73075=CARTESIAN_POINT('Origin',(0.,0.,0.95));
#73076=CARTESIAN_POINT('Origin',(0.,0.,0.95));
#73077=CARTESIAN_POINT('Origin',(0.,0.,0.975));
#73078=CARTESIAN_POINT('',(-0.75,-9.18485099360515E-17,1.));
#73079=CARTESIAN_POINT('Origin',(0.,0.,1.));
#73080=CARTESIAN_POINT('',(-0.775,-9.49101269339199E-17,0.975));
#73081=CARTESIAN_POINT('Origin',(0.,0.,1.));
#73082=CARTESIAN_POINT('',(0.,0.,0.));
#73083=CARTESIAN_POINT('Origin',(0.,0.,-0.975));
#73084=CARTESIAN_POINT('',(-0.294526041752932,0.000202016893245491,-1.92358238829104));
#73085=CARTESIAN_POINT('',(-0.294462282070766,0.000314061004039186,-1.93801761170896));
#73086=CARTESIAN_POINT('',(-0.2942,-3.60291088309151E-17,-0.975));
#73087=CARTESIAN_POINT('',(0.129046731032871,0.264647125805703,-1.9558));
#73088=CARTESIAN_POINT('Ctrl Pts',(-0.294526041752932,0.000202016893245491,
-1.92358238829104));
#73089=CARTESIAN_POINT('Ctrl Pts',(-0.294606382001833,0.0112270322590358,
-1.9241807531942));
#73090=CARTESIAN_POINT('Ctrl Pts',(-0.294040815978278,0.0222432322455178,
-1.92477911809736));
#73091=CARTESIAN_POINT('Ctrl Pts',(-0.292801839103187,0.0331825365608063,
-1.92537748300052));
#73092=CARTESIAN_POINT('Ctrl Pts',(-0.281871479166624,0.129690014646629,
-1.93065630934219));
#73093=CARTESIAN_POINT('Ctrl Pts',(-0.218530096272678,0.220212764718254,
-1.93593513568386));
#73094=CARTESIAN_POINT('Ctrl Pts',(-0.131611395378181,0.263625056394311,
-1.94121396202553));
#73095=CARTESIAN_POINT('Ctrl Pts',(-0.0515557548574951,0.303609533622244,
-1.94607597468368));
#73096=CARTESIAN_POINT('Ctrl Pts',(0.0485008907872385,0.303629477151138,
-1.95093798734184));
#73097=CARTESIAN_POINT('Ctrl Pts',(0.129201276660417,0.264831693691691,
-1.9558));
#73098=CARTESIAN_POINT('',(-0.128892185405329,0.264462557919714,-1.9558));
#73099=CARTESIAN_POINT('Origin',(0.,0.,-1.9558));
#73100=CARTESIAN_POINT('Ctrl Pts',(-0.128892185405329,0.264462557919714,
-1.9558));
#73101=CARTESIAN_POINT('Ctrl Pts',(-0.216608714343133,0.221711798795636,
-1.95052117365833));
#73102=CARTESIAN_POINT('Ctrl Pts',(-0.280643579713015,0.13227595083354,
-1.94524234731666));
#73103=CARTESIAN_POINT('Ctrl Pts',(-0.292444290812177,0.0360181640441311,
-1.93996352097499));
#73104=CARTESIAN_POINT('Ctrl Pts',(-0.29389430460864,0.0241904769082657,
-1.93931488455298));
#73105=CARTESIAN_POINT('Ctrl Pts',(-0.294555671724416,0.0122597901261511,
-1.93866624813097));
#73106=CARTESIAN_POINT('Ctrl Pts',(-0.294462282070766,0.000314061004039186,
-1.93801761170896));
#73107=CARTESIAN_POINT('Origin',(0.,0.,-0.975));
#73108=CARTESIAN_POINT('',(-0.29376368569052,0.000111582411140523,-1.82358238829104));
#73109=CARTESIAN_POINT('',(-0.293753041170369,9.93547412011704E-5,-1.83801761170896));
#73110=CARTESIAN_POINT('',(-0.2942,-3.60291088309151E-17,-0.975));
#73111=CARTESIAN_POINT('Ctrl Pts',(-0.29376368569052,0.000111582411140523,
-1.82358238829104));
#73112=CARTESIAN_POINT('Ctrl Pts',(-0.293906879889716,0.0420094747863047,
-1.82584112847753));
#73113=CARTESIAN_POINT('Ctrl Pts',(-0.285536454078649,0.0838527133558878,
-1.82809986866401));
#73114=CARTESIAN_POINT('Ctrl Pts',(-0.268369615014717,0.121706567466693,
-1.8303586088505));
#73115=CARTESIAN_POINT('Ctrl Pts',(-0.22824956809826,0.210173547161576,
-1.83563743519216));
#73116=CARTESIAN_POINT('Ctrl Pts',(-0.140084563281704,0.276850985726518,
-1.84091626153383));
#73117=CARTESIAN_POINT('Ctrl Pts',(-0.0440357056638973,0.291367766871805,
-1.8461950878755));
#73118=CARTESIAN_POINT('Ctrl Pts',(0.0520131519539096,0.305884548017093,
-1.85147391421717));
#73119=CARTESIAN_POINT('Ctrl Pts',(0.155945862372967,0.268240671742726,
-1.85675274055884));
#73120=CARTESIAN_POINT('Ctrl Pts',(0.220417510035407,0.195579651961848,
-1.8620315669005));
#73121=CARTESIAN_POINT('Ctrl Pts',(0.284889157697847,0.122918632180969,
-1.86731039324217));
#73122=CARTESIAN_POINT('Ctrl Pts',(0.30989974260367,0.0152404688935781,
-1.87258921958384));
#73123=CARTESIAN_POINT('Ctrl Pts',(0.284057777716934,-0.0783963834015649,
-1.87786804592551));
#73124=CARTESIAN_POINT('Ctrl Pts',(0.258215812830198,-0.172033235696708,
-1.88314687226718));
#73125=CARTESIAN_POINT('Ctrl Pts',(0.181521298150903,-0.251628776999603,
-1.88842569860885));
#73126=CARTESIAN_POINT('Ctrl Pts',(0.0889077647329698,-0.280940720221476,
-1.89370452495051));
#73127=CARTESIAN_POINT('Ctrl Pts',(-0.00370576868496414,-0.31025266344335,
-1.89898335129218));
#73128=CARTESIAN_POINT('Ctrl Pts',(-0.112238320841537,-0.289281008584203,
-1.90426217763385));
#73129=CARTESIAN_POINT('Ctrl Pts',(-0.187244928430233,-0.227549078104619,
-1.90954100397552));
#73130=CARTESIAN_POINT('Ctrl Pts',(-0.253749395849641,-0.172814578154573,
-1.91422146541402));
#73131=CARTESIAN_POINT('Ctrl Pts',(-0.293897613456161,-0.086036596043438,
-1.91890192685253));
#73132=CARTESIAN_POINT('Ctrl Pts',(-0.294526041752932,0.000202016893245491,
-1.92358238829104));
#73133=CARTESIAN_POINT('Ctrl Pts',(-0.294462282070766,0.000314061004039186,
-1.93801761170896));
#73134=CARTESIAN_POINT('Ctrl Pts',(-0.293795634595768,-0.084958662955309,
-1.9333874217893));
#73135=CARTESIAN_POINT('Ctrl Pts',(-0.254669634955265,-0.170997883718377,
-1.92875723186965));
#73136=CARTESIAN_POINT('Ctrl Pts',(-0.189411438041069,-0.225809910607879,
-1.92412704194999));
#73137=CARTESIAN_POINT('Ctrl Pts',(-0.115011317342356,-0.288300472853751,
-1.91884821560832));
#73138=CARTESIAN_POINT('Ctrl Pts',(-0.00664451911648993,-0.310201871728771,
-1.91356938926666));
#73139=CARTESIAN_POINT('Ctrl Pts',(0.0862516754582108,-0.281745185228748,
-1.90829056292499));
#73140=CARTESIAN_POINT('Ctrl Pts',(0.179147870032911,-0.253288498728725,
-1.90301173658332));
#73141=CARTESIAN_POINT('Ctrl Pts',(0.256573460956447,-0.17447372685366,
-1.89773291024165));
#73142=CARTESIAN_POINT('Ctrl Pts',(0.283296849325839,-0.081098014509368,
-1.89245408389998));
#73143=CARTESIAN_POINT('Ctrl Pts',(0.310020237695232,0.0122776978349239,
-1.88717525755831));
#73144=CARTESIAN_POINT('Ctrl Pts',(0.286041423510481,0.120214350648442,
-1.88189643121665));
#73145=CARTESIAN_POINT('Ctrl Pts',(0.222263652174004,0.193489302525945,
-1.87661760487498));
#73146=CARTESIAN_POINT('Ctrl Pts',(0.158485880837528,0.266764254403448,
-1.87133877853331));
#73147=CARTESIAN_POINT('Ctrl Pts',(0.0549091523493268,0.305377505344936,
-1.86605995219164));
#73148=CARTESIAN_POINT('Ctrl Pts',(-0.0412742315316208,0.291768235340026,
-1.86078112584997));
#73149=CARTESIAN_POINT('Ctrl Pts',(-0.137457615412569,0.278158965335116,
-1.85550229950831));
#73150=CARTESIAN_POINT('Ctrl Pts',(-0.226247654686263,0.212327174383808,
-1.85022347316664));
#73151=CARTESIAN_POINT('Ctrl Pts',(-0.267203521977581,0.124246060006099,
-1.84494464682497));
#73152=CARTESIAN_POINT('Ctrl Pts',(-0.285118030024829,0.0857184951737815,
-1.84263563511963));
#73153=CARTESIAN_POINT('Ctrl Pts',(-0.293880542962884,0.0429340217185596,
-1.8403266234143));
#73154=CARTESIAN_POINT('Ctrl Pts',(-0.293753041170369,9.93547412011704E-5,
-1.83801761170896));
#73155=CARTESIAN_POINT('Origin',(0.,0.,-0.975));
#73156=CARTESIAN_POINT('',(-0.294128475609455,-0.000264102212364226,-1.72358238829104));
#73157=CARTESIAN_POINT('',(-0.294155870929176,-0.000265231913958952,-1.73801761170896));
#73158=CARTESIAN_POINT('',(-0.2942,-3.60291088309151E-17,-0.975));
#73159=CARTESIAN_POINT('Ctrl Pts',(-0.294128475609455,-0.000264102212364226,
-1.72358238829104));
#73160=CARTESIAN_POINT('Ctrl Pts',(-0.293485479046885,0.0722049969462197,
-1.72750150376085));
#73161=CARTESIAN_POINT('Ctrl Pts',(-0.266422153164402,0.1451034209213,-1.73142061923066));
#73162=CARTESIAN_POINT('Ctrl Pts',(-0.217860899240002,0.198422075695203,
-1.73533973470047));
#73163=CARTESIAN_POINT('Ctrl Pts',(-0.15245164340784,0.270239280748482,
-1.74061856104214));
#73164=CARTESIAN_POINT('Ctrl Pts',(-0.0480396369288832,0.306533766850134,
-1.74589738738381));
#73165=CARTESIAN_POINT('Ctrl Pts',(0.0478126679033099,0.290772471240934,
-1.75117621372547));
#73166=CARTESIAN_POINT('Ctrl Pts',(0.143664972735503,0.275011175631734,
-1.75645504006714));
#73167=CARTESIAN_POINT('Ctrl Pts',(0.230957575920933,0.207194098311682,
-1.76173386640881));
#73168=CARTESIAN_POINT('Ctrl Pts',(0.269926346425774,0.118213643233769,
-1.76701269275048));
#73169=CARTESIAN_POINT('Ctrl Pts',(0.308895116930614,0.0292331881558552,
-1.77229151909215));
#73170=CARTESIAN_POINT('Ctrl Pts',(0.299540054754865,-0.0809106446799193,
-1.77757034543381));
#73171=CARTESIAN_POINT('Ctrl Pts',(0.246122671812768,-0.162044226057869,
-1.78284917177548));
#73172=CARTESIAN_POINT('Ctrl Pts',(0.192705288870672,-0.243177807435819,
-1.78812799811715));
#73173=CARTESIAN_POINT('Ctrl Pts',(0.0952255851622282,-0.295301137355943,
-1.79340682445882));
#73174=CARTESIAN_POINT('Ctrl Pts',(-0.00191188692827236,-0.294670966749634,
-1.79868565080049));
#73175=CARTESIAN_POINT('Ctrl Pts',(-0.0990493590187724,-0.294040796143324,
-1.80396447714215));
#73176=CARTESIAN_POINT('Ctrl Pts',(-0.195844599491329,-0.24065712501058,
-1.80924330348382));
#73177=CARTESIAN_POINT('Ctrl Pts',(-0.248204675219429,-0.158837029031797,
-1.81452212982549));
#73178=CARTESIAN_POINT('Ctrl Pts',(-0.278160564948661,-0.112026673265633,
-1.81754221598067));
#73179=CARTESIAN_POINT('Ctrl Pts',(-0.293572225503517,-0.055908691833193,
-1.82056230213586));
#73180=CARTESIAN_POINT('Ctrl Pts',(-0.29376368569052,0.000111582411140523,
-1.82358238829104));
#73181=CARTESIAN_POINT('Ctrl Pts',(-0.293753041170369,9.93547412011704E-5,
-1.83801761170896));
#73182=CARTESIAN_POINT('Ctrl Pts',(-0.293589050364825,-0.0549939220220992,
-1.83504779707263));
#73183=CARTESIAN_POINT('Ctrl Pts',(-0.278718574093716,-0.110170232427766,
-1.8320779824363));
#73184=CARTESIAN_POINT('Ctrl Pts',(-0.249699027023729,-0.156478964570943,
-1.82910816779997));
#73185=CARTESIAN_POINT('Ctrl Pts',(-0.198116969469617,-0.238792436966167,
-1.8238293414583));
#73186=CARTESIAN_POINT('Ctrl Pts',(-0.101831159052452,-0.293088943952504,
-1.81855051511663));
#73187=CARTESIAN_POINT('Ctrl Pts',(-0.00470384019102898,-0.294639071818577,
-1.81327168877496));
#73188=CARTESIAN_POINT('Ctrl Pts',(0.092423478670394,-0.29618919968465,
-1.80799286243329));
#73189=CARTESIAN_POINT('Ctrl Pts',(0.190392305976075,-0.244992948430459,
-1.80271403609162));
#73190=CARTESIAN_POINT('Ctrl Pts',(0.244575998013883,-0.164369434073953,
-1.79743520974996));
#73191=CARTESIAN_POINT('Ctrl Pts',(0.29875969005169,-0.0837459197174479,
-1.79215638340829));
#73192=CARTESIAN_POINT('Ctrl Pts',(0.309158246821627,0.0263048577413711,
-1.78687755706662));
#73193=CARTESIAN_POINT('Ctrl Pts',(0.271034440980663,0.115650703195309,
-1.78159873072495));
#73194=CARTESIAN_POINT('Ctrl Pts',(0.2329106351397,0.204996548649246,-1.77631990438328));
#73195=CARTESIAN_POINT('Ctrl Pts',(0.146264466687836,0.273637462098302,
-1.77104107804162));
#73196=CARTESIAN_POINT('Ctrl Pts',(0.0505657951064905,0.29030626034669,
-1.76576225169995));
#73197=CARTESIAN_POINT('Ctrl Pts',(-0.0451328764748552,0.306975058595079,
-1.76048342535828));
#73198=CARTESIAN_POINT('Ctrl Pts',(-0.149884051185683,0.2716717416428,-1.75520459901661));
#73199=CARTESIAN_POINT('Ctrl Pts',(-0.215970879562555,0.200477606298579,
-1.74992577267494));
#73200=CARTESIAN_POINT('Ctrl Pts',(-0.265664538664458,0.146943533341182,
-1.74595638568628));
#73201=CARTESIAN_POINT('Ctrl Pts',(-0.293496554389252,0.0731160286671296,
-1.74198699869762));
#73202=CARTESIAN_POINT('Ctrl Pts',(-0.294155870929176,-0.000265231913958952,
-1.73801761170896));
#73203=CARTESIAN_POINT('Origin',(0.,0.,-0.975));
#73204=CARTESIAN_POINT('',(-0.294635704950153,9.93244666355822E-5,-1.62358238829104));
#73205=CARTESIAN_POINT('',(-0.294621628357173,0.000114745350509935,-1.63801761170896));
#73206=CARTESIAN_POINT('',(-0.2942,-3.60291088309151E-17,-0.975));
#73207=CARTESIAN_POINT('Ctrl Pts',(-0.294635704950153,9.93244666355822E-5,
-1.62358238829104));
#73208=CARTESIAN_POINT('Ctrl Pts',(-0.29466007133164,0.00563415828093715,
-1.62388305270251));
#73209=CARTESIAN_POINT('Ctrl Pts',(-0.294517542364744,0.0111677125456974,
-1.62418371711397));
#73210=CARTESIAN_POINT('Ctrl Pts',(-0.294204148018538,0.016691572821619,
-1.62448438152544));
#73211=CARTESIAN_POINT('Ctrl Pts',(-0.288701819618525,0.113675113341228,
-1.62976320786711));
#73212=CARTESIAN_POINT('Ctrl Pts',(-0.230529314588497,0.207670429409272,
-1.63504203420877));
#73213=CARTESIAN_POINT('Ctrl Pts',(-0.146185764509842,0.255860140760567,
-1.64032086055044));
#73214=CARTESIAN_POINT('Ctrl Pts',(-0.0618422144311871,0.304049852111862,
-1.64559968689211));
#73215=CARTESIAN_POINT('Ctrl Pts',(0.0486723806960958,0.306433958746409,
-1.65087851323378));
#73216=CARTESIAN_POINT('Ctrl Pts',(0.135015667965605,0.261926437294344,
-1.65615733957545));
#73217=CARTESIAN_POINT('Ctrl Pts',(0.221358955235115,0.217418915842279,
-1.66143616591712));
#73218=CARTESIAN_POINT('Ctrl Pts',(0.283530934646851,0.126019766303602,
-1.66671499225878));
#73219=CARTESIAN_POINT('Ctrl Pts',(0.293210606856168,0.0293637433603259,
-1.67199381860045));
#73220=CARTESIAN_POINT('Ctrl Pts',(0.302890279065485,-0.0672922795829509,
-1.67727264494212));
#73221=CARTESIAN_POINT('Ctrl Pts',(0.260077644072382,-0.169205175930827,
-1.68255147128379));
#73222=CARTESIAN_POINT('Ctrl Pts',(0.184275002501595,-0.229950892928197,
-1.68783029762546));
#73223=CARTESIAN_POINT('Ctrl Pts',(0.108472360930808,-0.290696609925567,
-1.69310912396712));
#73224=CARTESIAN_POINT('Ctrl Pts',(-0.000320287217663959,-0.310275147572431,
-1.69838795030879));
#73225=CARTESIAN_POINT('Ctrl Pts',(-0.0925449829713599,-0.279767965087295,
-1.70366677665046));
#73226=CARTESIAN_POINT('Ctrl Pts',(-0.184769678725056,-0.249260782602159,
-1.70894560299213));
#73227=CARTESIAN_POINT('Ctrl Pts',(-0.260426422083976,-0.168667879985022,
-1.7142244293338));
#73228=CARTESIAN_POINT('Ctrl Pts',(-0.285051541170753,-0.0747014666740018,
-1.71950325567546));
#73229=CARTESIAN_POINT('Ctrl Pts',(-0.291394436347813,-0.0504977620057828,
-1.72086296654732));
#73230=CARTESIAN_POINT('Ctrl Pts',(-0.294351558961662,-0.0254067709494276,
-1.72222267741918));
#73231=CARTESIAN_POINT('Ctrl Pts',(-0.294128475609455,-0.000264102212364226,
-1.72358238829104));
#73232=CARTESIAN_POINT('Ctrl Pts',(-0.294155870929176,-0.000265231913958952,
-1.73801761170896));
#73233=CARTESIAN_POINT('Ctrl Pts',(-0.294373369254718,-0.0244725744211715,
-1.73670817235595));
#73234=CARTESIAN_POINT('Ctrl Pts',(-0.291633831150307,-0.0486313549496652,
-1.73539873300295));
#73235=CARTESIAN_POINT('Ctrl Pts',(-0.285746593491363,-0.0719970338945612,
-1.73408929364994));
#73236=CARTESIAN_POINT('Ctrl Pts',(-0.262012997000382,-0.166192585007317,
-1.72881046730827));
#73237=CARTESIAN_POINT('Ctrl Pts',(-0.187123321975502,-0.247498733496666,
-1.7235316409666));
#73238=CARTESIAN_POINT('Ctrl Pts',(-0.0951918484083055,-0.278878439174703,
-1.71825281462494));
#73239=CARTESIAN_POINT('Ctrl Pts',(-0.00326037484110897,-0.310258144852741,
-1.71297398828327));
#73240=CARTESIAN_POINT('Ctrl Pts',(0.105712897268404,-0.291711407719467,
-1.7076951619416));
#73241=CARTESIAN_POINT('Ctrl Pts',(0.182087744697166,-0.231686718226887,
-1.70241633559993));
#73242=CARTESIAN_POINT('Ctrl Pts',(0.258462592125928,-0.171662028734307,
-1.69713750925826));
#73243=CARTESIAN_POINT('Ctrl Pts',(0.302239014873937,-0.0701593868824198,
-1.6918586829166));
#73244=CARTESIAN_POINT('Ctrl Pts',(0.293475673477413,0.0265840167733769,
-1.68657985657493));
#73245=CARTESIAN_POINT('Ctrl Pts',(0.284712332080889,0.123327420429173,
-1.68130103023326));
#73246=CARTESIAN_POINT('Ctrl Pts',(0.223409226539831,0.215311585888878,
-1.67602220389159));
#73247=CARTESIAN_POINT('Ctrl Pts',(0.137491564974706,0.260635278388163,
-1.67074337754992));
#73248=CARTESIAN_POINT('Ctrl Pts',(0.0515739034095804,0.305958970887449,
-1.66546455120825));
#73249=CARTESIAN_POINT('Ctrl Pts',(-0.058958314179612,0.304622190426314,
-1.66018572486659));
#73250=CARTESIAN_POINT('Ctrl Pts',(-0.14375470950795,0.257233869898643,
-1.65490689852492));
#73251=CARTESIAN_POINT('Ctrl Pts',(-0.228551104836288,0.209845549370971,
-1.64962807218325));
#73252=CARTESIAN_POINT('Ctrl Pts',(-0.28761167790377,0.116405688776762,
-1.64434924584158));
#73253=CARTESIAN_POINT('Ctrl Pts',(-0.294032757280035,0.019478646388514,
-1.63907041949991));
#73254=CARTESIAN_POINT('Ctrl Pts',(-0.294459630095828,0.0130349447791417,
-1.6387194835696));
#73255=CARTESIAN_POINT('Ctrl Pts',(-0.294653858500483,0.0065758312936643,
-1.63836854763928));
#73256=CARTESIAN_POINT('Ctrl Pts',(-0.294621628357173,0.000114745350509935,
-1.63801761170896));
#73257=CARTESIAN_POINT('Origin',(0.,0.,-0.975));
#73258=CARTESIAN_POINT('',(-0.293848972356552,0.000185260601430967,-1.52358238829104));
#73259=CARTESIAN_POINT('',(-0.293831567852127,0.000174014199626464,-1.53801761170896));
#73260=CARTESIAN_POINT('',(-0.2942,-3.60291088309151E-17,-0.975));
#73261=CARTESIAN_POINT('Ctrl Pts',(-0.293848972356552,0.000185260601430967,
-1.52358238829104));
#73262=CARTESIAN_POINT('Ctrl Pts',(-0.294059652757306,0.0365345081610124,
-1.52554342798583));
#73263=CARTESIAN_POINT('Ctrl Pts',(-0.287810810463736,0.0728138920437894,
-1.52750446768062));
#73264=CARTESIAN_POINT('Ctrl Pts',(-0.274773239737348,0.106462932671202,
-1.52946550737541));
#73265=CARTESIAN_POINT('Ctrl Pts',(-0.23967804407933,0.197041130811557,
-1.53474433371708));
#73266=CARTESIAN_POINT('Ctrl Pts',(-0.155391308608968,0.268559701475745,
-1.54002316005875));
#73267=CARTESIAN_POINT('Ctrl Pts',(-0.0603078950404424,0.288440023412727,
-1.54530198640042));
#73268=CARTESIAN_POINT('Ctrl Pts',(0.034775518528081,0.308320345349709,
-1.55058081274209));
#73269=CARTESIAN_POINT('Ctrl Pts',(0.140655610194769,0.276562418559487,
-1.55585963908375));
#73270=CARTESIAN_POINT('Ctrl Pts',(0.209101167128348,0.20763282787565,-1.56113846542542));
#73271=CARTESIAN_POINT('Ctrl Pts',(0.277546724061928,0.138703237191812,
-1.56641729176709));
#73272=CARTESIAN_POINT('Ctrl Pts',(0.308557746262399,0.032601982614358,
-1.57169611810876));
#73273=CARTESIAN_POINT('Ctrl Pts',(0.288007883920642,-0.0623389774397669,
-1.57697494445043));
#73274=CARTESIAN_POINT('Ctrl Pts',(0.267458021578885,-0.157279937493893,
-1.58225377079209));
#73275=CARTESIAN_POINT('Ctrl Pts',(0.195347274694897,-0.241060603024691,
-1.58753259713376));
#73276=CARTESIAN_POINT('Ctrl Pts',(0.104524016624659,-0.275516640637564,
-1.59281142347543));
#73277=CARTESIAN_POINT('Ctrl Pts',(0.0137007585544223,-0.309972678250436,
-1.5980902498171));
#73278=CARTESIAN_POINT('Ctrl Pts',(-0.0958350107020636,-0.295104087945385,
-1.60336907615877));
#73279=CARTESIAN_POINT('Ctrl Pts',(-0.174186819445307,-0.237683910307274,
-1.60864790250043));
#73280=CARTESIAN_POINT('Ctrl Pts',(-0.248075969457547,-0.183534195230047,
-1.61362606443064));
#73281=CARTESIAN_POINT('Ctrl Pts',(-0.294232265806487,-0.0915420468882019,
-1.61860422636084));
#73282=CARTESIAN_POINT('Ctrl Pts',(-0.294635704950153,9.93244666355822E-5,
-1.62358238829104));
#73283=CARTESIAN_POINT('Ctrl Pts',(-0.294621628357173,0.000114745350509935,
-1.63801761170896));
#73284=CARTESIAN_POINT('Ctrl Pts',(-0.294169048269317,-0.0906127086249664,
-1.63308972129761));
#73285=CARTESIAN_POINT('Ctrl Pts',(-0.249063006756553,-0.18172909498379,
-1.62816183088626));
#73286=CARTESIAN_POINT('Ctrl Pts',(-0.176431238499582,-0.236022663853079,
-1.62323394047491));
#73287=CARTESIAN_POINT('Ctrl Pts',(-0.0986270546578152,-0.294182707524139,
-1.61795511413324));
#73288=CARTESIAN_POINT('Ctrl Pts',(0.0107628987107675,-0.310088570683974,
-1.61267628779157));
#73289=CARTESIAN_POINT('Ctrl Pts',(0.101908573247503,-0.276494706451795,
-1.6073974614499));
#73290=CARTESIAN_POINT('Ctrl Pts',(0.19305424778424,-0.242900842219616,
-1.60211863510824));
#73291=CARTESIAN_POINT('Ctrl Pts',(0.26595564348913,-0.159807250595422,
-1.59683980876657));
#73292=CARTESIAN_POINT('Ctrl Pts',(0.287404225167761,-0.0650652848440229,
-1.5915609824249));
#73293=CARTESIAN_POINT('Ctrl Pts',(0.308852806846392,0.0296766809073748,
-1.58628215608323));
#73294=CARTESIAN_POINT('Ctrl Pts',(0.278848574498767,0.136067020785977,
-1.58100332974156));
#73295=CARTESIAN_POINT('Ctrl Pts',(0.211059258319554,0.205642090503064,
-1.5757245033999));
#73296=CARTESIAN_POINT('Ctrl Pts',(0.143269942140342,0.275217160220151,
-1.57044567705823));
#73297=CARTESIAN_POINT('Ctrl Pts',(0.0376955421295423,0.307976959775722,
-1.56516685071656));
#73298=CARTESIAN_POINT('Ctrl Pts',(-0.0575719796483724,0.288998524391603,
-1.55988802437489));
#73299=CARTESIAN_POINT('Ctrl Pts',(-0.152839501426288,0.270020089007484,
-1.55460919803322));
#73300=CARTESIAN_POINT('Ctrl Pts',(-0.237800144971318,0.199303418683675,
-1.54933037169156));
#73301=CARTESIAN_POINT('Ctrl Pts',(-0.273752065399016,0.109061847682818,
-1.54405154534989));
#73302=CARTESIAN_POINT('Ctrl Pts',(-0.287450280878734,0.074678469268191,
-1.54204023413625));
#73303=CARTESIAN_POINT('Ctrl Pts',(-0.294033786615915,0.0374606158410958,
-1.5400289229226));
#73304=CARTESIAN_POINT('Ctrl Pts',(-0.293831567852127,0.000174014199626464,
-1.53801761170896));
#73305=CARTESIAN_POINT('Origin',(0.,0.,-0.975));
#73306=CARTESIAN_POINT('',(-0.293976078480642,-0.000239187850661487,-1.42358238829104));
#73307=CARTESIAN_POINT('',(-0.294000243181898,-0.000245490063885288,-1.43801761170896));
#73308=CARTESIAN_POINT('',(-0.2942,-3.60291088309151E-17,-0.975));
#73309=CARTESIAN_POINT('Ctrl Pts',(-0.293976078480642,-0.000239187850661488,
-1.42358238829104));
#73310=CARTESIAN_POINT('Ctrl Pts',(-0.293459100644232,0.0668131948144753,
-1.42720380326916));
#73311=CARTESIAN_POINT('Ctrl Pts',(-0.270685225221847,0.13418317542563,
-1.43082521824727));
#73312=CARTESIAN_POINT('Ctrl Pts',(-0.228646632964908,0.185890845774307,
-1.43444663322539));
#73313=CARTESIAN_POINT('Ctrl Pts',(-0.1673682571053,0.261263542345228,-1.43972545956705));
#73314=CARTESIAN_POINT('Ctrl Pts',(-0.0651562009534198,0.30335695397111,
-1.44500428590872));
#73315=CARTESIAN_POINT('Ctrl Pts',(0.0314292109107904,0.292996406139133,
-1.45028311225039));
#73316=CARTESIAN_POINT('Ctrl Pts',(0.128014622775002,0.282635858307157,
-1.45556193859206));
#73317=CARTESIAN_POINT('Ctrl Pts',(0.218973390351543,0.219821351017321,
-1.46084076493373));
#73318=CARTESIAN_POINT('Ctrl Pts',(0.262871362903329,0.133166571909731,
-1.46611959127539));
#73319=CARTESIAN_POINT('Ctrl Pts',(0.306769335455115,0.0465117928021422,
-1.47139841761706));
#73320=CARTESIAN_POINT('Ctrl Pts',(0.303606512982146,-0.0639832581232009,
-1.47667724395873));
#73321=CARTESIAN_POINT('Ctrl Pts',(0.254823645690022,-0.147985130692535,
-1.4819560703004));
#73322=CARTESIAN_POINT('Ctrl Pts',(0.206040778397898,-0.231987003261871,
-1.48723489664207));
#73323=CARTESIAN_POINT('Ctrl Pts',(0.111637866286618,-0.289495697475197,
-1.49251372298374));
#73324=CARTESIAN_POINT('Ctrl Pts',(0.0146179600206351,-0.29431446541747,
-1.4977925493254));
#73325=CARTESIAN_POINT('Ctrl Pts',(-0.0824019462453475,-0.299133233359743,
-1.50307137566707));
#73326=CARTESIAN_POINT('Ctrl Pts',(-0.182038846666034,-0.251262075030964,
-1.50835020200874));
#73327=CARTESIAN_POINT('Ctrl Pts',(-0.238905468953538,-0.172507583058315,
-1.51362902835041));
#73328=CARTESIAN_POINT('Ctrl Pts',(-0.274646618191435,-0.123009724076673,
-1.51694681499729));
#73329=CARTESIAN_POINT('Ctrl Pts',(-0.293492532544428,-0.0613122442668173,
-1.52026460164416));
#73330=CARTESIAN_POINT('Ctrl Pts',(-0.293848972356552,0.000185260601430967,
-1.52358238829104));
#73331=CARTESIAN_POINT('Ctrl Pts',(-0.293831567852127,0.000174014199626464,
-1.53801761170896));
#73332=CARTESIAN_POINT('Ctrl Pts',(-0.293503049388466,-0.0604006666900559,
-1.53475009658094));
#73333=CARTESIAN_POINT('Ctrl Pts',(-0.275265466965423,-0.121156789689294,
-1.53148258145291));
#73334=CARTESIAN_POINT('Ctrl Pts',(-0.240529380088274,-0.170236004540617,
-1.52821506632488));
#73335=CARTESIAN_POINT('Ctrl Pts',(-0.18441157703947,-0.249525814085292,
-1.52293623998321));
#73336=CARTESIAN_POINT('Ctrl Pts',(-0.0852327736314988,-0.298338961496739,
-1.51765741364155));
#73337=CARTESIAN_POINT('Ctrl Pts',(0.0118284332921869,-0.294439752917206,
-1.51237858729988));
#73338=CARTESIAN_POINT('Ctrl Pts',(0.108889640215873,-0.290540544337672,
-1.50709976095821));
#73339=CARTESIAN_POINT('Ctrl Pts',(0.203833250655272,-0.233928979767156,
-1.50182093461654));
#73340=CARTESIAN_POINT('Ctrl Pts',(0.253409911396691,-0.150393140588825,
-1.49654210827487));
#73341=CARTESIAN_POINT('Ctrl Pts',(0.302986572138111,-0.0668573014104933,
-1.49126328193321));
#73342=CARTESIAN_POINT('Ctrl Pts',(0.307196283181549,0.0436028123756558,
-1.48598445559154));
#73343=CARTESIAN_POINT('Ctrl Pts',(0.264121408586994,0.130669665401313,
-1.48070562924987));
#73344=CARTESIAN_POINT('Ctrl Pts',(0.221046533992439,0.217736518426971,
-1.4754268029082));
#73345=CARTESIAN_POINT('Ctrl Pts',(0.130687073759891,0.281410110692138,
-1.47014797656653));
#73346=CARTESIAN_POINT('Ctrl Pts',(0.0342041781057301,0.29268541837746,
-1.46486915022487));
#73347=CARTESIAN_POINT('Ctrl Pts',(-0.0622787175484317,0.303960726062782,
-1.4595903238832));
#73348=CARTESIAN_POINT('Ctrl Pts',(-0.164885048624206,0.262837749168258,
-1.45431149754153));
#73349=CARTESIAN_POINT('Ctrl Pts',(-0.226874887771002,0.188049103239753,
-1.44903267119986));
#73350=CARTESIAN_POINT('Ctrl Pts',(-0.269991906709058,0.136029877069238,
-1.44536098470289));
#73351=CARTESIAN_POINT('Ctrl Pts',(-0.29345909350785,0.0677235538611339,
-1.44168929820593));
#73352=CARTESIAN_POINT('Ctrl Pts',(-0.294000243181898,-0.000245490063885288,
-1.43801761170896));
#73353=CARTESIAN_POINT('Origin',(0.,0.,-0.975));
#73354=CARTESIAN_POINT('',(-0.294677260201263,1.00828370830571E-6,-1.32358238829104));
#73355=CARTESIAN_POINT('',(-0.29467583034949,1.80923891189878E-5,-1.33801761170896));
#73356=CARTESIAN_POINT('',(-0.2942,-3.60291088309151E-17,-0.975));
#73357=CARTESIAN_POINT('Ctrl Pts',(-0.294677258502014,1.00828011838765E-6,
-1.32358238829104));
#73358=CARTESIAN_POINT('Ctrl Pts',(-0.294682224165865,0.0971950549178843,
-1.32886417855248));
#73359=CARTESIAN_POINT('Ctrl Pts',(-0.241859572446614,0.194384460417949,
-1.33414596881392));
#73360=CARTESIAN_POINT('Ctrl Pts',(-0.160305775694497,0.24725846312689,
-1.33942775907536));
#73361=CARTESIAN_POINT('Ctrl Pts',(-0.0787977435219472,0.300102795157083,
-1.34470658541703));
#73362=CARTESIAN_POINT('Ctrl Pts',(0.0314091821623557,0.308681446350664,
-1.3499854117587));
#73363=CARTESIAN_POINT('Ctrl Pts',(0.120112799935227,0.269086611708214,
-1.35526423810036));
#73364=CARTESIAN_POINT('Ctrl Pts',(0.2088164177081,0.229491777065762,-1.36054306444203));
#73365=CARTESIAN_POINT('Ctrl Pts',(0.27601672756954,0.141723456587276,-1.3658218907837));
#73366=CARTESIAN_POINT('Ctrl Pts',(0.291102191538456,0.045762467048812,
-1.37110071712537));
#73367=CARTESIAN_POINT('Ctrl Pts',(0.306187655507372,-0.0501985224896504,
-1.37637954346704));
#73368=CARTESIAN_POINT('Ctrl Pts',(0.269158273583764,-0.15435218108809,
-1.38165836980871));
#73369=CARTESIAN_POINT('Ctrl Pts',(0.196881919346013,-0.219253732336566,
-1.38693719615037));
#73370=CARTESIAN_POINT('Ctrl Pts',(0.124605565108262,-0.284155283585041,
-1.39221602249204));
#73371=CARTESIAN_POINT('Ctrl Pts',(0.0170822385563674,-0.309804727483553,
-1.39749484883371));
#73372=CARTESIAN_POINT('Ctrl Pts',(-0.0767083100468562,-0.284518056507222,
-1.40277367517538));
#73373=CARTESIAN_POINT('Ctrl Pts',(-0.17049885865008,-0.259231385530891,
-1.40805250151705));
#73374=CARTESIAN_POINT('Ctrl Pts',(-0.250556629304634,-0.183008599679717,
-1.41333132785871));
#73375=CARTESIAN_POINT('Ctrl Pts',(-0.280413166848243,-0.0905712159961477,
-1.41861015420038));
#73376=CARTESIAN_POINT('Ctrl Pts',(-0.289787327200992,-0.0615483309421544,
-1.42026756556394));
#73377=CARTESIAN_POINT('Ctrl Pts',(-0.294212683494414,-0.0309270216543183,
-1.42192497692749));
#73378=CARTESIAN_POINT('Ctrl Pts',(-0.293976078480642,-0.000239187850661488,
-1.42358238829104));
#73379=CARTESIAN_POINT('Ctrl Pts',(-0.294000243181898,-0.000245490063885288,
-1.43801761170896));
#73380=CARTESIAN_POINT('Ctrl Pts',(-0.294237110682385,-0.0299963303898278,
-1.43641047186426));
#73381=CARTESIAN_POINT('Ctrl Pts',(-0.290081545205885,-0.0596825508847279,
-1.43480333201956));
#73382=CARTESIAN_POINT('Ctrl Pts',(-0.281258798274574,-0.0879100012713292,
-1.43319619217486));
#73383=CARTESIAN_POINT('Ctrl Pts',(-0.252279522413535,-0.180626144891419,
-1.42791736583319));
#73384=CARTESIAN_POINT('Ctrl Pts',(-0.172947623473641,-0.257604117169112,
-1.42263853949152));
#73385=CARTESIAN_POINT('Ctrl Pts',(-0.0794009026422469,-0.283778393451755,
-1.41735971314985));
#73386=CARTESIAN_POINT('Ctrl Pts',(0.0141458181891462,-0.309952669734398,
-1.41208088680818));
#73387=CARTESIAN_POINT('Ctrl Pts',(0.12190736091204,-0.285323250021994,
-1.40680206046652));
#73388=CARTESIAN_POINT('Ctrl Pts',(0.194795461428105,-0.221109493548848,
-1.40152323412485));
#73389=CARTESIAN_POINT('Ctrl Pts',(0.267683561944172,-0.156895737075701,
-1.39624440778318));
#73390=CARTESIAN_POINT('Ctrl Pts',(0.305698220253408,-0.0530976438418118,
-1.39096558144151));
#73391=CARTESIAN_POINT('Ctrl Pts',(0.291522743038951,0.0430019792738263,
-1.38568675509984));
#73392=CARTESIAN_POINT('Ctrl Pts',(0.277347265824494,0.139101602389462,
-1.38040792875818));
#73393=CARTESIAN_POINT('Ctrl Pts',(0.210981653086343,0.227502755386847,
-1.37512910241651));
#73394=CARTESIAN_POINT('Ctrl Pts',(0.122657215947318,0.267936349356492,
-1.36985027607484));
#73395=CARTESIAN_POINT('Ctrl Pts',(0.0343327788082925,0.308369943326136,
-1.36457144973317));
#73396=CARTESIAN_POINT('Ctrl Pts',(-0.0759504827316088,0.30083597826804,
-1.3592926233915));
#73397=CARTESIAN_POINT('Ctrl Pts',(-0.157955594225854,0.248766376713537,
-1.35401379704983));
#73398=CARTESIAN_POINT('Ctrl Pts',(-0.2399607057201,0.196696775159033,-1.34873497070817));
#73399=CARTESIAN_POINT('Ctrl Pts',(-0.29368766716869,0.10009153710812,-1.3434561443665));
#73400=CARTESIAN_POINT('Ctrl Pts',(-0.294662411050462,0.00295693157748309,
-1.33817731802483));
#73401=CARTESIAN_POINT('Ctrl Pts',(-0.29467224106091,0.00197735714252186,
-1.33812408258621));
#73402=CARTESIAN_POINT('Ctrl Pts',(-0.294676706097081,0.000997728870147867,
-1.33807084714758));
#73403=CARTESIAN_POINT('Ctrl Pts',(-0.29467583034949,1.80923891189878E-5,
-1.33801761170896));
#73404=CARTESIAN_POINT('Origin',(0.,0.,-0.975));
#73405=CARTESIAN_POINT('',(-0.293973278032798,0.000238391689448475,-1.22358238829104));
#73406=CARTESIAN_POINT('',(-0.293949969260341,0.000231200790277284,-1.23801761170896));
#73407=CARTESIAN_POINT('',(-0.2942,-3.60291088309151E-17,-0.975));
#73408=CARTESIAN_POINT('Ctrl Pts',(-0.293973278032798,0.000238391689448475,
-1.22358238829104));
#73409=CARTESIAN_POINT('Ctrl Pts',(-0.294209779461322,0.0310367239073477,
-1.22524572749414));
#73410=CARTESIAN_POINT('Ctrl Pts',(-0.28975201722522,0.0617683278239009,
-1.22690906669723));
#73411=CARTESIAN_POINT('Ctrl Pts',(-0.280311790129639,0.0908844850521986,
-1.22857240590033));
#73412=CARTESIAN_POINT('Ctrl Pts',(-0.250351984354179,0.183288450195776,
-1.233851232242));
#73413=CARTESIAN_POINT('Ctrl Pts',(-0.17020909453095,0.259421734217083,
-1.23913005858367));
#73414=CARTESIAN_POINT('Ctrl Pts',(-0.0763903498795328,0.28460359055038,
-1.24440888492533));
#73415=CARTESIAN_POINT('Ctrl Pts',(0.0174283947718846,0.309785446883678,
-1.249687711267));
#73416=CARTESIAN_POINT('Ctrl Pts',(0.124922994251492,0.284015875528968,
-1.25496653760867));
#73417=CARTESIAN_POINT('Ctrl Pts',(0.197126784246028,0.219033605279432,
-1.26024536395034));
#73418=CARTESIAN_POINT('Ctrl Pts',(0.269330574240564,0.154051335029895,
-1.26552419029201));
#73419=CARTESIAN_POINT('Ctrl Pts',(0.306243554750027,0.0498563658855321,
-1.27080301663368));
#73420=CARTESIAN_POINT('Ctrl Pts',(0.291050876152584,-0.0460877076854485,
-1.27608184297534));
#73421=CARTESIAN_POINT('Ctrl Pts',(0.275858197555141,-0.142031781256427,
-1.28136066931701));
#73422=CARTESIAN_POINT('Ctrl Pts',(0.208559859850791,-0.229724959254024,
-1.28663949565868));
#73423=CARTESIAN_POINT('Ctrl Pts',(0.119812055324197,-0.269220654311436,
-1.29191832200035));
#73424=CARTESIAN_POINT('Ctrl Pts',(0.0310642507976013,-0.308716349368848,
-1.29719714834201));
#73425=CARTESIAN_POINT('Ctrl Pts',(-0.0791330205512378,-0.300014561486076,
-1.30247597468368));
#73426=CARTESIAN_POINT('Ctrl Pts',(-0.160581955107085,-0.247079187716959,
-1.30775480102535));
#73427=CARTESIAN_POINT('Ctrl Pts',(-0.241985158265097,-0.194173535744089,
-1.31303066344725));
#73428=CARTESIAN_POINT('Ctrl Pts',(-0.294672298411209,-0.0970839558904198,
-1.31830652586914));
#73429=CARTESIAN_POINT('Ctrl Pts',(-0.294677258502014,1.00828011838765E-6,
-1.32358238829104));
#73430=CARTESIAN_POINT('Ctrl Pts',(-0.29467583034949,1.80923891189878E-5,
-1.33801761170896));
#73431=CARTESIAN_POINT('Ctrl Pts',(-0.294589866961943,-0.0961430291488454,
-1.33279202080592));
#73432=CARTESIAN_POINT('Ctrl Pts',(-0.243043387744428,-0.192383244249407,
-1.32756642990287));
#73433=CARTESIAN_POINT('Ctrl Pts',(-0.162916013713709,-0.245546436353821,
-1.32234083899983));
#73434=CARTESIAN_POINT('Ctrl Pts',(-0.0819723461802288,-0.299251225744129,
-1.31706201265816));
#73435=CARTESIAN_POINT('Ctrl Pts',(0.0281375152016859,-0.308996831514383,
-1.31178318631649));
#73436=CARTESIAN_POINT('Ctrl Pts',(0.117255584393945,-0.270343869652818,
-1.30650435997482));
#73437=CARTESIAN_POINT('Ctrl Pts',(0.206373653586204,-0.231690907791252,
-1.30122553363315));
#73438=CARTESIAN_POINT('Ctrl Pts',(0.274499930588806,-0.144639378297869,
-1.29594670729149));
#73439=CARTESIAN_POINT('Ctrl Pts',(0.290601074628839,-0.0488435804890409,
-1.29066788094982));
#73440=CARTESIAN_POINT('Ctrl Pts',(0.306702218668872,0.0469522173197857,
-1.28538905460815));
#73441=CARTESIAN_POINT('Ctrl Pts',(0.270778229746334,0.151492283444057,
-1.28011022826648));
#73442=CARTESIAN_POINT('Ctrl Pts',(0.19919344537101,0.217155822513817,-1.27483140192481));
#73443=CARTESIAN_POINT('Ctrl Pts',(0.127608660995684,0.282819361583577,
-1.26955257558315));
#73444=CARTESIAN_POINT('Ctrl Pts',(0.0203630811675721,0.309606373598827,
-1.26427374924148));
#73445=CARTESIAN_POINT('Ctrl Pts',(-0.0736900649097486,0.285314658340616,
-1.25899492289981));
#73446=CARTESIAN_POINT('Ctrl Pts',(-0.167743210987069,0.261022943082406,
-1.25371609655814));
#73447=CARTESIAN_POINT('Ctrl Pts',(-0.248603923313597,0.185652500550734,
-1.24843727021647));
#73448=CARTESIAN_POINT('Ctrl Pts',(-0.279437985325964,0.0935365826155301,
-1.2431584438748));
#73449=CARTESIAN_POINT('Ctrl Pts',(-0.289447327525483,0.0636339462302733,
-1.24144483315286));
#73450=CARTESIAN_POINT('Ctrl Pts',(-0.294184965742798,0.0319667066022578,
-1.23973122243091));
#73451=CARTESIAN_POINT('Ctrl Pts',(-0.293949969260341,0.000231200790277284,
-1.23801761170896));
#73452=CARTESIAN_POINT('Origin',(0.,0.,-0.975));
#73453=CARTESIAN_POINT('',(-0.293851097698083,-0.000186547984213553,-1.12358238829104));
#73454=CARTESIAN_POINT('',(-0.29386972337181,-0.000197122199406605,-1.13801761170896));
#73455=CARTESIAN_POINT('',(-0.2942,-3.60291088309151E-17,-0.975));
#73456=CARTESIAN_POINT('Ctrl Pts',(-0.293851097698083,-0.000186547984213553,
-1.12358238829104));
#73457=CARTESIAN_POINT('Ctrl Pts',(-0.293491376629239,0.0614197145543361,
-1.12690610277746));
#73458=CARTESIAN_POINT('Ctrl Pts',(-0.274572956169531,0.12322816383533,
-1.13022981726388));
#73459=CARTESIAN_POINT('Ctrl Pts',(-0.238712564810087,0.172774421459531,
-1.1335535317503));
#73460=CARTESIAN_POINT('Ctrl Pts',(-0.181757980021253,0.251465323143845,
-1.13883235809197));
#73461=CARTESIAN_POINT('Ctrl Pts',(-0.0820676519460495,0.299225120184297,
-1.14411118443364));
#73462=CARTESIAN_POINT('Ctrl Pts',(0.0149468094019105,0.294297948000982,
-1.14939001077531));
#73463=CARTESIAN_POINT('Ctrl Pts',(0.111961270749869,0.289370775817668,
-1.15466883711698));
#73464=CARTESIAN_POINT('Ctrl Pts',(0.206299865370584,0.231756634410589,
-1.15994766345864));
#73465=CARTESIAN_POINT('Ctrl Pts',(0.254988840936584,0.14770030570958,-1.16522648980031));
#73466=CARTESIAN_POINT('Ctrl Pts',(0.303677816502585,0.0636439770085698,
-1.17050531614198));
#73467=CARTESIAN_POINT('Ctrl Pts',(0.306717173013869,-0.0468545389863712,
-1.17578414248365));
#73468=CARTESIAN_POINT('Ctrl Pts',(0.262722402311544,-0.133460213668858,
-1.18106296882532));
#73469=CARTESIAN_POINT('Ctrl Pts',(0.218727631609219,-0.220065888351345,
-1.18634179516699));
#73470=CARTESIAN_POINT('Ctrl Pts',(0.127698733693286,-0.282778721721378,
-1.19162062150865));
#73471=CARTESIAN_POINT('Ctrl Pts',(0.0311018055456793,-0.293031341328338,
-1.19689944785032));
#73472=CARTESIAN_POINT('Ctrl Pts',(-0.0654951226019258,-0.303283960935298,
-1.20217827419199));
#73473=CARTESIAN_POINT('Ctrl Pts',(-0.167660080981204,-0.261076366779188,
-1.20745710053366));
#73474=CARTESIAN_POINT('Ctrl Pts',(-0.228854199306997,-0.185635246568208,
-1.21273592687533));
#73475=CARTESIAN_POINT('Ctrl Pts',(-0.270766270938664,-0.133965352127992,
-1.2163514140139));
#73476=CARTESIAN_POINT('Ctrl Pts',(-0.293459210985325,-0.0667058454306556,
-1.21996690115247));
#73477=CARTESIAN_POINT('Ctrl Pts',(-0.293973278032798,0.000238391689448475,
-1.22358238829104));
#73478=CARTESIAN_POINT('Ctrl Pts',(-0.293949969260341,0.000231200790277284,
-1.23801761170896));
#73479=CARTESIAN_POINT('Ctrl Pts',(-0.293461052425786,-0.0657954174909175,
-1.23445239608924));
#73480=CARTESIAN_POINT('Ctrl Pts',(-0.271447598728151,-0.132117532642881,
-1.23088718046952));
#73481=CARTESIAN_POINT('Ctrl Pts',(-0.230602957574135,-0.183458321938491,
-1.2273219648498));
#73482=CARTESIAN_POINT('Ctrl Pts',(-0.170126456111733,-0.259475915218572,
-1.22204313850813));
#73483=CARTESIAN_POINT('Ctrl Pts',(-0.0683660414887238,-0.302649708439997,
-1.21676431216646));
#73484=CARTESIAN_POINT('Ctrl Pts',(0.028323696507632,-0.293312884385547,
-1.2114854858248));
#73485=CARTESIAN_POINT('Ctrl Pts',(0.125013434503989,-0.283976060331096,
-1.20620665948313));
#73486=CARTESIAN_POINT('Ctrl Pts',(0.216632495873691,-0.222128619000769,
-1.20092783314146));
#73487=CARTESIAN_POINT('Ctrl Pts',(0.261445948401493,-0.135943723631765,
-1.19564900679979));
#73488=CARTESIAN_POINT('Ctrl Pts',(0.306259400929294,-0.0497588282627614,
-1.19037018045812));
#73489=CARTESIAN_POINT('Ctrl Pts',(0.304267244615197,0.0607635211449203,
-1.18509135411646));
#73490=CARTESIAN_POINT('Ctrl Pts',(0.256376959927654,0.145277439228119,
-1.17981252777479));
#73491=CARTESIAN_POINT('Ctrl Pts',(0.20848667524011,0.229791357311319,-1.17453370143312));
#73492=CARTESIAN_POINT('Ctrl Pts',(0.114698262179123,0.288296844070036,
-1.16925487509145));
#73493=CARTESIAN_POINT('Ctrl Pts',(0.0177348506606446,0.294143085933479,
-1.16397604874978));
#73494=CARTESIAN_POINT('Ctrl Pts',(-0.0792285608578346,0.299989327796923,
-1.15869722240811));
#73495=CARTESIAN_POINT('Ctrl Pts',(-0.179366970833807,0.253176324765089,
-1.15341839606645));
#73496=CARTESIAN_POINT('Ctrl Pts',(-0.23706465596679,0.175028651431054,
-1.14813956972478));
#73497=CARTESIAN_POINT('Ctrl Pts',(-0.273942395368571,0.12508020851821,
-1.14476558371951));
#73498=CARTESIAN_POINT('Ctrl Pts',(-0.293482310532986,0.0623309708912046,
-1.14139159771423));
#73499=CARTESIAN_POINT('Ctrl Pts',(-0.29386972337181,-0.000197122199406605,
-1.13801761170896));
#73500=CARTESIAN_POINT('Origin',(0.,0.,-0.975));
#73501=CARTESIAN_POINT('',(-0.294637244334855,-9.74749229996352E-5,-1.02358238829104));
#73502=CARTESIAN_POINT('',(-0.294649229866944,-8.15492747527925E-5,-1.03801761170896));
#73503=CARTESIAN_POINT('',(-0.2942,-3.60291088309151E-17,-0.975));
#73504=CARTESIAN_POINT('Ctrl Pts',(-0.294637244334855,-9.74749229996352E-5,
-1.02358238829104));
#73505=CARTESIAN_POINT('Ctrl Pts',(-0.294239924072814,0.0916517427871641,
-1.02856647806079));
#73506=CARTESIAN_POINT('Ctrl Pts',(-0.247958795653551,0.183746892171388,
-1.03355056783053));
#73507=CARTESIAN_POINT('Ctrl Pts',(-0.173921129559392,0.237878393305636,
-1.03853465760028));
#73508=CARTESIAN_POINT('Ctrl Pts',(-0.0955052100818042,0.295210987079538,
-1.04381348394195));
#73509=CARTESIAN_POINT('Ctrl Pts',(0.0140471045446477,0.3099571759117,-1.04909231028361));
#73510=CARTESIAN_POINT('Ctrl Pts',(0.104831805736983,0.275399676497285,
-1.05437113662528));
#73511=CARTESIAN_POINT('Ctrl Pts',(0.195616506929317,0.240842177082871,
-1.05964996296695));
#73512=CARTESIAN_POINT('Ctrl Pts',(0.267633594687535,0.156980989421882,
-1.06492878930862));
#73513=CARTESIAN_POINT('Ctrl Pts',(0.288077359904879,0.0620171268209079,
-1.07020761565029));
#73514=CARTESIAN_POINT('Ctrl Pts',(0.308521125122224,-0.0329467357800676,
-1.07548644199195));
#73515=CARTESIAN_POINT('Ctrl Pts',(0.277391567798695,-0.139013273321028,
-1.08076526833362));
#73516=CARTESIAN_POINT('Ctrl Pts',(0.208869033654551,-0.207866341886078,
-1.08604409467529));
#73517=CARTESIAN_POINT('Ctrl Pts',(0.140346499510407,-0.276719410451129,
-1.09132292101696));
#73518=CARTESIAN_POINT('Ctrl Pts',(0.034430988545649,-0.308359010040268,
-1.09660174735863));
#73519=CARTESIAN_POINT('Ctrl Pts',(-0.0606301519675207,-0.288372457043458,
-1.10188057370029));
#73520=CARTESIAN_POINT('Ctrl Pts',(-0.155691292480689,-0.268385904046649,
-1.10715940004196));
#73521=CARTESIAN_POINT('Ctrl Pts',(-0.239898062542269,-0.196773198463892,
-1.11243822638363));
#73522=CARTESIAN_POINT('Ctrl Pts',(-0.274892026821827,-0.106155842508426,
-1.1177170527253));
#73523=CARTESIAN_POINT('Ctrl Pts',(-0.287852694590911,-0.0725940135236007,
-1.11967216458055));
#73524=CARTESIAN_POINT('Ctrl Pts',(-0.294062696777712,-0.0364252606470018,
-1.12162727643579));
#73525=CARTESIAN_POINT('Ctrl Pts',(-0.293851097698083,-0.000186547984213553,
-1.12358238829104));
#73526=CARTESIAN_POINT('Ctrl Pts',(-0.29386972337181,-0.000197122199406605,
-1.13801761170896));
#73527=CARTESIAN_POINT('Ctrl Pts',(-0.294088443781758,-0.0354984049228036,
-1.13611277137257));
#73528=CARTESIAN_POINT('Ctrl Pts',(-0.28820257943375,-0.0707292010046517,
-1.13420793103617));
#73529=CARTESIAN_POINT('Ctrl Pts',(-0.275885583475611,-0.103546244551637,
-1.13230309069977));
#73530=CARTESIAN_POINT('Ctrl Pts',(-0.241751865561453,-0.194491123564061,
-1.12702426435811));
#73531=CARTESIAN_POINT('Ctrl Pts',(-0.158227469443138,-0.266898537952673,
-1.12174543801644));
#73532=CARTESIAN_POINT('Ctrl Pts',(-0.0633599908742501,-0.287784974393801,
-1.11646661167477));
#73533=CARTESIAN_POINT('Ctrl Pts',(0.0315074876946384,-0.308671410834929,
-1.1111877853331));
#73534=CARTESIAN_POINT('Ctrl Pts',(0.1377180487141,-0.278036869328573,-1.10590895899143));
#73535=CARTESIAN_POINT('Ctrl Pts',(0.206889941722803,-0.209836202654263,
-1.10063013264977));
#73536=CARTESIAN_POINT('Ctrl Pts',(0.276061834731505,-0.141635535979953,
-1.0953513063081));
#73537=CARTESIAN_POINT('Ctrl Pts',(0.308195059729448,-0.0358687441376901,
-1.09007247996643));
#73538=CARTESIAN_POINT('Ctrl Pts',(0.288652073534054,0.0592845711371557,
-1.08479365362476));
#73539=CARTESIAN_POINT('Ctrl Pts',(0.269109087338661,0.154437886412003,
-1.07951482728309));
#73540=CARTESIAN_POINT('Ctrl Pts',(0.197889889949928,0.238977725119432,
-1.07423600094143));
#73541=CARTESIAN_POINT('Ctrl Pts',(0.107436730076877,0.274393930255051,
-1.06895717459976));
#73542=CARTESIAN_POINT('Ctrl Pts',(0.016983570203827,0.30981013539067,-1.06367834825809));
#73543=CARTESIAN_POINT('Ctrl Pts',(-0.0927035521535406,0.296102706954478,
-1.05839952191642));
#73544=CARTESIAN_POINT('Ctrl Pts',(-0.171659219886249,0.239515745115994,
-1.05312069557475));
#73545=CARTESIAN_POINT('Ctrl Pts',(-0.246958411680323,0.185549353406856,
-1.04808633428615));
#73546=CARTESIAN_POINT('Ctrl Pts',(-0.294306617932949,0.092583010904962,
-1.04305197299756));
#73547=CARTESIAN_POINT('Ctrl Pts',(-0.294649229866944,-8.15492747527925E-5,
-1.03801761170896));
#73548=CARTESIAN_POINT('Origin',(0.,0.,-0.975));
#73549=CARTESIAN_POINT('',(-0.29412526541255,0.000263908637235785,-0.92358238829104));
#73550=CARTESIAN_POINT('',(-0.294098243270401,0.000261754509978144,-0.938017611708962));
#73551=CARTESIAN_POINT('',(-0.2942,-3.60291088309151E-17,-0.975));
#73552=CARTESIAN_POINT('Ctrl Pts',(-0.29412526541255,0.000263908637235785,
-0.92358238829104));
#73553=CARTESIAN_POINT('Ctrl Pts',(-0.294348950217361,0.0255168907584005,
-0.924948027002442));
#73554=CARTESIAN_POINT('Ctrl Pts',(-0.29136559975532,0.0507178350965381,
-0.926313665713845));
#73555=CARTESIAN_POINT('Ctrl Pts',(-0.284967893282825,0.0750199247322646,
-0.927679304425247));
#73556=CARTESIAN_POINT('Ctrl Pts',(-0.260237793607645,0.168958760718316,
-0.932958130766915));
#73557=CARTESIAN_POINT('Ctrl Pts',(-0.184491046602315,0.249467083537742,
-0.938236957108583));
#73558=CARTESIAN_POINT('Ctrl Pts',(-0.0922323208863506,0.279871199470048,
-0.943515783450251));
#73559=CARTESIAN_POINT('Ctrl Pts',(2.64048296138575E-5,0.310275315402353,
-0.948794609791919));
#73560=CARTESIAN_POINT('Ctrl Pts',(0.108797109256212,0.290575224447537,
-0.954073436133588));
#73561=CARTESIAN_POINT('Ctrl Pts',(0.184531828155626,0.229744844787491,
-0.959352262475256));
#73562=CARTESIAN_POINT('Ctrl Pts',(0.260266547055043,0.168914465127443,
-0.964631088816924));
#73563=CARTESIAN_POINT('Ctrl Pts',(0.302965280427273,0.0669537967621638,
-0.969909915158591));
#73564=CARTESIAN_POINT('Ctrl Pts',(0.293177613518818,-0.0296913495869845,
-0.97518874150026));
#73565=CARTESIAN_POINT('Ctrl Pts',(0.283389946610364,-0.126336495936132,
-0.980467567841928));
#73566=CARTESIAN_POINT('Ctrl Pts',(0.221115879421224,-0.21766612026915,
-0.985746394183598));
#73567=CARTESIAN_POINT('Ctrl Pts',(0.134722914674649,-0.262077136680126,
-0.991025220525266));
#73568=CARTESIAN_POINT('Ctrl Pts',(0.0483299499280749,-0.306488153091101,
-0.996304046866934));
#73569=CARTESIAN_POINT('Ctrl Pts',(-0.0621819123759332,-0.30398056158004,
-1.0015828732086));
#73570=CARTESIAN_POINT('Ctrl Pts',(-0.146471564030352,-0.255696637129604,
-1.00686169955027));
#73571=CARTESIAN_POINT('Ctrl Pts',(-0.230761215684771,-0.207412712679169,
-1.01214052589194));
#73572=CARTESIAN_POINT('Ctrl Pts',(-0.2888286566896,-0.113352455289359,
-1.01741935223361));
#73573=CARTESIAN_POINT('Ctrl Pts',(-0.294222615027652,-0.016362827236634,
-1.02269817857527));
#73574=CARTESIAN_POINT('Ctrl Pts',(-0.294523779848533,-0.0109475343980307,
-1.0229929151472));
#73575=CARTESIAN_POINT('Ctrl Pts',(-0.294660740061738,-0.00552310952303855,
-1.02328765171912));
#73576=CARTESIAN_POINT('Ctrl Pts',(-0.294637244334855,-9.74749229996352E-5,
-1.02358238829104));
#73577=CARTESIAN_POINT('Ctrl Pts',(-0.294649229866944,-8.15492747527925E-5,
-1.03801761170896));
#73578=CARTESIAN_POINT('Ctrl Pts',(-0.29466586686215,-0.00458127532211663,
-1.03777314665589));
#73579=CARTESIAN_POINT('Ctrl Pts',(-0.29457166440834,-0.00908028976511084,
-1.03752868160282));
#73580=CARTESIAN_POINT('Ctrl Pts',(-0.294364440693888,-0.0135740924337639,
-1.03728421654975));
#73581=CARTESIAN_POINT('Ctrl Pts',(-0.289889780660768,-0.110610472904263,
-1.03200539020808));
#73582=CARTESIAN_POINT('Ctrl Pts',(-0.232716247486482,-0.20521673860449,
-1.02672656386641));
#73583=CARTESIAN_POINT('Ctrl Pts',(-0.148887914269599,-0.254297205873116,
-1.02144773752474));
#73584=CARTESIAN_POINT('Ctrl Pts',(-0.0650595810527136,-0.303377673141744,
-1.01616891118308));
#73585=CARTESIAN_POINT('Ctrl Pts',(0.0454235522067678,-0.30693234197877,
-1.01089008484141));
#73586=CARTESIAN_POINT('Ctrl Pts',(0.132233464149777,-0.26334196568222,
-1.00561125849974));
#73587=CARTESIAN_POINT('Ctrl Pts',(0.219043376092787,-0.219751589385669,
-1.00033243215807));
#73588=CARTESIAN_POINT('Ctrl Pts',(0.282180066719323,-0.12901616795554,
-0.995053605816403));
#73589=CARTESIAN_POINT('Ctrl Pts',(0.292883085265098,-0.0324681119873491,
-0.989774779474735));
#73590=CARTESIAN_POINT('Ctrl Pts',(0.303586103810872,0.0640799439808387,
-0.984495953133067));
#73591=CARTESIAN_POINT('Ctrl Pts',(0.261855450275889,0.166440634487089,
-0.979217126791399));
#73592=CARTESIAN_POINT('Ctrl Pts',(0.186700553162723,0.227985928028813,
-0.973938300449731));
#73593=CARTESIAN_POINT('Ctrl Pts',(0.111545656049556,0.289531221570537,
-0.968659474108062));
#73594=CARTESIAN_POINT('Ctrl Pts',(0.00296651535820849,0.310261118147735,
-0.963380647766395));
#73595=CARTESIAN_POINT('Ctrl Pts',(-0.0895761670770488,0.280732595582006,
-0.958101821424727));
#73596=CARTESIAN_POINT('Ctrl Pts',(-0.182118849512305,0.251204073016278,
-0.952822995083059));
#73597=CARTESIAN_POINT('Ctrl Pts',(-0.258625073691471,0.171417131307622,
-0.94754416874139));
#73598=CARTESIAN_POINT('Ctrl Pts',(-0.284244208835023,0.0777168557918905,
-0.942265342399722));
#73599=CARTESIAN_POINT('Ctrl Pts',(-0.291115886968034,0.0525841520253224,
-0.940849432169469));
#73600=CARTESIAN_POINT('Ctrl Pts',(-0.294326526593178,0.0264504625115664,
-0.939433521939215));
#73601=CARTESIAN_POINT('Ctrl Pts',(-0.294098243270401,0.000261754509978144,
-0.938017611708962));
#73602=CARTESIAN_POINT('Origin',(0.,0.,-0.975));
#73603=CARTESIAN_POINT('',(-0.293765004739316,-0.0001128917701812,-0.82358238829104));
#73604=CARTESIAN_POINT('',(-0.2937764249955,-0.000126456787260676,-0.838017611708961));
#73605=CARTESIAN_POINT('',(-0.2942,-3.60291088309151E-17,-0.975));
#73606=CARTESIAN_POINT('Ctrl Pts',(-0.293765004739316,-0.0001128917701812,
-0.82358238829104));
#73607=CARTESIAN_POINT('Ctrl Pts',(-0.293570292716816,0.0560165899656169,
-0.826608402285767));
#73608=CARTESIAN_POINT('Ctrl Pts',(-0.278094099980171,0.11224550982072,
-0.829634416280494));
#73609=CARTESIAN_POINT('Ctrl Pts',(-0.248027007594724,0.159114087410551,
-0.832660430275221));
#73610=CARTESIAN_POINT('Ctrl Pts',(-0.195575512136267,0.24087546802836,
-0.837939256616889));
#73611=CARTESIAN_POINT('Ctrl Pts',(-0.0987207464390296,0.294151298259528,
-0.843218082958558));
#73612=CARTESIAN_POINT('Ctrl Pts',(-0.0015826460346202,0.294673012915019,
-0.848496909300226));
#73613=CARTESIAN_POINT('Ctrl Pts',(0.0955554543697892,0.295194727570511,
-0.853775735641894));
#73614=CARTESIAN_POINT('Ctrl Pts',(0.192976889481371,0.242962326650326,
-0.859054561983562));
#73615=CARTESIAN_POINT('Ctrl Pts',(0.24630359069836,0.161769065392555,-0.86433338832523));
#73616=CARTESIAN_POINT('Ctrl Pts',(0.299630291915349,0.0805758041347841,
-0.869612214666898));
#73617=CARTESIAN_POINT('Ctrl Pts',(0.308862259237749,-0.0295783174605727,
-0.874891041008567));
#73618=CARTESIAN_POINT('Ctrl Pts',(0.269794084700736,-0.118515151644751,
-0.880169867350235));
#73619=CARTESIAN_POINT('Ctrl Pts',(0.230725910163722,-0.207451985828931,
-0.885448693691903));
#73620=CARTESIAN_POINT('Ctrl Pts',(0.143357593767295,-0.275171532601932,
-0.89072752003357));
#73621=CARTESIAN_POINT('Ctrl Pts',(0.0474877397325926,-0.290825727685801,
-0.896006346375238));
#73622=CARTESIAN_POINT('Ctrl Pts',(-0.0483821143021094,-0.306479922769669,
-0.901285172716907));
#73623=CARTESIAN_POINT('Ctrl Pts',(-0.152753505975086,-0.270068766164406,
-0.906563999058575));
#73624=CARTESIAN_POINT('Ctrl Pts',(-0.21808247563906,-0.198178513285434,
-0.911842825400243));
#73625=CARTESIAN_POINT('Ctrl Pts',(-0.266510762428707,-0.14488635512481,
-0.915756013030509));
#73626=CARTESIAN_POINT('Ctrl Pts',(-0.293484304810044,-0.0720975852474555,
-0.919669200660775));
#73627=CARTESIAN_POINT('Ctrl Pts',(-0.29412526541255,0.000263908637235785,
-0.92358238829104));
#73628=CARTESIAN_POINT('Ctrl Pts',(-0.294098243270401,0.000261754509978144,
-0.938017611708962));
#73629=CARTESIAN_POINT('Ctrl Pts',(-0.293475435901207,-0.0711868302342345,
-0.934154695597547));
#73630=CARTESIAN_POINT('Ctrl Pts',(-0.267256071083065,-0.143044928045731,
-0.930291779486133));
#73631=CARTESIAN_POINT('Ctrl Pts',(-0.219950575785256,-0.196103095697544,
-0.926428863374718));
#73632=CARTESIAN_POINT('Ctrl Pts',(-0.155305761483999,-0.268609162348436,
-0.92115003703305));
#73633=CARTESIAN_POINT('Ctrl Pts',(-0.0512840867735439,-0.306007686327414,
-0.915871210691381));
#73634=CARTESIAN_POINT('Ctrl Pts',(0.0447297941261825,-0.291262639979547,
-0.910592384349713));
#73635=CARTESIAN_POINT('Ctrl Pts',(0.140743675025909,-0.276517593631679,
-0.905313558008045));
#73636=CARTESIAN_POINT('Ctrl Pts',(0.228749762114909,-0.20962897695697,
-0.900034731666377));
#73637=CARTESIAN_POINT('Ctrl Pts',(0.268658929568512,-0.121066343355727,
-0.894755905324709));
#73638=CARTESIAN_POINT('Ctrl Pts',(0.308568097022116,-0.0325037097544837,
-0.889477078983041));
#73639=CARTESIAN_POINT('Ctrl Pts',(0.30038034484032,0.0777329407732916,
-0.884198252641374));
#73640=CARTESIAN_POINT('Ctrl Pts',(0.247825413070598,0.159427866343413,
-0.878919426299705));
#73641=CARTESIAN_POINT('Ctrl Pts',(0.195270481300876,0.241122791913534,
-0.873640599958037));
#73642=CARTESIAN_POINT('Ctrl Pts',(0.098348369943227,0.294275992526002,
-0.868361773616368));
#73643=CARTESIAN_POINT('Ctrl Pts',(0.00120969227830445,0.294674764062037,
-0.8630829472747));
#73644=CARTESIAN_POINT('Ctrl Pts',(-0.0959289853866181,0.295073535598073,
-0.857804120933032));
#73645=CARTESIAN_POINT('Ctrl Pts',(-0.193284229358815,0.242717878057679,
-0.852525294591365));
#73646=CARTESIAN_POINT('Ctrl Pts',(-0.24650812287037,0.161457193365153,
-0.847246468249697));
#73647=CARTESIAN_POINT('Ctrl Pts',(-0.277524845525826,0.114101767942294,
-0.844170182736118));
#73648=CARTESIAN_POINT('Ctrl Pts',(-0.293554187180766,0.0569299500855454,
-0.84109389722254));
#73649=CARTESIAN_POINT('Ctrl Pts',(-0.2937764249955,-0.000126456787260676,
-0.838017611708961));
#73650=CARTESIAN_POINT('Origin',(0.,0.,-0.975));
#73651=CARTESIAN_POINT('',(-0.294532285647886,-0.000180704995970699,-0.72358238829104));
#73652=CARTESIAN_POINT('',(-0.294553488267971,-0.000168236264217633,-0.738017611708961));
#73653=CARTESIAN_POINT('',(-0.2942,-3.60291088309151E-17,-0.975));
#73654=CARTESIAN_POINT('Ctrl Pts',(-0.294532285647886,-0.000180704995970699,
-0.72358238829104));
#73655=CARTESIAN_POINT('Ctrl Pts',(-0.293907652305694,0.0861696131302375,
-0.728268777569092));
#73656=CARTESIAN_POINT('Ctrl Pts',(-0.253640104222023,0.17302692605204,
-0.732955166847143));
#73657=CARTESIAN_POINT('Ctrl Pts',(-0.186988963747787,0.227749460472281,
-0.737641556125195));
#73658=CARTESIAN_POINT('Ctrl Pts',(-0.111912017475864,0.28938982772331,
-0.742920382466863));
#73659=CARTESIAN_POINT('Ctrl Pts',(-0.00335919464726699,0.310257131838362,
-0.748199208808531));
#73660=CARTESIAN_POINT('Ctrl Pts',(0.0892207913939141,0.280845757831465,
-0.7534780351502));
#73661=CARTESIAN_POINT('Ctrl Pts',(0.181800777435094,0.251434383824568,
-0.758756861491868));
#73662=CARTESIAN_POINT('Ctrl Pts',(0.258407926688858,0.171744331695723,
-0.764035687833536));
#73663=CARTESIAN_POINT('Ctrl Pts',(0.284145634305615,0.0780765509864899,
-0.769314514175204));
#73664=CARTESIAN_POINT('Ctrl Pts',(0.309883341922372,-0.0155912297227443,
-0.774593340516872));
#73665=CARTESIAN_POINT('Ctrl Pts',(0.28475160790212,-0.123236739012367,
-0.77987216685854));
#73666=CARTESIAN_POINT('Ctrl Pts',(0.220198609077346,-0.195824569115543,
-0.785150993200208));
#73667=CARTESIAN_POINT('Ctrl Pts',(0.155645610252571,-0.268412399218721,
-0.790429819541876));
#73668=CARTESIAN_POINT('Ctrl Pts',(0.0516713466232729,-0.305942550135451,
-0.795708645883544));
#73669=CARTESIAN_POINT('Ctrl Pts',(-0.0443611246057961,-0.291319034621144,
-0.800987472225212));
#73670=CARTESIAN_POINT('Ctrl Pts',(-0.140393595834861,-0.276695519106837,
-0.806266298566881));
#73671=CARTESIAN_POINT('Ctrl Pts',(-0.228484274663697,-0.209918337161498,
-0.811545124908549));
#73672=CARTESIAN_POINT('Ctrl Pts',(-0.268505501468278,-0.121406280686605,
-0.816823951250217));
#73673=CARTESIAN_POINT('Ctrl Pts',(-0.285585115012941,-0.0836325331196868,
-0.819076763597158));
#73674=CARTESIAN_POINT('Ctrl Pts',(-0.293909964296394,-0.0419002693904203,
-0.821329575944099));
#73675=CARTESIAN_POINT('Ctrl Pts',(-0.293765004739316,-0.0001128917701812,
-0.82358238829104));
#73676=CARTESIAN_POINT('Ctrl Pts',(-0.2937764249955,-0.000126456787260676,
-0.838017611708961));
#73677=CARTESIAN_POINT('Ctrl Pts',(-0.293935541520392,-0.0409773677598496,
-0.835815070880871));
#73678=CARTESIAN_POINT('Ctrl Pts',(-0.285991637114493,-0.08176911687534,
-0.833612530052781));
#73679=CARTESIAN_POINT('Ctrl Pts',(-0.269643855541951,-0.118856514751599,
-0.831409989224691));
#73680=CARTESIAN_POINT('Ctrl Pts',(-0.230463151651064,-0.207743826331163,
-0.826131162883023));
#73681=CARTESIAN_POINT('Ctrl Pts',(-0.143009200818376,-0.275352737645629,
-0.820852336541356));
#73682=CARTESIAN_POINT('Ctrl Pts',(-0.0471196160404858,-0.29088558182664,
-0.815573510199688));
#73683=CARTESIAN_POINT('Ctrl Pts',(0.0487699687374031,-0.30641842600765,
-0.81029468385802));
#73684=CARTESIAN_POINT('Ctrl Pts',(0.153095187460496,-0.269875203055206,
-0.805015857516351));
#73685=CARTESIAN_POINT('Ctrl Pts',(0.218333113494785,-0.197902328137137,
-0.799737031174683));
#73686=CARTESIAN_POINT('Ctrl Pts',(0.283571039529076,-0.125929453219066,
-0.794458204833014));
#73687=CARTESIAN_POINT('Ctrl Pts',(0.309721672874562,-0.0185269263353678,
-0.789179378491347));
#73688=CARTESIAN_POINT('Ctrl Pts',(0.284872700812218,0.0753805297300195,
-0.783900552149679));
#73689=CARTESIAN_POINT('Ctrl Pts',(0.260023728749873,0.169287985795408,
-0.778621725808011));
#73690=CARTESIAN_POINT('Ctrl Pts',(0.184175151279699,0.249700371042483,
-0.773342899466342));
#73691=CARTESIAN_POINT('Ctrl Pts',(0.0918780235207456,0.27998769388019,
-0.768064073124674));
#73692=CARTESIAN_POINT('Ctrl Pts',(-0.000419104238205001,0.310275016717896,
-0.762785246783006));
#73693=CARTESIAN_POINT('Ctrl Pts',(-0.109164782285933,0.290437277146233,
-0.757506420441339));
#73694=CARTESIAN_POINT('Ctrl Pts',(-0.184822446569363,0.229511095972593,
-0.752227594099671));
#73695=CARTESIAN_POINT('Ctrl Pts',(-0.252709637623149,0.174842380771212,
-0.747490933302768));
#73696=CARTESIAN_POINT('Ctrl Pts',(-0.293956442416001,0.0870918383276761,
-0.742754272505864));
#73697=CARTESIAN_POINT('Ctrl Pts',(-0.294553488267971,-0.000168236264217633,
-0.738017611708961));
#73698=CARTESIAN_POINT('Origin',(0.,0.,-0.975));
#73699=CARTESIAN_POINT('',(-0.294289870872604,0.000257612574092375,-0.62358238829104));
#73700=CARTESIAN_POINT('',(-0.294261921046506,0.000260993808666907,-0.63801761170896));
#73701=CARTESIAN_POINT('',(-0.2942,-3.60291088309151E-17,-0.975));
#73702=CARTESIAN_POINT('Ctrl Pts',(-0.294289870872604,0.000257612574092375,
-0.62358238829104));
#73703=CARTESIAN_POINT('Ctrl Pts',(-0.294469946841187,0.0199773350686368,
-0.624650326510748));
#73704=CARTESIAN_POINT('Ctrl Pts',(-0.292656187844798,0.0396641190350218,
-0.625718264730457));
#73705=CARTESIAN_POINT('Ctrl Pts',(-0.288726891356599,0.0589191948047397,
-0.626786202950165));
#73706=CARTESIAN_POINT('Ctrl Pts',(-0.269304350404941,0.154097173556868,
-0.632065029291833));
#73707=CARTESIAN_POINT('Ctrl Pts',(-0.198192203928323,0.238727087585969,
-0.637343855633501));
#73708=CARTESIAN_POINT('Ctrl Pts',(-0.107783936082899,0.274257748170153,
-0.642622681975169));
#73709=CARTESIAN_POINT('Ctrl Pts',(-0.0173756682374762,0.309788408754337,
-0.647901508316837));
#73710=CARTESIAN_POINT('Ctrl Pts',(0.0923287209767527,0.296219815893605,
-0.653180334658506));
#73711=CARTESIAN_POINT('Ctrl Pts',(0.171355948935814,0.239732826440589,
-0.658459161000174));
#73712=CARTESIAN_POINT('Ctrl Pts',(0.250383176894875,0.183245836987572,
-0.663737987341842));
#73713=CARTESIAN_POINT('Ctrl Pts',(0.298733243598769,0.0838404509422697,
-0.669016813683509));
#73714=CARTESIAN_POINT('Ctrl Pts',(0.29438140085294,-0.0132015203952617,
-0.674295640025178));
#73715=CARTESIAN_POINT('Ctrl Pts',(0.290029558107111,-0.110243491732796,
-0.679574466366846));
#73716=CARTESIAN_POINT('Ctrl Pts',(0.232975805911557,-0.204922048362555,
-0.684853292708514));
#73717=CARTESIAN_POINT('Ctrl Pts',(0.149209653926263,-0.254108576171862,
-0.690132119050183));
#73718=CARTESIAN_POINT('Ctrl Pts',(0.0654435019409706,-0.303295103981167,
-0.695410945391851));
#73719=CARTESIAN_POINT('Ctrl Pts',(-0.0450350498340619,-0.306989602970016,
-0.700689771733518));
#73720=CARTESIAN_POINT('Ctrl Pts',(-0.13190006702843,-0.263509130063423,
-0.705968598075186));
#73721=CARTESIAN_POINT('Ctrl Pts',(-0.218765084222795,-0.22002865715683,
-0.711247424416854));
#73722=CARTESIAN_POINT('Ctrl Pts',(-0.282016566836498,-0.129373212354797,
-0.716526250758523));
#73723=CARTESIAN_POINT('Ctrl Pts',(-0.292841773285728,-0.0328387747602788,
-0.721805077100191));
#73724=CARTESIAN_POINT('Ctrl Pts',(-0.294056674687428,-0.0220048175423813,
-0.722397514163807));
#73725=CARTESIAN_POINT('Ctrl Pts',(-0.294611249626576,-0.011096812446243,
-0.722989951227423));
#73726=CARTESIAN_POINT('Ctrl Pts',(-0.294532285647886,-0.000180704995970699,
-0.72358238829104));
#73727=CARTESIAN_POINT('Ctrl Pts',(-0.294553488267971,-0.000168236264217633,
-0.738017611708961));
#73728=CARTESIAN_POINT('Ctrl Pts',(-0.294621827062633,-0.010156159804845,
-0.737475446164196));
#73729=CARTESIAN_POINT('Ctrl Pts',(-0.294157595202237,-0.0201376575069966,
-0.73693328061943));
#73730=CARTESIAN_POINT('Ctrl Pts',(-0.293139784064339,-0.0300623839563357,
-0.736391115074665));
#73731=CARTESIAN_POINT('Ctrl Pts',(-0.283229806756751,-0.126695059936001,
-0.731112288732997));
#73732=CARTESIAN_POINT('Ctrl Pts',(-0.220840201622442,-0.217945789119709,
-0.725833462391329));
#73733=CARTESIAN_POINT('Ctrl Pts',(-0.134391102008002,-0.262247424451605,
-0.720554636049661));
#73734=CARTESIAN_POINT('Ctrl Pts',(-0.0479420023935621,-0.306549059783502,
-0.715275809707993));
#73735=CARTESIAN_POINT('Ctrl Pts',(0.0625665917010075,-0.303901601263588,
-0.709996983366325));
#73736=CARTESIAN_POINT('Ctrl Pts',(0.14679506082547,-0.255511037036901,
-0.704718157024657));
#73737=CARTESIAN_POINT('Ctrl Pts',(0.231023529949932,-0.207120472810213,
-0.699439330682989));
#73738=CARTESIAN_POINT('Ctrl Pts',(0.288971874104287,-0.112986802876749,
-0.694160504341321));
#73739=CARTESIAN_POINT('Ctrl Pts',(0.294243073071214,-0.0159904308895527,
-0.688881677999653));
#73740=CARTESIAN_POINT('Ctrl Pts',(0.299514272038142,0.0810059410976467,
-0.683602851657985));
#73741=CARTESIAN_POINT('Ctrl Pts',(0.252108325817643,0.180865015138582,
-0.678324025316316));
#73742=CARTESIAN_POINT('Ctrl Pts',(0.17361991047967,0.238098312920224,-0.673045198974648));
#73743=CARTESIAN_POINT('Ctrl Pts',(0.0951314951417017,0.295331610701864,
-0.66776637263298));
#73744=CARTESIAN_POINT('Ctrl Pts',(-0.0144393893137351,0.309939132224215,
-0.662487546291313));
#73745=CARTESIAN_POINT('Ctrl Pts',(-0.105180275250029,0.275266760849823,
-0.657208719949645));
#73746=CARTESIAN_POINT('Ctrl Pts',(-0.195921161186326,0.24059438947543,
-0.651929893607977));
#73747=CARTESIAN_POINT('Ctrl Pts',(-0.267832048603478,0.156642125204293,
-0.646651067266307));
#73748=CARTESIAN_POINT('Ctrl Pts',(-0.288155605489729,0.0616524691741799,
-0.641372240924639));
#73749=CARTESIAN_POINT('Ctrl Pts',(-0.292460728970111,0.0415308831320555,
-0.640254031186079));
#73750=CARTESIAN_POINT('Ctrl Pts',(-0.294451045139812,0.0209140313944282,
-0.63913582144752));
#73751=CARTESIAN_POINT('Ctrl Pts',(-0.294261921046506,0.000260993808666907,
-0.63801761170896));
#73752=CARTESIAN_POINT('Origin',(0.,0.,-0.975));
#73753=CARTESIAN_POINT('',(-0.293725317215226,-2.67421958787539E-5,-0.523582388291039));
#73754=CARTESIAN_POINT('',(-0.293728549452813,-4.17646313764225E-5,-0.538017611708961));
#73755=CARTESIAN_POINT('',(-0.2942,-3.60291088309151E-17,-0.975));
#73756=CARTESIAN_POINT('Ctrl Pts',(-0.293725317215226,-2.67421958787539E-5,
-0.523582388291039));
#73757=CARTESIAN_POINT('Ctrl Pts',(-0.293684051702583,0.0505977877572564,
-0.526310701794073));
#73758=CARTESIAN_POINT('Ctrl Pts',(-0.281256995427662,0.101241301522957,
-0.529039015297106));
#73759=CARTESIAN_POINT('Ctrl Pts',(-0.256560638597973,0.144952847612736,
-0.531767328800139));
#73760=CARTESIAN_POINT('Ctrl Pts',(-0.208777354590888,0.229527314834789,
-0.537046155141807));
#73761=CARTESIAN_POINT('Ctrl Pts',(-0.115063058962679,0.288151461053719,
-0.542324981483475));
#73762=CARTESIAN_POINT('Ctrl Pts',(-0.0181071191562859,0.294120420142335,
-0.547603807825143));
#73763=CARTESIAN_POINT('Ctrl Pts',(0.0788488206501062,0.30008937923095,
-0.552882634166811));
#73764=CARTESIAN_POINT('Ctrl Pts',(0.179046404634681,0.253403151189252,
-0.558161460508479));
#73765=CARTESIAN_POINT('Ctrl Pts',(0.23684295415351,0.17532856121226,-0.563440286850147));
#73766=CARTESIAN_POINT('Ctrl Pts',(0.29463950367234,0.0972539712352662,
-0.568719113191816));
#73767=CARTESIAN_POINT('Ctrl Pts',(0.31003501872542,-0.0122089806770256,
-0.573997939533484));
#73768=CARTESIAN_POINT('Ctrl Pts',(0.276016430552402,-0.103196993047219,
-0.579276765875152));
#73769=CARTESIAN_POINT('Ctrl Pts',(0.241997842379385,-0.194185005417411,
-0.58455559221682));
#73770=CARTESIAN_POINT('Ctrl Pts',(0.158565150980273,-0.266698078245509,
-0.589834418558488));
#73771=CARTESIAN_POINT('Ctrl Pts',(0.0637241781569158,-0.287704567963574,
-0.595113244900156));
#73772=CARTESIAN_POINT('Ctrl Pts',(-0.0311167946664433,-0.30871105768164,
-0.600392071241824));
#73773=CARTESIAN_POINT('Ctrl Pts',(-0.137366048914047,-0.278210964289672,
-0.605670897583492));
#73774=CARTESIAN_POINT('Ctrl Pts',(-0.206624208324501,-0.210097895856109,
-0.61094972392516));
#73775=CARTESIAN_POINT('Ctrl Pts',(-0.261871026828121,-0.155764509559018,
-0.61516061204712));
#73776=CARTESIAN_POINT('Ctrl Pts',(-0.293579830026457,-0.0774973958039037,
-0.61937150016908));
#73777=CARTESIAN_POINT('Ctrl Pts',(-0.294289870872604,0.000257612574092375,
-0.62358238829104));
#73778=CARTESIAN_POINT('Ctrl Pts',(-0.294261921046506,0.000260993808666907,
-0.63801761170896));
#73779=CARTESIAN_POINT('Ctrl Pts',(-0.293558231196988,-0.076584492436715,
-0.633856995105852));
#73780=CARTESIAN_POINT('Ctrl Pts',(-0.262681865646731,-0.15393094394333,
-0.629696378502744));
#73781=CARTESIAN_POINT('Ctrl Pts',(-0.208605769399056,-0.208130518915065,
-0.625535761899636));
#73782=CARTESIAN_POINT('Ctrl Pts',(-0.139996150066782,-0.276896803185108,
-0.620256935557968));
#73783=CARTESIAN_POINT('Ctrl Pts',(-0.0340406850468888,-0.308402323936105,
-0.614978109216299));
#73784=CARTESIAN_POINT('Ctrl Pts',(0.0609950782479923,-0.288295474053871,
-0.609699282874631));
#73785=CARTESIAN_POINT('Ctrl Pts',(0.156030841542874,-0.268188624171638,
-0.604420456532963));
#73786=CARTESIAN_POINT('Ctrl Pts',(0.24014690311274,-0.196469403656172,
-0.599141630191295));
#73787=CARTESIAN_POINT('Ctrl Pts',(0.27502614777056,-0.10580783512061,-0.593862803849627));
#73788=CARTESIAN_POINT('Ctrl Pts',(0.309905392428379,-0.0151462665850486,
-0.588583977507959));
#73789=CARTESIAN_POINT('Ctrl Pts',(0.295547820174153,0.0944576499706106,
-0.58330515116629));
#73790=CARTESIAN_POINT('Ctrl Pts',(0.238493689070395,0.173076399904854,
-0.578026324824622));
#73791=CARTESIAN_POINT('Ctrl Pts',(0.181439557966637,0.251695149839096,
-0.572747498482954));
#73792=CARTESIAN_POINT('Ctrl Pts',(0.081688868013349,0.299328733151925,
-0.567468672141286));
#73793=CARTESIAN_POINT('Ctrl Pts',(-0.0153192743263493,0.294278778991172,
-0.562189845799618));
#73794=CARTESIAN_POINT('Ctrl Pts',(-0.11232741666605,0.289228824830418,
-0.55691101945795));
#73795=CARTESIAN_POINT('Ctrl Pts',(-0.206593011392159,0.231495333196083,
-0.551632193116282));
#73796=CARTESIAN_POINT('Ctrl Pts',(-0.255175559581209,0.147377453237708,
-0.546353366774613));
#73797=CARTESIAN_POINT('Ctrl Pts',(-0.280747672014141,0.10310081555405,
-0.543574781752729));
#73798=CARTESIAN_POINT('Ctrl Pts',(-0.293662874536158,0.0515141394341178,
-0.540796196730845));
#73799=CARTESIAN_POINT('Ctrl Pts',(-0.293728549452813,-4.17646313764225E-5,
-0.538017611708961));
#73800=CARTESIAN_POINT('Origin',(0.,0.,-0.975));
#73801=CARTESIAN_POINT('',(-0.294386747729473,-0.000238138617797895,-0.423582388291039));
#73802=CARTESIAN_POINT('',(-0.294413163117196,-0.000230549972553652,-0.43801761170896));
#73803=CARTESIAN_POINT('',(-0.2942,-3.60291088309151E-17,-0.975));
#73804=CARTESIAN_POINT('Ctrl Pts',(-0.294386747729473,-0.000238138617797895,
-0.423582388291039));
#73805=CARTESIAN_POINT('Ctrl Pts',(-0.293675360816675,0.0807311351263202,
-0.427971077077397));
#73806=CARTESIAN_POINT('Ctrl Pts',(-0.258912863574874,0.162237187363098,
-0.432359765863755));
#73807=CARTESIAN_POINT('Ctrl Pts',(-0.199468139510034,0.216903551444156,
-0.436748454650113));
#73808=CARTESIAN_POINT('Ctrl Pts',(-0.127966515552986,0.282657642645915,
-0.442027280991781));
#73809=CARTESIAN_POINT('Ctrl Pts',(-0.0207549187866649,0.309580369841428,
-0.447306107333449));
#73810=CARTESIAN_POINT('Ctrl Pts',(0.0733289018073996,0.28540771094313,
-0.452584933675117));
#73811=CARTESIAN_POINT('Ctrl Pts',(0.167412722401464,0.261235052044833,
-0.457863760016785));
#73812=CARTESIAN_POINT('Ctrl Pts',(0.248368766823272,0.185967007052725,
-0.463142586358453));
#73813=CARTESIAN_POINT('Ctrl Pts',(0.279319392175962,0.0938901830065047,
-0.468421412700121));
#73814=CARTESIAN_POINT('Ctrl Pts',(0.310270017528652,0.00181335896028451,
-0.47370023904179));
#73815=CARTESIAN_POINT('Ctrl Pts',(0.291215223812225,-0.107072244140048,
-0.478979065383458));
#73816=CARTESIAN_POINT('Ctrl Pts',(0.230834979070049,-0.183166322631758,
-0.484257891725126));
#73817=CARTESIAN_POINT('Ctrl Pts',(0.170454734327874,-0.259260401123467,
-0.489536718066794));
#73818=CARTESIAN_POINT('Ctrl Pts',(0.0687490385599515,-0.302562955006556,
-0.494815544408462));
#73819=CARTESIAN_POINT('Ctrl Pts',(-0.0279524443521768,-0.293348513143104,
-0.50009437075013));
#73820=CARTESIAN_POINT('Ctrl Pts',(-0.124653927264306,-0.284134071279652,
-0.505373197091798));
#73821=CARTESIAN_POINT('Ctrl Pts',(-0.216351197320642,-0.222402633669659,
-0.510652023433466));
#73822=CARTESIAN_POINT('Ctrl Pts',(-0.26127369615583,-0.136274520752074,
-0.515930849775135));
#73823=CARTESIAN_POINT('Ctrl Pts',(-0.282978409023217,-0.0946609416066995,
-0.51848136261377));
#73824=CARTESIAN_POINT('Ctrl Pts',(-0.29376389350775,-0.0473521369687958,
-0.521031875452404));
#73825=CARTESIAN_POINT('Ctrl Pts',(-0.293725317215226,-2.67421958787539E-5,
-0.523582388291039));
#73826=CARTESIAN_POINT('Ctrl Pts',(-0.293728549452813,-4.17646313764225E-5,
-0.538017611708961));
#73827=CARTESIAN_POINT('Ctrl Pts',(-0.293787645409568,-0.0464330755353523,
-0.535517370389177));
#73828=CARTESIAN_POINT('Ctrl Pts',(-0.283442662454548,-0.092799470746512,
-0.533017129069394));
#73829=CARTESIAN_POINT('Ctrl Pts',(-0.262553264006026,-0.133792613735755,
-0.53051688774961));
#73830=CARTESIAN_POINT('Ctrl Pts',(-0.218448918589804,-0.220342532468435,
-0.525238061407942));
#73831=CARTESIAN_POINT('Ctrl Pts',(-0.12734072610537,-0.282940101651383,
-0.519959235066273));
#73832=CARTESIAN_POINT('Ctrl Pts',(-0.0307309043311849,-0.29307045475341,
-0.514680408724605));
#73833=CARTESIAN_POINT('Ctrl Pts',(0.0658789174429986,-0.303200807855436,
-0.509401582382937));
#73834=CARTESIAN_POINT('Ctrl Pts',(0.167990368506934,-0.260863944876541,
-0.504122756041269));
#73835=CARTESIAN_POINT('Ctrl Pts',(0.229088952588978,-0.185345438929759,
-0.498843929699601));
#73836=CARTESIAN_POINT('Ctrl Pts',(0.290187536671023,-0.109826932982976,
-0.493565103357933));
#73837=CARTESIAN_POINT('Ctrl Pts',(0.310273253771179,-0.00112678406830562,
-0.488286277016264));
#73838=CARTESIAN_POINT('Ctrl Pts',(0.280196522685982,0.0912391834978892,
-0.483007450674596));
#73839=CARTESIAN_POINT('Ctrl Pts',(0.250119791600785,0.183605151064081,
-0.477728624332928));
#73840=CARTESIAN_POINT('Ctrl Pts',(0.169880612330235,0.2596369372818,-0.47244979799126));
#73841=CARTESIAN_POINT('Ctrl Pts',(0.0760300765142607,0.284700030550235,
-0.467170971649592));
#73842=CARTESIAN_POINT('Ctrl Pts',(-0.0178204593017165,0.309763123818671,
-0.461892145307924));
#73843=CARTESIAN_POINT('Ctrl Pts',(-0.125282351663119,0.283857524137824,
-0.456613318966256));
#73844=CARTESIAN_POINT('Ctrl Pts',(-0.197403835228254,0.218783924837785,
-0.451334492624587));
#73845=CARTESIAN_POINT('Ctrl Pts',(-0.258050725649971,0.164063593932058,
-0.446895532319378));
#73846=CARTESIAN_POINT('Ctrl Pts',(-0.29370801395702,0.0816471282206012,
-0.442456572014169));
#73847=CARTESIAN_POINT('Ctrl Pts',(-0.294413163117196,-0.000230549972553652,
-0.43801761170896));
#73848=CARTESIAN_POINT('Origin',(0.,0.,-0.975));
#73849=CARTESIAN_POINT('',(-0.294448752700369,0.000218575078071742,-0.323582388291039));
#73850=CARTESIAN_POINT('',(-0.294423182665938,0.000227389813808373,-0.33801761170896));
#73851=CARTESIAN_POINT('',(-0.2942,-3.60291088309151E-17,-0.975));
#73852=CARTESIAN_POINT('Ctrl Pts',(-0.294448752700369,0.000218575078071742,
-0.323582388291039));
#73853=CARTESIAN_POINT('Ctrl Pts',(-0.294566832082909,0.0144213289353346,
-0.324352626019054));
#73854=CARTESIAN_POINT('Ctrl Pts',(-0.293627558021379,0.0286084018818293,
-0.325122863747068));
#73855=CARTESIAN_POINT('Ctrl Pts',(-0.291576951458356,0.0426329811729054,
-0.325893101475082));
#73856=CARTESIAN_POINT('Ctrl Pts',(-0.277523113860461,0.138750473084658,
-0.33117192781675));
#73857=CARTESIAN_POINT('Ctrl Pts',(-0.211269433961597,0.227235556895007,
-0.336450754158418));
#73858=CARTESIAN_POINT('Ctrl Pts',(-0.122996237149932,0.267780908662382,
-0.341729580500087));
#73859=CARTESIAN_POINT('Ctrl Pts',(-0.0347230403382674,0.308326260429757,
-0.347008406841755));
#73860=CARTESIAN_POINT('Ctrl Pts',(0.0755696733861977,0.300931880154159,
-0.352287233183423));
#73861=CARTESIAN_POINT('Ctrl Pts',(0.157640625250177,0.248966106971692,
-0.357566059525091));
#73862=CARTESIAN_POINT('Ctrl Pts',(0.239711577114155,0.197000333789225,
-0.362844885866759));
#73863=CARTESIAN_POINT('Ctrl Pts',(0.293560767117647,0.100463167699891,
-0.368123712208427));
#73864=CARTESIAN_POINT('Ctrl Pts',(0.294658448633633,0.00332986849060328,
-0.373402538550095));
#73865=CARTESIAN_POINT('Ctrl Pts',(0.295756130149619,-0.0938034307186845,
-0.378681364891763));
#73866=CARTESIAN_POINT('Ctrl Pts',(0.244102303178098,-0.191532863047926,
-0.383960191233431));
#73867=CARTESIAN_POINT('Ctrl Pts',(0.163226667435956,-0.245340058596889,
-0.3892390175751));
#73868=CARTESIAN_POINT('Ctrl Pts',(0.0823510316938124,-0.299147254145853,
-0.394517843916768));
#73869=CARTESIAN_POINT('Ctrl Pts',(-0.0277464128189549,-0.309032212914535,
-0.399796670258436));
#73870=CARTESIAN_POINT('Ctrl Pts',(-0.116913336480491,-0.270492072047274,
-0.405075496600104));
#73871=CARTESIAN_POINT('Ctrl Pts',(-0.206080260142024,-0.231951931180014,
-0.410354322941772));
#73872=CARTESIAN_POINT('Ctrl Pts',(-0.274316662952327,-0.144986690676814,
-0.41563314928344));
#73873=CARTESIAN_POINT('Ctrl Pts',(-0.290539038783592,-0.049211342821212,
-0.420911975625108));
#73874=CARTESIAN_POINT('Ctrl Pts',(-0.293274522966844,-0.0330613070971267,
-0.421802113180419));
#73875=CARTESIAN_POINT('Ctrl Pts',(-0.294531035064088,-0.0166607638925458,
-0.422692250735729));
#73876=CARTESIAN_POINT('Ctrl Pts',(-0.294386747729473,-0.000238138617797895,
-0.423582388291039));
#73877=CARTESIAN_POINT('Ctrl Pts',(-0.294413163117196,-0.000230549972553652,
-0.43801761170896));
#73878=CARTESIAN_POINT('Ctrl Pts',(-0.294546579680884,-0.0157220786933341,
-0.437177745672501));
#73879=CARTESIAN_POINT('Ctrl Pts',(-0.293428783164059,-0.0311943199539772,
-0.436337879636042));
#73880=CARTESIAN_POINT('Ctrl Pts',(-0.290992296495885,-0.0464560363369899,
-0.435498013599583));
#73881=CARTESIAN_POINT('Ctrl Pts',(-0.275678199429516,-0.142380799292502,
-0.430219187257915));
#73882=CARTESIAN_POINT('Ctrl Pts',(-0.208268930527908,-0.229988726284298,
-0.424940360916247));
#73883=CARTESIAN_POINT('Ctrl Pts',(-0.1194712142193,-0.269372064068582,
-0.419661534574579));
#73884=CARTESIAN_POINT('Ctrl Pts',(-0.0306734979106905,-0.308755401852867,
-0.414382708232911));
#73885=CARTESIAN_POINT('Ctrl Pts',(0.0795126658049214,-0.299914150429641,
-0.409103881891243));
#73886=CARTESIAN_POINT('Ctrl Pts',(0.160894533168858,-0.246875736204659,
-0.403825055549575));
#73887=CARTESIAN_POINT('Ctrl Pts',(0.242276400532795,-0.193837321979676,
-0.398546229207906));
#73888=CARTESIAN_POINT('Ctrl Pts',(0.294853971545057,-0.0966017449529404,
-0.393267402866238));
#73889=CARTESIAN_POINT('Ctrl Pts',(0.29467675669896,0.000537589563172465,
-0.38798857652457));
#73890=CARTESIAN_POINT('Ctrl Pts',(0.294499541852863,0.0976769240792826,
-0.382709750182902));
#73891=CARTESIAN_POINT('Ctrl Pts',(0.241567541148409,0.194720016084768,
-0.377430923841234));
#73892=CARTESIAN_POINT('Ctrl Pts',(0.159992696350693,0.247461142451306,
-0.372152097499566));
#73893=CARTESIAN_POINT('Ctrl Pts',(0.0784178515529763,0.300202268817844,
-0.366873271157898));
#73894=CARTESIAN_POINT('Ctrl Pts',(-0.0317998373380048,0.308641429545435,
-0.36159444481623));
#73895=CARTESIAN_POINT('Ctrl Pts',(-0.120453266197856,0.268934361133685,
-0.356315618474562));
#73896=CARTESIAN_POINT('Ctrl Pts',(-0.209106695057707,0.229227292721936,
-0.351036792132893));
#73897=CARTESIAN_POINT('Ctrl Pts',(-0.27619586388643,0.141373995170845,
-0.345757965791225));
#73898=CARTESIAN_POINT('Ctrl Pts',(-0.291159861981142,0.0453939948487563,
-0.340479139449557));
#73899=CARTESIAN_POINT('Ctrl Pts',(-0.293485776495486,0.0304754366918415,
-0.339658630202691));
#73900=CARTESIAN_POINT('Ctrl Pts',(-0.29455236057389,0.0153605395301952,
-0.338838120955826));
#73901=CARTESIAN_POINT('Ctrl Pts',(-0.294423182665938,0.000227389813808373,
-0.33801761170896));
#73902=CARTESIAN_POINT('Origin',(0.,0.,-0.975));
#73903=CARTESIAN_POINT('',(-0.293735363568813,6.2383603337629E-5,-0.223582388291039));
#73904=CARTESIAN_POINT('',(-0.293730171905116,4.7521135793488E-5,-0.23801761170896));
#73905=CARTESIAN_POINT('',(-0.2942,-3.60291088309151E-17,-0.975));
#73906=CARTESIAN_POINT('Ctrl Pts',(-0.293735363568813,6.2383603337629E-5,
-0.223582388291039));
#73907=CARTESIAN_POINT('Ctrl Pts',(-0.29382126570124,0.0451591115892455,
-0.226013001302378));
#73908=CARTESIAN_POINT('Ctrl Pts',(-0.284069503228078,0.0902206310502946,
-0.228443614313717));
#73909=CARTESIAN_POINT('Ctrl Pts',(-0.264286630962371,0.130335250310531,
-0.230874227325056));
#73910=CARTESIAN_POINT('Ctrl Pts',(-0.221322018026089,0.21745652706214,
-0.236153053666724));
#73911=CARTESIAN_POINT('Ctrl Pts',(-0.131043140145507,0.281244498566885,
-0.241431880008393));
#73912=CARTESIAN_POINT('Ctrl Pts',(-0.0345745696175421,0.292641926382959,
-0.246710706350061));
#73913=CARTESIAN_POINT('Ctrl Pts',(0.0618940009104224,0.304039354199033,
-0.251989532691729));
#73914=CARTESIAN_POINT('Ctrl Pts',(0.16455226408577,0.263046238326436,-0.257268359033397));
#73915=CARTESIAN_POINT('Ctrl Pts',(0.226636703894443,0.188336097685639,
-0.262547185375065));
#73916=CARTESIAN_POINT('Ctrl Pts',(0.288721143703115,0.113625957044842,
-0.267826011716733));
#73917=CARTESIAN_POINT('Ctrl Pts',(0.310231760145113,0.00519879163584851,
-0.273104838058401));
#73918=CARTESIAN_POINT('Ctrl Pts',(0.281369856774462,-0.0875539561617508,
-0.278383664400069));
#73919=CARTESIAN_POINT('Ctrl Pts',(0.252507953403812,-0.180306703959349,
-0.283662490741737));
#73920=CARTESIAN_POINT('Ctrl Pts',(0.173273530220512,-0.257385034145551,
-0.288941317083405));
#73921=CARTESIAN_POINT('Ctrl Pts',(0.0797600041809775,-0.283677690310886,
-0.294220143425073));
#73922=CARTESIAN_POINT('Ctrl Pts',(-0.0137535218585596,-0.309970346476223,
-0.299498969766742));
#73923=CARTESIAN_POINT('Ctrl Pts',(-0.121546150754334,-0.285477328620691,
-0.30477779610841));
#73924=CARTESIAN_POINT('Ctrl Pts',(-0.194515467553757,-0.221355869686345,
-0.310056622450078));
#73925=CARTESIAN_POINT('Ctrl Pts',(-0.256837773607114,-0.166590423556724,
-0.314565211063732));
#73926=CARTESIAN_POINT('Ctrl Pts',(-0.293757574716917,-0.0829172828452477,
-0.319073799677386));
#73927=CARTESIAN_POINT('Ctrl Pts',(-0.294448752700369,0.000218575078071742,
-0.323582388291039));
#73928=CARTESIAN_POINT('Ctrl Pts',(-0.294423182665938,0.000227389813808373,
-0.33801761170896));
#73929=CARTESIAN_POINT('Ctrl Pts',(-0.293721281892129,-0.0820000565391896,
-0.333559294614158));
#73930=CARTESIAN_POINT('Ctrl Pts',(-0.257715724385328,-0.164766391010743,
-0.329100977519356));
#73931=CARTESIAN_POINT('Ctrl Pts',(-0.196604252665232,-0.219502728012081,
-0.324642660424553));
#73932=CARTESIAN_POINT('Ctrl Pts',(-0.124245817893906,-0.284312747457746,
-0.319363834082885));
#73933=CARTESIAN_POINT('Ctrl Pts',(-0.0166901209905529,-0.309826083255983,
-0.314085007741217));
#73934=CARTESIAN_POINT('Ctrl Pts',(0.0770683438040029,-0.284420727799746,
-0.308806181399548));
#73935=CARTESIAN_POINT('Ctrl Pts',(0.170826808598556,-0.259015372343509,
-0.30352735505788));
#73936=CARTESIAN_POINT('Ctrl Pts',(0.250788041284313,-0.182691325632801,
-0.298248528716212));
#73937=CARTESIAN_POINT('Ctrl Pts',(0.280527559302708,-0.090216233574742,
-0.292969702374544));
#73938=CARTESIAN_POINT('Ctrl Pts',(0.310267077321103,0.00225885848331649,
-0.287690876032876));
#73939=CARTESIAN_POINT('Ctrl Pts',(0.289784880672137,0.110884995888725,
-0.282412049691208));
#73940=CARTESIAN_POINT('Ctrl Pts',(0.228411163365634,0.18618007205291,-0.27713322334954));
#73941=CARTESIAN_POINT('Ctrl Pts',(0.16703744605913,0.261475148217097,-0.271854397007872));
#73942=CARTESIAN_POINT('Ctrl Pts',(0.0647722080950876,0.303439163140058,
-0.266575570666204));
#73943=CARTESIAN_POINT('Ctrl Pts',(-0.0318000112318368,0.292956379272552,
-0.261296744324536));
#73944=CARTESIAN_POINT('Ctrl Pts',(-0.128372230558761,0.282473595405046,
-0.256017917982867));
#73945=CARTESIAN_POINT('Ctrl Pts',(-0.219251431248568,0.219544012747072,
-0.250739091641199));
#73946=CARTESIAN_POINT('Ctrl Pts',(-0.263039686358181,0.132833751630507,
-0.245460265299531));
#73947=CARTESIAN_POINT('Ctrl Pts',(-0.283618807108558,0.0920826203203491,
-0.242979380769341));
#73948=CARTESIAN_POINT('Ctrl Pts',(-0.293796911898982,0.0460790309603713,
-0.240498496239151));
#73949=CARTESIAN_POINT('Ctrl Pts',(-0.293730171905116,4.7521135793488E-5,
-0.23801761170896));
#73950=CARTESIAN_POINT('Origin',(0.,0.,-0.975));
#73951=CARTESIAN_POINT('',(-0.294218898388376,-0.000260431939339084,-0.123582388291039));
#73952=CARTESIAN_POINT('',(-0.29425044853364,-0.000261621567235155,-0.138017611708961));
#73953=CARTESIAN_POINT('',(-0.2942,-3.60291088309151E-17,-0.975));
#73954=CARTESIAN_POINT('Ctrl Pts',(-0.294218898388376,-0.000260431939339084,
-0.123582388291039));
#73955=CARTESIAN_POINT('Ctrl Pts',(-0.293528319942296,0.0753241966819701,
-0.127673376585703));
#73956=CARTESIAN_POINT('Ctrl Pts',(-0.263787073930481,0.151388528324872,
-0.131764364880366));
#73957=CARTESIAN_POINT('Ctrl Pts',(-0.211321206681247,0.205373225174826,
-0.13585535317503));
#73958=CARTESIAN_POINT('Ctrl Pts',(-0.143621623567071,0.275032637339418,
-0.141134179516698));
#73959=CARTESIAN_POINT('Ctrl Pts',(-0.0380851942254879,0.30792911569359,
-0.146413005858366));
#73960=CARTESIAN_POINT('Ctrl Pts',(0.0572071270478631,0.289072004190402,
-0.151691832200035));
#73961=CARTESIAN_POINT('Ctrl Pts',(0.152499448321213,0.270214892687215,
-0.156970658541703));
#73962=CARTESIAN_POINT('Ctrl Pts',(0.237547661526332,0.199604191326667,
-0.162249484883371));
#73963=CARTESIAN_POINT('Ctrl Pts',(0.273613323874537,0.109407805679064,
-0.167528311225039));
#73964=CARTESIAN_POINT('Ctrl Pts',(0.309678986222741,0.0192114200314617,
-0.172807137566707));
#73965=CARTESIAN_POINT('Ctrl Pts',(0.296762097714034,-0.0905706499031973,
-0.178085963908375));
#73966=CARTESIAN_POINT('Ctrl Pts',(0.240744922753791,-0.169931224311318,
-0.183364790250043));
#73967=CARTESIAN_POINT('Ctrl Pts',(0.184727747793547,-0.249291798719439,
-0.188643616591711));
#73968=CARTESIAN_POINT('Ctrl Pts',(0.0856102863817663,-0.29823087760102,
-0.193922442933379));
#73969=CARTESIAN_POINT('Ctrl Pts',(-0.0114559051328922,-0.294454622701047,
-0.199201269275047));
#73970=CARTESIAN_POINT('Ctrl Pts',(-0.108522096647551,-0.290678367801075,
-0.204480095616716));
#73971=CARTESIAN_POINT('Ctrl Pts',(-0.203537018265085,-0.234186779119548,
-0.209758921958384));
#73972=CARTESIAN_POINT('Ctrl Pts',(-0.253219305077861,-0.150713693779547,
-0.215037748300052));
#73973=CARTESIAN_POINT('Ctrl Pts',(-0.28002559542017,-0.105675433567722,
-0.217885961630381));
#73974=CARTESIAN_POINT('Ctrl Pts',(-0.293634702707729,-0.0527823519446433,
-0.22073417496071));
#73975=CARTESIAN_POINT('Ctrl Pts',(-0.293735363568813,6.2383603337629E-5,
-0.223582388291039));
#73976=CARTESIAN_POINT('Ctrl Pts',(-0.293730171905116,4.7521135793488E-5,
-0.23801761170896));
#73977=CARTESIAN_POINT('Ctrl Pts',(-0.293654902533621,-0.0518668200664407,
-0.235219669897483));
#73978=CARTESIAN_POINT('Ctrl Pts',(-0.280548876420359,-0.103816674230558,
-0.232421728086005));
#73979=CARTESIAN_POINT('Ctrl Pts',(-0.254636118965327,-0.14830751416629,
-0.229623786274527));
#73980=CARTESIAN_POINT('Ctrl Pts',(-0.20574698693344,-0.232247579271372,
-0.224344959932859));
#73981=CARTESIAN_POINT('Ctrl Pts',(-0.111271413340247,-0.289636769906379,
-0.219066133591191));
#73982=CARTESIAN_POINT('Ctrl Pts',(-0.0142454713261084,-0.294332728605281,
-0.213787307249522));
#73983=CARTESIAN_POINT('Ctrl Pts',(0.0827804706880292,-0.299028687304183,
-0.208508480907854));
#73984=CARTESIAN_POINT('Ctrl Pts',(0.182356781123111,-0.25103141406698,
-0.203229654566186));
#73985=CARTESIAN_POINT('Ctrl Pts',(0.239123641436347,-0.172205039277174,
-0.197950828224518));
#73986=CARTESIAN_POINT('Ctrl Pts',(0.295890501749582,-0.093378664487369,
-0.19267200188285));
#73987=CARTESIAN_POINT('Ctrl Pts',(0.309847911940974,0.0162768118550433,
-0.187393175541182));
#73988=CARTESIAN_POINT('Ctrl Pts',(0.274638178457899,0.106810558300942,
-0.182114349199514));
#73989=CARTESIAN_POINT('Ctrl Pts',(0.239428444974822,0.197344304746844,
-0.176835522857845));
#73990=CARTESIAN_POINT('Ctrl Pts',(0.155051567817281,0.268756321296234,
-0.171556696516177));
#73991=CARTESIAN_POINT('Ctrl Pts',(0.0599429359410212,0.288516200200336,
-0.166277870174509));
#73992=CARTESIAN_POINT('Ctrl Pts',(-0.0351656959352371,0.308276079104439,
-0.160999043832841));
#73993=CARTESIAN_POINT('Ctrl Pts',(-0.141006082530208,0.276383820363254,
-0.155720217491173));
#73994=CARTESIAN_POINT('Ctrl Pts',(-0.209364076589891,0.207367820782157,
-0.150441391149505));
#73995=CARTESIAN_POINT('Ctrl Pts',(-0.262991189021549,0.153224500457582,
-0.14630013133599));
#73996=CARTESIAN_POINT('Ctrl Pts',(-0.293549899495509,0.0762335090548516,
-0.142158871522476));
#73997=CARTESIAN_POINT('Ctrl Pts',(-0.29425044853364,-0.000261621567235155,
-0.138017611708961));
#73998=CARTESIAN_POINT('Origin',(0.,0.,-0.975));
#73999=CARTESIAN_POINT('',(-0.2942,-3.60291088309151E-17,-0.025));
#74000=CARTESIAN_POINT('',(-0.294543724507234,0.000174101626290112,-0.0380176117089602));
#74001=CARTESIAN_POINT('',(-0.2942,-3.60291088309151E-17,-0.975));
#74002=CARTESIAN_POINT('',(-0.293033728012268,0.0261701021632011,-0.0249999999999999));
#74003=CARTESIAN_POINT('Origin',(0.,0.,-0.025));
#74004=CARTESIAN_POINT('Ctrl Pts',(-0.293033728012268,0.0261701021632011,
-0.0249999999999999));
#74005=CARTESIAN_POINT('Ctrl Pts',(-0.284353669323579,0.123363072257456,
-0.030278826341668));
#74006=CARTESIAN_POINT('Ctrl Pts',(-0.223613800042068,0.215068700053739,
-0.0355576526833361));
#74007=CARTESIAN_POINT('Ctrl Pts',(-0.137883282056386,0.260401867148505,
-0.0408364790250042));
#74008=CARTESIAN_POINT('Ctrl Pts',(-0.0521527640707002,0.305735034243272,
-0.0461153053666725));
#74009=CARTESIAN_POINT('Ctrl Pts',(0.0585684026191602,0.30469574063652,
-0.0513941317083408));
#74010=CARTESIAN_POINT('Ctrl Pts',(0.14347220086852,0.257453935168375,-0.0566729580500089));
#74011=CARTESIAN_POINT('Ctrl Pts',(0.228375999117877,0.21021212970023,-0.0619517843916768));
#74012=CARTESIAN_POINT('Ctrl Pts',(0.287462428926736,0.116767812370693,
-0.0672306107333447));
#74013=CARTESIAN_POINT('Ctrl Pts',(0.293983851229169,0.0198299008762353,
-0.0725094370750127));
#74014=CARTESIAN_POINT('Ctrl Pts',(0.300505273531603,-0.0771080106182236,
-0.0777882634166808));
#74015=CARTESIAN_POINT('Ctrl Pts',(0.254461688327612,-0.177539516277601,
-0.0830670897583489));
#74016=CARTESIAN_POINT('Ctrl Pts',(0.176742574349081,-0.235788167911957,
-0.0883459161000171));
#74017=CARTESIAN_POINT('Ctrl Pts',(0.0990234603705489,-0.294036819546313,
-0.0936247424416854));
#74018=CARTESIAN_POINT('Ctrl Pts',(-0.0103711823825235,-0.310102617155643,
-0.0989035687833535));
#74019=CARTESIAN_POINT('Ctrl Pts',(-0.101565243497955,-0.276629259989442,
-0.104182395125022));
#74020=CARTESIAN_POINT('Ctrl Pts',(-0.192759304613383,-0.243155902823242,
-0.10946122146669));
#74021=CARTESIAN_POINT('Ctrl Pts',(-0.265752784091173,-0.160143390881513,
-0.114740047808358));
#74022=CARTESIAN_POINT('Ctrl Pts',(-0.287318155386683,-0.0654259619231444,
-0.120018874150026));
#74023=CARTESIAN_POINT('Ctrl Pts',(-0.292170781115319,-0.0441127080767178,
-0.12120671219703));
#74024=CARTESIAN_POINT('Ctrl Pts',(-0.294419411148035,-0.0222067909064837,
-0.122394550244035));
#74025=CARTESIAN_POINT('Ctrl Pts',(-0.294218898388376,-0.000260431939339084,
-0.123582388291039));
#74026=CARTESIAN_POINT('Ctrl Pts',(-0.29425044853364,-0.000261621567235155,
-0.138017611708961));
#74027=CARTESIAN_POINT('Ctrl Pts',(-0.294442883003582,-0.0212741404819942,
-0.136880045180808));
#74028=CARTESIAN_POINT('Ctrl Pts',(-0.292382366633133,-0.0422492441672564,
-0.135742478652654));
#74029=CARTESIAN_POINT('Ctrl Pts',(-0.287928169201029,-0.0627030951006328,
-0.134604912124501));
#74030=CARTESIAN_POINT('Ctrl Pts',(-0.267258666228093,-0.157618270981318,
-0.129326085782833));
#74031=CARTESIAN_POINT('Ctrl Pts',(-0.195044058757831,-0.241308882321678,
-0.124047259441165));
#74032=CARTESIAN_POINT('Ctrl Pts',(-0.104176307233433,-0.275649355995977,
-0.118768433099497));
#74033=CARTESIAN_POINT('Ctrl Pts',(-0.0133085557090344,-0.309989829670276,
-0.113489606757829));
#74034=CARTESIAN_POINT('Ctrl Pts',(0.0962123398695022,-0.294980165678509,
-0.10821078041616));
#74035=CARTESIAN_POINT('Ctrl Pts',(0.174489570858358,-0.23746198694934,
-0.102931954074492));
#74036=CARTESIAN_POINT('Ctrl Pts',(0.252766801847212,-0.179943808220172,
-0.097653127732824));
#74037=CARTESIAN_POINT('Ctrl Pts',(0.29980036824639,-0.0799171147536053,
-0.0923743013911559));
#74038=CARTESIAN_POINT('Ctrl Pts',(0.294178806556978,0.0170615097418389,
-0.0870954750494878));
#74039=CARTESIAN_POINT('Ctrl Pts',(0.288557244867566,0.114040134237284,
-0.0818166487078195));
#74040=CARTESIAN_POINT('Ctrl Pts',(0.230280555089563,0.207970689761605,
-0.0765378223661514));
#74041=CARTESIAN_POINT('Ctrl Pts',(0.145869376933614,0.256049538454383,
-0.0712589960244833));
#74042=CARTESIAN_POINT('Ctrl Pts',(0.0614581987776668,0.304128387147161,
-0.0659801696828152));
#74043=CARTESIAN_POINT('Ctrl Pts',(-0.049087467756228,0.306355529008397,
-0.060701343341147));
#74044=CARTESIAN_POINT('Ctrl Pts',(-0.135361470776523,0.261746566404462,
-0.0554225169994788));
#74045=CARTESIAN_POINT('Ctrl Pts',(-0.221635473796818,0.217137603800527,
-0.0501436906578107));
#74046=CARTESIAN_POINT('Ctrl Pts',(-0.283637813303516,0.125692536731422,
-0.0448648643161426));
#74047=CARTESIAN_POINT('Ctrl Pts',(-0.293220335795911,0.0290092329209717,
-0.0395860379744745));
#74048=CARTESIAN_POINT('Ctrl Pts',(-0.294169377558491,0.0194338321709952,
-0.0390632292193031));
#74049=CARTESIAN_POINT('Ctrl Pts',(-0.294604249652088,0.00980705118726834,
-0.0385404204641317));
#74050=CARTESIAN_POINT('Ctrl Pts',(-0.294543724507234,0.000174101626290112,
-0.0380176117089602));
#74051=CARTESIAN_POINT('Origin',(0.,0.,-2.1406589891905));
#74052=CARTESIAN_POINT('',(-0.237190235300011,-0.000209952227111018,-0.0906589891905002));
#74053=CARTESIAN_POINT('',(-0.237452100135973,0.00014035538139405,-0.0709410108094966));
#74054=CARTESIAN_POINT('',(-0.237175,-2.3095687792789E-14,-2.1406589891905));
#74055=CARTESIAN_POINT('',(0.131476569578105,0.197850242677352,-0.0250000000000002));
#74056=CARTESIAN_POINT('Ctrl Pts',(-0.237190235300011,-0.000209952227111019,
-0.0906589891905003));
#74057=CARTESIAN_POINT('Ctrl Pts',(-0.237351882525612,-0.0179024324719509,
-0.0894711511434962));
#74058=CARTESIAN_POINT('Ctrl Pts',(-0.227483014572861,-0.114043905631837,
-0.0830044867548241));
#74059=CARTESIAN_POINT('Ctrl Pts',(-0.0965515281323339,-0.262946953677372,
-0.0712589960244833));
#74060=CARTESIAN_POINT('Ctrl Pts',(0.168020270592608,-0.224091696559834,
-0.0554225169994791));
#74061=CARTESIAN_POINT('Ctrl Pts',(0.276446148350078,0.0124097424002016,
-0.0400028516579843));
#74062=CARTESIAN_POINT('Ctrl Pts',(0.19136777761438,0.157552650588978,-0.0298620126581583));
#74063=CARTESIAN_POINT('Ctrl Pts',(0.131476569578105,0.197850242677352,
-0.0250000000000002));
#74064=CARTESIAN_POINT('',(0.229503519150545,-0.0598340649004849,-0.0249999999999999));
#74065=CARTESIAN_POINT('Origin',(0.,0.,-0.0249999999999999));
#74066=CARTESIAN_POINT('Ctrl Pts',(-0.237452100135973,0.000140355381394047,
-0.0709410108094966));
#74067=CARTESIAN_POINT('Ctrl Pts',(-0.237008223098924,-0.0705054087783698,
-0.0661849932230005));
#74068=CARTESIAN_POINT('Ctrl Pts',(-0.16633709501764,-0.220431044668647,
-0.0561501492948366));
#74069=CARTESIAN_POINT('Ctrl Pts',(0.0886436604710861,-0.265605608028242,
-0.0408364790250042));
#74070=CARTESIAN_POINT('Ctrl Pts',(0.209657849780202,-0.135955434357285,
-0.030278826341668));
#74071=CARTESIAN_POINT('Ctrl Pts',(0.229503519150545,-0.0598340649004849,
-0.0249999999999999));
#74072=CARTESIAN_POINT('Origin',(0.,0.,-2.1406589891905));
#74073=CARTESIAN_POINT('',(-0.236800424386245,5.02917441071152E-5,-0.1906589891905));
#74074=CARTESIAN_POINT('',(-0.237215670057668,-0.000210911268586855,-0.170941010809497));
#74075=CARTESIAN_POINT('',(-0.237175,-2.3095687792789E-14,-2.1406589891905));
#74076=CARTESIAN_POINT('Ctrl Pts',(-0.236800424386245,5.02917441071067E-5,
-0.1906589891905));
#74077=CARTESIAN_POINT('Ctrl Pts',(-0.236719274693082,-0.0425515102735373,
-0.187810775860172));
#74078=CARTESIAN_POINT('Ctrl Pts',(-0.205414127958568,-0.164221921599079,
-0.179683736188175));
#74079=CARTESIAN_POINT('Ctrl Pts',(-0.0108890694688725,-0.279877751287428,
-0.166277870174509));
#74080=CARTESIAN_POINT('Ctrl Pts',(0.228827285837098,-0.161518206415849,
-0.150441391149505));
#74081=CARTESIAN_POINT('Ctrl Pts',(0.260066881677195,0.103990587976603,
-0.134604912124501));
#74082=CARTESIAN_POINT('Ctrl Pts',(0.054377113149757,0.274763121238199,
-0.118768433099496));
#74083=CARTESIAN_POINT('Ctrl Pts',(-0.181718869422876,0.201170273454141,
-0.104119792121496));
#74084=CARTESIAN_POINT('Ctrl Pts',(-0.236633512176461,0.0607240528485506,
-0.0947499774851641));
#74085=CARTESIAN_POINT('Ctrl Pts',(-0.237190235300011,-0.000209952227111019,
-0.0906589891905003));
#74086=CARTESIAN_POINT('Ctrl Pts',(-0.237215670057668,-0.00021091126858686,
-0.170941010809497));
#74087=CARTESIAN_POINT('Ctrl Pts',(-0.237370804814323,-0.0171505583576599,
-0.169803444281345));
#74088=CARTESIAN_POINT('Ctrl Pts',(-0.228001304010126,-0.112527743254352,
-0.163387051411524));
#74089=CARTESIAN_POINT('Ctrl Pts',(-0.0990213293987983,-0.262004605402092,
-0.151691832200035));
#74090=CARTESIAN_POINT('Ctrl Pts',(0.165855812771546,-0.225703615695282,
-0.13585535317503));
#74091=CARTESIAN_POINT('Ctrl Pts',(0.279606860807486,0.0162117244434021,
-0.120018874150026));
#74092=CARTESIAN_POINT('Ctrl Pts',(0.138664230983235,0.2433835073103,-0.104182395125021));
#74093=CARTESIAN_POINT('Ctrl Pts',(-0.128691327754114,0.248769867313068,
-0.0883459161000173));
#74094=CARTESIAN_POINT('Ctrl Pts',(-0.233610483961208,0.0940282986476538,
-0.0772654546615087));
#74095=CARTESIAN_POINT('Ctrl Pts',(-0.237500893647975,0.00790614332200466,
-0.0714638195646687));
#74096=CARTESIAN_POINT('Ctrl Pts',(-0.237452100135973,0.000140355381394047,
-0.0709410108094966));
#74097=CARTESIAN_POINT('Origin',(0.,0.,-2.1406589891905));
#74098=CARTESIAN_POINT('',(-0.237375536783514,0.000176208511683888,-0.2906589891905));
#74099=CARTESIAN_POINT('',(-0.236796239026498,3.83100794477953E-5,-0.270941010809497));
#74100=CARTESIAN_POINT('',(-0.237175,-2.3095687792789E-14,-2.1406589891905));
#74101=CARTESIAN_POINT('Ctrl Pts',(-0.237375536783514,0.000176208511683873,
-0.2906589891905));
#74102=CARTESIAN_POINT('Ctrl Pts',(-0.236818330331351,-0.0668453655976375,
-0.286150400576847));
#74103=CARTESIAN_POINT('Ctrl Pts',(-0.172206359973546,-0.213278616180841,
-0.276362985621525));
#74104=CARTESIAN_POINT('Ctrl Pts',(0.0758114385164903,-0.269634087135906,
-0.261296744324535));
#74105=CARTESIAN_POINT('Ctrl Pts',(0.267440510425046,-0.0832195429967548,
-0.245460265299531));
#74106=CARTESIAN_POINT('Ctrl Pts',(0.215416916394134,0.17901240420799,-0.229623786274526));
#74107=CARTESIAN_POINT('Ctrl Pts',(-0.0328628956583448,0.278154575422294,
-0.213787307249523));
#74108=CARTESIAN_POINT('Ctrl Pts',(-0.211934276390539,0.151628854238979,
-0.200799041554847));
#74109=CARTESIAN_POINT('Ctrl Pts',(-0.236869676045862,0.0364058881413166,
-0.19308960220184));
#74110=CARTESIAN_POINT('Ctrl Pts',(-0.236800424386245,5.02917441071067E-5,
-0.1906589891905));
#74111=CARTESIAN_POINT('Ctrl Pts',(-0.236796239026498,3.83100794478057E-5,
-0.270941010809497));
#74112=CARTESIAN_POINT('Ctrl Pts',(-0.236735559172027,-0.0418134366052485,
-0.26814306899802));
#74113=CARTESIAN_POINT('Ctrl Pts',(-0.206235814196846,-0.16270876290859,
-0.260066300844874));
#74114=CARTESIAN_POINT('Ctrl Pts',(-0.0135402899116431,-0.27976166618424,
-0.246710706350061));
#74115=CARTESIAN_POINT('Ctrl Pts',(0.227285795344374,-0.163679885626449,
-0.230874227325056));
#74116=CARTESIAN_POINT('Ctrl Pts',(0.261041901008646,0.101522741173457,
-0.215037748300052));
#74117=CARTESIAN_POINT('Ctrl Pts',(0.056975763960648,0.274233261483808,
-0.199201269275047));
#74118=CARTESIAN_POINT('Ctrl Pts',(-0.180612775457958,0.202642109780299,
-0.184502356778196));
#74119=CARTESIAN_POINT('Ctrl Pts',(-0.236650908949183,0.0614571125427528,
-0.175082270623013));
#74120=CARTESIAN_POINT('Ctrl Pts',(-0.237215670057668,-0.00021091126858686,
-0.170941010809497));
#74121=CARTESIAN_POINT('Origin',(0.,0.,-2.1406589891905));
#74122=CARTESIAN_POINT('',(-0.23732555028123,-0.000191980036303487,-0.390658989190501));
#74123=CARTESIAN_POINT('',(-0.237354923007457,0.000183314680767349,-0.370941010809497));
#74124=CARTESIAN_POINT('',(-0.237175,-2.3095687792789E-14,-2.1406589891905));
#74125=CARTESIAN_POINT('Ctrl Pts',(-0.23732555028123,-0.000191980036303481,
-0.3906589891905));
#74126=CARTESIAN_POINT('Ctrl Pts',(-0.237441870296821,-0.0134313959082863,
-0.38976885163519));
#74127=CARTESIAN_POINT('Ctrl Pts',(-0.230421693992145,-0.105061794884267,
-0.383599887738212));
#74128=CARTESIAN_POINT('Ctrl Pts',(-0.111125482197992,-0.25710122431668,
-0.372152097499565));
#74129=CARTESIAN_POINT('Ctrl Pts',(0.155146048077143,-0.23319437425588,
-0.356315618474562));
#74130=CARTESIAN_POINT('Ctrl Pts',(0.280071232427623,0.00316502186262762,
-0.340479139449557));
#74131=CARTESIAN_POINT('Ctrl Pts',(0.149836545421379,0.236640912759002,
-0.324642660424553));
#74132=CARTESIAN_POINT('Ctrl Pts',(-0.116907244968831,0.254524279263399,
-0.308806181399548));
#74133=CARTESIAN_POINT('Ctrl Pts',(-0.231523947454547,0.101447974052937,
-0.297478290988198));
#74134=CARTESIAN_POINT('Ctrl Pts',(-0.237470728753447,0.0116260322577658,
-0.291429226918515));
#74135=CARTESIAN_POINT('Ctrl Pts',(-0.237375536783514,0.000176208511683873,
-0.2906589891905));
#74136=CARTESIAN_POINT('Ctrl Pts',(-0.237354923007457,0.000183314680767349,
-0.370941010809497));
#74137=CARTESIAN_POINT('Ctrl Pts',(-0.236789072171188,-0.0661059259336786,
-0.366482693714695));
#74138=CARTESIAN_POINT('Ctrl Pts',(-0.173393869560153,-0.211833111027387,
-0.356745550278225));
#74139=CARTESIAN_POINT('Ctrl Pts',(0.0732530352383368,-0.270340335534277,
-0.341729580500087));
#74140=CARTESIAN_POINT('Ctrl Pts',(0.266639901610645,-0.0857500318774511,
-0.325893101475082));
#74141=CARTESIAN_POINT('Ctrl Pts',(0.217103548889173,0.176963130656145,
-0.310056622450078));
#74142=CARTESIAN_POINT('Ctrl Pts',(-0.0302257286171684,0.27845342881406,
-0.294220143425073));
#74143=CARTESIAN_POINT('Ctrl Pts',(-0.211185581776565,0.153147220674766,
-0.281181606211547));
#74144=CARTESIAN_POINT('Ctrl Pts',(-0.236850042758812,0.0371474988715844,
-0.273421895339688));
#74145=CARTESIAN_POINT('Ctrl Pts',(-0.236796239026498,3.83100794478057E-5,
-0.270941010809497));
#74146=CARTESIAN_POINT('Origin',(0.,0.,-2.1406589891905));
#74147=CARTESIAN_POINT('',(-0.236792325324681,-2.1558736610646E-5,-0.490658989190501));
#74148=CARTESIAN_POINT('',(-0.237346845555136,-0.000185862303693607,-0.470941010809497));
#74149=CARTESIAN_POINT('',(-0.237175,-2.3095687792789E-14,-2.1406589891905));
#74150=CARTESIAN_POINT('Ctrl Pts',(-0.236792325324681,-2.15587366106523E-5,
-0.4906589891905));
#74151=CARTESIAN_POINT('Ctrl Pts',(-0.236823424346363,-0.0381738378163725,
-0.488108476351866));
#74152=CARTESIAN_POINT('Ctrl Pts',(-0.210132507448376,-0.15524928073634,
-0.480279137171563));
#74153=CARTESIAN_POINT('Ctrl Pts',(-0.0265686443687933,-0.278826145720265,
-0.467170971649592));
#74154=CARTESIAN_POINT('Ctrl Pts',(0.219407375961836,-0.174098580622825,
-0.451334492624588));
#74155=CARTESIAN_POINT('Ctrl Pts',(0.265491543531784,0.0892421017223949,
-0.435498013599583));
#74156=CARTESIAN_POINT('Ctrl Pts',(0.0696987171985843,0.271278456967154,
-0.419661534574579));
#74157=CARTESIAN_POINT('Ctrl Pts',(-0.175019066077197,0.209825495554917,
-0.404715193104885));
#74158=CARTESIAN_POINT('Ctrl Pts',(-0.236752052011204,0.065082960481243,
-0.395047677976859));
#74159=CARTESIAN_POINT('Ctrl Pts',(-0.23732555028123,-0.000191980036303481,
-0.3906589891905));
#74160=CARTESIAN_POINT('Ctrl Pts',(-0.237346845555136,-0.000185862303693581,
-0.470941010809497));
#74161=CARTESIAN_POINT('Ctrl Pts',(-0.237454401889236,-0.0126746567440396,
-0.470101144773039));
#74162=CARTESIAN_POINT('Ctrl Pts',(-0.230889358616771,-0.103546234772025,
-0.463982452394912));
#74163=CARTESIAN_POINT('Ctrl Pts',(-0.113556730952469,-0.256036662952951,
-0.452584933675117));
#74164=CARTESIAN_POINT('Ctrl Pts',(0.15292936740834,-0.23465402726664,-0.436748454650113));
#74165=CARTESIAN_POINT('Ctrl Pts',(0.280088633943004,0.000510975941890648,
-0.420911975625108));
#74166=CARTESIAN_POINT('Ctrl Pts',(0.152072176426899,0.235210452621709,
-0.405075496600104));
#74167=CARTESIAN_POINT('Ctrl Pts',(-0.114490165816999,0.255620628817145,
-0.389239017575099));
#74168=CARTESIAN_POINT('Ctrl Pts',(-0.231067303341457,0.102962813414217,
-0.377860855644897));
#74169=CARTESIAN_POINT('Ctrl Pts',(-0.237459062267548,0.0123831949798373,
-0.371761520056363));
#74170=CARTESIAN_POINT('Ctrl Pts',(-0.237354923007457,0.000183314680767349,
-0.370941010809497));
#74171=CARTESIAN_POINT('Origin',(0.,0.,-2.1406589891905));
#74172=CARTESIAN_POINT('',(-0.237247451135996,0.000207679341461782,-0.590658989190501));
#74173=CARTESIAN_POINT('',(-0.236794931055306,-3.36693625221374E-5,-0.570941010809498));
#74174=CARTESIAN_POINT('',(-0.237175,-2.3095687792789E-14,-2.1406589891905));
#74175=CARTESIAN_POINT('Ctrl Pts',(-0.237247451135996,0.000207679341461783,
-0.590658989190501));
#74176=CARTESIAN_POINT('Ctrl Pts',(-0.236675038023536,-0.0624760192039184,
-0.586448101068542));
#74177=CARTESIAN_POINT('Ctrl Pts',(-0.179066675139839,-0.204671240602264,
-0.576958386604914));
#74178=CARTESIAN_POINT('Ctrl Pts',(0.0605694802894751,-0.273461606920063,
-0.562189845799617));
#74179=CARTESIAN_POINT('Ctrl Pts',(0.262352096699239,-0.0980881733918026,
-0.546353366774615));
#74180=CARTESIAN_POINT('Ctrl Pts',(0.225117923184134,0.166648831568735,
-0.530516887749609));
#74181=CARTESIAN_POINT('Ctrl Pts',(-0.0172107170083428,0.279559839071688,
-0.514680408724605));
#74182=CARTESIAN_POINT('Ctrl Pts',(-0.20735700595603,0.160611456954188,
-0.501394442538236));
#74183=CARTESIAN_POINT('Ctrl Pts',(-0.236759058336372,0.0407903817516132,
-0.493387302693534));
#74184=CARTESIAN_POINT('Ctrl Pts',(-0.236792325324681,-2.15587366106523E-5,
-0.4906589891905));
#74185=CARTESIAN_POINT('Ctrl Pts',(-0.236794931055306,-3.366936252212E-5,
-0.570941010809498));
#74186=CARTESIAN_POINT('Ctrl Pts',(-0.236842572399773,-0.0374329187291053,
-0.568440769489714));
#74187=CARTESIAN_POINT('Ctrl Pts',(-0.210894706723823,-0.153731708204917,
-0.560661701828262));
#74188=CARTESIAN_POINT('Ctrl Pts',(-0.0292095552737704,-0.278561852753679,
-0.547603807825144));
#74189=CARTESIAN_POINT('Ctrl Pts',(0.217747787412377,-0.176169818657624,
-0.531767328800138));
#74190=CARTESIAN_POINT('Ctrl Pts',(0.26632525124544,0.0867223412897275,
-0.515930849775135));
#74191=CARTESIAN_POINT('Ctrl Pts',(0.0722661688848724,0.270605810659411,
-0.50009437075013));
#74192=CARTESIAN_POINT('Ctrl Pts',(-0.173847952832261,0.211275626043213,
-0.485097757761584));
#74193=CARTESIAN_POINT('Ctrl Pts',(-0.236778375969605,0.0658214059677648,
-0.475379971114707));
#74194=CARTESIAN_POINT('Ctrl Pts',(-0.237346845555136,-0.000185862303693581,
-0.470941010809497));
#74195=CARTESIAN_POINT('Origin',(0.,0.,-2.1406589891905));
#74196=CARTESIAN_POINT('',(-0.237442878479053,-0.000145678815165409,-0.690658989190501));
#74197=CARTESIAN_POINT('',(-0.23722491884502,0.000210405188862381,-0.670941010809497));
#74198=CARTESIAN_POINT('',(-0.237175,-2.3095687792789E-14,-2.1406589891905));
#74199=CARTESIAN_POINT('Ctrl Pts',(-0.237442878479053,-0.000145678815165355,
-0.690658989190501));
#74200=CARTESIAN_POINT('Ctrl Pts',(-0.237506536812315,-0.00894590921801271,
-0.690066552126885));
#74201=CARTESIAN_POINT('Ctrl Pts',(-0.233075801309679,-0.0960946100168791,
-0.6841952887216));
#74202=CARTESIAN_POINT('Ctrl Pts',(-0.125370287089174,-0.250463976485706,
-0.673045198974649));
#74203=CARTESIAN_POINT('Ctrl Pts',(0.141822954079178,-0.241528801798274,
-0.657208719949644));
#74204=CARTESIAN_POINT('Ctrl Pts',(0.279807899799573,-0.0125479724101313,
-0.64137224092464));
#74205=CARTESIAN_POINT('Ctrl Pts',(0.162872885484516,0.227864730872955,
-0.625535761899635));
#74206=CARTESIAN_POINT('Ctrl Pts',(-0.102448037478282,0.260680478783321,
-0.609699282874631));
#74207=CARTESIAN_POINT('Ctrl Pts',(-0.228702776867451,0.110425870116913,
-0.598073691971586));
#74208=CARTESIAN_POINT('Ctrl Pts',(-0.237392622848602,0.016105113680835,
-0.59172692741021));
#74209=CARTESIAN_POINT('Ctrl Pts',(-0.237247451135996,0.000207679341461783,
-0.590658989190501));
#74210=CARTESIAN_POINT('Ctrl Pts',(-0.23722491884502,0.000210405188862376,
-0.670941010809497));
#74211=CARTESIAN_POINT('Ctrl Pts',(-0.23665762571089,-0.0617400645604461,
-0.666780394206389));
#74212=CARTESIAN_POINT('Ctrl Pts',(-0.180184596641873,-0.203207116348255,
-0.657340951261613));
#74213=CARTESIAN_POINT('Ctrl Pts',(0.057975485860299,-0.274023259903682,
-0.64262268197517));
#74214=CARTESIAN_POINT('Ctrl Pts',(0.261410838370488,-0.100569764399713,
-0.626786202950165));
#74215=CARTESIAN_POINT('Ctrl Pts',(0.22668693762885,0.16450816465285,-0.610949723925161));
#74216=CARTESIAN_POINT('Ctrl Pts',(-0.0145608858552237,0.279710358285275,
-0.595113244900156));
#74217=CARTESIAN_POINT('Ctrl Pts',(-0.206549469757811,0.162125874414636,
-0.581777007194936));
#74218=CARTESIAN_POINT('Ctrl Pts',(-0.236741985955522,0.0415291163163889,
-0.573719595831383));
#74219=CARTESIAN_POINT('Ctrl Pts',(-0.236794931055306,-3.366936252212E-5,
-0.570941010809498));
#74220=CARTESIAN_POINT('Origin',(0.,0.,-2.1406589891905));
#74221=CARTESIAN_POINT('',(-0.236824320187109,-9.1009876261151E-5,-0.790658989190501));
#74222=CARTESIAN_POINT('',(-0.237459971379865,-0.000135626906777819,-0.770941010809498));
#74223=CARTESIAN_POINT('',(-0.237175,-2.3095687792789E-14,-2.1406589891905));
#74224=CARTESIAN_POINT('Ctrl Pts',(-0.236824320187109,-9.10098762611847E-5,
-0.790658989190501));
#74225=CARTESIAN_POINT('Ctrl Pts',(-0.236941182127794,-0.0337787096963821,
-0.788406176843561));
#74226=CARTESIAN_POINT('Ctrl Pts',(-0.214504063690713,-0.146255429941878,
-0.780874538154952));
#74227=CARTESIAN_POINT('Ctrl Pts',(-0.0421650045577871,-0.276897137566454,
-0.768064073124674));
#74228=CARTESIAN_POINT('Ctrl Pts',(0.209297564880806,-0.186130174170711,
-0.752227594099669));
#74229=CARTESIAN_POINT('Ctrl Pts',(0.270078860083927,0.0742113315984893,
-0.736391115074667));
#74230=CARTESIAN_POINT('Ctrl Pts',(0.0848038707134778,0.266942345673866,
-0.720554636049661));
#74231=CARTESIAN_POINT('Ctrl Pts',(-0.167910606883227,0.218362587719398,
-0.705310594088274));
#74232=CARTESIAN_POINT('Ctrl Pts',(-0.236939318271937,0.0694672943377367,
-0.695345378468553));
#74233=CARTESIAN_POINT('Ctrl Pts',(-0.237442878479053,-0.000145678815165355,
-0.690658989190501));
#74234=CARTESIAN_POINT('Ctrl Pts',(-0.237459971379865,-0.000135626906777798,
-0.770941010809498));
#74235=CARTESIAN_POINT('Ctrl Pts',(-0.237515064016247,-0.0081875839623386,
-0.770398845264733));
#74236=CARTESIAN_POINT('Ctrl Pts',(-0.233496912921487,-0.0945822701972211,
-0.764577853378301));
#74237=CARTESIAN_POINT('Ctrl Pts',(-0.127738002114452,-0.249264732252255,
-0.753478035150199));
#74238=CARTESIAN_POINT('Ctrl Pts',(0.139527896638572,-0.242861833124507,
-0.737641556125195));
#74239=CARTESIAN_POINT('Ctrl Pts',(0.279676420005076,-0.015198816471186,
-0.721805077100191));
#74240=CARTESIAN_POINT('Ctrl Pts',(0.165024768460067,0.226311134776178,
-0.705968598075186));
#74241=CARTESIAN_POINT('Ctrl Pts',(-0.0999732721998829,0.261639539776823,
-0.690132119050183));
#74242=CARTESIAN_POINT('Ctrl Pts',(-0.228198205810638,0.111943521562034,
-0.678456256628286));
#74243=CARTESIAN_POINT('Ctrl Pts',(-0.237377384877754,0.0168602494764385,
-0.672059220548058));
#74244=CARTESIAN_POINT('Ctrl Pts',(-0.23722491884502,0.000210405188862376,
-0.670941010809497));
#74245=CARTESIAN_POINT('Origin',(0.,0.,-2.1406589891905));
#74246=CARTESIAN_POINT('',(-0.237114751271997,0.000212755034102921,-0.890658989190501));
#74247=CARTESIAN_POINT('',(-0.236833526846729,-0.000101945576229834,-0.870941010809498));
#74248=CARTESIAN_POINT('',(-0.237175,-2.3095687792789E-14,-2.1406589891905));
#74249=CARTESIAN_POINT('Ctrl Pts',(-0.237114751271997,0.000212755034102929,
-0.890658989190501));
#74250=CARTESIAN_POINT('Ctrl Pts',(-0.236598028529304,-0.0581228578554325,
-0.886745801560236));
#74251=CARTESIAN_POINT('Ctrl Pts',(-0.185518811696717,-0.195961385216037,
-0.877553787588303));
#74252=CARTESIAN_POINT('Ctrl Pts',(0.0451368350116836,-0.276428252041976,
-0.8630829472747));
#74253=CARTESIAN_POINT('Ctrl Pts',(0.256437791245425,-0.112647998752851,
-0.847246468249696));
#74254=CARTESIAN_POINT('Ctrl Pts',(0.23411020610242,0.153760605489627,-0.831409989224693));
#74255=CARTESIAN_POINT('Ctrl Pts',(-0.00150429633730956,0.280085075458125,
-0.815573510199687));
#74256=CARTESIAN_POINT('Ctrl Pts',(-0.20242601141066,0.169566288850719,
-0.801989843521624));
#74257=CARTESIAN_POINT('Ctrl Pts',(-0.236667349337564,0.0451588535863105,
-0.793685003185228));
#74258=CARTESIAN_POINT('Ctrl Pts',(-0.236824320187109,-9.10098762611847E-5,
-0.790658989190501));
#74259=CARTESIAN_POINT('Ctrl Pts',(-0.236833526846729,-0.000101945576229823,
-0.870941010809498));
#74260=CARTESIAN_POINT('Ctrl Pts',(-0.236961801699857,-0.0330346947601913,
-0.868738469981408));
#74261=CARTESIAN_POINT('Ctrl Pts',(-0.21520889725179,-0.144735311414088,
-0.861257102811651));
#74262=CARTESIAN_POINT('Ctrl Pts',(-0.0447869354702739,-0.276485143073116,
-0.848496909300226));
#74263=CARTESIAN_POINT('Ctrl Pts',(0.20752442160637,-0.188105072674614,
-0.832660430275222));
#74264=CARTESIAN_POINT('Ctrl Pts',(0.270769932793133,0.0716487782462665,
-0.816823951250217));
#74265=CARTESIAN_POINT('Ctrl Pts',(0.0873295552116665,0.266126760615149,
-0.800987472225213));
#74266=CARTESIAN_POINT('Ctrl Pts',(-0.166668773296624,0.219791561064743,
-0.785693158744973));
#74267=CARTESIAN_POINT('Ctrl Pts',(-0.236978651359679,0.0702107639543191,
-0.775677671606401));
#74268=CARTESIAN_POINT('Ctrl Pts',(-0.237459971379865,-0.000135626906777798,
-0.770941010809498));
#74269=CARTESIAN_POINT('Origin',(0.,0.,-2.1406589891905));
#74270=CARTESIAN_POINT('',(-0.23752749294738,-7.85812877829553E-5,-0.990658989190501));
#74271=CARTESIAN_POINT('',(-0.237092966851317,0.000211018442878422,-0.970941010809499));
#74272=CARTESIAN_POINT('',(-0.237175,-2.3095687792789E-14,-2.1406589891905));
#74273=CARTESIAN_POINT('Ctrl Pts',(-0.23752749294738,-7.85812877829419E-5,
-0.990658989190501));
#74274=CARTESIAN_POINT('Ctrl Pts',(-0.237546434480431,-0.00445256118670738,
-0.990364252618579));
#74275=CARTESIAN_POINT('Ctrl Pts',(-0.235458487126414,-0.0871474789275883,
-0.984790689704989));
#74276=CARTESIAN_POINT('Ctrl Pts',(-0.139220414716906,-0.24303824499018,
-0.973938300449731));
#74277=CARTESIAN_POINT('Ctrl Pts',(0.128053388226197,-0.249102874663553,
-0.958101821424727));
#74278=CARTESIAN_POINT('Ctrl Pts',(0.278663706570009,-0.0282214642164085,
-0.942265342399722));
#74279=CARTESIAN_POINT('Ctrl Pts',(0.175396486098643,0.218371209334249,
-0.926428863374717));
#74280=CARTESIAN_POINT('Ctrl Pts',(-0.0876663129058996,0.26601603332006,
-0.910592384349715));
#74281=CARTESIAN_POINT('Ctrl Pts',(-0.225593223953284,0.119418790281913,
-0.898669092954974));
#74282=CARTESIAN_POINT('Ctrl Pts',(-0.237295079088385,0.020570933261798,
-0.892024627901903));
#74283=CARTESIAN_POINT('Ctrl Pts',(-0.237114751271997,0.000212755034102929,
-0.890658989190501));
#74284=CARTESIAN_POINT('Ctrl Pts',(-0.237092966851317,0.000211018442878404,
-0.970941010809499));
#74285=CARTESIAN_POINT('Ctrl Pts',(-0.236590878687514,-0.0573886351489161,
-0.967078094698084));
#74286=CARTESIAN_POINT('Ctrl Pts',(-0.186568756555997,-0.19448175581739,
-0.957936352245));
#74287=CARTESIAN_POINT('Ctrl Pts',(0.0425154229059733,-0.276843534770285,
-0.943515783450253));
#74288=CARTESIAN_POINT('Ctrl Pts',(0.255358832545678,-0.115072892419929,
-0.927679304425247));
#74289=CARTESIAN_POINT('Ctrl Pts',(0.2355566898837,0.151535308690796,-0.911842825400244));
#74290=CARTESIAN_POINT('Ctrl Pts',(0.00114980584647748,0.280086739913719,
-0.896006346375237));
#74291=CARTESIAN_POINT('Ctrl Pts',(-0.201557562819165,0.171074866061252,
-0.882372408178324));
#74292=CARTESIAN_POINT('Ctrl Pts',(-0.236654365549286,0.045895176449807,
-0.874017296323077));
#74293=CARTESIAN_POINT('Ctrl Pts',(-0.236833526846729,-0.000101945576229823,
-0.870941010809498));
#74294=CARTESIAN_POINT('Origin',(0.,0.,-2.1406589891905));
#74295=CARTESIAN_POINT('',(-0.236893725685054,-0.000150389252750359,-1.0906589891905));
#74296=CARTESIAN_POINT('',(-0.237537155315066,-6.57425195367267E-5,-1.0709410108095));
#74297=CARTESIAN_POINT('',(-0.237175,-2.3095687792789E-14,-2.1406589891905));
#74298=CARTESIAN_POINT('Ctrl Pts',(-0.236893725685054,-0.000150389252750339,
-1.0906589891905));
#74299=CARTESIAN_POINT('Ctrl Pts',(-0.237064310361161,-0.0293649258802016,
-1.08870387733525));
#74300=CARTESIAN_POINT('Ctrl Pts',(-0.218540890155226,-0.137250396400922,
-1.08146993913834));
#74301=CARTESIAN_POINT('Ctrl Pts',(-0.0576286254410279,-0.2740964318112,
-1.06895717459976));
#74302=CARTESIAN_POINT('Ctrl Pts',(0.198528865854686,-0.197575812852451,
-1.05312069557475));
#74303=CARTESIAN_POINT('Ctrl Pts',(0.273815943606632,0.0589469373985079,
-1.03728421654975));
#74304=CARTESIAN_POINT('Ctrl Pts',(0.0996420538473957,0.261765875367525,
-1.02144773752474));
#74305=CARTESIAN_POINT('Ctrl Pts',(-0.160379968251884,0.226765849567329,
-1.00590599507166));
#74306=CARTESIAN_POINT('Ctrl Pts',(-0.237207185560743,0.0738868188155779,
-0.995643078960248));
#74307=CARTESIAN_POINT('Ctrl Pts',(-0.23752749294738,-7.85812877829419E-5,
-0.990658989190501));
#74308=CARTESIAN_POINT('Ctrl Pts',(-0.237537155315066,-6.57425195367272E-5,
-1.0709410108095));
#74309=CARTESIAN_POINT('Ctrl Pts',(-0.23755056754939,-0.00369328339404799,
-1.07069654575643));
#74310=CARTESIAN_POINT('Ctrl Pts',(-0.235834755836577,-0.0856387249952216,
-1.06517325436169));
#74311=CARTESIAN_POINT('Ctrl Pts',(-0.141517142307931,-0.241708093290185,
-1.05437113662528));
#74312=CARTESIAN_POINT('Ctrl Pts',(0.125687179216381,-0.250305087662256,
-1.03853465760028));
#74313=CARTESIAN_POINT('Ctrl Pts',(0.278383759087368,-0.0308607615811162,
-1.02269817857527));
#74314=CARTESIAN_POINT('Ctrl Pts',(0.177457847270645,0.216699368644785,
-1.00686169955027));
#74315=CARTESIAN_POINT('Ctrl Pts',(-0.0851416533425872,0.26683478557915,
-0.991025220525264));
#74316=CARTESIAN_POINT('Ctrl Pts',(-0.225038857388908,0.120938550544616,
-0.979051657611676));
#74317=CARTESIAN_POINT('Ctrl Pts',(-0.23727700185159,0.0213235501229567,
-0.972356921039753));
#74318=CARTESIAN_POINT('Ctrl Pts',(-0.237092966851317,0.000211018442878404,
-0.970941010809499));
#74319=CARTESIAN_POINT('Origin',(0.,0.,-2.1406589891905));
#74320=CARTESIAN_POINT('',(-0.236992223716617,0.000192184054864515,-1.1906589891905));
#74321=CARTESIAN_POINT('',(-0.236908741130895,-0.000158913860137805,-1.1709410108095));
#74322=CARTESIAN_POINT('',(-0.237175,-2.3095687792789E-14,-2.1406589891905));
#74323=CARTESIAN_POINT('Ctrl Pts',(-0.236992223716617,0.000192184054864528,
-1.1906589891905));
#74324=CARTESIAN_POINT('Ctrl Pts',(-0.236577798658883,-0.0537762028892547,
-1.18704350205193));
#74325=CARTESIAN_POINT('Ctrl Pts',(-0.191572606767969,-0.18716689616996,
-1.17814918857169));
#74326=CARTESIAN_POINT('Ctrl Pts',(0.0295620948351317,-0.278524675658752,
-1.16397604874978));
#74327=CARTESIAN_POINT('Ctrl Pts',(0.249716196091533,-0.126853197876244,
-1.14813956972478));
#74328=CARTESIAN_POINT('Ctrl Pts',(0.242365488607872,0.140388326914034,
-1.13230309069977));
#74329=CARTESIAN_POINT('Ctrl Pts',(0.0142068599963639,0.27972857832352,
-1.11646661167477));
#74330=CARTESIAN_POINT('Ctrl Pts',(-0.197129456028173,0.178481248161311,
-1.10258524450501));
#74331=CARTESIAN_POINT('Ctrl Pts',(-0.236603729612646,0.0495146866057853,
-1.09398270367692));
#74332=CARTESIAN_POINT('Ctrl Pts',(-0.236893725685054,-0.000150389252750339,
-1.0906589891905));
#74333=CARTESIAN_POINT('Ctrl Pts',(-0.236908741130895,-0.000158913860137808,
-1.1709410108095));
#74334=CARTESIAN_POINT('Ctrl Pts',(-0.237085066804682,-0.0286177232752274,
-1.1690361704731));
#74335=CARTESIAN_POINT('Ctrl Pts',(-0.219190380754614,-0.135729270178569,
-1.16185250379504));
#74336=CARTESIAN_POINT('Ctrl Pts',(-0.0602233222835258,-0.273538032789071,
-1.14939001077531));
#74337=CARTESIAN_POINT('Ctrl Pts',(0.196647749876134,-0.199448154660888,
-1.1335535317503));
#74338=CARTESIAN_POINT('Ctrl Pts',(0.274362205745136,0.0563496582744192,
-1.1177170527253));
#74339=CARTESIAN_POINT('Ctrl Pts',(0.102118020082256,0.260809919104815,
-1.1018805737003));
#74340=CARTESIAN_POINT('Ctrl Pts',(-0.159066073200517,0.228170150730898,
-1.08628855972836));
#74341=CARTESIAN_POINT('Ctrl Pts',(-0.237260952101461,0.0746375785566909,
-1.0759753720981));
#74342=CARTESIAN_POINT('Ctrl Pts',(-0.237537155315066,-6.57425195367272E-5,
-1.0709410108095));
#74343=CARTESIAN_POINT('Origin',(0.,0.,-2.1406589891905));
#74344=CARTESIAN_POINT('',(-0.237559752509291,8.12847334188233E-7,-1.2906589891905));
#74345=CARTESIAN_POINT('',(-0.23697343290048,0.000186386972896829,-1.2709410108095));
#74346=CARTESIAN_POINT('',(-0.237175,-2.3095687792789E-14,-2.1406589891905));
#74347=CARTESIAN_POINT('Ctrl Pts',(-0.237559751139412,8.1284444012185E-7,
-1.2906589891905));
#74348=CARTESIAN_POINT('Ctrl Pts',(-0.237555752466613,-0.0782661021016744,
-1.2853831267686));
#74349=CARTESIAN_POINT('Ctrl Pts',(-0.152582383736732,-0.234851345594784,
-1.27482843800504));
#74350=CARTESIAN_POINT('Ctrl Pts',(0.11388069855569,-0.255892748819348,
-1.25899492289981));
#74351=CARTESIAN_POINT('Ctrl Pts',(0.27664225441934,-0.0438061122634664,
-1.2431584438748));
#74352=CARTESIAN_POINT('Ctrl Pts',(0.187367922478493,0.208190235188752,
-1.2273219648498));
#74353=CARTESIAN_POINT('Ctrl Pts',(-0.0726086067354031,0.270514144971751,
-1.2114854858248));
#74354=CARTESIAN_POINT('Ctrl Pts',(-0.222184057315321,0.128422060611755,
-1.19926449393836));
#74355=CARTESIAN_POINT('Ctrl Pts',(-0.237182883901222,0.0250208531363774,
-1.1923223283936));
#74356=CARTESIAN_POINT('Ctrl Pts',(-0.236992223716617,0.000192184054864528,
-1.1906589891905));
#74357=CARTESIAN_POINT('Ctrl Pts',(-0.23697343290048,0.000186386972896805,
-1.2709410108095));
#74358=CARTESIAN_POINT('Ctrl Pts',(-0.236579283171597,-0.0530422438593269,
-1.26737579518978));
#74359=CARTESIAN_POINT('Ctrl Pts',(-0.192556305014578,-0.185674636157468,
-1.25853175322839));
#74360=CARTESIAN_POINT('Ctrl Pts',(0.0269215174987288,-0.278792280783643,
-1.24440888492533));
#74361=CARTESIAN_POINT('Ctrl Pts',(0.248502933681857,-0.129213760414636,
-1.22857240590033));
#74362=CARTESIAN_POINT('Ctrl Pts',(0.243684888061905,0.138085405670681,
-1.21273592687532));
#74363=CARTESIAN_POINT('Ctrl Pts',(0.0168568778538109,0.279581382781475,
-1.19689944785032));
#74364=CARTESIAN_POINT('Ctrl Pts',(-0.196198136324593,0.179981788309436,
-1.18296780916171));
#74365=CARTESIAN_POINT('Ctrl Pts',(-0.236596420804428,0.0502493134640227,
-1.17431499681477));
#74366=CARTESIAN_POINT('Ctrl Pts',(-0.236908741130895,-0.000158913860137808,
-1.1709410108095));
#74367=CARTESIAN_POINT('Origin',(0.,0.,-2.1406589891905));
#74368=CARTESIAN_POINT('',(-0.236994481351619,-0.000192825895592933,-1.3906589891905));
#74369=CARTESIAN_POINT('',(-0.237558599806732,1.45855281510868E-5,-1.3709410108095));
#74370=CARTESIAN_POINT('',(-0.237175,-2.3095687792789E-14,-2.1406589891905));
#74371=CARTESIAN_POINT('Ctrl Pts',(-0.236994481351619,-0.000192825895592965,
-1.3906589891905));
#74372=CARTESIAN_POINT('Ctrl Pts',(-0.237185225043465,-0.0249324145508677,
-1.38900157782695));
#74373=CARTESIAN_POINT('Ctrl Pts',(-0.222254938630742,-0.128242721718558,
-1.38206534012173));
#74374=CARTESIAN_POINT('Ctrl Pts',(-0.0729108261228343,-0.270432845334947,
-1.36985027607484));
#74375=CARTESIAN_POINT('Ctrl Pts',(0.187135179739969,-0.208399464743887,
-1.35401379704983));
#74376=CARTESIAN_POINT('Ctrl Pts',(0.276691029410919,0.0434969728300605,
-1.33817731802483));
#74377=CARTESIAN_POINT('Ctrl Pts',(0.114166554651702,0.255765342063417,
-1.32234083899983));
#74378=CARTESIAN_POINT('Ctrl Pts',(-0.152369756692705,0.235017807085461,
-1.30650435997482));
#74379=CARTESIAN_POINT('Ctrl Pts',(-0.237539870154193,0.0783996340976714,
-1.29594374337171));
#74380=CARTESIAN_POINT('Ctrl Pts',(-0.237559753385822,4.47823110714604E-5,
-1.29066195311027));
#74381=CARTESIAN_POINT('Ctrl Pts',(-0.237559751139412,8.1284444012185E-7,
-1.2906589891905));
#74382=CARTESIAN_POINT('Ctrl Pts',(-0.237558599806732,1.45855281510935E-5,
-1.3709410108095));
#74383=CARTESIAN_POINT('Ctrl Pts',(-0.237489298765113,-0.0775075558748563,
-1.36571541990645));
#74384=CARTESIAN_POINT('Ctrl Pts',(-0.153955582115517,-0.233469766690094,
-1.35521100266174));
#74385=CARTESIAN_POINT('Ctrl Pts',(0.11145078701977,-0.256960358813676,
-1.33942775907536));
#74386=CARTESIAN_POINT('Ctrl Pts',(0.276214720548922,-0.0464255541815164,
-1.32359128005036));
#74387=CARTESIAN_POINT('Ctrl Pts',(0.189332272492804,0.206405413014511,
-1.30775480102535));
#74388=CARTESIAN_POINT('Ctrl Pts',(-0.0700420007471637,0.271190010989185,
-1.29191832200035));
#74389=CARTESIAN_POINT('Ctrl Pts',(-0.221577961557814,0.129943018511057,
-1.27964705859506));
#74390=CARTESIAN_POINT('Ctrl Pts',(-0.23716287984381,0.025770576609058,
-1.27265462153145));
#74391=CARTESIAN_POINT('Ctrl Pts',(-0.23697343290048,0.000186386972896805,
-1.2709410108095));
#74392=CARTESIAN_POINT('Origin',(0.,0.,-2.1406589891905));
#74393=CARTESIAN_POINT('',(-0.236892012300018,0.000149351404289912,-1.4906589891905));
#74394=CARTESIAN_POINT('',(-0.237013962191253,-0.000197906546256954,-1.4709410108095));
#74395=CARTESIAN_POINT('',(-0.237175,-2.3095687792789E-14,-2.1406589891905));
#74396=CARTESIAN_POINT('Ctrl Pts',(-0.236892012300018,0.000149351404289903,
-1.4906589891905));
#74397=CARTESIAN_POINT('Ctrl Pts',(-0.236604661475949,-0.0494280473622855,
-1.48734120254363));
#74398=CARTESIAN_POINT('Ctrl Pts',(-0.197238562986412,-0.178304207004023,
-1.47874458955508));
#74399=CARTESIAN_POINT('Ctrl Pts',(0.0138942904708965,-0.279744278037816,
-1.46486915022487));
#74400=CARTESIAN_POINT('Ctrl Pts',(0.242208471436148,-0.140659051490779,
-1.44903267119986));
#74401=CARTESIAN_POINT('Ctrl Pts',(0.249857782313367,0.12657409300159,-1.43319619217486));
#74402=CARTESIAN_POINT('Ctrl Pts',(0.0298732918310454,0.278491469954,-1.41735971314985));
#74403=CARTESIAN_POINT('Ctrl Pts',(-0.191455883315294,0.187342730509716,
-1.4031806454884));
#74404=CARTESIAN_POINT('Ctrl Pts',(-0.23657770970529,0.0538627446639044,
-1.39428040416862));
#74405=CARTESIAN_POINT('Ctrl Pts',(-0.236994481351619,-0.000192825895592965,
-1.3906589891905));
#74406=CARTESIAN_POINT('Ctrl Pts',(-0.237013962191253,-0.000197906546256975,
-1.4709410108095));
#74407=CARTESIAN_POINT('Ctrl Pts',(-0.237204917491822,-0.0241821198511639,
-1.4693338709648));
#74408=CARTESIAN_POINT('Ctrl Pts',(-0.222851094449599,-0.126721896491833,
-1.46244790477843));
#74409=CARTESIAN_POINT('Ctrl Pts',(-0.0754701205516332,-0.269729799675546,
-1.45028311225039));
#74410=CARTESIAN_POINT('Ctrl Pts',(0.185152012983061,-0.210163355552944,
-1.43444663322539));
#74411=CARTESIAN_POINT('Ctrl Pts',(0.277090761295361,0.0408731444070958,
-1.41861015420038));
#74412=CARTESIAN_POINT('Ctrl Pts',(0.116585008054319,0.254672024034776,
-1.40277367517538));
#74413=CARTESIAN_POINT('Ctrl Pts',(-0.150135922153628,0.236451070642649,
-1.38693719615037));
#74414=CARTESIAN_POINT('Ctrl Pts',(-0.237198772362554,0.0799053226037852,
-1.37632630802841));
#74415=CARTESIAN_POINT('Ctrl Pts',(-0.23755930580753,0.000804338357484877,
-1.37099424624812));
#74416=CARTESIAN_POINT('Ctrl Pts',(-0.237558599806732,1.45855281510935E-5,
-1.3709410108095));
#74417=CARTESIAN_POINT('Origin',(0.,0.,-2.1406589891905));
#74418=CARTESIAN_POINT('',(-0.237526251942735,8.00723330132329E-5,-1.5906589891905));
#74419=CARTESIAN_POINT('',(-0.236877981323345,0.000140284900710816,-1.5709410108095));
#74420=CARTESIAN_POINT('',(-0.237175,-2.3095687792789E-14,-2.1406589891905));
#74421=CARTESIAN_POINT('Ctrl Pts',(-0.237526251942735,8.0072333013226E-5,
-1.5906589891905));
#74422=CARTESIAN_POINT('Ctrl Pts',(-0.237201011701744,-0.0737983853525183,
-1.5856808272603));
#74423=CARTESIAN_POINT('Ctrl Pts',(-0.160534088655561,-0.22659996424131,
-1.57542383898843));
#74424=CARTESIAN_POINT('Ctrl Pts',(0.0993495019835277,-0.261877049183029,
-1.55988802437489));
#74425=CARTESIAN_POINT('Ctrl Pts',(0.273749907070638,-0.059252854615386,
-1.54405154534989));
#74426=CARTESIAN_POINT('Ctrl Pts',(0.198749507440483,0.197353859059745,
-1.52821506632488));
#74427=CARTESIAN_POINT('Ctrl Pts',(-0.057322322005953,0.27416065327936,
-1.51237858729988));
#74428=CARTESIAN_POINT('Ctrl Pts',(-0.21846369760357,0.137429757328886,
-1.49985989492175));
#74429=CARTESIAN_POINT('Ctrl Pts',(-0.237061856365447,0.0294529978690901,
-1.49262002888529));
#74430=CARTESIAN_POINT('Ctrl Pts',(-0.236892012300018,0.000149351404289903,
-1.4906589891905));
#74431=CARTESIAN_POINT('Ctrl Pts',(-0.236877981323345,0.000140284900710819,
-1.5709410108095));
#74432=CARTESIAN_POINT('Ctrl Pts',(-0.236613139832454,-0.0486931615303172,
-1.56767349568147));
#74433=CARTESIAN_POINT('Ctrl Pts',(-0.198157845242651,-0.176801951054827,
-1.55912715421178));
#74434=CARTESIAN_POINT('Ctrl Pts',(0.011242860680614,-0.279863363121343,
-1.54530198640042));
#74435=CARTESIAN_POINT('Ctrl Pts',(0.240864724779504,-0.142947851629034,
-1.52946550737541));
#74436=CARTESIAN_POINT('Ctrl Pts',(0.251045943848778,0.124200797119059,
-1.51362902835041));
#74437=CARTESIAN_POINT('Ctrl Pts',(0.0325108828631745,0.278195877800473,
-1.4977925493254));
#74438=CARTESIAN_POINT('Ctrl Pts',(-0.190459795941901,0.188832794874465,
-1.4835632101451));
#74439=CARTESIAN_POINT('Ctrl Pts',(-0.236577703952162,0.0545966481543488,
-1.47461269730646));
#74440=CARTESIAN_POINT('Ctrl Pts',(-0.237013962191253,-0.000197906546256975,
-1.4709410108095));
#74441=CARTESIAN_POINT('Origin',(0.,0.,-2.1406589891905));
#74442=CARTESIAN_POINT('',(-0.237117339234101,-0.000212911088445047,-1.6906589891905));
#74443=CARTESIAN_POINT('',(-0.237514903826011,9.25041757272732E-5,-1.6709410108095));
#74444=CARTESIAN_POINT('',(-0.237175,-2.3095687792789E-14,-2.1406589891905));
#74445=CARTESIAN_POINT('Ctrl Pts',(-0.237117339234101,-0.000212911088445088,
-1.6906589891905));
#74446=CARTESIAN_POINT('Ctrl Pts',(-0.237297182177879,-0.0204821580555165,
-1.68929927831864));
#74447=CARTESIAN_POINT('Ctrl Pts',(-0.225658028636196,-0.119239611010002,
-1.68266074110512));
#74448=CARTESIAN_POINT('Ctrl Pts',(-0.087963495735764,-0.265917905478881,
-1.67074337754992));
#74449=CARTESIAN_POINT('Ctrl Pts',(0.175152374331677,-0.218567059118628,
-1.65490689852492));
#74450=CARTESIAN_POINT('Ctrl Pts',(0.27869506676358,0.0279100774344748,
-1.63907041949991));
#74451=CARTESIAN_POINT('Ctrl Pts',(0.128331648507507,0.248959635135041,
-1.62323394047491));
#74452=CARTESIAN_POINT('Ctrl Pts',(-0.138948763790046,0.243193654600889,
-1.6073974614499));
#74453=CARTESIAN_POINT('Ctrl Pts',(-0.235413626753898,0.0873254264909276,
-1.5965391443551));
#74454=CARTESIAN_POINT('Ctrl Pts',(-0.237545895370774,0.00454208528307148,
-1.59095965360197));
#74455=CARTESIAN_POINT('Ctrl Pts',(-0.237526251942735,8.0072333013226E-5,
-1.5906589891905));
#74456=CARTESIAN_POINT('Ctrl Pts',(-0.237514903826011,9.25041757272602E-5,
-1.6709410108095));
#74457=CARTESIAN_POINT('Ctrl Pts',(-0.23715004766578,-0.0730491814008578,
-1.66601312039815));
#74458=CARTESIAN_POINT('Ctrl Pts',(-0.161834267745582,-0.225190701072496,
-1.65580640364513));
#74459=CARTESIAN_POINT('Ctrl Pts',(0.0968635373620719,-0.262806695604708,
-1.64032086055044));
#74460=CARTESIAN_POINT('Ctrl Pts',(0.273176132803676,-0.0618441946515969,
-1.62448438152544));
#74461=CARTESIAN_POINT('Ctrl Pts',(0.200610662303521,0.195461674084374,
-1.60864790250043));
#74462=CARTESIAN_POINT('Ctrl Pts',(-0.054721849483307,0.274691505419439,
-1.59281142347543));
#74463=CARTESIAN_POINT('Ctrl Pts',(-0.21780389038128,0.138950785472986,
-1.58024245957845));
#74464=CARTESIAN_POINT('Ctrl Pts',(-0.237041003877058,0.0301995974238838,
-1.57295232202314));
#74465=CARTESIAN_POINT('Ctrl Pts',(-0.236877981323345,0.000140284900710819,
-1.5709410108095));
#74466=CARTESIAN_POINT('Origin',(0.,0.,-2.1406589891905));
#74467=CARTESIAN_POINT('',(-0.2368232568105,8.99543112184168E-5,-1.7906589891905));
#74468=CARTESIAN_POINT('',(-0.237139424499073,-0.000213821819175564,-1.7709410108095));
#74469=CARTESIAN_POINT('',(-0.237175,-2.3095687792789E-14,-2.1406589891905));
#74470=CARTESIAN_POINT('Ctrl Pts',(-0.2368232568105,8.99543112184049E-5,
-1.7906589891905));
#74471=CARTESIAN_POINT('Ctrl Pts',(-0.23666890749081,-0.0450718694273936,
-1.78763890303532));
#74472=CARTESIAN_POINT('Ctrl Pts',(-0.202527805976921,-0.169388758838487,
-1.77933999053847));
#74473=CARTESIAN_POINT('Ctrl Pts',(-0.0018172011087593,-0.280082930068666,
-1.76576225169995));
#74474=CARTESIAN_POINT('Ctrl Pts',(0.23393822438801,-0.154022249166496,
-1.74992577267494));
#74475=CARTESIAN_POINT('Ctrl Pts',(0.256563515396163,0.112361471630493,
-1.73408929364994));
#74476=CARTESIAN_POINT('Ctrl Pts',(0.0454456721551229,0.27637760331013,
-1.71825281462493));
#74477=CARTESIAN_POINT('Ctrl Pts',(-0.185394253897758,0.196135715711487,
-1.70377604647179));
#74478=CARTESIAN_POINT('Ctrl Pts',(-0.23659897516297,0.0582094498664757,
-1.69457810466031));
#74479=CARTESIAN_POINT('Ctrl Pts',(-0.237117339234101,-0.000212911088445088,
-1.6906589891905));
#74480=CARTESIAN_POINT('Ctrl Pts',(-0.237139424499073,-0.00021382181917559,
-1.7709410108095));
#74481=CARTESIAN_POINT('Ctrl Pts',(-0.237314764965966,-0.0197290375198751,
-1.76963157145649));
#74482=CARTESIAN_POINT('Ctrl Pts',(-0.226202839931557,-0.117720212646404,
-1.76304330576182));
#74483=CARTESIAN_POINT('Ctrl Pts',(-0.0904793175238351,-0.265072392539203,
-1.75117621372547));
#74484=CARTESIAN_POINT('Ctrl Pts',(0.173073393005469,-0.22021696378749,
-1.73533973470047));
#74485=CARTESIAN_POINT('Ctrl Pts',(0.278947013657325,0.025267969059772,
-1.71950325567547));
#74486=CARTESIAN_POINT('Ctrl Pts',(0.130684973650179,0.247732392338888,
-1.70366677665046));
#74487=CARTESIAN_POINT('Ctrl Pts',(-0.136638058709272,0.244499378342932,
-1.68783029762546));
#74488=CARTESIAN_POINT('Ctrl Pts',(-0.235028993377773,0.0888348674575675,
-1.6769217090118));
#74489=CARTESIAN_POINT('Ctrl Pts',(-0.2375408867772,0.00530123313075793,
-1.67129194673982));
#74490=CARTESIAN_POINT('Ctrl Pts',(-0.237514903826011,9.25041757272602E-5,
-1.6709410108095));
#74491=CARTESIAN_POINT('Origin',(0.,0.,-2.1406589891905));
#74492=CARTESIAN_POINT('',(-0.2374378448428,0.000162859811871453,-1.8906589891905));
#74493=CARTESIAN_POINT('',(-0.236814675525433,8.00967394152252E-5,-1.8709410108095));
#74494=CARTESIAN_POINT('',(-0.237175,-2.3095687792789E-14,-2.1406589891905));
#74495=CARTESIAN_POINT('Ctrl Pts',(-0.2374378448428,0.00016285981187146,
-1.8906589891905));
#74496=CARTESIAN_POINT('Ctrl Pts',(-0.236931225259905,-0.0693600600496425,
-1.88597852775199));
#74497=CARTESIAN_POINT('Ctrl Pts',(-0.168060902149697,-0.218219163221255,
-1.87601923997182));
#74498=CARTESIAN_POINT('Ctrl Pts',(0.0845081317806936,-0.26702286775457,
-1.86078112584997));
#74499=CARTESIAN_POINT('Ctrl Pts',(0.269994415115787,-0.0745204288506152,
-1.84494464682497));
#74500=CARTESIAN_POINT('Ctrl Pts',(0.209506119993022,0.185900050867469,
-1.82910816779996));
#74501=CARTESIAN_POINT('Ctrl Pts',(-0.0418559526817564,0.27694205992973,
-1.81327168877496));
#74502=CARTESIAN_POINT('Ctrl Pts',(-0.214420236326383,0.146435126422962,
-1.80045529590514));
#74503=CARTESIAN_POINT('Ctrl Pts',(-0.236938695573908,0.033866747730932,
-1.79291772937699));
#74504=CARTESIAN_POINT('Ctrl Pts',(-0.2368232568105,8.99543112184049E-5,
-1.7906589891905));
#74505=CARTESIAN_POINT('Ctrl Pts',(-0.236814675525433,8.00967394152356E-5,
-1.8709410108095));
#74506=CARTESIAN_POINT('Ctrl Pts',(-0.236682471177008,-0.0443344101141993,
-1.86797119617317));
#74507=CARTESIAN_POINT('Ctrl Pts',(-0.203385542392388,-0.167881339256242,
-1.85972255519517));
#74508=CARTESIAN_POINT('Ctrl Pts',(-0.00447048967563682,-0.280051476296464,
-1.8461950878755));
#74509=CARTESIAN_POINT('Ctrl Pts',(0.232467885064925,-0.156232942395582,
-1.8303586088505));
#74510=CARTESIAN_POINT('Ctrl Pts',(0.257616875906963,0.109925723244754,
-1.81452212982549));
#74511=CARTESIAN_POINT('Ctrl Pts',(0.0480624401227571,0.27593430904298,
-1.79868565080049));
#74512=CARTESIAN_POINT('Ctrl Pts',(-0.18433154866488,0.197612718219552,
-1.78415861112849));
#74513=CARTESIAN_POINT('Ctrl Pts',(-0.236607903763674,0.0589438956462287,
-1.77491039779816));
#74514=CARTESIAN_POINT('Ctrl Pts',(-0.237139424499073,-0.00021382181917559,
-1.7709410108095));
#74515=CARTESIAN_POINT('Origin',(3.51939854619125E-17,0.,-0.0249999999999999));
#74516=CARTESIAN_POINT('Ctrl Pts',(0.131476569578105,0.197850242677352,
-0.0250000000000002));
#74517=CARTESIAN_POINT('Ctrl Pts',(0.126716365602224,0.201929436190152,
-0.0250000000000002));
#74518=CARTESIAN_POINT('Ctrl Pts',(0.121794351938759,0.20579944606451,-0.0250000000000006));
#74519=CARTESIAN_POINT('Ctrl Pts',(0.116719086571287,0.20944676365964,-0.0250000000000006));
#74520=CARTESIAN_POINT('Ctrl Pts',(0.106659704771955,0.216675895059939,
-0.0250000000000007));
#74521=CARTESIAN_POINT('Ctrl Pts',(0.0959995500509429,0.223031524528497,
-0.0250000000000006));
#74522=CARTESIAN_POINT('Ctrl Pts',(0.0848629171244075,0.228527486118004,
-0.0250000000000008));
#74523=CARTESIAN_POINT('Ctrl Pts',(0.0793089010339903,0.231268409636073,
-0.025000000000001));
#74524=CARTESIAN_POINT('Ctrl Pts',(0.0736338496400286,0.233795650870042,
-0.0250000000000003));
#74525=CARTESIAN_POINT('Ctrl Pts',(0.0678738710164064,0.236101576769272,
-0.0250000000000002));
#74526=CARTESIAN_POINT('Ctrl Pts',(0.0569403363432262,0.240478662592059,
-0.0250000000000001));
#74527=CARTESIAN_POINT('Ctrl Pts',(0.0456859446130353,0.244067694746422,
-0.0250000000000007));
#74528=CARTESIAN_POINT('Ctrl Pts',(0.0342108064996598,0.246877609869612,
-0.0250000000000009));
#74529=CARTESIAN_POINT('Ctrl Pts',(0.0287705040427049,0.248209775809358,
-0.025000000000001));
#74530=CARTESIAN_POINT('Ctrl Pts',(0.0232804045968881,0.249366613402048,
-0.0250000000000005));
#74531=CARTESIAN_POINT('Ctrl Pts',(0.0177504039195654,0.250347887861532,
-0.0250000000000006));
#74532=CARTESIAN_POINT('Ctrl Pts',(0.0130278961939813,0.251185876224686,
-0.0250000000000008));
#74533=CARTESIAN_POINT('Ctrl Pts',(0.00828050256328347,0.251894890254572,
-0.0250000000000001));
#74534=CARTESIAN_POINT('Ctrl Pts',(0.0035240847247141,0.25247435018727,
-0.0250000000000001));
#74535=CARTESIAN_POINT('Ctrl Pts',(-0.0123782977924341,0.254411689129278,
-0.0250000000000002));
#74536=CARTESIAN_POINT('Ctrl Pts',(-0.0284103017332684,0.254910094217844,
-0.0250000000000004));
#74537=CARTESIAN_POINT('Ctrl Pts',(-0.0443431569787997,0.253981160003125,
-0.0250000000000001));
#74538=CARTESIAN_POINT('Ctrl Pts',(-0.0551143822635383,0.253353164609503,
-0.025));
#74539=CARTESIAN_POINT('Ctrl Pts',(-0.0658410506795728,0.252071912508136,
-0.0250000000000004));
#74540=CARTESIAN_POINT('Ctrl Pts',(-0.0764558373066276,0.25012806300835,
-0.0250000000000005));
#74541=CARTESIAN_POINT('Ctrl Pts',(-0.0819514088173798,0.249121677830057,
-0.0250000000000005));
#74542=CARTESIAN_POINT('Ctrl Pts',(-0.0874204046766468,0.24793629687224,
-0.0250000000000001));
#74543=CARTESIAN_POINT('Ctrl Pts',(-0.0928277779543753,0.246576938729842,
-0.0250000000000002));
#74544=CARTESIAN_POINT('Ctrl Pts',(-0.103820657960877,0.243813441523762,
-0.0250000000000004));
#74545=CARTESIAN_POINT('Ctrl Pts',(-0.114579390862407,0.240328871965648,
-0.0250000000000003));
#74546=CARTESIAN_POINT('Ctrl Pts',(-0.125027804890083,0.236123432466162,
-0.0250000000000002));
#74547=CARTESIAN_POINT('Ctrl Pts',(-0.135775670547118,0.231797465037082,
-0.0250000000000002));
#74548=CARTESIAN_POINT('Ctrl Pts',(-0.146195566282993,0.226708934356136,
-0.0250000000000006));
#74549=CARTESIAN_POINT('Ctrl Pts',(-0.156252054460305,0.220927740860517,
-0.0250000000000006));
#74550=CARTESIAN_POINT('Ctrl Pts',(-0.162623320317708,0.21726507849924,
-0.0250000000000006));
#74551=CARTESIAN_POINT('Ctrl Pts',(-0.168848671260019,0.213324078716014,
-0.0250000000000001));
#74552=CARTESIAN_POINT('Ctrl Pts',(-0.174918101511351,0.209119677449694,
-0.025));
#74553=CARTESIAN_POINT('Ctrl Pts',(-0.178478882090543,0.206653062008656,
-0.025));
#74554=CARTESIAN_POINT('Ctrl Pts',(-0.181984449689504,0.204096577325674,
-0.0250000000000006));
#74555=CARTESIAN_POINT('Ctrl Pts',(-0.185423585478161,0.201460877808261,
-0.0250000000000006));
#74556=CARTESIAN_POINT('Ctrl Pts',(-0.198547347273593,0.191403033408821,
-0.0250000000000004));
#74557=CARTESIAN_POINT('Ctrl Pts',(-0.210743690822958,0.180169353014819,
-0.0250000000000002));
#74558=CARTESIAN_POINT('Ctrl Pts',(-0.221915859342723,0.167954146424944,
-0.0249999999999998));
#74559=CARTESIAN_POINT('Ctrl Pts',(-0.232159167234076,0.156754519258988,
-0.0249999999999995));
#74560=CARTESIAN_POINT('Ctrl Pts',(-0.241542045610028,0.144728551000905,
-0.0250000000000004));
#74561=CARTESIAN_POINT('Ctrl Pts',(-0.249971624146837,0.131994872381627,
-0.0250000000000007));
#74562=CARTESIAN_POINT('Ctrl Pts',(-0.252429636980731,0.128281810651176,
-0.0250000000000007));
#74563=CARTESIAN_POINT('Ctrl Pts',(-0.254804760717037,0.124510660490947,
-0.025));
#74564=CARTESIAN_POINT('Ctrl Pts',(-0.257089474046572,0.120693732425444,
-0.025));
#74565=CARTESIAN_POINT('Ctrl Pts',(-0.266057137277679,0.105712016764972,
-0.0249999999999999));
#74566=CARTESIAN_POINT('Ctrl Pts',(-0.273660374531991,0.08998965119933,
-0.0250000000000001));
#74567=CARTESIAN_POINT('Ctrl Pts',(-0.279780120884689,0.0737160442147271,
-0.025));
#74568=CARTESIAN_POINT('Ctrl Pts',(-0.285570983375405,0.0583170039858358,
-0.025));
#74569=CARTESIAN_POINT('Ctrl Pts',(-0.290034213990896,0.0424230946399918,
-0.0249999999999999));
#74570=CARTESIAN_POINT('Ctrl Pts',(-0.293033728012268,0.0261701021632011,
-0.0249999999999999));
#74571=CARTESIAN_POINT('',(-0.201387638828722,-0.215099443244976,-0.0249999999999996));
#74572=CARTESIAN_POINT('Origin',(0.,0.,-0.025));
#74573=CARTESIAN_POINT('Ctrl Pts',(-0.201391095966877,-0.215105632705572,
-0.0250000000000002));
#74574=CARTESIAN_POINT('Ctrl Pts',(-0.195338847091654,-0.219844285114016,
-0.0250000000000002));
#74575=CARTESIAN_POINT('Ctrl Pts',(-0.189099169329539,-0.224321659220154,
-0.025));
#74576=CARTESIAN_POINT('Ctrl Pts',(-0.182677962217615,-0.228519790588707,
-0.025));
#74577=CARTESIAN_POINT('Ctrl Pts',(-0.172360604925975,-0.235265192275904,
-0.0249999999999999));
#74578=CARTESIAN_POINT('Ctrl Pts',(-0.161574657667912,-0.241290326536744,
-0.0249999999999998));
#74579=CARTESIAN_POINT('Ctrl Pts',(-0.150403499846521,-0.246587801858931,
-0.0249999999999996));
#74580=CARTESIAN_POINT('Ctrl Pts',(-0.145346996730436,-0.248985646460386,
-0.0249999999999995));
#74581=CARTESIAN_POINT('Ctrl Pts',(-0.140211528852807,-0.251234232658866,
-0.0249999999999997));
#74582=CARTESIAN_POINT('Ctrl Pts',(-0.135004748169044,-0.253332011186455,
-0.0249999999999997));
#74583=CARTESIAN_POINT('Ctrl Pts',(-0.12994533197591,-0.255370417506351,
-0.0249999999999997));
#74584=CARTESIAN_POINT('Ctrl Pts',(-0.124827943389512,-0.25726265675066,
-0.0249999999999999));
#74585=CARTESIAN_POINT('Ctrl Pts',(-0.119660402636152,-0.259008400564028,
-0.0249999999999999));
#74586=CARTESIAN_POINT('Ctrl Pts',(-0.110196620014646,-0.262205538380852,
-0.0249999999999998));
#74587=CARTESIAN_POINT('Ctrl Pts',(-0.100564090906767,-0.264911882417756,
-0.0249999999999998));
#74588=CARTESIAN_POINT('Ctrl Pts',(-0.0908073980509052,-0.267122077440192,
-0.0249999999999994));
#74589=CARTESIAN_POINT('Ctrl Pts',(-0.0835768486991839,-0.268760022225657,
-0.0249999999999992));
#74590=CARTESIAN_POINT('Ctrl Pts',(-0.0762780787142024,-0.27012535733669,
-0.0249999999999998));
#74591=CARTESIAN_POINT('Ctrl Pts',(-0.0689294737833452,-0.271213850448778,
-0.0249999999999998));
#74592=CARTESIAN_POINT('Ctrl Pts',(-0.0632148208849618,-0.272060318639189,
-0.0249999999999998));
#74593=CARTESIAN_POINT('Ctrl Pts',(-0.0574681181846967,-0.272739188122278,
-0.0249999999999998));
#74594=CARTESIAN_POINT('Ctrl Pts',(-0.051719859743331,-0.273246779822699,
-0.0249999999999998));
#74595=CARTESIAN_POINT('Ctrl Pts',(-0.0350403730953272,-0.27471963791984,
-0.0249999999999999));
#74596=CARTESIAN_POINT('Ctrl Pts',(-0.0183065933647195,-0.274761316818117,
-0.0249999999999997));
#74597=CARTESIAN_POINT('Ctrl Pts',(-0.00173104857140306,-0.27333838879637,
-0.0249999999999999));
#74598=CARTESIAN_POINT('Ctrl Pts',(0.00953470964504997,-0.27237127952471,
-0.0250000000000001));
#74599=CARTESIAN_POINT('Ctrl Pts',(0.0207273828667504,-0.270726566241235,
-0.0250000000000006));
#74600=CARTESIAN_POINT('Ctrl Pts',(0.0317746405774151,-0.268380747632881,
-0.0250000000000006));
#74601=CARTESIAN_POINT('Ctrl Pts',(0.0362763732629953,-0.267424831822799,
-0.0250000000000006));
#74602=CARTESIAN_POINT('Ctrl Pts',(0.0407560491401004,-0.266351784795418,
-0.0249999999999997));
#74603=CARTESIAN_POINT('Ctrl Pts',(0.045201428945242,-0.265161414452212,
-0.0249999999999998));
#74604=CARTESIAN_POINT('Ctrl Pts',(0.0584062062305173,-0.261625479176028,
-0.0249999999999999));
#74605=CARTESIAN_POINT('Ctrl Pts',(0.0712526578246137,-0.257072554296891,
-0.0249999999999997));
#74606=CARTESIAN_POINT('Ctrl Pts',(0.0836175868965339,-0.251475521354251,
-0.0249999999999999));
#74607=CARTESIAN_POINT('Ctrl Pts',(0.0983243165227789,-0.244818463338163,
-0.0250000000000001));
#74608=CARTESIAN_POINT('Ctrl Pts',(0.112351532683777,-0.236684173702826,
-0.0249999999999998));
#74609=CARTESIAN_POINT('Ctrl Pts',(0.125552777046004,-0.227237104745598,
-0.0249999999999998));
#74610=CARTESIAN_POINT('Ctrl Pts',(0.129065689842232,-0.224723195562791,
-0.0249999999999998));
#74611=CARTESIAN_POINT('Ctrl Pts',(0.132522069792216,-0.222114399692458,
-0.0250000000000002));
#74612=CARTESIAN_POINT('Ctrl Pts',(0.135911222128229,-0.219419463926651,
-0.0250000000000001));
#74613=CARTESIAN_POINT('Ctrl Pts',(0.148285308267569,-0.209580022083998,
-0.025));
#74614=CARTESIAN_POINT('Ctrl Pts',(0.159725584980566,-0.198630141850697,
-0.0250000000000001));
#74615=CARTESIAN_POINT('Ctrl Pts',(0.170107075094728,-0.186737543339766,
-0.0250000000000002));
#74616=CARTESIAN_POINT('Ctrl Pts',(0.17813376360681,-0.177542506519736,
-0.0250000000000002));
#74617=CARTESIAN_POINT('Ctrl Pts',(0.185526921828335,-0.167782839977552,
-0.025));
#74618=CARTESIAN_POINT('Ctrl Pts',(0.19220906976002,-0.157527458546528,
-0.0250000000000002));
#74619=CARTESIAN_POINT('Ctrl Pts',(0.194577331723896,-0.153892784484171,
-0.0250000000000002));
#74620=CARTESIAN_POINT('Ctrl Pts',(0.196857099713073,-0.150194088388506,
-0.0249999999999999));
#74621=CARTESIAN_POINT('Ctrl Pts',(0.199041135849217,-0.146439874642851,
-0.0249999999999999));
#74622=CARTESIAN_POINT('Ctrl Pts',(0.206823250530982,-0.133062933929713,
-0.0250000000000001));
#74623=CARTESIAN_POINT('Ctrl Pts',(0.213351473427119,-0.119058256565258,
-0.0249999999999998));
#74624=CARTESIAN_POINT('Ctrl Pts',(0.218485133420207,-0.104575147054428,
-0.0249999999999999));
#74625=CARTESIAN_POINT('Ctrl Pts',(0.223304523482539,-0.0909786575825654,
-0.0249999999999999));
#74626=CARTESIAN_POINT('Ctrl Pts',(0.226894965471101,-0.0769592713588295,
-0.0249999999999996));
#74627=CARTESIAN_POINT('Ctrl Pts',(0.22909166963358,-0.0626392569880559,
-0.0249999999999996));
#74628=CARTESIAN_POINT('Ctrl Pts',(0.229234915574686,-0.0617054562650307,
-0.0249999999999996));
#74629=CARTESIAN_POINT('Ctrl Pts',(0.229372216589657,-0.0607703803898239,
-0.0249999999999999));
#74630=CARTESIAN_POINT('Ctrl Pts',(0.229503519150545,-0.0598340649004849,
-0.0249999999999999));
#74631=CARTESIAN_POINT('Ctrl Pts',(-0.103908919352511,0.213201587949043,
-1.98872339910054));
#74632=CARTESIAN_POINT('Ctrl Pts',(-0.174623289681621,0.178737239562729,
-1.98344457275887));
#74633=CARTESIAN_POINT('Ctrl Pts',(-0.277869171354646,0.0345363745701341,
-1.97288692007553));
#74634=CARTESIAN_POINT('Ctrl Pts',(-0.180080572943209,-0.214762747691729,
-1.95705044105053));
#74635=CARTESIAN_POINT('Ctrl Pts',(0.0820053757571985,-0.267731452091956,
-1.94121396202553));
#74636=CARTESIAN_POINT('Ctrl Pts',(0.269259772704402,-0.077117310153115,
-1.92537748300052));
#74637=CARTESIAN_POINT('Ctrl Pts',(0.211266823136741,0.183928328504729,
-1.90954100397552));
#74638=CARTESIAN_POINT('Ctrl Pts',(-0.0392343044552656,0.277314777777813,
-1.89370452495051));
#74639=CARTESIAN_POINT('Ctrl Pts',(-0.253973708582438,0.118100076701569,
-1.87786804592551));
#74640=CARTESIAN_POINT('Ctrl Pts',(-0.237338474913823,-0.148734949670181,
-1.8620315669005));
#74641=CARTESIAN_POINT('Ctrl Pts',(-0.00447048967563682,-0.280051476296464,
-1.8461950878755));
#74642=CARTESIAN_POINT('Ctrl Pts',(0.232467885064925,-0.156232942395582,
-1.8303586088505));
#74643=CARTESIAN_POINT('Ctrl Pts',(0.257616875906963,0.109925723244754,
-1.81452212982549));
#74644=CARTESIAN_POINT('Ctrl Pts',(0.0480624401227571,0.27593430904298,
-1.79868565080049));
#74645=CARTESIAN_POINT('Ctrl Pts',(-0.205279094840265,0.190552960999229,
-1.78284917177548));
#74646=CARTESIAN_POINT('Ctrl Pts',(-0.271600582044837,-0.0684328367816128,
-1.76701269275048));
#74647=CARTESIAN_POINT('Ctrl Pts',(-0.0904793175238351,-0.265072392539203,
-1.75117621372547));
#74648=CARTESIAN_POINT('Ctrl Pts',(0.173073393005469,-0.22021696378749,
-1.73533973470047));
#74649=CARTESIAN_POINT('Ctrl Pts',(0.278947013657325,0.025267969059772,
-1.71950325567547));
#74650=CARTESIAN_POINT('Ctrl Pts',(0.130684973650179,0.247732392338888,
-1.70366677665046));
#74651=CARTESIAN_POINT('Ctrl Pts',(-0.136638058709272,0.244499378342932,
-1.68783029762546));
#74652=CARTESIAN_POINT('Ctrl Pts',(-0.279476516397372,0.018514345000666,
-1.67199381860045));
#74653=CARTESIAN_POINT('Ctrl Pts',(-0.167696920049829,-0.224338241203619,
-1.65615733957545));
#74654=CARTESIAN_POINT('Ctrl Pts',(0.0968635373620719,-0.262806695604708,
-1.64032086055044));
#74655=CARTESIAN_POINT('Ctrl Pts',(0.273176132803676,-0.0618441946515969,
-1.62448438152544));
#74656=CARTESIAN_POINT('Ctrl Pts',(0.200610662303521,0.195461674084374,
-1.60864790250043));
#74657=CARTESIAN_POINT('Ctrl Pts',(-0.054721849483307,0.274691505419439,
-1.59281142347543));
#74658=CARTESIAN_POINT('Ctrl Pts',(-0.260199830103213,0.103662685391739,
-1.57697494445043));
#74659=CARTESIAN_POINT('Ctrl Pts',(-0.22862185072271,-0.161808384494801,
-1.56113846542542));
#74660=CARTESIAN_POINT('Ctrl Pts',(0.011242860680614,-0.279863363121343,
-1.54530198640042));
#74661=CARTESIAN_POINT('Ctrl Pts',(0.240864724779504,-0.142947851629034,
-1.52946550737541));
#74662=CARTESIAN_POINT('Ctrl Pts',(0.251045943848778,0.124200797119059,
-1.51362902835041));
#74663=CARTESIAN_POINT('Ctrl Pts',(0.0325108828631745,0.278195877800473,
-1.4977925493254));
#74664=CARTESIAN_POINT('Ctrl Pts',(-0.215643331000489,0.178739636689401,
-1.4819560703004));
#74665=CARTESIAN_POINT('Ctrl Pts',(-0.267334938339562,-0.083557971922713,
-1.46611959127539));
#74666=CARTESIAN_POINT('Ctrl Pts',(-0.0754701205516332,-0.269729799675546,
-1.45028311225039));
#74667=CARTESIAN_POINT('Ctrl Pts',(0.185152012983061,-0.210163355552944,
-1.43444663322539));
#74668=CARTESIAN_POINT('Ctrl Pts',(0.277090761295361,0.0408731444070958,
-1.41861015420038));
#74669=CARTESIAN_POINT('Ctrl Pts',(0.116585008054319,0.254672024034776,
-1.40277367517538));
#74670=CARTESIAN_POINT('Ctrl Pts',(-0.150135922153628,0.236451070642649,
-1.38693719615037));
#74671=CARTESIAN_POINT('Ctrl Pts',(-0.280074998444266,0.00281054717502342,
-1.37110071712537));
#74672=CARTESIAN_POINT('Ctrl Pts',(-0.154850773550475,-0.233390535069016,
-1.35526423810037));
#74673=CARTESIAN_POINT('Ctrl Pts',(0.11145078701977,-0.256960358813676,
-1.33942775907536));
#74674=CARTESIAN_POINT('Ctrl Pts',(0.276214720548922,-0.0464255541815164,
-1.32359128005036));
#74675=CARTESIAN_POINT('Ctrl Pts',(0.189332272492804,0.206405413014511,
-1.30775480102535));
#74676=CARTESIAN_POINT('Ctrl Pts',(-0.0700420007471637,0.271190010989185,
-1.29191832200035));
#74677=CARTESIAN_POINT('Ctrl Pts',(-0.265604265662634,0.0889060064944594,
-1.27608184297534));
#74678=CARTESIAN_POINT('Ctrl Pts',(-0.219186840810713,-0.174376124353075,
-1.26024536395034));
#74679=CARTESIAN_POINT('Ctrl Pts',(0.0269215174987288,-0.278792280783643,
-1.24440888492533));
#74680=CARTESIAN_POINT('Ctrl Pts',(0.248502933681857,-0.129213760414636,
-1.22857240590033));
#74681=CARTESIAN_POINT('Ctrl Pts',(0.243684888061905,0.138085405670681,
-1.21273592687532));
#74682=CARTESIAN_POINT('Ctrl Pts',(0.0168568778538109,0.279581382781475,
-1.19689944785032));
#74683=CARTESIAN_POINT('Ctrl Pts',(-0.22532864953623,0.166363768973774,
-1.18106296882532));
#74684=CARTESIAN_POINT('Ctrl Pts',(-0.262227727273618,-0.0984201350227347,
-1.16522648980031));
#74685=CARTESIAN_POINT('Ctrl Pts',(-0.0602233222835258,-0.273538032789071,
-1.14939001077531));
#74686=CARTESIAN_POINT('Ctrl Pts',(0.196647749876134,-0.199448154660888,
-1.1335535317503));
#74687=CARTESIAN_POINT('Ctrl Pts',(0.274362205745136,0.0563496582744192,
-1.1177170527253));
#74688=CARTESIAN_POINT('Ctrl Pts',(0.102118020082256,0.260809919104815,
-1.1018805737003));
#74689=CARTESIAN_POINT('Ctrl Pts',(-0.16316114285223,0.227658396269794,
-1.08604409467529));
#74690=CARTESIAN_POINT('Ctrl Pts',(-0.279791779261826,-0.012902100080281,
-1.07020761565029));
#74691=CARTESIAN_POINT('Ctrl Pts',(-0.141517142307931,-0.241708093290185,
-1.05437113662528));
#74692=CARTESIAN_POINT('Ctrl Pts',(0.125687179216381,-0.250305087662256,
-1.03853465760028));
#74693=CARTESIAN_POINT('Ctrl Pts',(0.278383759087368,-0.0308607615811162,
-1.02269817857527));
#74694=CARTESIAN_POINT('Ctrl Pts',(0.177457847270645,0.216699368644785,
-1.00686169955027));
#74695=CARTESIAN_POINT('Ctrl Pts',(-0.0851416533425872,0.26683478557915,
-0.991025220525264));
#74696=CARTESIAN_POINT('Ctrl Pts',(-0.270172554631098,0.0738694432975277,
-0.975188741500262));
#74697=CARTESIAN_POINT('Ctrl Pts',(-0.209061810603051,-0.186394912152542,
-0.959352262475254));
#74698=CARTESIAN_POINT('Ctrl Pts',(0.0425154229059733,-0.276843534770285,
-0.943515783450253));
#74699=CARTESIAN_POINT('Ctrl Pts',(0.255358832545678,-0.115072892419929,
-0.927679304425247));
#74700=CARTESIAN_POINT('Ctrl Pts',(0.2355566898837,0.151535308690796,-0.911842825400244));
#74701=CARTESIAN_POINT('Ctrl Pts',(0.00114980584647748,0.280086739913719,
-0.896006346375237));
#74702=CARTESIAN_POINT('Ctrl Pts',(-0.23430461280518,0.153464172845634,
-0.880169867350236));
#74703=CARTESIAN_POINT('Ctrl Pts',(-0.25629499925759,-0.112972462505392,
-0.86433338832523));
#74704=CARTESIAN_POINT('Ctrl Pts',(-0.0447869354702739,-0.276485143073116,
-0.848496909300226));
#74705=CARTESIAN_POINT('Ctrl Pts',(0.20752442160637,-0.188105072674614,
-0.832660430275222));
#74706=CARTESIAN_POINT('Ctrl Pts',(0.270769932793133,0.0716487782462665,
-0.816823951250217));
#74707=CARTESIAN_POINT('Ctrl Pts',(0.0873295552116665,0.266126760615149,
-0.800987472225213));
#74708=CARTESIAN_POINT('Ctrl Pts',(-0.175672717299923,0.218149032373378,
-0.785150993200208));
#74709=CARTESIAN_POINT('Ctrl Pts',(-0.278627749881924,-0.0285741303405044,
-0.769314514175204));
#74710=CARTESIAN_POINT('Ctrl Pts',(-0.127738002114452,-0.249264732252255,
-0.753478035150199));
#74711=CARTESIAN_POINT('Ctrl Pts',(0.139527896638572,-0.242861833124507,
-0.737641556125195));
#74712=CARTESIAN_POINT('Ctrl Pts',(0.279676420005076,-0.015198816471186,
-0.721805077100191));
#74713=CARTESIAN_POINT('Ctrl Pts',(0.165024768460067,0.226311134776178,
-0.705968598075186));
#74714=CARTESIAN_POINT('Ctrl Pts',(-0.0999732721998829,0.261639539776823,
-0.690132119050183));
#74715=CARTESIAN_POINT('Ctrl Pts',(-0.273890315603988,0.0586003323141388,
-0.674295640025178));
#74716=CARTESIAN_POINT('Ctrl Pts',(-0.198278634630123,-0.197826911663192,
-0.658459161000173));
#74717=CARTESIAN_POINT('Ctrl Pts',(0.057975485860299,-0.274023259903682,
-0.64262268197517));
#74718=CARTESIAN_POINT('Ctrl Pts',(0.261410838370488,-0.100569764399713,
-0.626786202950165));
#74719=CARTESIAN_POINT('Ctrl Pts',(0.22668693762885,0.16450816465285,-0.610949723925161));
#74720=CARTESIAN_POINT('Ctrl Pts',(-0.0145608858552237,0.279710358285275,
-0.595113244900156));
#74721=CARTESIAN_POINT('Ctrl Pts',(-0.242542963650923,0.140081457418103,
-0.579276765875153));
#74722=CARTESIAN_POINT('Ctrl Pts',(-0.249555431064008,-0.12716914230876,
-0.563440286850147));
#74723=CARTESIAN_POINT('Ctrl Pts',(-0.0292095552737704,-0.278561852753679,
-0.547603807825144));
#74724=CARTESIAN_POINT('Ctrl Pts',(0.217747787412377,-0.176169818657624,
-0.531767328800138));
#74725=CARTESIAN_POINT('Ctrl Pts',(0.26632525124544,0.0867223412897275,
-0.515930849775135));
#74726=CARTESIAN_POINT('Ctrl Pts',(0.0722661688848724,0.270605810659411,
-0.50009437075013));
#74727=CARTESIAN_POINT('Ctrl Pts',(-0.187631257907944,0.207952915306194,
-0.484257891725126));
#74728=CARTESIAN_POINT('Ctrl Pts',(-0.276586574783934,-0.0441562066210817,
-0.468421412700122));
#74729=CARTESIAN_POINT('Ctrl Pts',(-0.113556730952469,-0.256036662952951,
-0.452584933675117));
#74730=CARTESIAN_POINT('Ctrl Pts',(0.15292936740834,-0.23465402726664,-0.436748454650113));
#74731=CARTESIAN_POINT('Ctrl Pts',(0.280088633943004,0.000510975941890648,
-0.420911975625108));
#74732=CARTESIAN_POINT('Ctrl Pts',(0.152072176426899,0.235210452621709,
-0.405075496600104));
#74733=CARTESIAN_POINT('Ctrl Pts',(-0.114490165816999,0.255620628817145,
-0.389239017575099));
#74734=CARTESIAN_POINT('Ctrl Pts',(-0.276745845119702,0.0431467418693552,
-0.373402538550095));
#74735=CARTESIAN_POINT('Ctrl Pts',(-0.18687125857253,-0.208636133447806,
-0.357566059525091));
#74736=CARTESIAN_POINT('Ctrl Pts',(0.0732530352383368,-0.270340335534277,
-0.341729580500087));
#74737=CARTESIAN_POINT('Ctrl Pts',(0.266639901610645,-0.0857500318774511,
-0.325893101475082));
#74738=CARTESIAN_POINT('Ctrl Pts',(0.217103548889173,0.176963130656145,
-0.310056622450078));
#74739=CARTESIAN_POINT('Ctrl Pts',(-0.0302257286171684,0.27845342881406,
-0.294220143425073));
#74740=CARTESIAN_POINT('Ctrl Pts',(-0.250017785961877,0.126257741184162,
-0.27838366440007));
#74741=CARTESIAN_POINT('Ctrl Pts',(-0.242030203238965,-0.140965459975633,
-0.262547185375064));
#74742=CARTESIAN_POINT('Ctrl Pts',(-0.0135402899116431,-0.27976166618424,
-0.246710706350061));
#74743=CARTESIAN_POINT('Ctrl Pts',(0.227285795344374,-0.163679885626449,
-0.230874227325056));
#74744=CARTESIAN_POINT('Ctrl Pts',(0.261041901008646,0.101522741173457,
-0.215037748300052));
#74745=CARTESIAN_POINT('Ctrl Pts',(0.056975763960648,0.274233261483808,
-0.199201269275047));
#74746=CARTESIAN_POINT('Ctrl Pts',(-0.199000038459435,0.197101584390596,
-0.183364790250044));
#74747=CARTESIAN_POINT('Ctrl Pts',(-0.27367292212579,-0.0595982075980484,
-0.167528311225039));
#74748=CARTESIAN_POINT('Ctrl Pts',(-0.0990213293987983,-0.262004605402092,
-0.151691832200035));
#74749=CARTESIAN_POINT('Ctrl Pts',(0.165855812771546,-0.225703615695282,
-0.13585535317503));
#74750=CARTESIAN_POINT('Ctrl Pts',(0.279606860807486,0.0162117244434021,
-0.120018874150026));
#74751=CARTESIAN_POINT('Ctrl Pts',(0.138664230983235,0.2433835073103,-0.104182395125021));
#74752=CARTESIAN_POINT('Ctrl Pts',(-0.128691327754114,0.248769867313068,
-0.0883459161000173));
#74753=CARTESIAN_POINT('Ctrl Pts',(-0.278644470573634,0.027609257706179,
-0.0725094370750125));
#74754=CARTESIAN_POINT('Ctrl Pts',(-0.175042138878516,-0.218888784921681,
-0.0566729580500086));
#74755=CARTESIAN_POINT('Ctrl Pts',(0.0886436604710861,-0.265605608028242,
-0.0408364790250042));
#74756=CARTESIAN_POINT('Ctrl Pts',(0.209657849780202,-0.135955434357285,
-0.030278826341668));
#74757=CARTESIAN_POINT('Ctrl Pts',(0.229503519150545,-0.0598340649004849,
-0.0249999999999999));
#74758=CARTESIAN_POINT('Ctrl Pts',(-0.112236674703449,0.230288577939267,
-1.97774893273369));
#74759=CARTESIAN_POINT('Ctrl Pts',(-0.188618431235458,0.193062092640366,
-1.97247010639202));
#74760=CARTESIAN_POINT('Ctrl Pts',(-0.300138929264063,0.0373042840039045,
-1.96191245370869));
#74761=CARTESIAN_POINT('Ctrl Pts',(-0.194513087151547,-0.231974856454063,
-1.94607597468368));
#74762=CARTESIAN_POINT('Ctrl Pts',(0.0885776768745912,-0.289188724929234,
-1.93023949565868));
#74763=CARTESIAN_POINT('Ctrl Pts',(0.290839532429595,-0.0832978584282747,
-1.91440301663368));
#74764=CARTESIAN_POINT('Ctrl Pts',(0.228198751866404,0.198669220157139,
-1.89856653760867));
#74765=CARTESIAN_POINT('Ctrl Pts',(-0.0423787283498021,0.29954010394735,
-1.88273005858367));
#74766=CARTESIAN_POINT('Ctrl Pts',(-0.274328370374944,0.127565178945213,
-1.86689357955866));
#74767=CARTESIAN_POINT('Ctrl Pts',(-0.25635990990481,-0.160655276440064,
-1.85105710053366));
#74768=CARTESIAN_POINT('Ctrl Pts',(-0.00482877599551976,-0.30249613451059,
-1.83522062150865));
#74769=CARTESIAN_POINT('Ctrl Pts',(0.251098967803868,-0.168754193989144,
-1.81938414248365));
#74770=CARTESIAN_POINT('Ctrl Pts',(0.278263518468496,0.118735693896566,
-1.80354766345864));
#74771=CARTESIAN_POINT('Ctrl Pts',(0.0519143928271621,0.298048997877773,
-1.78771118443364));
#74772=CARTESIAN_POINT('Ctrl Pts',(-0.22173113852568,0.20582478222966,-1.77187470540863));
#74773=CARTESIAN_POINT('Ctrl Pts',(-0.293367945371645,-0.0739173700270646,
-1.75603822638363));
#74774=CARTESIAN_POINT('Ctrl Pts',(-0.0977307606660977,-0.28631655568814,
-1.74020174735863));
#74775=CARTESIAN_POINT('Ctrl Pts',(0.186944318462953,-0.237866199387058,
-1.72436526833362));
#74776=CARTESIAN_POINT('Ctrl Pts',(0.301303154978865,0.0272930643630038,
-1.70852878930862));
#74777=CARTESIAN_POINT('Ctrl Pts',(0.141158689433044,0.26758684534212,-1.69269231028361));
#74778=CARTESIAN_POINT('Ctrl Pts',(-0.14758888306245,0.264094722217014,
-1.67685583125861));
#74779=CARTESIAN_POINT('Ctrl Pts',(-0.301875094588665,0.0199981727279622,
-1.6610193522336));
#74780=CARTESIAN_POINT('Ctrl Pts',(-0.181136949375352,-0.242317775590514,
-1.6451828732086));
#74781=CARTESIAN_POINT('Ctrl Pts',(0.104626642267832,-0.283869275017742,
-1.6293463941836));
#74782=CARTESIAN_POINT('Ctrl Pts',(0.295069768267124,-0.066800682758141,
-1.61350991515859));
#74783=CARTESIAN_POINT('Ctrl Pts',(0.216688555586061,0.211126902944442,
-1.59767343613359));
#74784=CARTESIAN_POINT('Ctrl Pts',(-0.0591075189492908,0.296706590056724,
-1.58183695710859));
#74785=CARTESIAN_POINT('Ctrl Pts',(-0.281053482907591,0.111970706381115,
-1.56600047808358));
#74786=CARTESIAN_POINT('Ctrl Pts',(-0.246944693964287,-0.174776478554483,
-1.55016399905858));
#74787=CARTESIAN_POINT('Ctrl Pts',(0.0121439170459008,-0.302292945050291,
-1.53432752003357));
#74788=CARTESIAN_POINT('Ctrl Pts',(0.260168770217893,-0.154404372818236,
-1.51849104100857));
#74789=CARTESIAN_POINT('Ctrl Pts',(0.271165960640848,0.134154840133307,
-1.50265456198356));
#74790=CARTESIAN_POINT('Ctrl Pts',(0.0351164597512303,0.300491819519417,
-1.48681808295856));
#74791=CARTESIAN_POINT('Ctrl Pts',(-0.23292601390032,0.193064681884179,
-1.47098160393355));
#74792=CARTESIAN_POINT('Ctrl Pts',(-0.288760432677517,-0.0902547054863841,
-1.45514512490855));
#74793=CARTESIAN_POINT('Ctrl Pts',(-0.0815186552123387,-0.291347229599299,
-1.43930864588355));
#74794=CARTESIAN_POINT('Ctrl Pts',(0.199990976533686,-0.227006847138492,
-1.42347216685854));
#74795=CARTESIAN_POINT('Ctrl Pts',(0.299298133717789,0.0441489127354228,
-1.40763568783354));
#74796=CARTESIAN_POINT('Ctrl Pts',(0.12592868548561,0.275082652151262,-1.39179920880853));
#74797=CARTESIAN_POINT('Ctrl Pts',(-0.162168529526256,0.255401384831746,
-1.37596272978353));
#74798=CARTESIAN_POINT('Ctrl Pts',(-0.30252154183527,0.00303579780241857,
-1.36012625075852));
#74799=CARTESIAN_POINT('Ctrl Pts',(-0.167261251554365,-0.252095563370635,
-1.34428977173352));
#74800=CARTESIAN_POINT('Ctrl Pts',(0.120382983541046,-0.277554384970663,
-1.32845329270851));
#74801=CARTESIAN_POINT('Ctrl Pts',(0.298351882896418,-0.0501463190558393,
-1.31261681368351));
#74802=CARTESIAN_POINT('Ctrl Pts',(0.204506261936469,0.222947725199116,
-1.2967803346585));
#74803=CARTESIAN_POINT('Ctrl Pts',(-0.0756555000516231,0.292924469197482,
-1.2809438556335));
#74804=CARTESIAN_POINT('Ctrl Pts',(-0.286891055655131,0.0960313570026611,
-1.2651073766085));
#74805=CARTESIAN_POINT('Ctrl Pts',(-0.236753517452057,-0.188351456901099,
-1.24927089758349));
#74806=CARTESIAN_POINT('Ctrl Pts',(0.0290791360439149,-0.301136021076236,
-1.23343441855849));
#74807=CARTESIAN_POINT('Ctrl Pts',(0.268419141535702,-0.139569566166572,
-1.21759793953348));
#74808=CARTESIAN_POINT('Ctrl Pts',(0.263214954808303,0.149152227297988,
-1.20176146050848));
#74809=CARTESIAN_POINT('Ctrl Pts',(0.0182078682752508,0.301988365463902,
-1.18592498148348));
#74810=CARTESIAN_POINT('Ctrl Pts',(-0.243387559960744,0.179696953226935,
-1.17008850245847));
#74811=CARTESIAN_POINT('Ctrl Pts',(-0.283243905409001,-0.10630799307364,
-1.15425202343347));
#74812=CARTESIAN_POINT('Ctrl Pts',(-0.0650499059639579,-0.295460672639808,
-1.13841554440846));
#74813=CARTESIAN_POINT('Ctrl Pts',(0.212408036495276,-0.215432879047998,
-1.12257906538346));
#74814=CARTESIAN_POINT('Ctrl Pts',(0.296350898739221,0.0608657880844716,
-1.10674258635845));
#74815=CARTESIAN_POINT('Ctrl Pts',(0.110302244241902,0.281712467345497,
-1.09090610733345));
#74816=CARTESIAN_POINT('Ctrl Pts',(-0.176237653405123,0.245904023685958,
-1.07506962830844));
#74817=CARTESIAN_POINT('Ctrl Pts',(-0.302215624119569,-0.0139361357881993,
-1.05923314928344));
#74818=CARTESIAN_POINT('Ctrl Pts',(-0.152858999642686,-0.261079730295029,
-1.04339667025844));
#74819=CARTESIAN_POINT('Ctrl Pts',(0.135760347966338,-0.270365728713436,
-1.02756019123343));
#74820=CARTESIAN_POINT('Ctrl Pts',(0.300694758506864,-0.033334089895883,
-1.01172371220843));
#74821=CARTESIAN_POINT('Ctrl Pts',(0.191680163760733,0.234066687427635,
-0.995887233183423));
#74822=CARTESIAN_POINT('Ctrl Pts',(-0.091965310672772,0.288220195294412,
-0.980050754158418));
#74823=CARTESIAN_POINT('Ctrl Pts',(-0.291825469044278,0.0797896920646727,
-0.964214275133414));
#74824=CARTESIAN_POINT('Ctrl Pts',(-0.225817019133517,-0.201333487558182,
-0.94837779610841));
#74825=CARTESIAN_POINT('Ctrl Pts',(0.0459228112496179,-0.29903109328232,
-0.932541317083406));
#74826=CARTESIAN_POINT('Ctrl Pts',(0.275824504765089,-0.124295381707372,
-0.9167048380584));
#74827=CARTESIAN_POINT('Ctrl Pts',(0.254435324141974,0.163680069560886,
-0.900868359033398));
#74828=CARTESIAN_POINT('Ctrl Pts',(0.00124195675951194,0.302534224321969,
-0.885031880008392));
#74829=CARTESIAN_POINT('Ctrl Pts',(-0.253082899647124,0.165763522069517,
-0.869195400983389));
#74830=CARTESIAN_POINT('Ctrl Pts',(-0.276835700332977,-0.122026613342493,
-0.853358921958384));
#74831=CARTESIAN_POINT('Ctrl Pts',(-0.0483763736420793,-0.298643978368776,
-0.83752244293338));
#74832=CARTESIAN_POINT('Ctrl Pts',(0.224156416465443,-0.203180708483996,
-0.821685963908375));
#74833=CARTESIAN_POINT('Ctrl Pts',(0.292470723935438,0.0773910523469543,
-0.805849484883371));
#74834=CARTESIAN_POINT('Ctrl Pts',(0.0943285614109523,0.287455425839952,
-0.790013005858366));
#74835=CARTESIAN_POINT('Ctrl Pts',(-0.189751964977836,0.235632534107109,
-0.774176526833362));
#74836=CARTESIAN_POINT('Ctrl Pts',(-0.300958303884969,-0.0308641971444335,
-0.758340047808358));
#74837=CARTESIAN_POINT('Ctrl Pts',(-0.137975533572346,-0.269241994269309,
-0.742503568783354));
#74838=CARTESIAN_POINT('Ctrl Pts',(0.150710326357575,-0.262325936330895,
-0.726667089758349));
#74839=CARTESIAN_POINT('Ctrl Pts',(0.30209101942293,-0.0164169219618871,
-0.710830610733345));
#74840=CARTESIAN_POINT('Ctrl Pts',(0.178250638839094,0.244448786243956,
-0.69499413170834));
#74841=CARTESIAN_POINT('Ctrl Pts',(-0.107985606056314,0.282608577766738,
-0.679157652683337));
#74842=CARTESIAN_POINT('Ctrl Pts',(-0.295841189076202,0.0632968418538111,
-0.663321173658332));
#74843=CARTESIAN_POINT('Ctrl Pts',(-0.214169628115642,-0.213681701920165,
-0.647484694633328));
#74844=CARTESIAN_POINT('Ctrl Pts',(0.0626219172312024,-0.295984788164822,
-0.631648215608323));
#74845=CARTESIAN_POINT('Ctrl Pts',(0.282361547141194,-0.108629903980044,
-0.615811736583319));
#74846=CARTESIAN_POINT('Ctrl Pts',(0.244854707725876,0.177692631943989,
-0.599975257558314));
#74847=CARTESIAN_POINT('Ctrl Pts',(-0.015727864550129,0.302127677678435,
-0.584138778533311));
#74848=CARTESIAN_POINT('Ctrl Pts',(-0.261981511140039,0.151308252132651,
-0.568302299508305));
#74849=CARTESIAN_POINT('Ctrl Pts',(-0.269555991067417,-0.137361082634337,
-0.552465820483302));
#74850=CARTESIAN_POINT('Ctrl Pts',(-0.0315505480561581,-0.30088712544723,
-0.536629341458297));
#74851=CARTESIAN_POINT('Ctrl Pts',(0.235199131465207,-0.190288906404298,
-0.520792862433293));
#74852=CARTESIAN_POINT('Ctrl Pts',(0.287669824454071,0.0936726824752729,
-0.504956383408288));
#74853=CARTESIAN_POINT('Ctrl Pts',(0.0780579236098103,0.29229344827278,
-0.489119904383284));
#74854=CARTESIAN_POINT('Ctrl Pts',(-0.202668919946804,0.224619251689788,
-0.473283425358279));
#74855=CARTESIAN_POINT('Ctrl Pts',(-0.298753539299663,-0.0476950951809576,
-0.457446946333276));
#74856=CARTESIAN_POINT('Ctrl Pts',(-0.122657707843746,-0.276556659727332,
-0.441610467308271));
#74857=CARTESIAN_POINT('Ctrl Pts',(0.165185854779071,-0.253460317846565,
-0.425773988283267));
#74858=CARTESIAN_POINT('Ctrl Pts',(0.302536270147776,0.000551927985859205,
-0.409937509258262));
#74859=CARTESIAN_POINT('Ctrl Pts',(0.164259964432584,0.254061337777891,
-0.394101030233258));
#74860=CARTESIAN_POINT('Ctrl Pts',(-0.123665952620994,0.276107282635772,
-0.378264551208253));
#74861=CARTESIAN_POINT('Ctrl Pts',(-0.298925574318185,0.0466047271194889,
-0.362428072183249));
#74862=CARTESIAN_POINT('Ctrl Pts',(-0.201848010647438,-0.22535722618504,
-0.346591593158245));
#74863=CARTESIAN_POINT('Ctrl Pts',(0.0791238821298226,-0.292006696707592,
-0.330755114133241));
#74864=CARTESIAN_POINT('Ctrl Pts',(0.28800969239712,-0.0926224475589986,
-0.314918635108236));
#74865=CARTESIAN_POINT('Ctrl Pts',(0.234503260600505,0.191145798202142,
-0.299082156083232));
#74866=CARTESIAN_POINT('Ctrl Pts',(-0.0326481623677637,0.300770011897047,
-0.283245677058228));
#74867=CARTESIAN_POINT('Ctrl Pts',(-0.270055401287376,0.136376637485807,
-0.267409198033223));
#74868=CARTESIAN_POINT('Ctrl Pts',(-0.261427655668188,-0.152263102862543,
-0.251572719008219));
#74869=CARTESIAN_POINT('Ctrl Pts',(-0.0146254731901128,-0.302183097636622,
-0.235736239983215));
#74870=CARTESIAN_POINT('Ctrl Pts',(0.245501560748979,-0.176797970694225,
-0.21989976095821));
#74871=CARTESIAN_POINT('Ctrl Pts',(0.281963041383219,0.109659256848121,
-0.204063281933207));
#74872=CARTESIAN_POINT('Ctrl Pts',(0.0615420728603457,0.29621162027108,
-0.188226802908201));
#74873=CARTESIAN_POINT('Ctrl Pts',(-0.21494884868135,0.212898243467754,
-0.172390323883198));
#74874=CARTESIAN_POINT('Ctrl Pts',(-0.295606372649979,-0.0643746916123519,
-0.156553844858193));
#74875=CARTESIAN_POINT('Ctrl Pts',(-0.106957370028386,-0.283002901488742,
-0.140717365833189));
#74876=CARTESIAN_POINT('Ctrl Pts',(0.179148286997041,-0.243792577692436,
-0.124880886808184));
#74877=CARTESIAN_POINT('Ctrl Pts',(0.30201588542018,0.0175110091999229,
-0.10904440778318));
#74878=CARTESIAN_POINT('Ctrl Pts',(0.149777442426009,0.262889419968842,
-0.0932079287581753));
#74879=CARTESIAN_POINT('Ctrl Pts',(-0.139005263266115,0.268707468498589,
-0.0773714497331711));
#74880=CARTESIAN_POINT('Ctrl Pts',(-0.300976364652495,0.0298219950248908,
-0.0615349707081665));
#74881=CARTESIAN_POINT('Ctrl Pts',(-0.189070849000505,-0.236431573945479,
-0.0456984916831625));
#74882=CARTESIAN_POINT('Ctrl Pts',(0.0957479853203354,-0.286892505604309,
-0.0298620126581582));
#74883=CARTESIAN_POINT('Ctrl Pts',(0.226460827727168,-0.146851549945951,
-0.0193043599748219));
#74884=CARTESIAN_POINT('Ctrl Pts',(0.247897023496224,-0.0646294516415712,
-0.0140255336331538));
#74885=CARTESIAN_POINT('Ctrl Pts',(-0.120564430054386,0.247375567929492,
-1.96677446636685));
#74886=CARTESIAN_POINT('Ctrl Pts',(-0.202613572789294,0.207386945718002,
-1.96149564002518));
#74887=CARTESIAN_POINT('Ctrl Pts',(-0.322408687173481,0.0400721934376747,
-1.95093798734184));
#74888=CARTESIAN_POINT('Ctrl Pts',(-0.208945601359885,-0.249186965216397,
-1.93510150831684));
#74889=CARTESIAN_POINT('Ctrl Pts',(0.0951499779919838,-0.310645997766512,
-1.91926502929183));
#74890=CARTESIAN_POINT('Ctrl Pts',(0.312419292154789,-0.0894784067034342,
-1.90342855026683));
#74891=CARTESIAN_POINT('Ctrl Pts',(0.245130680596067,0.213410111809549,
-1.88759207124182));
#74892=CARTESIAN_POINT('Ctrl Pts',(-0.0455231522443386,0.321765430116887,
-1.87175559221682));
#74893=CARTESIAN_POINT('Ctrl Pts',(-0.29468303216745,0.137030281188856,
-1.85591911319181));
#74894=CARTESIAN_POINT('Ctrl Pts',(-0.275381344895796,-0.172575603209946,
-1.84008263416681));
#74895=CARTESIAN_POINT('Ctrl Pts',(-0.00518706231540278,-0.324940792724715,
-1.82424615514181));
#74896=CARTESIAN_POINT('Ctrl Pts',(0.269730050542811,-0.181275445582706,
-1.8084096761168));
#74897=CARTESIAN_POINT('Ctrl Pts',(0.29891016103003,0.127545664548378,-1.7925731970918));
#74898=CARTESIAN_POINT('Ctrl Pts',(0.0557663455315671,0.320163686712565,
-1.7767367180668));
#74899=CARTESIAN_POINT('Ctrl Pts',(-0.238183182211095,0.22109660346009,
-1.76090023904179));
#74900=CARTESIAN_POINT('Ctrl Pts',(-0.315135308698453,-0.0794019032725162,
-1.74506376001679));
#74901=CARTESIAN_POINT('Ctrl Pts',(-0.10498220380836,-0.307560718837078,
-1.72922728099178));
#74902=CARTESIAN_POINT('Ctrl Pts',(0.200815243920436,-0.255515434986625,
-1.71339080196678));
#74903=CARTESIAN_POINT('Ctrl Pts',(0.323659296300406,0.0293181596662353,
-1.69755432294177));
#74904=CARTESIAN_POINT('Ctrl Pts',(0.151632405215908,0.287441298345352,
-1.68171784391677));
#74905=CARTESIAN_POINT('Ctrl Pts',(-0.158539707415627,0.283690066091096,
-1.66588136489176));
#74906=CARTESIAN_POINT('Ctrl Pts',(-0.324273672779959,0.0214820004552588,
-1.65004488586676));
#74907=CARTESIAN_POINT('Ctrl Pts',(-0.194576978700875,-0.26029730997741,
-1.63420840684176));
#74908=CARTESIAN_POINT('Ctrl Pts',(0.112389747173591,-0.304931854430775,
-1.61837192781675));
#74909=CARTESIAN_POINT('Ctrl Pts',(0.316963403730571,-0.0717571708646853,
-1.60253544879175));
#74910=CARTESIAN_POINT('Ctrl Pts',(0.232766448868601,0.226792131804511,
-1.58669896976674));
#74911=CARTESIAN_POINT('Ctrl Pts',(-0.0634931884152743,0.318721674694008,
-1.57086249074174));
#74912=CARTESIAN_POINT('Ctrl Pts',(-0.30190713571197,0.12027872737049,-1.55502601171673));
#74913=CARTESIAN_POINT('Ctrl Pts',(-0.265267537205865,-0.187744572614164,
-1.53918953269173));
#74914=CARTESIAN_POINT('Ctrl Pts',(0.0130449734111871,-0.324722526979239,
-1.52335305366672));
#74915=CARTESIAN_POINT('Ctrl Pts',(0.279472815656283,-0.165860894007438,
-1.50751657464172));
#74916=CARTESIAN_POINT('Ctrl Pts',(0.291285977432917,0.144108883147556,
-1.49168009561671));
#74917=CARTESIAN_POINT('Ctrl Pts',(0.0377220366392867,0.322787761238361,
-1.47584361659171));
#74918=CARTESIAN_POINT('Ctrl Pts',(-0.25020869680015,0.207389727078957,
-1.46000713756671));
#74919=CARTESIAN_POINT('Ctrl Pts',(-0.310185927015473,-0.0969514390500553,
-1.4441706585417));
#74920=CARTESIAN_POINT('Ctrl Pts',(-0.0875671898730442,-0.312964659523051,
-1.4283341795167));
#74921=CARTESIAN_POINT('Ctrl Pts',(0.21482994008431,-0.243850338724041,
-1.4124977004917));
#74922=CARTESIAN_POINT('Ctrl Pts',(0.321505506140217,0.0474246810637503,
-1.39666122146669));
#74923=CARTESIAN_POINT('Ctrl Pts',(0.135272362916901,0.295493280267748,
-1.38082474244169));
#74924=CARTESIAN_POINT('Ctrl Pts',(-0.174201136898885,0.274351699020844,
-1.36498826341668));
#74925=CARTESIAN_POINT('Ctrl Pts',(-0.324968085226274,0.00326104842981355,
-1.34915178439168));
#74926=CARTESIAN_POINT('Ctrl Pts',(-0.179671729558254,-0.270800591672255,
-1.33331530536667));
#74927=CARTESIAN_POINT('Ctrl Pts',(0.129315180062322,-0.298148411127651,
-1.31747882634167));
#74928=CARTESIAN_POINT('Ctrl Pts',(0.320489045243914,-0.0538670839301619,
-1.30164234731666));
#74929=CARTESIAN_POINT('Ctrl Pts',(0.219680251380133,0.239490037383722,
-1.28580586829166));
#74930=CARTESIAN_POINT('Ctrl Pts',(-0.0812689993560826,0.314658927405779,
-1.26996938926666));
#74931=CARTESIAN_POINT('Ctrl Pts',(-0.308177845647628,0.103156707510862,
-1.25413291024165));
#74932=CARTESIAN_POINT('Ctrl Pts',(-0.2543201940934,-0.202326789449123,
-1.23829643121665));
#74933=CARTESIAN_POINT('Ctrl Pts',(0.0312367545891007,-0.323479761368829,
-1.22245995219164));
#74934=CARTESIAN_POINT('Ctrl Pts',(0.288335349389547,-0.149925371918507,
-1.20662347316664));
#74935=CARTESIAN_POINT('Ctrl Pts',(0.282745021554701,0.160219048925294,
-1.19078699414163));
#74936=CARTESIAN_POINT('Ctrl Pts',(0.0195588586966912,0.324395348146328,
-1.17495051511663));
#74937=CARTESIAN_POINT('Ctrl Pts',(-0.261446470385259,0.193030137480096,
-1.15911403609162));
#74938=CARTESIAN_POINT('Ctrl Pts',(-0.304260083544383,-0.114195851124544,
-1.14327755706662));
#74939=CARTESIAN_POINT('Ctrl Pts',(-0.0698764896443907,-0.317383312490547,
-1.12744107804161));
#74940=CARTESIAN_POINT('Ctrl Pts',(0.228168323114419,-0.231417603435108,
-1.11160459901661));
#74941=CARTESIAN_POINT('Ctrl Pts',(0.318339591733306,0.0653819178945236,
-1.09576811999161));
#74942=CARTESIAN_POINT('Ctrl Pts',(0.118486468401548,0.302615015586179,
-1.0799316409666));
#74943=CARTESIAN_POINT('Ctrl Pts',(-0.189314163958016,0.264149651102121,
-1.0640951619416));
#74944=CARTESIAN_POINT('Ctrl Pts',(-0.324639468977312,-0.0149701714961173,
-1.04825868291659));
#74945=CARTESIAN_POINT('Ctrl Pts',(-0.16420085697744,-0.280451367299874,
-1.03242220389159));
#74946=CARTESIAN_POINT('Ctrl Pts',(0.145833516716294,-0.290426369764615,
-1.01658572486659));
#74947=CARTESIAN_POINT('Ctrl Pts',(0.32300575792636,-0.0358074182106502,
-1.00074924584158));
#74948=CARTESIAN_POINT('Ctrl Pts',(0.205902480250821,0.251434006210486,
-0.984912766816576));
#74949=CARTESIAN_POINT('Ctrl Pts',(-0.0987889680029566,0.309605605009673,
-0.969076287791573));
#74950=CARTESIAN_POINT('Ctrl Pts',(-0.313478383457458,0.0857099408318177,
-0.953239808766568));
#74951=CARTESIAN_POINT('Ctrl Pts',(-0.242572227663983,-0.216272062963821,
-0.937403329741564));
#74952=CARTESIAN_POINT('Ctrl Pts',(0.0493301995932623,-0.321218651794355,
-0.921566850716559));
#74953=CARTESIAN_POINT('Ctrl Pts',(0.2962901769845,-0.133517870994815,-0.905730371691556));
#74954=CARTESIAN_POINT('Ctrl Pts',(0.273313958400249,0.175824830430977,
-0.889893892666551));
#74955=CARTESIAN_POINT('Ctrl Pts',(0.00133410767254648,0.324981708730219,
-0.874057413641547));
#74956=CARTESIAN_POINT('Ctrl Pts',(-0.271861186489069,0.1780628712934,-0.858220934616542));
#74957=CARTESIAN_POINT('Ctrl Pts',(-0.297376401408364,-0.131080764179595,
-0.842384455591539));
#74958=CARTESIAN_POINT('Ctrl Pts',(-0.0519658118138847,-0.320802813664435,
-0.826547976566532));
#74959=CARTESIAN_POINT('Ctrl Pts',(0.240788411324516,-0.218256344293379,
-0.81071149754153));
#74960=CARTESIAN_POINT('Ctrl Pts',(0.314171515077743,0.0831333264476419,
-0.794875018516525));
#74961=CARTESIAN_POINT('Ctrl Pts',(0.101327567610238,0.308784091064756,
-0.77903853949152));
#74962=CARTESIAN_POINT('Ctrl Pts',(-0.203831212655749,0.253116035840839,
-0.763202060466517));
#74963=CARTESIAN_POINT('Ctrl Pts',(-0.323288857888015,-0.0331542639483626,
-0.747365581441511));
#74964=CARTESIAN_POINT('Ctrl Pts',(-0.14821306503024,-0.289219256286362,
-0.731529102416508));
#74965=CARTESIAN_POINT('Ctrl Pts',(0.161892756076577,-0.281790039537284,
-0.715692623391503));
#74966=CARTESIAN_POINT('Ctrl Pts',(0.324505618840786,-0.0176350274525877,
-0.699856144366499));
#74967=CARTESIAN_POINT('Ctrl Pts',(0.19147650921812,0.262586437711734,-0.684019665341494));
#74968=CARTESIAN_POINT('Ctrl Pts',(-0.115997939912744,0.303577615756652,
-0.668183186316491));
#74969=CARTESIAN_POINT('Ctrl Pts',(-0.317792062548416,0.0679933513934832,
-0.652346707291485));
#74970=CARTESIAN_POINT('Ctrl Pts',(-0.230060621601161,-0.229536492177137,
-0.636510228266482));
#74971=CARTESIAN_POINT('Ctrl Pts',(0.0672683486021056,-0.317946316425962,
-0.620673749241476));
#74972=CARTESIAN_POINT('Ctrl Pts',(0.3033122559119,-0.116690043560375,-0.604837270216474));
#74973=CARTESIAN_POINT('Ctrl Pts',(0.263022477822901,0.190877099235128,
-0.589000791191468));
#74974=CARTESIAN_POINT('Ctrl Pts',(-0.0168948432450345,0.324544997071594,
-0.573164312166465));
#74975=CARTESIAN_POINT('Ctrl Pts',(-0.281420058629155,0.162535046847199,
-0.557327833141459));
#74976=CARTESIAN_POINT('Ctrl Pts',(-0.289556551070826,-0.147553022959913,
-0.541491354116455));
#74977=CARTESIAN_POINT('Ctrl Pts',(-0.0338915408385456,-0.32321239814078,
-0.525654875091451));
#74978=CARTESIAN_POINT('Ctrl Pts',(0.252650475518037,-0.204407994150972,
-0.509818396066447));
#74979=CARTESIAN_POINT('Ctrl Pts',(0.309014397662703,0.100623023660818,
-0.493981917041442));
#74980=CARTESIAN_POINT('Ctrl Pts',(0.0838496783347481,0.313981085886149,
-0.478145438016439));
#74981=CARTESIAN_POINT('Ctrl Pts',(-0.217706581985663,0.241285588073381,
-0.462308958991433));
#74982=CARTESIAN_POINT('Ctrl Pts',(-0.320920503815392,-0.0512339837408334,
-0.44647247996643));
#74983=CARTESIAN_POINT('Ctrl Pts',(-0.131758684735023,-0.297076656501713,
-0.430636000941424));
#74984=CARTESIAN_POINT('Ctrl Pts',(0.177442342149801,-0.272266608426489,
-0.414799521916421));
#74985=CARTESIAN_POINT('Ctrl Pts',(0.324983906352547,0.000592880029827996,
-0.398963042891416));
#74986=CARTESIAN_POINT('Ctrl Pts',(0.17644775243827,0.272912222934072,-0.383126563866412));
#74987=CARTESIAN_POINT('Ctrl Pts',(-0.13284173942499,0.296593936454399,
-0.367290084841407));
#74988=CARTESIAN_POINT('Ctrl Pts',(-0.321105303516668,0.050062712369623,
-0.351453605816403));
#74989=CARTESIAN_POINT('Ctrl Pts',(-0.216824762722347,-0.242078318922273,
-0.335617126791399));
#74990=CARTESIAN_POINT('Ctrl Pts',(0.0849947290213087,-0.313673057880906,
-0.319780647766394));
#74991=CARTESIAN_POINT('Ctrl Pts',(0.309379483183595,-0.0994948632405462,
-0.303944168741391));
#74992=CARTESIAN_POINT('Ctrl Pts',(0.251902972311837,0.205328465748139,
-0.288107689716385));
#74993=CARTESIAN_POINT('Ctrl Pts',(-0.0350705961183589,0.323086594980033,
-0.272271210691382));
#74994=CARTESIAN_POINT('Ctrl Pts',(-0.290093016612875,0.146495533787453,
-0.256434731666377));
#74995=CARTESIAN_POINT('Ctrl Pts',(-0.280825108097411,-0.163560745749454,
-0.240598252641373));
#74996=CARTESIAN_POINT('Ctrl Pts',(-0.0157106564685821,-0.324604529089004,
-0.224761773616368));
#74997=CARTESIAN_POINT('Ctrl Pts',(0.263717326153585,-0.189916055762002,
-0.208925294591364));
#74998=CARTESIAN_POINT('Ctrl Pts',(0.302884181757793,0.117795772522785,
-0.19308881556636));
#74999=CARTESIAN_POINT('Ctrl Pts',(0.0661083817600436,0.318189979058352,
-0.177252336541355));
#75000=CARTESIAN_POINT('Ctrl Pts',(-0.230897658903266,0.228694902544912,
-0.161415857516351));
#75001=CARTESIAN_POINT('Ctrl Pts',(-0.317539823174168,-0.0691511756266552,
-0.145579378491346));
#75002=CARTESIAN_POINT('Ctrl Pts',(-0.114893410657975,-0.304001197575392,
-0.129742899466343));
#75003=CARTESIAN_POINT('Ctrl Pts',(0.192440761222538,-0.261881539689589,
-0.113906420441338));
#75004=CARTESIAN_POINT('Ctrl Pts',(0.324424910032874,0.0188102939564436,
-0.0980699414163339));
#75005=CARTESIAN_POINT('Ctrl Pts',(0.160890653868784,0.282395332627384,
-0.0822334623913293));
#75006=CARTESIAN_POINT('Ctrl Pts',(-0.149319198778117,0.288645069684111,
-0.0663969833663251));
#75007=CARTESIAN_POINT('Ctrl Pts',(-0.323308258731355,0.0320347323436027,
-0.0505605043413203));
#75008=CARTESIAN_POINT('Ctrl Pts',(-0.203099559122495,-0.253974362969278,
-0.0347240253163165));
#75009=CARTESIAN_POINT('Ctrl Pts',(0.102852310169585,-0.308179403180376,
-0.0188875462913121));
#75010=CARTESIAN_POINT('Ctrl Pts',(0.243263805674134,-0.157747665534617,
-0.00832989360797585));
#75011=CARTESIAN_POINT('Ctrl Pts',(0.266290527841904,-0.0694248383826575,
-0.00305106726630777));
#75012=CARTESIAN_POINT('Ctrl Pts',(-0.128892185405323,0.264462557919717,
-1.9558));
#75013=CARTESIAN_POINT('Ctrl Pts',(-0.216608714343131,0.221711798795639,
-1.95052117365833));
#75014=CARTESIAN_POINT('Ctrl Pts',(-0.344678445082899,0.0428401028714452,
-1.93996352097499));
#75015=CARTESIAN_POINT('Ctrl Pts',(-0.223378115568222,-0.266399073978732,
-1.92412704194999));
#75016=CARTESIAN_POINT('Ctrl Pts',(0.101722279109376,-0.33210327060379,
-1.90829056292499));
#75017=CARTESIAN_POINT('Ctrl Pts',(0.333999051879982,-0.0956589549785939,
-1.89245408389998));
#75018=CARTESIAN_POINT('Ctrl Pts',(0.262062609325731,0.228151003461959,
-1.87661760487498));
#75019=CARTESIAN_POINT('Ctrl Pts',(-0.0486675761388747,0.343990756286424,
-1.86078112584997));
#75020=CARTESIAN_POINT('Ctrl Pts',(-0.315037693959957,0.1464953834325,-1.84494464682497));
#75021=CARTESIAN_POINT('Ctrl Pts',(-0.294402779886782,-0.184495929979829,
-1.82910816779997));
#75022=CARTESIAN_POINT('Ctrl Pts',(-0.00554534863528576,-0.347385450938841,
-1.81327168877496));
#75023=CARTESIAN_POINT('Ctrl Pts',(0.288361133281754,-0.193796697176269,
-1.79743520974996));
#75024=CARTESIAN_POINT('Ctrl Pts',(0.319556803591563,0.13635563520019,-1.78159873072495));
#75025=CARTESIAN_POINT('Ctrl Pts',(0.059618298235972,0.342278375547357,
-1.76576225169995));
#75026=CARTESIAN_POINT('Ctrl Pts',(-0.25463522589651,0.236368424690521,
-1.74992577267494));
#75027=CARTESIAN_POINT('Ctrl Pts',(-0.336902672025262,-0.0848864365179679,
-1.73408929364994));
#75028=CARTESIAN_POINT('Ctrl Pts',(-0.112233646950622,-0.328804881986015,
-1.71825281462494));
#75029=CARTESIAN_POINT('Ctrl Pts',(0.214686169377919,-0.273164670586193,
-1.70241633559993));
#75030=CARTESIAN_POINT('Ctrl Pts',(0.346015437621946,0.0313432549694672,
-1.68657985657493));
#75031=CARTESIAN_POINT('Ctrl Pts',(0.162106120998773,0.307295751348583,
-1.67074337754992));
#75032=CARTESIAN_POINT('Ctrl Pts',(-0.169490531768806,0.303285409965179,
-1.65490689852492));
#75033=CARTESIAN_POINT('Ctrl Pts',(-0.346672250971252,0.0229658281825551,
-1.63907041949991));
#75034=CARTESIAN_POINT('Ctrl Pts',(-0.208017008026398,-0.278276844364305,
-1.62323394047491));
#75035=CARTESIAN_POINT('Ctrl Pts',(0.120152852079351,-0.325994433843809,
-1.6073974614499));
#75036=CARTESIAN_POINT('Ctrl Pts',(0.338857039194018,-0.0767136589712294,
-1.5915609824249));
#75037=CARTESIAN_POINT('Ctrl Pts',(0.248844342151141,0.242457360664579,
-1.5757245033999));
#75038=CARTESIAN_POINT('Ctrl Pts',(-0.067878857881258,0.340736759331293,
-1.55988802437489));
#75039=CARTESIAN_POINT('Ctrl Pts',(-0.322760788516348,0.128586748359866,
-1.54405154534989));
#75040=CARTESIAN_POINT('Ctrl Pts',(-0.283590380447442,-0.200712666673845,
-1.52821506632488));
#75041=CARTESIAN_POINT('Ctrl Pts',(0.0139460297764737,-0.347152108908187,
-1.51237858729988));
#75042=CARTESIAN_POINT('Ctrl Pts',(0.298776861094673,-0.17731741519664,
-1.49654210827488));
#75043=CARTESIAN_POINT('Ctrl Pts',(0.311405994224987,0.154062926161804,
-1.48070562924987));
#75044=CARTESIAN_POINT('Ctrl Pts',(0.0403276135273424,0.345083702957305,
-1.46486915022487));
#75045=CARTESIAN_POINT('Ctrl Pts',(-0.267491379699981,0.221714772273735,
-1.44903267119986));
#75046=CARTESIAN_POINT('Ctrl Pts',(-0.331611421353429,-0.103648172613727,
-1.43319619217486));
#75047=CARTESIAN_POINT('Ctrl Pts',(-0.0936157245337495,-0.334582089446802,
-1.41735971314985));
#75048=CARTESIAN_POINT('Ctrl Pts',(0.229668903634934,-0.26069383030959,
-1.40152323412485));
#75049=CARTESIAN_POINT('Ctrl Pts',(0.343712878562645,0.0507004493920776,
-1.38568675509984));
#75050=CARTESIAN_POINT('Ctrl Pts',(0.144616040348191,0.315903908384234,
-1.36985027607484));
#75051=CARTESIAN_POINT('Ctrl Pts',(-0.186233744271513,0.293302013209942,
-1.35401379704983));
#75052=CARTESIAN_POINT('Ctrl Pts',(-0.347414628617279,0.00348629905720863,
-1.33817731802483));
#75053=CARTESIAN_POINT('Ctrl Pts',(-0.192082207562143,-0.289505619973874,
-1.32234083899983));
#75054=CARTESIAN_POINT('Ctrl Pts',(0.138247376583598,-0.318742437284638,
-1.30650435997482));
#75055=CARTESIAN_POINT('Ctrl Pts',(0.34262620759141,-0.0575878488044848,
-1.29066788094982));
#75056=CARTESIAN_POINT('Ctrl Pts',(0.234854240823797,0.256032349568327,
-1.27483140192481));
#75057=CARTESIAN_POINT('Ctrl Pts',(-0.0868824986605421,0.336393385614076,
-1.25899492289981));
#75058=CARTESIAN_POINT('Ctrl Pts',(-0.329464635640125,0.110282058019064,
-1.2431584438748));
#75059=CARTESIAN_POINT('Ctrl Pts',(-0.271886870734743,-0.216302121997147,
-1.2273219648498));
#75060=CARTESIAN_POINT('Ctrl Pts',(0.0333943731342868,-0.345823501661423,
-1.2114854858248));
#75061=CARTESIAN_POINT('Ctrl Pts',(0.308251557243392,-0.160281177670443,
-1.19564900679979));
#75062=CARTESIAN_POINT('Ctrl Pts',(0.302275088301099,0.171285870552601,
-1.17981252777479));
#75063=CARTESIAN_POINT('Ctrl Pts',(0.0209098491181311,0.346802330828755,
-1.16397604874978));
#75064=CARTESIAN_POINT('Ctrl Pts',(-0.279505380809773,0.206363321733258,
-1.14813956972478));
#75065=CARTESIAN_POINT('Ctrl Pts',(-0.325276261679767,-0.122083709175449,
-1.13230309069977));
#75066=CARTESIAN_POINT('Ctrl Pts',(-0.0747030733248228,-0.339305952341285,
-1.11646661167477));
#75067=CARTESIAN_POINT('Ctrl Pts',(0.243928609733561,-0.247402327822217,
-1.10063013264977));
#75068=CARTESIAN_POINT('Ctrl Pts',(0.340328284727392,0.0698980477045754,
-1.08479365362476));
#75069=CARTESIAN_POINT('Ctrl Pts',(0.126670692561194,0.323517563826862,
-1.06895717459976));
#75070=CARTESIAN_POINT('Ctrl Pts',(-0.202390674510908,0.282395278518285,
-1.05312069557475));
#75071=CARTESIAN_POINT('Ctrl Pts',(-0.347063313835056,-0.0160042072040358,
-1.03728421654975));
#75072=CARTESIAN_POINT('Ctrl Pts',(-0.175542714312195,-0.299823004304718,
-1.02144773752474));
#75073=CARTESIAN_POINT('Ctrl Pts',(0.15590668546625,-0.310487010815796,
-1.00561125849974));
#75074=CARTESIAN_POINT('Ctrl Pts',(0.345316757345856,-0.0382807465254171,
-0.989774779474735));
#75075=CARTESIAN_POINT('Ctrl Pts',(0.220124796740909,0.268801324993337,
-0.973938300449731));
#75076=CARTESIAN_POINT('Ctrl Pts',(-0.105612625333141,0.330991014724935,
-0.958101821424727));
#75077=CARTESIAN_POINT('Ctrl Pts',(-0.335131297870638,0.0916301895989631,
-0.942265342399722));
#75078=CARTESIAN_POINT('Ctrl Pts',(-0.259327436194449,-0.23121063836946,
-0.926428863374718));
#75079=CARTESIAN_POINT('Ctrl Pts',(0.0527375879369066,-0.34340621030639,
-0.910592384349713));
#75080=CARTESIAN_POINT('Ctrl Pts',(0.316755849203911,-0.142740360282258,
-0.894755905324709));
#75081=CARTESIAN_POINT('Ctrl Pts',(0.292192592658523,0.187969591301068,
-0.878919426299706));
#75082=CARTESIAN_POINT('Ctrl Pts',(0.00142625858558128,0.347429193138468,
-0.863082947274699));
#75083=CARTESIAN_POINT('Ctrl Pts',(-0.290639473331014,0.190362220517284,
-0.847246468249698));
#75084=CARTESIAN_POINT('Ctrl Pts',(-0.31791710248375,-0.140134915016696,
-0.83140998922469));
#75085=CARTESIAN_POINT('Ctrl Pts',(-0.0555552499856906,-0.342961648960095,
-0.815573510199689));
#75086=CARTESIAN_POINT('Ctrl Pts',(0.25742040618359,-0.233331980102762,
-0.799737031174682));
#75087=CARTESIAN_POINT('Ctrl Pts',(0.335872306220048,0.08887560054833,-0.78390055214968));
#75088=CARTESIAN_POINT('Ctrl Pts',(0.108326573809524,0.330112756289559,
-0.768064073124673));
#75089=CARTESIAN_POINT('Ctrl Pts',(-0.217910460333662,0.270599537574571,
-0.752227594099671));
#75090=CARTESIAN_POINT('Ctrl Pts',(-0.34561941189106,-0.0354443307522923,
-0.736391115074665));
#75091=CARTESIAN_POINT('Ctrl Pts',(-0.158450596488134,-0.309196518303415,
-0.720554636049662));
#75092=CARTESIAN_POINT('Ctrl Pts',(0.173075185795579,-0.301254142743674,
-0.704718157024656));
#75093=CARTESIAN_POINT('Ctrl Pts',(0.346920218258641,-0.0188531329432885,
-0.688881677999654));
#75094=CARTESIAN_POINT('Ctrl Pts',(0.204702379597146,0.280724089179512,
-0.673045198974647));
#75095=CARTESIAN_POINT('Ctrl Pts',(-0.124010273769175,0.324546653746567,
-0.657208719949646));
#75096=CARTESIAN_POINT('Ctrl Pts',(-0.33974293602063,0.0726898609331555,
-0.641372240924638));
#75097=CARTESIAN_POINT('Ctrl Pts',(-0.24595161508668,-0.24539128243411,
-0.625535761899637));
#75098=CARTESIAN_POINT('Ctrl Pts',(0.0719147799730091,-0.339907844687102,
-0.609699282874629));
#75099=CARTESIAN_POINT('Ctrl Pts',(0.324262964682606,-0.124750183140707,
-0.593862803849628));
#75100=CARTESIAN_POINT('Ctrl Pts',(0.281190247919927,0.204061566526267,
-0.578026324824621));
#75101=CARTESIAN_POINT('Ctrl Pts',(-0.0180618219399402,0.346962316464754,
-0.562189845799619));
#75102=CARTESIAN_POINT('Ctrl Pts',(-0.30085860611827,0.173761841561747,
-0.546353366774613));
#75103=CARTESIAN_POINT('Ctrl Pts',(-0.309557111074236,-0.157744963285489,
-0.53051688774961));
#75104=CARTESIAN_POINT('Ctrl Pts',(-0.036232533620933,-0.34553767083433,
-0.514680408724605));
#75105=CARTESIAN_POINT('Ctrl Pts',(0.270101819570867,-0.218527081897646,
-0.498843929699601));
#75106=CARTESIAN_POINT('Ctrl Pts',(0.330358970871335,0.107573364846364,
-0.483007450674596));
#75107=CARTESIAN_POINT('Ctrl Pts',(0.0896414330596858,0.335668723499518,
-0.467170971649592));
#75108=CARTESIAN_POINT('Ctrl Pts',(-0.232744244024522,0.257951924456976,
-0.451334492624587));
#75109=CARTESIAN_POINT('Ctrl Pts',(-0.343087468331121,-0.0547728723007094,
-0.435498013599583));
#75110=CARTESIAN_POINT('Ctrl Pts',(-0.1408596616263,-0.317596653276093,
-0.419661534574579));
#75111=CARTESIAN_POINT('Ctrl Pts',(0.189698829520533,-0.291072899006414,
-0.403825055549575));
#75112=CARTESIAN_POINT('Ctrl Pts',(0.347431542557318,0.00063383207379672,
-0.38798857652457));
#75113=CARTESIAN_POINT('Ctrl Pts',(0.188635540443955,0.291763108090254,
-0.372152097499566));
#75114=CARTESIAN_POINT('Ctrl Pts',(-0.142017526228985,0.317080590273025,
-0.356315618474562));
#75115=CARTESIAN_POINT('Ctrl Pts',(-0.343285032715151,0.053520697619757,
-0.340479139449557));
#75116=CARTESIAN_POINT('Ctrl Pts',(-0.231801514797257,-0.258799411659507,
-0.324642660424553));
#75117=CARTESIAN_POINT('Ctrl Pts',(0.0908655759127951,-0.33533941905422,
-0.308806181399548));
#75118=CARTESIAN_POINT('Ctrl Pts',(0.33074927397007,-0.106367278922094,
-0.292969702374544));
#75119=CARTESIAN_POINT('Ctrl Pts',(0.269302684023171,0.219511133294136,
-0.27713322334954));
#75120=CARTESIAN_POINT('Ctrl Pts',(-0.0374930298689546,0.34540317806302,
-0.261296744324536));
#75121=CARTESIAN_POINT('Ctrl Pts',(-0.310130631938373,0.156614430089098,
-0.245460265299531));
#75122=CARTESIAN_POINT('Ctrl Pts',(-0.300222560526634,-0.174858388636364,
-0.229623786274527));
#75123=CARTESIAN_POINT('Ctrl Pts',(-0.0167958397470517,-0.347025960541386,
-0.213787307249522));
#75124=CARTESIAN_POINT('Ctrl Pts',(0.28193309155819,-0.203034140829778,
-0.197950828224518));
#75125=CARTESIAN_POINT('Ctrl Pts',(0.323805322132367,0.125932288197448,
-0.182114349199514));
#75126=CARTESIAN_POINT('Ctrl Pts',(0.0706746906597415,0.340168337845624,
-0.166277870174509));
#75127=CARTESIAN_POINT('Ctrl Pts',(-0.246846469125181,0.24449156162207,
-0.150441391149505));
#75128=CARTESIAN_POINT('Ctrl Pts',(-0.339473273698357,-0.0739276596409582,
-0.134604912124501));
#75129=CARTESIAN_POINT('Ctrl Pts',(-0.122829451287563,-0.324999493662042,
-0.118768433099497));
#75130=CARTESIAN_POINT('Ctrl Pts',(0.205733235448034,-0.279970501686742,
-0.102931954074492));
#75131=CARTESIAN_POINT('Ctrl Pts',(0.346833934645568,0.0201095787129644,
-0.0870954750494877));
#75132=CARTESIAN_POINT('Ctrl Pts',(0.172003865311559,0.301901245285926,
-0.0712589960244833));
#75133=CARTESIAN_POINT('Ctrl Pts',(-0.159633134290119,0.308582670869633,
-0.055422516999479));
#75134=CARTESIAN_POINT('Ctrl Pts',(-0.345640152810216,0.0342474696623144,
-0.0395860379744743));
#75135=CARTESIAN_POINT('Ctrl Pts',(-0.217128269244485,-0.271517151993076,
-0.0237495589494704));
#75136=CARTESIAN_POINT('Ctrl Pts',(0.109956635018834,-0.329466300756443,
-0.00791307992446606));
#75137=CARTESIAN_POINT('Ctrl Pts',(0.260066783621101,-0.168643781123282,
0.00264457275887023));
#75138=CARTESIAN_POINT('Ctrl Pts',(0.284684032187583,-0.0742202251237438,
0.0079233991005383));
#75139=CARTESIAN_POINT('Ctrl Pts',(-0.294543724507234,0.000174101626290112,
-0.0380176117089602));
#75140=CARTESIAN_POINT('Ctrl Pts',(-0.294041378396576,-0.0797773756946391,
-0.0336784078059734));
#75141=CARTESIAN_POINT('Ctrl Pts',(-0.259412827341036,-0.160153784999754,
-0.0293392039029866));
#75142=CARTESIAN_POINT('Ctrl Pts',(-0.201391095966871,-0.215105632705578,
-0.0249999999999998));
#75143=CARTESIAN_POINT('',(-0.137702479013099,-0.193106208855767,-1.9558));
#75144=CARTESIAN_POINT('Ctrl Pts',(-0.137997372405516,-0.193358576631783,
-1.9558));
#75145=CARTESIAN_POINT('Ctrl Pts',(-0.143505274448249,-0.19036485287795,
-1.9558));
#75146=CARTESIAN_POINT('Ctrl Pts',(-0.14887540128292,-0.187145389562404,
-1.9558));
#75147=CARTESIAN_POINT('Ctrl Pts',(-0.154092081256687,-0.183703367937111,
-1.9558));
#75148=CARTESIAN_POINT('Ctrl Pts',(-0.16443175217884,-0.176881141714411,
-1.9558));
#75149=CARTESIAN_POINT('Ctrl Pts',(-0.174169408604617,-0.169186267076578,
-1.9558));
#75150=CARTESIAN_POINT('Ctrl Pts',(-0.183273675663744,-0.160739807585122,
-1.9558));
#75151=CARTESIAN_POINT('Ctrl Pts',(-0.187814117952941,-0.156527424356474,
-1.9558));
#75152=CARTESIAN_POINT('Ctrl Pts',(-0.192198049343805,-0.152125795074728,
-1.9558));
#75153=CARTESIAN_POINT('Ctrl Pts',(-0.196405468670295,-0.147565936149503,
-1.9558));
#75154=CARTESIAN_POINT('Ctrl Pts',(-0.204392135759571,-0.138910256174714,
-1.9558));
#75155=CARTESIAN_POINT('Ctrl Pts',(-0.211756830622369,-0.129673890671042,
-1.9558));
#75156=CARTESIAN_POINT('Ctrl Pts',(-0.218472220131354,-0.119953568208016,
-1.9558));
#75157=CARTESIAN_POINT('Ctrl Pts',(-0.221655180907846,-0.115346329105464,
-1.9558));
#75158=CARTESIAN_POINT('Ctrl Pts',(-0.224692139350014,-0.110630122164558,
-1.9558));
#75159=CARTESIAN_POINT('Ctrl Pts',(-0.227579351596024,-0.105814103687251,
-1.9558));
#75160=CARTESIAN_POINT('Ctrl Pts',(-0.230045055361972,-0.101701183027268,
-1.9558));
#75161=CARTESIAN_POINT('Ctrl Pts',(-0.232399169828432,-0.0975190606622559,
-1.9558));
#75162=CARTESIAN_POINT('Ctrl Pts',(-0.234635497318627,-0.0932823518783036,
-1.9558));
#75163=CARTESIAN_POINT('Ctrl Pts',(-0.24211369915942,-0.0791149441234151,
-1.9558));
#75164=CARTESIAN_POINT('Ctrl Pts',(-0.248293672678524,-0.0643135493120521,
-1.9558));
#75165=CARTESIAN_POINT('Ctrl Pts',(-0.253104718557175,-0.0490960513030699,
-1.9558));
#75166=CARTESIAN_POINT('Ctrl Pts',(-0.256357398355311,-0.0388077169989578,
-1.9558));
#75167=CARTESIAN_POINT('Ctrl Pts',(-0.258983760288555,-0.0283281491712129,
-1.9558));
#75168=CARTESIAN_POINT('Ctrl Pts',(-0.260951076224304,-0.0177169355128009,
-1.9558));
#75169=CARTESIAN_POINT('Ctrl Pts',(-0.261969717926436,-0.0122226351077254,
-1.9558));
#75170=CARTESIAN_POINT('Ctrl Pts',(-0.262811586922912,-0.00668935134157141,
-1.9558));
#75171=CARTESIAN_POINT('Ctrl Pts',(-0.263468876989419,-0.00115163278850291,
-1.9558));
#75172=CARTESIAN_POINT('Ctrl Pts',(-0.264804897455981,0.0101044407503528,
-1.9558));
#75173=CARTESIAN_POINT('Ctrl Pts',(-0.265383724412674,0.0213987430783344,
-1.9558));
#75174=CARTESIAN_POINT('Ctrl Pts',(-0.265178397174566,0.0326600289712171,
-1.9558));
#75175=CARTESIAN_POINT('Ctrl Pts',(-0.26496718827068,0.0442438980754525,
-1.9558));
#75176=CARTESIAN_POINT('Ctrl Pts',(-0.263926601173681,0.055793119684933,
-1.9558));
#75177=CARTESIAN_POINT('Ctrl Pts',(-0.262109315712585,0.0672496706236925,
-1.9558));
#75178=CARTESIAN_POINT('Ctrl Pts',(-0.260957978128992,0.0745079456479108,
-1.9558));
#75179=CARTESIAN_POINT('Ctrl Pts',(-0.259494575539872,0.081729090187899,
-1.9558));
#75180=CARTESIAN_POINT('Ctrl Pts',(-0.257729496911758,0.0888984323365508,
-1.9558));
#75181=CARTESIAN_POINT('Ctrl Pts',(-0.256693970271012,0.0931045026346703,
-1.9558));
#75182=CARTESIAN_POINT('Ctrl Pts',(-0.255554797525397,0.0972910160978816,
-1.9558));
#75183=CARTESIAN_POINT('Ctrl Pts',(-0.254317934884101,0.101443693338831,
-1.9558));
#75184=CARTESIAN_POINT('Ctrl Pts',(-0.249598061917379,0.117290326905624,
-1.9558));
#75185=CARTESIAN_POINT('Ctrl Pts',(-0.243449028228328,0.132689526577699,
-1.9558));
#75186=CARTESIAN_POINT('Ctrl Pts',(-0.236017898320946,0.147481637055776,
-1.9558));
#75187=CARTESIAN_POINT('Ctrl Pts',(-0.229204595498085,0.161043925608455,
-1.9558));
#75188=CARTESIAN_POINT('Ctrl Pts',(-0.221312550750061,0.174096807174637,
-1.9558));
#75189=CARTESIAN_POINT('Ctrl Pts',(-0.212419504558069,0.186511230090778,
-1.9558));
#75190=CARTESIAN_POINT('Ctrl Pts',(-0.209826346911981,0.19013119956038,
-1.9558));
#75191=CARTESIAN_POINT('Ctrl Pts',(-0.207149372890048,0.193694426785744,
-1.9558));
#75192=CARTESIAN_POINT('Ctrl Pts',(-0.204397403906373,0.197189496801417,
-1.9558));
#75193=CARTESIAN_POINT('Ctrl Pts',(-0.193595728644106,0.210907896809613,
-1.9558));
#75194=CARTESIAN_POINT('Ctrl Pts',(-0.181615745101179,0.223615451460463,
-1.9558));
#75195=CARTESIAN_POINT('Ctrl Pts',(-0.168591987669066,0.235133409074003,
-1.9558));
#75196=CARTESIAN_POINT('Ctrl Pts',(-0.156268150773333,0.246032370586542,
-1.9558));
#75197=CARTESIAN_POINT('Ctrl Pts',(-0.143008760997121,0.255867267553694,
-1.9558));
#75198=CARTESIAN_POINT('Ctrl Pts',(-0.128892185405323,0.264462557919717,
-1.9558));
#75199=CARTESIAN_POINT('Ctrl Pts',(-0.137997372405514,-0.193358576631784,
-1.9558));
#75200=CARTESIAN_POINT('Ctrl Pts',(-0.0790002241827612,-0.234954131459917,
-1.95093798734184));
#75201=CARTESIAN_POINT('Ctrl Pts',(0.0869338825813326,-0.262714517298233,
-1.94079714834202));
#75202=CARTESIAN_POINT('Ctrl Pts',(0.269259772704402,-0.077117310153115,
-1.92537748300052));
#75203=CARTESIAN_POINT('Ctrl Pts',(0.211266823136741,0.183928328504729,
-1.90954100397552));
#75204=CARTESIAN_POINT('Ctrl Pts',(-0.0392343044552656,0.277314777777813,
-1.89370452495051));
#75205=CARTESIAN_POINT('Ctrl Pts',(-0.213703631858497,0.147957606827352,
-1.88083786056184));
#75206=CARTESIAN_POINT('Ctrl Pts',(-0.236917463552764,0.0346120890587808,
-1.87325002251484));
#75207=CARTESIAN_POINT('Ctrl Pts',(-0.236814675525433,8.00967394152356E-5,
-1.8709410108095));
#75208=CARTESIAN_POINT('Origin',(-3.51939854619125E-17,0.,-1.9558));
#75209=CARTESIAN_POINT('',(-0.2942,-3.60291088309151E-17,-1.9558));
#75210=CARTESIAN_POINT('Origin',(0.,0.,-1.9558));
#75211=CARTESIAN_POINT('Origin',(0.,0.,-1.9558));
#75212=CARTESIAN_POINT('',(0.137702479013102,-0.193106208855765,-1.9558));
#75213=CARTESIAN_POINT('Ctrl Pts',(0.129201276660418,0.26483169369169,-1.9558));
#75214=CARTESIAN_POINT('Ctrl Pts',(0.135785829563373,0.260865815094269,
-1.9558));
#75215=CARTESIAN_POINT('Ctrl Pts',(0.142193064090495,0.256631694188274,
-1.9558));
#75216=CARTESIAN_POINT('Ctrl Pts',(0.148404092834589,0.25212844043442,-1.9558));
#75217=CARTESIAN_POINT('Ctrl Pts',(0.158383745515504,0.244892777833401,
-1.9558));
#75218=CARTESIAN_POINT('Ctrl Pts',(0.167857441197493,0.23696258771659,-1.9558));
#75219=CARTESIAN_POINT('Ctrl Pts',(0.176788556648393,0.228413138989074,
-1.9558));
#75220=CARTESIAN_POINT('Ctrl Pts',(0.180831129606409,0.22454332335162,-1.9558));
#75221=CARTESIAN_POINT('Ctrl Pts',(0.184762389846773,0.220546531359166,
-1.9558));
#75222=CARTESIAN_POINT('Ctrl Pts',(0.188578162618967,0.216429360238014,
-1.9558));
#75223=CARTESIAN_POINT('Ctrl Pts',(0.192285937148445,0.212428717870695,
-1.9558));
#75224=CARTESIAN_POINT('Ctrl Pts',(0.195877805523516,0.208321814842972,
-1.9558));
#75225=CARTESIAN_POINT('Ctrl Pts',(0.199350673797985,0.204115840696008,
-1.9558));
#75226=CARTESIAN_POINT('Ctrl Pts',(0.205710856757708,0.19641305355167,-1.9558));
#75227=CARTESIAN_POINT('Ctrl Pts',(0.211672619239862,0.188377677017422,
-1.9558));
#75228=CARTESIAN_POINT('Ctrl Pts',(0.217215067993658,0.180049457174739,
-1.9558));
#75229=CARTESIAN_POINT('Ctrl Pts',(0.221322515103539,0.173877506103499,
-1.9558));
#75230=CARTESIAN_POINT('Ctrl Pts',(0.225199567589628,0.167544651916967,
-1.9558));
#75231=CARTESIAN_POINT('Ctrl Pts',(0.228835718112123,0.161066564540105,
-1.9558));
#75232=CARTESIAN_POINT('Ctrl Pts',(0.23166334902431,0.156028918269595,-1.9558));
#75233=CARTESIAN_POINT('Ctrl Pts',(0.234345811865076,0.15090159384628,-1.9558));
#75234=CARTESIAN_POINT('Ctrl Pts',(0.236868800988663,0.145711771031545,
-1.9558));
#75235=CARTESIAN_POINT('Ctrl Pts',(0.244189693097608,0.130652596762418,
-1.9558));
#75236=CARTESIAN_POINT('Ctrl Pts',(0.250192743403271,0.115032605157703,
-1.9558));
#75237=CARTESIAN_POINT('Ctrl Pts',(0.254770972596117,0.099038452029079,
-1.9558));
#75238=CARTESIAN_POINT('Ctrl Pts',(0.257882624658325,0.0881678211651359,
-1.9558));
#75239=CARTESIAN_POINT('Ctrl Pts',(0.26033512079411,0.0771239681159206,
-1.9558));
#75240=CARTESIAN_POINT('Ctrl Pts',(0.262080723507159,0.0659660971856748,
-1.9558));
#75241=CARTESIAN_POINT('Ctrl Pts',(0.262792052894065,0.0614192885512388,
-1.9558));
#75242=CARTESIAN_POINT('Ctrl Pts',(0.263386081399267,0.056851340822549,
-1.9558));
#75243=CARTESIAN_POINT('Ctrl Pts',(0.263858267251122,0.0522736216863439,
-1.9558));
#75244=CARTESIAN_POINT('Ctrl Pts',(0.265260862420264,0.0386758259859476,
-1.9558));
#75245=CARTESIAN_POINT('Ctrl Pts',(0.26558555294751,0.0250503556577028,
-1.9558));
#75246=CARTESIAN_POINT('Ctrl Pts',(0.264763093706556,0.011502649672878,
-1.9558));
#75247=CARTESIAN_POINT('Ctrl Pts',(0.263784864463184,-0.00461092959650045,
-1.9558));
#75248=CARTESIAN_POINT('Ctrl Pts',(0.261184230539979,-0.0206161268211077,
-1.9558));
#75249=CARTESIAN_POINT('Ctrl Pts',(0.257062644120522,-0.0363174874293233,
-1.9558));
#75250=CARTESIAN_POINT('Ctrl Pts',(0.255965870831883,-0.0404956924110467,
-1.9558));
#75251=CARTESIAN_POINT('Ctrl Pts',(0.254760293306619,-0.0446548960531295,
-1.9558));
#75252=CARTESIAN_POINT('Ctrl Pts',(0.253450272167277,-0.0487819884203261,
-1.9558));
#75253=CARTESIAN_POINT('Ctrl Pts',(0.248667272494634,-0.0638503570507704,
-1.9558));
#75254=CARTESIAN_POINT('Ctrl Pts',(0.242513938635288,-0.0784420159944107,
-1.9558));
#75255=CARTESIAN_POINT('Ctrl Pts',(0.235102432119141,-0.0923804165550677,
-1.9558));
#75256=CARTESIAN_POINT('Ctrl Pts',(0.229372055048817,-0.103157212176276,
-1.9558));
#75257=CARTESIAN_POINT('Ctrl Pts',(0.222888330661629,-0.113543323222854,
-1.9558));
#75258=CARTESIAN_POINT('Ctrl Pts',(0.215688032875387,-0.123441795139812,
-1.9558));
#75259=CARTESIAN_POINT('Ctrl Pts',(0.213136130361168,-0.126949974401518,
-1.9558));
#75260=CARTESIAN_POINT('Ctrl Pts',(0.210492869904086,-0.130398289364971,
-1.9558));
#75261=CARTESIAN_POINT('Ctrl Pts',(0.207763617706553,-0.133776946374647,
-1.9558));
#75262=CARTESIAN_POINT('Ctrl Pts',(0.198038798706408,-0.145815712126074,
-1.9558));
#75263=CARTESIAN_POINT('Ctrl Pts',(0.187280564674133,-0.15690666222773,
-1.9558));
#75264=CARTESIAN_POINT('Ctrl Pts',(0.175578277424442,-0.166865148238431,
-1.9558));
#75265=CARTESIAN_POINT('Ctrl Pts',(0.164592385110822,-0.176213991980338,
-1.9558));
#75266=CARTESIAN_POINT('Ctrl Pts',(0.152773356677846,-0.184565318985801,
-1.9558));
#75267=CARTESIAN_POINT('Ctrl Pts',(0.140176697278149,-0.191721582677799,
-1.9558));
#75268=CARTESIAN_POINT('Ctrl Pts',(0.139355263502201,-0.19218824582393,
-1.9558));
#75269=CARTESIAN_POINT('Ctrl Pts',(0.138530519371653,-0.192649808777216,
-1.9558));
#75270=CARTESIAN_POINT('Ctrl Pts',(0.137702479013106,-0.193106208855762,
-1.9558));
#75271=CARTESIAN_POINT('Origin',(0.,0.,-1.9558));
#75272=CARTESIAN_POINT('Origin',(0.,0.,-2.1406589891905));
#75273=CARTESIAN_POINT('Ctrl Pts',(0.137702479013101,-0.193106208855765,
-1.9558));
#75274=CARTESIAN_POINT('Ctrl Pts',(0.201751645331416,-0.147433265282304,
-1.95052117365833));
#75275=CARTESIAN_POINT('Ctrl Pts',(0.279756535851592,0.0118428723253114,
-1.939963520975));
#75276=CARTESIAN_POINT('Ctrl Pts',(0.142127113353835,0.241561378807579,
-1.92412704194999));
#75277=CARTESIAN_POINT('Ctrl Pts',(-0.125108372180837,0.250505423930283,
-1.90829056292499));
#75278=CARTESIAN_POINT('Ctrl Pts',(-0.23302431186425,0.0962800630305547,
-1.89713454533849));
#75279=CARTESIAN_POINT('Ctrl Pts',(-0.237502612682818,0.00905088842975674,
-1.89125735409366));
#75280=CARTESIAN_POINT('Ctrl Pts',(-0.2374378448428,0.00016285981187146,
-1.8906589891905));
#75281=CARTESIAN_POINT('Ctrl Pts',(0.170810875200393,-0.239535560853239,
-1.98872339910054));
#75282=CARTESIAN_POINT('Ctrl Pts',(0.250259656610106,-0.182881276045346,
-1.98344457275887));
#75283=CARTESIAN_POINT('Ctrl Pts',(0.34701959670091,0.014690304788047,-1.97288692007553));
#75284=CARTESIAN_POINT('Ctrl Pts',(0.176299343306418,0.299641014631343,
-1.95705044105053));
#75285=CARTESIAN_POINT('Ctrl Pts',(-0.155188713378732,0.310735514789881,
-1.94121396202552));
#75286=CARTESIAN_POINT('Ctrl Pts',(-0.34521286206057,0.0391672645750027,
-1.92537748300052));
#75287=CARTESIAN_POINT('Ctrl Pts',(-0.220770872998109,-0.268309353725055,
-1.90954100397551));
#75288=CARTESIAN_POINT('Ctrl Pts',(0.104826783471608,-0.331224318302498,
-1.89370452495051));
#75289=CARTESIAN_POINT('Ctrl Pts',(0.334910327509493,-0.0924376943938123,
-1.87786804592551));
#75290=CARTESIAN_POINT('Ctrl Pts',(0.259878572792024,0.23059679546836,-1.8620315669005));
#75291=CARTESIAN_POINT('Ctrl Pts',(-0.0519195584651473,0.34352842429146,
-1.8461950878755));
#75292=CARTESIAN_POINT('Ctrl Pts',(-0.316414572914817,0.143496108596634,
-1.8303586088505));
#75293=CARTESIAN_POINT('Ctrl Pts',(-0.292639839963886,-0.187273453877836,
-1.81452212982549));
#75294=CARTESIAN_POINT('Ctrl Pts',(-0.00225411854621495,-0.347424467276068,
-1.79868565080049));
#75295=CARTESIAN_POINT('Ctrl Pts',(0.290184992579116,-0.191054477515693,
-1.78284917177548));
#75296=CARTESIAN_POINT('Ctrl Pts',(0.318250179106363,0.13937702099163,-1.76701269275048));
#75297=CARTESIAN_POINT('Ctrl Pts',(0.0563723695500736,0.342828252951786,
-1.75117621372547));
#75298=CARTESIAN_POINT('Ctrl Pts',(-0.256863649886797,0.233944794646829,
-1.73533973470047));
#75299=CARTESIAN_POINT('Ctrl Pts',(-0.336083165442897,-0.0880749773678852,
-1.71950325567546));
#75300=CARTESIAN_POINT('Ctrl Pts',(-0.109112935366136,-0.329853685219295,
-1.70366677665046));
#75301=CARTESIAN_POINT('Ctrl Pts',(0.21726500907928,-0.271118072278702,
-1.68783029762546));
#75302=CARTESIAN_POINT('Ctrl Pts',(0.345702914058587,0.0346206167649245,
-1.67199381860045));
#75303=CARTESIAN_POINT('Ctrl Pts',(0.159186975823379,0.308818065380956,
-1.65615733957545));
#75304=CARTESIAN_POINT('Ctrl Pts',(-0.172356809558471,0.301665745477315,
-1.64032086055044));
#75305=CARTESIAN_POINT('Ctrl Pts',(-0.346874324648551,0.0196797972731843,
-1.62448438152544));
#75306=CARTESIAN_POINT('Ctrl Pts',(-0.20537077995855,-0.280235497640334,
-1.60864790250043));
#75307=CARTESIAN_POINT('Ctrl Pts',(0.123236527810909,-0.324841268555487,
-1.59281142347543));
#75308=CARTESIAN_POINT('Ctrl Pts',(0.339568768462871,-0.0734992719630991,
-1.57697494445043));
#75309=CARTESIAN_POINT('Ctrl Pts',(0.246535701861457,0.244804491769266,
-1.56113846542542));
#75310=CARTESIAN_POINT('Ctrl Pts',(-0.07110457313861,0.340078272139931,
-1.54530198640042));
#75311=CARTESIAN_POINT('Ctrl Pts',(-0.323964779549688,0.125522560147371,
-1.52946550737541));
#75312=CARTESIAN_POINT('Ctrl Pts',(-0.28167574708672,-0.203390916702184,
-1.51362902835041));
#75313=CARTESIAN_POINT('Ctrl Pts',(0.0172349541753397,-0.347004391688523,
-1.4977925493254));
#75314=CARTESIAN_POINT('Ctrl Pts',(0.300443690509177,-0.174478309048545,
-1.4819560703004));
#75315=CARTESIAN_POINT('Ctrl Pts',(0.309932157928084,0.157006843727486,
-1.46611959127539));
#75316=CARTESIAN_POINT('Ctrl Pts',(0.0370558551984614,0.345450365596992,
-1.45028311225039));
#75317=CARTESIAN_POINT('Ctrl Pts',(-0.269580313257183,0.219170130719346,
-1.43444663322538));
#75318=CARTESIAN_POINT('Ctrl Pts',(-0.330614399959186,-0.106785813828543,
-1.41861015420038));
#75319=CARTESIAN_POINT('Ctrl Pts',(-0.0904410879955278,-0.335454171382065,
-1.40277367517538));
#75320=CARTESIAN_POINT('Ctrl Pts',(0.232128891660156,-0.258505839686529,
-1.38693719615037));
#75321=CARTESIAN_POINT('Ctrl Pts',(0.34321703743098,0.0539551361087899,
-1.37110071712537));
#75322=CARTESIAN_POINT('Ctrl Pts',(0.141616107846662,0.317260097544246,
-1.35526423810036));
#75323=CARTESIAN_POINT('Ctrl Pts',(-0.18900466920625,0.291524143963502,
-1.33942775907536));
#75324=CARTESIAN_POINT('Ctrl Pts',(-0.34743208518864,0.000194105363083371,
-1.32359128005036));
#75325=CARTESIAN_POINT('Ctrl Pts',(-0.189330291900079,-0.291312773603304,
-1.30775480102535));
#75326=CARTESIAN_POINT('Ctrl Pts',(0.141261522146442,-0.317418137251619,
-1.29191832200035));
#75327=CARTESIAN_POINT('Ctrl Pts',(0.34315653525949,-0.0543386032588314,
-1.27608184297534));
#75328=CARTESIAN_POINT('Ctrl Pts',(0.2324175937311,0.258246304174259,-1.26024536395034));
#75329=CARTESIAN_POINT('Ctrl Pts',(-0.0900662047077227,0.335555018238388,
-1.24440888492533));
#75330=CARTESIAN_POINT('Ctrl Pts',(-0.330494874177406,0.107155166174472,
-1.22857240590033));
#75331=CARTESIAN_POINT('Ctrl Pts',(-0.269825039360483,-0.218868772623077,
-1.21273592687533));
#75332=CARTESIAN_POINT('Ctrl Pts',(0.0366698357773552,-0.345491555091409,
-1.19689944785032));
#75333=CARTESIAN_POINT('Ctrl Pts',(0.309756529525153,-0.15735305498131,
-1.18106296882532));
#75334=CARTESIAN_POINT('Ctrl Pts',(0.3006384599913,0.17414249300351,-1.16522648980031));
#75335=CARTESIAN_POINT('Ctrl Pts',(0.0176226761291528,0.346984917224748,
-1.14939001077531));
#75336=CARTESIAN_POINT('Ctrl Pts',(-0.281448308096457,0.203705526103394,
-1.1335535317503));
#75337=CARTESIAN_POINT('Ctrl Pts',(-0.324104832603851,-0.125160492881134,
-1.1177170527253));
#75338=CARTESIAN_POINT('Ctrl Pts',(-0.0714845224191077,-0.339998609629407,
-1.10188057370029));
#75339=CARTESIAN_POINT('Ctrl Pts',(0.246262010475165,-0.245079810861989,
-1.08604409467529));
#75340=CARTESIAN_POINT('Ctrl Pts',(0.339650682445754,0.0731198017608916,
-1.07020761565029));
#75341=CARTESIAN_POINT('Ctrl Pts',(0.123599419171098,0.324703364743862,
-1.05437113662528));
#75342=CARTESIAN_POINT('Ctrl Pts',(-0.205057524708256,0.280464798247376,
-1.03853465760028));
#75343=CARTESIAN_POINT('Ctrl Pts',(-0.346896097694429,-0.0192921978995482,
-1.02269817857527));
#75344=CARTESIAN_POINT('Ctrl Pts',(-0.172693774679941,-0.301472970068979,
-1.00686169955027));
#75345=CARTESIAN_POINT('Ctrl Pts',(0.158841812232089,-0.308995744602162,
-0.991025220525266));
#75346=CARTESIAN_POINT('Ctrl Pts',(0.345664013799501,-0.0350068716031159,
-0.975188741500259));
#75347=CARTESIAN_POINT('Ctrl Pts',(0.217567813682816,0.270875133492718,
-0.959352262475257));
#75348=CARTESIAN_POINT('Ctrl Pts',(-0.108744299596982,0.329975406357171,
-0.943515783450251));
#75349=CARTESIAN_POINT('Ctrl Pts',(-0.335984540612977,0.0884504378988902,
-0.927679304425247));
#75350=CARTESIAN_POINT('Ctrl Pts',(-0.257124897648059,-0.233657609559144,
-0.911842825400244));
#75351=CARTESIAN_POINT('Ctrl Pts',(0.0559892773708684,-0.342891079374932,
-0.896006346375238));
#75352=CARTESIAN_POINT('Ctrl Pts',(0.318094226560149,-0.13973243905593,
-0.880169867350236));
#75353=CARTESIAN_POINT('Ctrl Pts',(0.290398324592949,0.190729925730144,
-0.864333388325229));
#75354=CARTESIAN_POINT('Ctrl Pts',(-0.00186598074179355,0.347427128490695,
-0.848496909300226));
#75355=CARTESIAN_POINT('Ctrl Pts',(-0.292430277833504,0.187599637797193,
-0.83266043027522));
#75356=CARTESIAN_POINT('Ctrl Pts',(-0.316574953492537,-0.143141155216159,
-0.816823951250218));
#75357=CARTESIAN_POINT('Ctrl Pts',(-0.0523029170060187,-0.343472701052179,
-0.800987472225212));
#75358=CARTESIAN_POINT('Ctrl Pts',(0.259619873881868,-0.230882248301989,
-0.785150993200208));
#75359=CARTESIAN_POINT('Ctrl Pts',(0.335015075942623,0.0920542795668767,
-0.769314514175204));
#75360=CARTESIAN_POINT('Ctrl Pts',(0.105193628181329,0.331124435953414,
-0.753478035150199));
#75361=CARTESIAN_POINT('Ctrl Pts',(-0.220464840304462,0.268522523608257,
-0.737641556125195));
#75362=CARTESIAN_POINT('Ctrl Pts',(-0.345268049450204,-0.0387177675527577,
-0.721805077100192));
#75363=CARTESIAN_POINT('Ctrl Pts',(-0.155513601609092,-0.310684101958866,
-0.705968598075186));
#75364=CARTESIAN_POINT('Ctrl Pts',(0.175922053716002,-0.299600604992318,
-0.690132119050183));
#75365=CARTESIAN_POINT('Ctrl Pts',(0.347083310302664,-0.0155649351030341,
-0.674295640025177));
#75366=CARTESIAN_POINT('Ctrl Pts',(0.20203311019098,0.282651223032876,-0.658459161000174));
#75367=CARTESIAN_POINT('Ctrl Pts',(-0.127080057451709,0.323357001615068,
-0.642622681975168));
#75368=CARTESIAN_POINT('Ctrl Pts',(-0.34041649688156,0.0694672595277645,
-0.626786202950166));
#75369=CARTESIAN_POINT('Ctrl Pts',(-0.243615303161651,-0.247710870897704,
-0.61094972392516));
#75370=CARTESIAN_POINT('Ctrl Pts',(0.0751324595811616,-0.339211151073608,
-0.595113244900157));
#75371=CARTESIAN_POINT('Ctrl Pts',(0.325430533778499,-0.121671932589311,
-0.579276765875152));
#75372=CARTESIAN_POINT('Ctrl Pts',(0.27924398861926,0.206716923147551,-0.563440286850148));
#75373=CARTESIAN_POINT('Ctrl Pts',(-0.0213487633344698,0.346775607272649,
-0.547603807825143));
#75374=CARTESIAN_POINT('Ctrl Pts',(-0.302491650219096,0.17090316861586,
-0.531767328800139));
#75375=CARTESIAN_POINT('Ctrl Pts',(-0.308048467376976,-0.160671196059666,
-0.515930849775135));
#75376=CARTESIAN_POINT('Ctrl Pts',(-0.0329566572079708,-0.345865508889646,
-0.50009437075013));
#75377=CARTESIAN_POINT('Ctrl Pts',(0.272160430095799,-0.215957847240377,
-0.484257891725126));
#75378=CARTESIAN_POINT('Ctrl Pts',(0.329324811245078,0.110698962060618,
-0.468421412700121));
#75379=CARTESIAN_POINT('Ctrl Pts',(0.0864566779796564,0.336503097036941,
-0.452584933675117));
#75380=CARTESIAN_POINT('Ctrl Pts',(-0.235178112319307,0.255734915450402,
-0.436748454650113));
#75381=CARTESIAN_POINT('Ctrl Pts',(-0.342553065762632,-0.0580214501736126,
-0.420911975625108));
#75382=CARTESIAN_POINT('Ctrl Pts',(-0.13784385733172,-0.318917171683215,
-0.405075496600104));
#75383=CARTESIAN_POINT('Ctrl Pts',(0.192448476206574,-0.289262295377172,
-0.3892390175751));
#75384=CARTESIAN_POINT('Ctrl Pts',(0.347409957121141,0.00392600161055561,
-0.373402538550095));
#75385=CARTESIAN_POINT('Ctrl Pts',(0.185862387110661,0.293537499878561,
-0.357566059525091));
#75386=CARTESIAN_POINT('Ctrl Pts',(-0.145015754062733,0.315720640705355,
-0.341729580500086));
#75387=CARTESIAN_POINT('Ctrl Pts',(-0.343776793759324,0.0502653892743109,
-0.325893101475083));
#75388=CARTESIAN_POINT('Ctrl Pts',(-0.229338779650105,-0.260984310765158,
-0.310056622450078));
#75389=CARTESIAN_POINT('Ctrl Pts',(0.0940391070372089,-0.334463364331755,
-0.294220143425074));
#75390=CARTESIAN_POINT('Ctrl Pts',(0.331742376587111,-0.10322837377315,
-0.27838366440007));
#75391=CARTESIAN_POINT('Ctrl Pts',(0.267210527261116,0.22205312245384,-0.262547185375064));
#75392=CARTESIAN_POINT('Ctrl Pts',(-0.0407642622649248,0.34503247007163,
-0.246710706350061));
#75393=CARTESIAN_POINT('Ctrl Pts',(-0.31160089590667,0.153668555557396,
-0.230874227325056));
#75394=CARTESIAN_POINT('Ctrl Pts',(-0.298551939882619,-0.177695190438021,
-0.215037748300052));
#75395=CARTESIAN_POINT('Ctrl Pts',(-0.0135071750300152,-0.347169956482602,
-0.199201269275047));
#75396=CARTESIAN_POINT('Ctrl Pts',(0.283845209205327,-0.200352719837858,
-0.183364790250043));
#75397=CARTESIAN_POINT('Ctrl Pts',(0.322595874731448,0.128993489966123,
-0.167528311225039));
#75398=CARTESIAN_POINT('Ctrl Pts',(0.0674512351160957,0.340825594047761,
-0.151691832200035));
#75399=CARTESIAN_POINT('Ctrl Pts',(-0.249158052908653,0.242136158985246,
-0.13585535317503));
#75400=CARTESIAN_POINT('Ctrl Pts',(-0.338746263568963,-0.0771308789397851,
-0.120018874150026));
#75401=CARTESIAN_POINT('Ctrl Pts',(-0.119765825135592,-0.326168414764973,
-0.104182395125021));
#75402=CARTESIAN_POINT('Ctrl Pts',(0.208418103123617,-0.277971021936984,
-0.0883459161000174));
#75403=CARTESIAN_POINT('Ctrl Pts',(0.346548858735595,0.0233234950411567,
-0.0725094370750124));
#75404=CARTESIAN_POINT('Ctrl Pts',(0.169289569309017,0.303656447029769,
-0.0566729580500089));
#75405=CARTESIAN_POINT('Ctrl Pts',(-0.162873930760557,0.306774327850024,
-0.0408364790250043));
#75406=CARTESIAN_POINT('Ctrl Pts',(-0.284353669323579,0.123363072257457,
-0.030278826341668));
#75407=CARTESIAN_POINT('Ctrl Pts',(-0.293033728012268,0.0261701021632011,
-0.0249999999999999));
#75408=CARTESIAN_POINT('Ctrl Pts',(0.159774743137963,-0.224059110187414,
-1.97774893273369));
#75409=CARTESIAN_POINT('Ctrl Pts',(0.234090319517209,-0.171065272457665,
-1.97247010639202));
#75410=CARTESIAN_POINT('Ctrl Pts',(0.324598576417804,0.0137411606338018,
-1.96191245370869));
#75411=CARTESIAN_POINT('Ctrl Pts',(0.16490859998889,0.280281136023422,-1.94607597468369));
#75412=CARTESIAN_POINT('Ctrl Pts',(-0.145161932979434,0.290658817836682,
-1.93023949565868));
#75413=CARTESIAN_POINT('Ctrl Pts',(-0.322908575340647,0.0366366581141018,
-1.91440301663368));
#75414=CARTESIAN_POINT('Ctrl Pts',(-0.206506813364393,-0.250973821325134,
-1.89856653760867));
#75415=CARTESIAN_POINT('Ctrl Pts',(0.0980538995746365,-0.309823834786522,
-1.88273005858367));
#75416=CARTESIAN_POINT('Ctrl Pts',(0.313271690044925,-0.0864652725460799,
-1.86689357955866));
#75417=CARTESIAN_POINT('Ctrl Pts',(0.243087755192357,0.215697880601396,
-1.85105710053365));
#75418=CARTESIAN_POINT('Ctrl Pts',(-0.0485650232040169,0.321332969504216,
-1.83522062150865));
#75419=CARTESIAN_POINT('Ctrl Pts',(-0.295970950639192,0.134224790227357,
-1.81938414248365));
#75420=CARTESIAN_POINT('Ctrl Pts',(-0.27373230894877,-0.17517367061545,
-1.80354766345864));
#75421=CARTESIAN_POINT('Ctrl Pts',(-0.00210847940039634,-0.324977288206934,
-1.78771118443364));
#75422=CARTESIAN_POINT('Ctrl Pts',(0.271436069848747,-0.178710401399294,
-1.77187470540864));
#75423=CARTESIAN_POINT('Ctrl Pts',(0.29768795786963,0.130371837871251,-1.75603822638363));
#75424=CARTESIAN_POINT('Ctrl Pts',(0.0527301370850901,0.320678036404567,
-1.74020174735863));
#75425=CARTESIAN_POINT('Ctrl Pts',(-0.240267627187054,0.218829564741168,
-1.72436526833362));
#75426=CARTESIAN_POINT('Ctrl Pts',(-0.314368750635077,-0.0823844317250094,
-1.70852878930862));
#75427=CARTESIAN_POINT('Ctrl Pts',(-0.102063122156012,-0.308541758639157,
-1.69269231028361));
#75428=CARTESIAN_POINT('Ctrl Pts',(0.203227464163412,-0.253601067892011,
-1.67685583125861));
#75429=CARTESIAN_POINT('Ctrl Pts',(0.323366964960251,0.0323837703214412,
-1.6610193522336));
#75430=CARTESIAN_POINT('Ctrl Pts',(0.148901866718088,0.288865255298984,
-1.6451828732086));
#75431=CARTESIAN_POINT('Ctrl Pts',(-0.16122079430233,0.282175048518507,
-1.6293463941836));
#75432=CARTESIAN_POINT('Ctrl Pts',(-0.324462690427972,0.0184082807996913,
-1.61350991515859));
#75433=CARTESIAN_POINT('Ctrl Pts',(-0.192101724070109,-0.262129414190369,
-1.59767343613359));
#75434=CARTESIAN_POINT('Ctrl Pts',(0.115274185868449,-0.303853195431335,
-1.58183695710858));
#75435=CARTESIAN_POINT('Ctrl Pts',(0.317629147998793,-0.068750466180528,
-1.56600047808358));
#75436=CARTESIAN_POINT('Ctrl Pts',(0.230606970387799,0.228987614199426,
-1.55016399905857));
#75437=CARTESIAN_POINT('Ctrl Pts',(-0.0665104894277243,0.318105732519741,
-1.53432752003357));
#75438=CARTESIAN_POINT('Ctrl Pts',(-0.303033336592719,0.117412517101364,
-1.51849104100857));
#75439=CARTESIAN_POINT('Ctrl Pts',(-0.263476608770811,-0.190249780258789,
-1.50265456198356));
#75440=CARTESIAN_POINT('Ctrl Pts',(0.0161213996071919,-0.324584353804954,
-1.48681808295856));
#75441=CARTESIAN_POINT('Ctrl Pts',(0.281031950818167,-0.163205223195956,
-1.47098160393355));
#75442=CARTESIAN_POINT('Ctrl Pts',(0.289907366056511,0.146862593485521,
-1.45514512490855));
#75443=CARTESIAN_POINT('Ctrl Pts',(0.034661667409323,0.323130733715994,
-1.43930864588355));
#75444=CARTESIAN_POINT('Ctrl Pts',(-0.252162663853728,0.205009495432385,
-1.42347216685854));
#75445=CARTESIAN_POINT('Ctrl Pts',(-0.309253323415256,-0.0998863565052127,
-1.40763568783354));
#75446=CARTESIAN_POINT('Ctrl Pts',(-0.0845976673712967,-0.313780396033026,
-1.39179920880853));
#75447=CARTESIAN_POINT('Ctrl Pts',(0.21713098768676,-0.241803714705649,
-1.37596272978353));
#75448=CARTESIAN_POINT('Ctrl Pts',(0.321041701424293,0.0504690816825467,
-1.36012625075852));
#75449=CARTESIAN_POINT('Ctrl Pts',(0.132466256781675,0.296761845717303,
-1.34428977173352));
#75450=CARTESIAN_POINT('Ctrl Pts',(-0.176793031701735,0.272688698337488,
-1.32845329270851));
#75451=CARTESIAN_POINT('Ctrl Pts',(-0.324984413924328,0.000181564168509011,
-1.31261681368351));
#75452=CARTESIAN_POINT('Ctrl Pts',(-0.177097615834361,-0.272490984667515,
-1.29678033465851));
#75453=CARTESIAN_POINT('Ctrl Pts',(0.132134580949525,-0.296909674440862,
-1.2809438556335));
#75454=CARTESIAN_POINT('Ctrl Pts',(0.320985108312774,-0.0508277729270431,
-1.2651073766085));
#75455=CARTESIAN_POINT('Ctrl Pts',(0.217401036646898,0.241560947845756,
-1.24927089758349));
#75456=CARTESIAN_POINT('Ctrl Pts',(-0.0842470053836159,0.313874727149509,
-1.23343441855849));
#75457=CARTESIAN_POINT('Ctrl Pts',(-0.309141520223219,0.100231844906513,
-1.21759793953349));
#75458=CARTESIAN_POINT('Ctrl Pts',(-0.252391578144153,-0.204727608155788,
-1.20176146050848));
#75459=CARTESIAN_POINT('Ctrl Pts',(0.034300588796614,-0.32316926194719,
-1.18592498148348));
#75460=CARTESIAN_POINT('Ctrl Pts',(0.28974308504728,-0.147186435946288,
-1.17008850245847));
#75461=CARTESIAN_POINT('Ctrl Pts',(0.281214136196824,0.162891104307017,
-1.15425202343347));
#75462=CARTESIAN_POINT('Ctrl Pts',(0.0164840707515565,0.324566137591005,
-1.13841554440846));
#75463=CARTESIAN_POINT('Ctrl Pts',(-0.263263864668857,0.190544062670301,
-1.12257906538346));
#75464=CARTESIAN_POINT('Ctrl Pts',(-0.303164340785093,-0.117073843088991,
-1.10674258635845));
#75465=CARTESIAN_POINT('Ctrl Pts',(-0.0668658900930811,-0.318031217023338,
-1.09090610733345));
#75466=CARTESIAN_POINT('Ctrl Pts',(0.230350962268339,-0.22924514485881,
-1.07506962830844));
#75467=CARTESIAN_POINT('Ctrl Pts',(0.31770576949938,0.0683955136400972,
-1.05923314928344));
#75468=CARTESIAN_POINT('Ctrl Pts',(0.115613630729864,0.303724201618416,
-1.04339667025844));
#75469=CARTESIAN_POINT('Ctrl Pts',(-0.191808708317494,0.262343899629591,
-1.02756019123343));
#75470=CARTESIAN_POINT('Ctrl Pts',(-0.324483056712076,-0.018045724315569,
-1.01172371220843));
#75471=CARTESIAN_POINT('Ctrl Pts',(-0.161535988025596,-0.281994728376046,
-0.995887233183423));
#75472=CARTESIAN_POINT('Ctrl Pts',(0.148579004230125,-0.289031454622626,
-0.980050754158418));
#75473=CARTESIAN_POINT('Ctrl Pts',(0.323330578056337,-0.0327450691408802,
-0.964214275133415));
#75474=CARTESIAN_POINT('Ctrl Pts',(0.203510704488092,0.253373825439895,
-0.948377796108409));
#75475=CARTESIAN_POINT('Ctrl Pts',(-0.101718304033287,0.308655615344801,
-0.932541317083407));
#75476=CARTESIAN_POINT('Ctrl Pts',(-0.314276497979333,0.0827356336600666,
-0.9167048380584));
#75477=CARTESIAN_POINT('Ctrl Pts',(-0.240511995667115,-0.218560934751633,
-0.900868359033399));
#75478=CARTESIAN_POINT('Ctrl Pts',(0.0523717965844736,-0.32073680359728,
-0.885031880008391));
#75479=CARTESIAN_POINT('Ctrl Pts',(0.297542081455241,-0.130704292288237,
-0.86919540098339));
#75480=CARTESIAN_POINT('Ctrl Pts',(0.27163561842944,0.178406818983305,-0.853358921958384));
#75481=CARTESIAN_POINT('Ctrl Pts',(-0.00174541927363239,0.324979777479838,
-0.83752244293338));
#75482=CARTESIAN_POINT('Ctrl Pts',(-0.273536286678446,0.175478779712686,
-0.821685963908374));
#75483=CARTESIAN_POINT('Ctrl Pts',(-0.296120968988897,-0.133892770470861,
-0.805849484883371));
#75484=CARTESIAN_POINT('Ctrl Pts',(-0.0489236128566082,-0.321280846556937,
-0.790013005858366));
#75485=CARTESIAN_POINT('Ctrl Pts',(0.242845770881514,-0.21596489025823,
-0.774176526833362));
#75486=CARTESIAN_POINT('Ctrl Pts',(0.313369670656391,0.0861066302440811,
-0.758340047808358));
#75487=CARTESIAN_POINT('Ctrl Pts',(0.0983970423587119,0.309730405860231,
-0.742503568783354));
#75488=CARTESIAN_POINT('Ctrl Pts',(-0.206220553517287,0.251173218250494,
-0.726667089758349));
#75489=CARTESIAN_POINT('Ctrl Pts',(-0.322960197059656,-0.0362162032034551,
-0.710830610733345));
#75490=CARTESIAN_POINT('Ctrl Pts',(-0.145465830102453,-0.290610726801146,
-0.694994131708341));
#75491=CARTESIAN_POINT('Ctrl Pts',(0.164555687170394,-0.28024333726097,
-0.679157652683335));
#75492=CARTESIAN_POINT('Ctrl Pts',(0.3246581734683,-0.0145592808720665,
-0.663321173658333));
#75493=CARTESIAN_POINT('Ctrl Pts',(0.188979701955492,0.264389058979569,
-0.647484694633327));
#75494=CARTESIAN_POINT('Ctrl Pts',(-0.118869384127234,0.302464827337819,
-0.631648215608323));
#75495=CARTESIAN_POINT('Ctrl Pts',(-0.318422104478806,0.0649789630462639,
-0.615811736583319));
#75496=CARTESIAN_POINT('Ctrl Pts',(-0.227875259356083,-0.231706211467678,
-0.599975257558315));
#75497=CARTESIAN_POINT('Ctrl Pts',(0.0702781331505997,-0.31729463635576,
-0.58413877853331));
#75498=CARTESIAN_POINT('Ctrl Pts',(0.304404388085412,-0.113810679523475,
-0.568302299508307));
#75499=CARTESIAN_POINT('Ctrl Pts',(0.261201966807552,0.193360892621279,
-0.552465820483301));
#75500=CARTESIAN_POINT('Ctrl Pts',(-0.0199694145590941,0.324370351205662,
-0.536629341458298));
#75501=CARTESIAN_POINT('Ctrl Pts',(-0.282947591354669,0.159861073453475,
-0.520792862433293));
#75502=CARTESIAN_POINT('Ctrl Pts',(-0.288145381208641,-0.15029019112504,
-0.504956383408289));
#75503=CARTESIAN_POINT('Ctrl Pts',(-0.0308273195949118,-0.323519054499852,
-0.489119904383284));
#75504=CARTESIAN_POINT('Ctrl Pts',(0.254576078717811,-0.202004758367859,
-0.47328342535828));
#75505=CARTESIAN_POINT('Ctrl Pts',(0.308047055340646,0.10354667528121,-0.457446946333275));
#75506=CARTESIAN_POINT('Ctrl Pts',(0.0808706910526324,0.314761550347012,
-0.441610467308271));
#75507=CARTESIAN_POINT('Ctrl Pts',(-0.219983197459793,0.23921182055627,
-0.425773988283267));
#75508=CARTESIAN_POINT('Ctrl Pts',(-0.320420629126427,-0.0542726702097004,
-0.409937509258262));
#75509=CARTESIAN_POINT('Ctrl Pts',(-0.128937732287144,-0.29831185589437,
-0.394101030233258));
#75510=CARTESIAN_POINT('Ctrl Pts',(0.180014333496764,-0.270572988336741,
-0.378264551208253));
#75511=CARTESIAN_POINT('Ctrl Pts',(0.324963715556635,0.00367234169457965,
-0.362428072183249));
#75512=CARTESIAN_POINT('Ctrl Pts',(0.173853773214234,0.274571970838708,
-0.346591593158245));
#75513=CARTESIAN_POINT('Ctrl Pts',(-0.135646251031432,0.295321853558036,
-0.330755114133241));
#75514=CARTESIAN_POINT('Ctrl Pts',(-0.321565291760542,0.0470177302856763,
-0.314918635108236));
#75515=CARTESIAN_POINT('Ctrl Pts',(-0.214521145490182,-0.244122051166946,
-0.299082156083232));
#75516=CARTESIAN_POINT('Ctrl Pts',(0.0879632175303027,-0.312853605266472,
-0.283245677058228));
#75517=CARTESIAN_POINT('Ctrl Pts',(0.310308421199756,-0.0965587635143514,
-0.267409198033223));
#75518=CARTESIAN_POINT('Ctrl Pts',(0.249945990305456,0.20770621637189,-0.251572719008219));
#75519=CARTESIAN_POINT('Ctrl Pts',(-0.0381304733960651,0.322739838521851,
-0.235736239983215));
#75520=CARTESIAN_POINT('Ctrl Pts',(-0.291468286469691,0.143739992923516,
-0.21989976095821));
#75521=CARTESIAN_POINT('Ctrl Pts',(-0.279262426658274,-0.166214261098879,
-0.204063281933206));
#75522=CARTESIAN_POINT('Ctrl Pts',(-0.0126344731763009,-0.324739221417544,
-0.188226802908201));
#75523=CARTESIAN_POINT('Ctrl Pts',(0.265505901415917,-0.187407882030522,
-0.172390323883198));
#75524=CARTESIAN_POINT('Ctrl Pts',(0.301752877046697,0.120659189302949,
-0.156553844858192));
#75525=CARTESIAN_POINT('Ctrl Pts',(0.0630931944606496,0.318804769777907,
-0.140717365833189));
#75526=CARTESIAN_POINT('Ctrl Pts',(-0.233059890698008,0.226491683043557,
-0.124880886808183));
#75527=CARTESIAN_POINT('Ctrl Pts',(-0.316859785345509,-0.0721474341499148,
-0.10904440778318));
#75528=CARTESIAN_POINT('Ctrl Pts',(-0.112027726134506,-0.305094594402439,
-0.0932079287581754));
#75529=CARTESIAN_POINT('Ctrl Pts',(0.194952158946614,-0.260011246811268,
-0.0773714497331713));
#75530=CARTESIAN_POINT('Ctrl Pts',(0.324158252946565,0.021816558371408,
-0.0615349707081665));
#75531=CARTESIAN_POINT('Ctrl Pts',(0.158351729189089,0.284037130360981,
-0.0456984916831627));
#75532=CARTESIAN_POINT('Ctrl Pts',(-0.152350606602819,0.28695356414546,
-0.0298620126581584));
#75533=CARTESIAN_POINT('Ctrl Pts',(-0.265981509802645,0.115392554247619,
-0.0193043599748219));
#75534=CARTESIAN_POINT('Ctrl Pts',(-0.274100747794842,0.0244792455170898,
-0.0140255336331538));
#75535=CARTESIAN_POINT('Ctrl Pts',(0.148738611075532,-0.20858265952159,
-1.96677446636685));
#75536=CARTESIAN_POINT('Ctrl Pts',(0.217920982424313,-0.159249268869985,
-1.96149564002518));
#75537=CARTESIAN_POINT('Ctrl Pts',(0.302177556134698,0.0127920164795567,
-1.95093798734184));
#75538=CARTESIAN_POINT('Ctrl Pts',(0.153517856671363,0.2609212574155,-1.93510150831684));
#75539=CARTESIAN_POINT('Ctrl Pts',(-0.135135152580135,0.270582120883482,
-1.91926502929183));
#75540=CARTESIAN_POINT('Ctrl Pts',(-0.300604288620724,0.034106051653201,
-1.90342855026683));
#75541=CARTESIAN_POINT('Ctrl Pts',(-0.192242753730676,-0.233638288925213,
-1.88759207124182));
#75542=CARTESIAN_POINT('Ctrl Pts',(0.0912810156776652,-0.288423351270546,
-1.87175559221682));
#75543=CARTESIAN_POINT('Ctrl Pts',(0.291633052580356,-0.0804928506983476,
-1.85591911319182));
#75544=CARTESIAN_POINT('Ctrl Pts',(0.22629693759269,0.200798965734433,-1.84008263416681));
#75545=CARTESIAN_POINT('Ctrl Pts',(-0.0452104879428866,0.299137514716973,
-1.82424615514181));
#75546=CARTESIAN_POINT('Ctrl Pts',(-0.275527328363567,0.124953471858079,
-1.8084096761168));
#75547=CARTESIAN_POINT('Ctrl Pts',(-0.254824777933654,-0.163073887353064,
-1.7925731970918));
#75548=CARTESIAN_POINT('Ctrl Pts',(-0.00196284025457797,-0.3025301091378,
-1.7767367180668));
#75549=CARTESIAN_POINT('Ctrl Pts',(0.252687147118379,-0.166366325282896,
-1.76090023904179));
#75550=CARTESIAN_POINT('Ctrl Pts',(0.277125736632896,0.121366654750872,
-1.74506376001679));
#75551=CARTESIAN_POINT('Ctrl Pts',(0.0490879046201066,0.298527819857348,
-1.72922728099178));
#75552=CARTESIAN_POINT('Ctrl Pts',(-0.22367160448731,0.203714334835507,
-1.71339080196678));
#75553=CARTESIAN_POINT('Ctrl Pts',(-0.292654335827258,-0.0766938860821337,
-1.69755432294177));
#75554=CARTESIAN_POINT('Ctrl Pts',(-0.095013308945888,-0.287229832059019,
-1.68171784391677));
#75555=CARTESIAN_POINT('Ctrl Pts',(0.189189919247545,-0.236084063505319,
-1.66588136489176));
#75556=CARTESIAN_POINT('Ctrl Pts',(0.301031015861915,0.0301469238779581,
-1.65004488586676));
#75557=CARTESIAN_POINT('Ctrl Pts',(0.138616757612798,0.268912445217012,
-1.63420840684176));
#75558=CARTESIAN_POINT('Ctrl Pts',(-0.150084779046188,0.262684351559698,
-1.61837192781675));
#75559=CARTESIAN_POINT('Ctrl Pts',(-0.302051056207392,0.0171367643261984,
-1.60253544879175));
#75560=CARTESIAN_POINT('Ctrl Pts',(-0.178832668181669,-0.244023330740404,
-1.58669896976674));
#75561=CARTESIAN_POINT('Ctrl Pts',(0.107311843925988,-0.282865122307182,
-1.57086249074174));
#75562=CARTESIAN_POINT('Ctrl Pts',(0.295689527534716,-0.0640016603979571,
-1.55502601171673));
#75563=CARTESIAN_POINT('Ctrl Pts',(0.214678238914141,0.213170736629585,
-1.53918953269173));
#75564=CARTESIAN_POINT('Ctrl Pts',(-0.0619164057168387,0.29613319289955,
-1.52335305366672));
#75565=CARTESIAN_POINT('Ctrl Pts',(-0.282101893635751,0.109302474055358,
-1.50751657464172));
#75566=CARTESIAN_POINT('Ctrl Pts',(-0.245277470454903,-0.177108643815393,
-1.49168009561672));
#75567=CARTESIAN_POINT('Ctrl Pts',(0.0150078450390444,-0.302164315921385,
-1.47584361659171));
#75568=CARTESIAN_POINT('Ctrl Pts',(0.261620211127157,-0.151932137343368,
-1.46000713756671));
#75569=CARTESIAN_POINT('Ctrl Pts',(0.269882574184939,0.136718343243556,
-1.4441706585417));
#75570=CARTESIAN_POINT('Ctrl Pts',(0.0322674796201843,0.300811101834997,
-1.4283341795167));
#75571=CARTESIAN_POINT('Ctrl Pts',(-0.234745014450272,0.190848860145424,
-1.41249770049169));
#75572=CARTESIAN_POINT('Ctrl Pts',(-0.287892246871325,-0.0929868991818828,
-1.39666122146669));
#75573=CARTESIAN_POINT('Ctrl Pts',(-0.0787542467470654,-0.292106620683986,
-1.38082474244169));
#75574=CARTESIAN_POINT('Ctrl Pts',(0.202133083713364,-0.225101589724768,
-1.36498826341668));
#75575=CARTESIAN_POINT('Ctrl Pts',(0.298866365417606,0.0469830272563036,
-1.34915178439168));
#75576=CARTESIAN_POINT('Ctrl Pts',(0.123316405716688,0.27626359389036,-1.33331530536667));
#75577=CARTESIAN_POINT('Ctrl Pts',(-0.16458139419722,0.253853252711475,
-1.31747882634167));
#75578=CARTESIAN_POINT('Ctrl Pts',(-0.302536742660015,0.000169022973934383,
-1.30164234731666));
#75579=CARTESIAN_POINT('Ctrl Pts',(-0.164864939768642,-0.253669195731725,
-1.28580586829166));
#75580=CARTESIAN_POINT('Ctrl Pts',(0.123007639752607,-0.276401211630105,
-1.26996938926665));
#75581=CARTESIAN_POINT('Ctrl Pts',(0.298813681366057,-0.0473169425952548,
-1.25413291024165));
#75582=CARTESIAN_POINT('Ctrl Pts',(0.202384479562695,0.224875591517254,
-1.23829643121665));
#75583=CARTESIAN_POINT('Ctrl Pts',(-0.0784278060595097,0.29219443606063,
-1.22245995219164));
#75584=CARTESIAN_POINT('Ctrl Pts',(-0.287788166269031,0.0933085236385542,
-1.20662347316664));
#75585=CARTESIAN_POINT('Ctrl Pts',(-0.234958116927824,-0.190586443688498,
-1.19078699414163));
#75586=CARTESIAN_POINT('Ctrl Pts',(0.0319313418158729,-0.300846968802971,
-1.17495051511663));
#75587=CARTESIAN_POINT('Ctrl Pts',(0.269729640569406,-0.137019816911266,
-1.15911403609162));
#75588=CARTESIAN_POINT('Ctrl Pts',(0.261789812402348,0.151639715610526,
-1.14327755706662));
#75589=CARTESIAN_POINT('Ctrl Pts',(0.0153454653739602,0.302147357957263,
-1.12744107804161));
#75590=CARTESIAN_POINT('Ctrl Pts',(-0.245079421241258,0.177382599237209,
-1.11160459901661));
#75591=CARTESIAN_POINT('Ctrl Pts',(-0.282223848966336,-0.108987193296848,
-1.09576811999161));
#75592=CARTESIAN_POINT('Ctrl Pts',(-0.0622472577670544,-0.296063824417269,
-1.0799316409666));
#75593=CARTESIAN_POINT('Ctrl Pts',(0.214439914061512,-0.21341047885563,
-1.0640951619416));
#75594=CARTESIAN_POINT('Ctrl Pts',(0.295760856553006,0.0636712255193022,
-1.04825868291659));
#75595=CARTESIAN_POINT('Ctrl Pts',(0.10762784228863,0.282745038492971,-1.03242220389159));
#75596=CARTESIAN_POINT('Ctrl Pts',(-0.178559891926731,0.244223001011805,
-1.01658572486658));
#75597=CARTESIAN_POINT('Ctrl Pts',(-0.302070015729723,-0.0167992507315895,
-1.00074924584158));
#75598=CARTESIAN_POINT('Ctrl Pts',(-0.150378201371251,-0.262516486683113,
-0.984912766816576));
#75599=CARTESIAN_POINT('Ctrl Pts',(0.138316196228161,-0.269067164643089,
-0.969076287791573));
#75600=CARTESIAN_POINT('Ctrl Pts',(0.300997142313173,-0.0304832666786445,
-0.953239808766568));
#75601=CARTESIAN_POINT('Ctrl Pts',(0.189453595293367,0.235872517387072,
-0.937403329741564));
#75602=CARTESIAN_POINT('Ctrl Pts',(-0.0946923084695934,0.28733582433243,
-0.92156685071656));
#75603=CARTESIAN_POINT('Ctrl Pts',(-0.292568455345688,0.077020829421243,
-0.905730371691556));
#75604=CARTESIAN_POINT('Ctrl Pts',(-0.22389909368617,-0.203464259944122,
-0.88989389266655));
#75605=CARTESIAN_POINT('Ctrl Pts',(0.0487543157980785,-0.298582527819628,
-0.874057413641548));
#75606=CARTESIAN_POINT('Ctrl Pts',(0.276989936350333,-0.121676145520544,
-0.858220934616541));
#75607=CARTESIAN_POINT('Ctrl Pts',(0.25287291226593,0.166083712236466,-0.842384455591539));
#75608=CARTESIAN_POINT('Ctrl Pts',(-0.00162485780547096,0.302532426468981,
-0.826547976566533));
#75609=CARTESIAN_POINT('Ctrl Pts',(-0.254642295523387,0.163357921628179,
-0.810711497541529));
#75610=CARTESIAN_POINT('Ctrl Pts',(-0.275666984485257,-0.124644385725563,
-0.794875018516526));
#75611=CARTESIAN_POINT('Ctrl Pts',(-0.0455443087071976,-0.299088992061696,
-0.77903853949152));
#75612=CARTESIAN_POINT('Ctrl Pts',(0.22607166788116,-0.201047532214471,
-0.763202060466516));
#75613=CARTESIAN_POINT('Ctrl Pts',(0.291724265370159,0.0801589809212851,
-0.747365581441513));
#75614=CARTESIAN_POINT('Ctrl Pts',(0.0916004565360948,0.288336375767049,
-0.731529102416506));
#75615=CARTESIAN_POINT('Ctrl Pts',(-0.191976266730112,0.23382391289273,
-0.715692623391504));
#75616=CARTESIAN_POINT('Ctrl Pts',(-0.300652344669107,-0.0337146388541525,
-0.699856144366498));
#75617=CARTESIAN_POINT('Ctrl Pts',(-0.135418058595813,-0.270537351643426,
-0.684019665341495));
#75618=CARTESIAN_POINT('Ctrl Pts',(0.153189320624786,-0.260886069529622,
-0.668183186316489));
#75619=CARTESIAN_POINT('Ctrl Pts',(0.302233036633937,-0.013553626641099,
-0.652346707291486));
#75620=CARTESIAN_POINT('Ctrl Pts',(0.175926293720004,0.246126894926262,
-0.636510228266482));
#75621=CARTESIAN_POINT('Ctrl Pts',(-0.110658710802758,0.28157265306057,
-0.620673749241477));
#75622=CARTESIAN_POINT('Ctrl Pts',(-0.296427712076052,0.0604906665647636,
-0.604837270216473));
#75623=CARTESIAN_POINT('Ctrl Pts',(-0.212135215550515,-0.215701552037653,
-0.589000791191469));
#75624=CARTESIAN_POINT('Ctrl Pts',(0.0654238067200374,-0.295378121637912,
-0.573164312166464));
#75625=CARTESIAN_POINT('Ctrl Pts',(0.283378242392325,-0.105949426457638,
-0.55732783314146));
#75626=CARTESIAN_POINT('Ctrl Pts',(0.243159944995843,0.180004862095007,
-0.541491354116455));
#75627=CARTESIAN_POINT('Ctrl Pts',(-0.0185900657837185,0.301965095138675,
-0.525654875091452));
#75628=CARTESIAN_POINT('Ctrl Pts',(-0.263403532490242,0.14881897829109,
-0.509818396066446));
#75629=CARTESIAN_POINT('Ctrl Pts',(-0.268242295040306,-0.139909186190414,
-0.493981917041443));
#75630=CARTESIAN_POINT('Ctrl Pts',(-0.0286979819818524,-0.301172600110059,
-0.478145438016438));
#75631=CARTESIAN_POINT('Ctrl Pts',(0.236991727339823,-0.188051669495342,
-0.462308958991434));
#75632=CARTESIAN_POINT('Ctrl Pts',(0.286769299436215,0.0963943885018026,
-0.446472479966429));
#75633=CARTESIAN_POINT('Ctrl Pts',(0.0752847041256083,0.293020003657083,
-0.430636000941425));
#75634=CARTESIAN_POINT('Ctrl Pts',(-0.204788282600279,0.222688725662139,
-0.414799521916421));
#75635=CARTESIAN_POINT('Ctrl Pts',(-0.298288192490222,-0.0505238902457886,
-0.398963042891416));
#75636=CARTESIAN_POINT('Ctrl Pts',(-0.120031607242568,-0.277706540105525,
-0.383126563866412));
#75637=CARTESIAN_POINT('Ctrl Pts',(0.167580190786954,-0.25188368129631,
-0.367290084841407));
#75638=CARTESIAN_POINT('Ctrl Pts',(0.302517473992129,0.00341868177860365,
-0.351453605816403));
#75639=CARTESIAN_POINT('Ctrl Pts',(0.161845159317807,0.255606441798855,
-0.335617126791399));
#75640=CARTESIAN_POINT('Ctrl Pts',(-0.126276748000131,0.274923066410718,
-0.319780647766394));
#75641=CARTESIAN_POINT('Ctrl Pts',(-0.29935378976176,0.0437700712970414,
-0.303944168741391));
#75642=CARTESIAN_POINT('Ctrl Pts',(-0.199703511330258,-0.227259791568734,
-0.288107689716386));
#75643=CARTESIAN_POINT('Ctrl Pts',(0.0818873280233965,-0.291243846201189,
-0.272271210691382));
#75644=CARTESIAN_POINT('Ctrl Pts',(0.288874465812401,-0.0898891532555531,
-0.256434731666377));
#75645=CARTESIAN_POINT('Ctrl Pts',(0.232681453349795,0.19335931028994,-0.240598252641373));
#75646=CARTESIAN_POINT('Ctrl Pts',(-0.035496684527205,0.300447206972072,
-0.224761773616368));
#75647=CARTESIAN_POINT('Ctrl Pts',(-0.271335677032713,0.133811430289637,
-0.208925294591364));
#75648=CARTESIAN_POINT('Ctrl Pts',(-0.259972913433929,-0.154733331759737,
-0.19308881556636));
#75649=CARTESIAN_POINT('Ctrl Pts',(-0.0117617713225866,-0.302308486352486,
-0.177252336541355));
#75650=CARTESIAN_POINT('Ctrl Pts',(0.247166593626507,-0.174463044223185,
-0.161415857516351));
#75651=CARTESIAN_POINT('Ctrl Pts',(0.280909879361946,0.112324888639776,
-0.145579378491347));
#75652=CARTESIAN_POINT('Ctrl Pts',(0.0587351538052031,0.296783945508053,
-0.129742899466343));
#75653=CARTESIAN_POINT('Ctrl Pts',(-0.216961728487364,0.210847207101868,
-0.113906420441338));
#75654=CARTESIAN_POINT('Ctrl Pts',(-0.294973307122055,-0.0671639893600439,
-0.0980699414163342));
#75655=CARTESIAN_POINT('Ctrl Pts',(-0.10428962713342,-0.284020774039906,
-0.0822334623913293));
#75656=CARTESIAN_POINT('Ctrl Pts',(0.181486214769611,-0.242051471685551,
-0.0663969833663252));
#75657=CARTESIAN_POINT('Ctrl Pts',(0.301767647157536,0.0203096217016589,
-0.0505605043413204));
#75658=CARTESIAN_POINT('Ctrl Pts',(0.147413889069162,0.264417813692194,
-0.0347240253163167));
#75659=CARTESIAN_POINT('Ctrl Pts',(-0.141827282445081,0.267132800440896,
-0.0188875462913122));
#75660=CARTESIAN_POINT('Ctrl Pts',(-0.247609350281711,0.107422036237781,
-0.00832989360797585));
#75661=CARTESIAN_POINT('Ctrl Pts',(-0.255167767577417,0.0227883888709785,
-0.00305106726630777));
#75662=CARTESIAN_POINT('Ctrl Pts',(0.137702479013101,-0.193106208855765,
-1.9558));
#75663=CARTESIAN_POINT('Ctrl Pts',(0.201751645331416,-0.147433265282304,
-1.95052117365833));
#75664=CARTESIAN_POINT('Ctrl Pts',(0.279756535851592,0.0118428723253114,
-1.939963520975));
#75665=CARTESIAN_POINT('Ctrl Pts',(0.142127113353835,0.241561378807579,
-1.92412704194999));
#75666=CARTESIAN_POINT('Ctrl Pts',(-0.125108372180837,0.250505423930283,
-1.90829056292499));
#75667=CARTESIAN_POINT('Ctrl Pts',(-0.278300001900802,0.0315754451923003,
-1.89245408389998));
#75668=CARTESIAN_POINT('Ctrl Pts',(-0.177978694096959,-0.216302756525292,
-1.87661760487498));
#75669=CARTESIAN_POINT('Ctrl Pts',(0.0845081317806936,-0.26702286775457,
-1.86078112584997));
#75670=CARTESIAN_POINT('Ctrl Pts',(0.269994415115787,-0.0745204288506152,
-1.84494464682497));
#75671=CARTESIAN_POINT('Ctrl Pts',(0.209506119993022,0.185900050867469,
-1.82910816779996));
#75672=CARTESIAN_POINT('Ctrl Pts',(-0.0418559526817564,0.27694205992973,
-1.81327168877496));
#75673=CARTESIAN_POINT('Ctrl Pts',(-0.255083706087942,0.115682153488801,
-1.79743520974995));
#75674=CARTESIAN_POINT('Ctrl Pts',(-0.235917246918538,-0.150974104090677,
-1.78159873072495));
#75675=CARTESIAN_POINT('Ctrl Pts',(-0.0018172011087593,-0.280082930068666,
-1.76576225169995));
#75676=CARTESIAN_POINT('Ctrl Pts',(0.23393822438801,-0.154022249166496,
-1.74992577267494));
#75677=CARTESIAN_POINT('Ctrl Pts',(0.256563515396163,0.112361471630493,
-1.73408929364994));
#75678=CARTESIAN_POINT('Ctrl Pts',(0.0454456721551229,0.27637760331013,
-1.71825281462493));
#75679=CARTESIAN_POINT('Ctrl Pts',(-0.207075581787567,0.188599104929845,
-1.70241633559993));
#75680=CARTESIAN_POINT('Ctrl Pts',(-0.270939921019438,-0.0710033404392579,
-1.68657985657493));
#75681=CARTESIAN_POINT('Ctrl Pts',(-0.087963495735764,-0.265917905478881,
-1.67074337754992));
#75682=CARTESIAN_POINT('Ctrl Pts',(0.175152374331677,-0.218567059118628,
-1.65490689852492));
#75683=CARTESIAN_POINT('Ctrl Pts',(0.27869506676358,0.0279100774344748,
-1.63907041949991));
#75684=CARTESIAN_POINT('Ctrl Pts',(0.128331648507507,0.248959635135041,
-1.62323394047491));
#75685=CARTESIAN_POINT('Ctrl Pts',(-0.138948763790046,0.243193654600889,
-1.6073974614499));
#75686=CARTESIAN_POINT('Ctrl Pts',(-0.279639421986813,0.0158652478527055,
-1.5915609824249));
#75687=CARTESIAN_POINT('Ctrl Pts',(-0.165563612293228,-0.225917247290439,
-1.5757245033999));
#75688=CARTESIAN_POINT('Ctrl Pts',(0.0993495019835277,-0.261877049183029,
-1.55988802437489));
#75689=CARTESIAN_POINT('Ctrl Pts',(0.273749907070638,-0.059252854615386,
-1.54405154534989));
#75690=CARTESIAN_POINT('Ctrl Pts',(0.198749507440483,0.197353859059745,
-1.52821506632488));
#75691=CARTESIAN_POINT('Ctrl Pts',(-0.057322322005953,0.27416065327936,
-1.51237858729988));
#75692=CARTESIAN_POINT('Ctrl Pts',(-0.261170450678782,0.101192431009352,
-1.49654210827487));
#75693=CARTESIAN_POINT('Ctrl Pts',(-0.227078332138994,-0.163967507371998,
-1.48070562924987));
#75694=CARTESIAN_POINT('Ctrl Pts',(0.0138942904708965,-0.279744278037816,
-1.46486915022487));
#75695=CARTESIAN_POINT('Ctrl Pts',(0.242208471436148,-0.140659051490779,
-1.44903267119986));
#75696=CARTESIAN_POINT('Ctrl Pts',(0.249857782313367,0.12657409300159,-1.43319619217486));
#75697=CARTESIAN_POINT('Ctrl Pts',(0.0298732918310454,0.278491469954,-1.41735971314985));
#75698=CARTESIAN_POINT('Ctrl Pts',(-0.217327365046816,0.176688224858463,
-1.40152323412485));
#75699=CARTESIAN_POINT('Ctrl Pts',(-0.266531170327395,-0.0860874418585526,
-1.38568675509984));
#75700=CARTESIAN_POINT('Ctrl Pts',(-0.0729108261228343,-0.270432845334947,
-1.36985027607484));
#75701=CARTESIAN_POINT('Ctrl Pts',(0.187135179739969,-0.208399464743887,
-1.35401379704983));
#75702=CARTESIAN_POINT('Ctrl Pts',(0.276691029410919,0.0434969728300605,
-1.33817731802483));
#75703=CARTESIAN_POINT('Ctrl Pts',(0.114166554651702,0.255765342063417,
-1.32234083899983));
#75704=CARTESIAN_POINT('Ctrl Pts',(-0.152369756692705,0.235017807085461,
-1.30650435997482));
#75705=CARTESIAN_POINT('Ctrl Pts',(-0.280089071395702,0.000156481779360123,
-1.29066788094982));
#75706=CARTESIAN_POINT('Ctrl Pts',(-0.152632263702923,-0.234847406795936,
-1.27483140192481));
#75707=CARTESIAN_POINT('Ctrl Pts',(0.11388069855569,-0.255892748819348,
-1.25899492289981));
#75708=CARTESIAN_POINT('Ctrl Pts',(0.27664225441934,-0.0438061122634664,
-1.2431584438748));
#75709=CARTESIAN_POINT('Ctrl Pts',(0.187367922478493,0.208190235188752,
-1.2273219648498));
#75710=CARTESIAN_POINT('Ctrl Pts',(-0.0726086067354031,0.270514144971751,
-1.2114854858248));
#75711=CARTESIAN_POINT('Ctrl Pts',(-0.266434812314843,0.086385202370595,
-1.19564900679979));
#75712=CARTESIAN_POINT('Ctrl Pts',(-0.217524655711494,-0.176445279221209,
-1.17981252777479));
#75713=CARTESIAN_POINT('Ctrl Pts',(0.0295620948351317,-0.278524675658752,
-1.16397604874978));
#75714=CARTESIAN_POINT('Ctrl Pts',(0.249716196091533,-0.126853197876244,
-1.14813956972478));
#75715=CARTESIAN_POINT('Ctrl Pts',(0.242365488607872,0.140388326914034,
-1.13230309069977));
#75716=CARTESIAN_POINT('Ctrl Pts',(0.0142068599963639,0.27972857832352,
-1.11646661167477));
#75717=CARTESIAN_POINT('Ctrl Pts',(-0.226894977813658,0.164221135804117,
-1.10063013264977));
#75718=CARTESIAN_POINT('Ctrl Pts',(-0.261283357147579,-0.100900543504706,
-1.08479365362476));
#75719=CARTESIAN_POINT('Ctrl Pts',(-0.0576286254410279,-0.2740964318112,
-1.06895717459976));
#75720=CARTESIAN_POINT('Ctrl Pts',(0.198528865854686,-0.197575812852451,
-1.05312069557475));
#75721=CARTESIAN_POINT('Ctrl Pts',(0.273815943606632,0.0589469373985079,
-1.03728421654975));
#75722=CARTESIAN_POINT('Ctrl Pts',(0.0996420538473957,0.261765875367525,
-1.02144773752474));
#75723=CARTESIAN_POINT('Ctrl Pts',(-0.165311075535969,0.22610210239402,
-1.00561125849974));
#75724=CARTESIAN_POINT('Ctrl Pts',(-0.279656974747369,-0.0155527771476102,
-0.989774779474735));
#75725=CARTESIAN_POINT('Ctrl Pts',(-0.139220414716906,-0.24303824499018,
-0.973938300449731));
#75726=CARTESIAN_POINT('Ctrl Pts',(0.128053388226197,-0.249102874663553,
-0.958101821424727));
#75727=CARTESIAN_POINT('Ctrl Pts',(0.278663706570009,-0.0282214642164085,
-0.942265342399722));
#75728=CARTESIAN_POINT('Ctrl Pts',(0.175396486098643,0.218371209334249,
-0.926428863374717));
#75729=CARTESIAN_POINT('Ctrl Pts',(-0.0876663129058996,0.26601603332006,
-0.910592384349715));
#75730=CARTESIAN_POINT('Ctrl Pts',(-0.270860412712043,0.0713060251824191,
-0.894755905324708));
#75731=CARTESIAN_POINT('Ctrl Pts',(-0.207286191705226,-0.188367585136611,
-0.878919426299706));
#75732=CARTESIAN_POINT('Ctrl Pts',(0.0451368350116836,-0.276428252041976,
-0.8630829472747));
#75733=CARTESIAN_POINT('Ctrl Pts',(0.256437791245425,-0.112647998752851,
-0.847246468249696));
#75734=CARTESIAN_POINT('Ctrl Pts',(0.23411020610242,0.153760605489627,-0.831409989224693));
#75735=CARTESIAN_POINT('Ctrl Pts',(-0.00150429633730956,0.280085075458125,
-0.815573510199687));
#75736=CARTESIAN_POINT('Ctrl Pts',(-0.235748304368328,0.151237063543671,
-0.799737031174683));
#75737=CARTESIAN_POINT('Ctrl Pts',(-0.255212999981617,-0.115396000980265,
-0.78390055214968));
#75738=CARTESIAN_POINT('Ctrl Pts',(-0.0421650045577871,-0.276897137566454,
-0.768064073124674));
#75739=CARTESIAN_POINT('Ctrl Pts',(0.209297564880806,-0.186130174170711,
-0.752227594099669));
#75740=CARTESIAN_POINT('Ctrl Pts',(0.270078860083927,0.0742113315984893,
-0.736391115074667));
#75741=CARTESIAN_POINT('Ctrl Pts',(0.0848038707134778,0.266942345673866,
-0.720554636049661));
#75742=CARTESIAN_POINT('Ctrl Pts',(-0.177731979942937,0.216474607534967,
-0.704718157024658));
#75743=CARTESIAN_POINT('Ctrl Pts',(-0.278344492278559,-0.0312130745048499,
-0.688881677999652));
#75744=CARTESIAN_POINT('Ctrl Pts',(-0.125370287089174,-0.250463976485706,
-0.673045198974649));
#75745=CARTESIAN_POINT('Ctrl Pts',(0.141822954079178,-0.241528801798274,
-0.657208719949644));
#75746=CARTESIAN_POINT('Ctrl Pts',(0.279807899799573,-0.0125479724101313,
-0.64137224092464));
#75747=CARTESIAN_POINT('Ctrl Pts',(0.162872885484516,0.227864730872955,
-0.625535761899635));
#75748=CARTESIAN_POINT('Ctrl Pts',(-0.102448037478282,0.260680478783321,
-0.609699282874631));
#75749=CARTESIAN_POINT('Ctrl Pts',(-0.274433319673298,0.0560023700832632,
-0.593862803849627));
#75750=CARTESIAN_POINT('Ctrl Pts',(-0.196395171744947,-0.199696892607627,
-0.578026324824622));
#75751=CARTESIAN_POINT('Ctrl Pts',(0.0605694802894751,-0.273461606920063,
-0.562189845799617));
#75752=CARTESIAN_POINT('Ctrl Pts',(0.262352096699239,-0.0980881733918026,
-0.546353366774615));
#75753=CARTESIAN_POINT('Ctrl Pts',(0.225117923184134,0.166648831568735,
-0.530516887749609));
#75754=CARTESIAN_POINT('Ctrl Pts',(-0.0172107170083428,0.279559839071688,
-0.514680408724605));
#75755=CARTESIAN_POINT('Ctrl Pts',(-0.243859473625816,0.137776883128706,
-0.498843929699601));
#75756=CARTESIAN_POINT('Ctrl Pts',(-0.24833920887197,-0.129528181255788,
-0.483007450674596));
#75757=CARTESIAN_POINT('Ctrl Pts',(-0.0265686443687933,-0.278826145720265,
-0.467170971649592));
#75758=CARTESIAN_POINT('Ctrl Pts',(0.219407375961836,-0.174098580622825,
-0.451334492624588));
#75759=CARTESIAN_POINT('Ctrl Pts',(0.265491543531784,0.0892421017223949,
-0.435498013599583));
#75760=CARTESIAN_POINT('Ctrl Pts',(0.0696987171985843,0.271278456967154,
-0.419661534574579));
#75761=CARTESIAN_POINT('Ctrl Pts',(-0.189593367740764,0.206165630768008,
-0.403825055549574));
#75762=CARTESIAN_POINT('Ctrl Pts',(-0.276155755854017,-0.0467751102818765,
-0.38798857652457));
#75763=CARTESIAN_POINT('Ctrl Pts',(-0.111125482197992,-0.25710122431668,
-0.372152097499565));
#75764=CARTESIAN_POINT('Ctrl Pts',(0.155146048077143,-0.23319437425588,
-0.356315618474562));
#75765=CARTESIAN_POINT('Ctrl Pts',(0.280071232427623,0.00316502186262762,
-0.340479139449557));
#75766=CARTESIAN_POINT('Ctrl Pts',(0.149836545421379,0.236640912759002,
-0.324642660424553));
#75767=CARTESIAN_POINT('Ctrl Pts',(-0.116907244968831,0.254524279263399,
-0.308806181399548));
#75768=CARTESIAN_POINT('Ctrl Pts',(-0.277142287762978,0.0405224123084065,
-0.292969702374544));
#75769=CARTESIAN_POINT('Ctrl Pts',(-0.184885877170335,-0.210397531970522,
-0.277133223349539));
#75770=CARTESIAN_POINT('Ctrl Pts',(0.0758114385164903,-0.269634087135906,
-0.261296744324535));
#75771=CARTESIAN_POINT('Ctrl Pts',(0.267440510425046,-0.0832195429967548,
-0.245460265299531));
#75772=CARTESIAN_POINT('Ctrl Pts',(0.215416916394134,0.17901240420799,-0.229623786274526));
#75773=CARTESIAN_POINT('Ctrl Pts',(-0.0328628956583448,0.278154575422294,
-0.213787307249523));
#75774=CARTESIAN_POINT('Ctrl Pts',(-0.251203067595735,0.123882867655757,
-0.197950828224518));
#75775=CARTESIAN_POINT('Ctrl Pts',(-0.240683400209584,-0.143252402420595,
-0.182114349199514));
#75776=CARTESIAN_POINT('Ctrl Pts',(-0.0108890694688725,-0.279877751287428,
-0.166277870174509));
#75777=CARTESIAN_POINT('Ctrl Pts',(0.228827285837098,-0.161518206415849,
-0.150441391149505));
#75778=CARTESIAN_POINT('Ctrl Pts',(0.260066881677195,0.103990587976603,
-0.134604912124501));
#75779=CARTESIAN_POINT('Ctrl Pts',(0.054377113149757,0.274763121238199,
-0.118768433099496));
#75780=CARTESIAN_POINT('Ctrl Pts',(-0.200863566276719,0.195202731160179,
-0.102931954074492));
#75781=CARTESIAN_POINT('Ctrl Pts',(-0.273086828898601,-0.0621805445701736,
-0.0870954750494882));
#75782=CARTESIAN_POINT('Ctrl Pts',(-0.0965515281323339,-0.262946953677372,
-0.0712589960244833));
#75783=CARTESIAN_POINT('Ctrl Pts',(0.168020270592608,-0.224091696559834,
-0.0554225169994791));
#75784=CARTESIAN_POINT('Ctrl Pts',(0.279377041368506,0.0188026850319098,
-0.0395860379744744));
#75785=CARTESIAN_POINT('Ctrl Pts',(0.136476048949234,0.244798497023407,
-0.0237495589494706));
#75786=CARTESIAN_POINT('Ctrl Pts',(-0.131303958287343,0.247312036736331,
-0.00791307992446619));
#75787=CARTESIAN_POINT('Ctrl Pts',(-0.229237190760777,0.0994515182279436,
0.00264457275887023));
#75788=CARTESIAN_POINT('Ctrl Pts',(-0.236234787359992,0.0210975322248671,
0.0079233991005383));
#75789=CARTESIAN_POINT('Origin',(0.,0.,-0.025));
#75790=CARTESIAN_POINT('',(-0.3192,3.90907258287835E-17,0.));
#75791=CARTESIAN_POINT('Origin',(-0.3192,-3.90907258287835E-17,-0.025));
#75792=CARTESIAN_POINT('Origin',(0.,0.,0.));
#75793=CARTESIAN_POINT('Origin',(0.,0.,-0.025));
#75794=CARTESIAN_POINT('Origin',(0.,0.,-0.975));
#75795=CARTESIAN_POINT('Origin',(0.47,0.,0.));
#75796=CARTESIAN_POINT('',(-0.47,-5.75583995599256E-17,1.21430643318376E-17));
#75797=CARTESIAN_POINT('Origin',(0.,0.,0.));
#75798=CARTESIAN_POINT('Origin',(0.,0.,0.24));
#75799=CARTESIAN_POINT('',(0.144337567297406,0.25,0.24));
#75800=CARTESIAN_POINT('',(0.288675134594813,0.,0.24));
#75801=CARTESIAN_POINT('',(0.288675134594813,0.,0.24));
#75802=CARTESIAN_POINT('Origin',(0.,0.,0.24));
#75803=CARTESIAN_POINT('Origin',(0.,0.,0.24));
#75804=CARTESIAN_POINT('',(0.144337567297406,-0.25,0.24));
#75805=CARTESIAN_POINT('',(0.144337567297406,-0.25,0.24));
#75806=CARTESIAN_POINT('Origin',(0.,0.,0.24));
#75807=CARTESIAN_POINT('Origin',(0.,0.,0.24));
#75808=CARTESIAN_POINT('',(-0.144337567297407,-0.25,0.24));
#75809=CARTESIAN_POINT('',(-0.144337567297407,-0.25,0.24));
#75810=CARTESIAN_POINT('Origin',(0.,0.,0.24));
#75811=CARTESIAN_POINT('Origin',(0.,0.,0.24));
#75812=CARTESIAN_POINT('',(-0.288675134594813,5.55111512312578E-17,0.24));
#75813=CARTESIAN_POINT('',(-0.288675134594813,3.53525079574969E-17,0.24));
#75814=CARTESIAN_POINT('Origin',(0.,0.,0.24));
#75815=CARTESIAN_POINT('Origin',(0.,0.,0.24));
#75816=CARTESIAN_POINT('',(-0.144337567297406,0.25,0.24));
#75817=CARTESIAN_POINT('',(-0.144337567297406,0.25,0.24));
#75818=CARTESIAN_POINT('Origin',(0.,0.,0.24));
#75819=CARTESIAN_POINT('Origin',(0.,0.,0.24));
#75820=CARTESIAN_POINT('',(0.144337567297406,0.25,0.24));
#75821=CARTESIAN_POINT('Origin',(0.,0.,0.24));
#75822=CARTESIAN_POINT('Origin',(0.,0.,0.153397459621556));
#75823=CARTESIAN_POINT('',(0.,0.,0.0667949192431123));
#75824=CARTESIAN_POINT('',(-0.144337567297406,-1.76762539787485E-17,0.153397459621556));
#75825=CARTESIAN_POINT('Origin',(0.144337567297406,0.25,0.6));
#75826=CARTESIAN_POINT('',(0.144337567297406,0.25,0.6));
#75827=CARTESIAN_POINT('',(0.288675134594813,0.,0.6));
#75828=CARTESIAN_POINT('',(0.180421959121758,0.1875,0.6));
#75829=CARTESIAN_POINT('',(0.144337567297406,0.25,0.6));
#75830=CARTESIAN_POINT('',(0.288675134594813,0.,0.6));
#75831=CARTESIAN_POINT('Origin',(-0.144337567297406,0.25,0.6));
#75832=CARTESIAN_POINT('',(-0.144337567297406,0.25,0.6));
#75833=CARTESIAN_POINT('',(-0.0721687836487032,0.25,0.6));
#75834=CARTESIAN_POINT('',(-0.144337567297406,0.25,0.6));
#75835=CARTESIAN_POINT('Origin',(-0.288675134594813,5.55111512312578E-17,
0.6));
#75836=CARTESIAN_POINT('',(-0.288675134594813,3.53525079574969E-17,0.6));
#75837=CARTESIAN_POINT('',(-0.252590742770461,0.0625000000000001,0.6));
#75838=CARTESIAN_POINT('',(-0.288675134594813,3.53525079574969E-17,0.6));
#75839=CARTESIAN_POINT('Origin',(-0.144337567297407,-0.25,0.6));
#75840=CARTESIAN_POINT('',(-0.144337567297407,-0.25,0.6));
#75841=CARTESIAN_POINT('',(-0.180421959121758,-0.1875,0.6));
#75842=CARTESIAN_POINT('',(-0.144337567297407,-0.25,0.6));
#75843=CARTESIAN_POINT('Origin',(0.144337567297406,-0.25,0.6));
#75844=CARTESIAN_POINT('',(0.144337567297406,-0.25,0.6));
#75845=CARTESIAN_POINT('',(0.0721687836487032,-0.25,0.6));
#75846=CARTESIAN_POINT('',(0.144337567297406,-0.25,0.6));
#75847=CARTESIAN_POINT('Origin',(0.288675134594813,0.,0.6));
#75848=CARTESIAN_POINT('',(0.252590742770461,-0.0625,0.6));
#75849=CARTESIAN_POINT('Origin',(0.497072620864318,-0.210994809384208,0.55));
#75850=CARTESIAN_POINT('',(0.466514061501753,-0.179901724341759,0.05));
#75851=CARTESIAN_POINT('',(0.466514061501753,-0.179901724341759,0.55));
#75852=CARTESIAN_POINT('',(0.466514061501753,-0.179901724341759,0.29));
#75853=CARTESIAN_POINT('',(0.451052457977236,-0.164169668796321,0.05));
#75854=CARTESIAN_POINT('',(0.497072620864318,-0.210994809384208,0.05));
#75855=CARTESIAN_POINT('',(0.451052457977236,-0.164169668796321,0.55));
#75856=CARTESIAN_POINT('',(0.451052457977236,-0.164169668796321,0.55));
#75857=CARTESIAN_POINT('',(0.497072620864318,-0.210994809384208,0.55));
#75858=CARTESIAN_POINT('Origin',(0.483728513098638,-0.184437764967243,0.55));
#75859=CARTESIAN_POINT('',(0.473009103818409,-0.162056742238344,0.55));
#75860=CARTESIAN_POINT('Origin',(0.,0.,0.55));
#75861=CARTESIAN_POINT('',(0.451052457977236,-0.164169668796321,0.55));
#75862=CARTESIAN_POINT('Origin',(0.451052457977236,-0.164169668796321,0.55));
#75863=CARTESIAN_POINT('',(0.473009103818409,-0.162056742238344,0.05));
#75864=CARTESIAN_POINT('',(0.473009103818409,-0.162056742238344,0.29));
#75865=CARTESIAN_POINT('',(0.451052457977236,-0.164169668796321,0.05));
#75866=CARTESIAN_POINT('Origin',(0.483728513098638,-0.184437764967243,0.05));
#75867=CARTESIAN_POINT('Origin',(0.,0.,0.05));
#75868=CARTESIAN_POINT('Origin',(0.394930998874352,-0.368279114433749,0.55));
#75869=CARTESIAN_POINT('',(0.376849807542158,-0.328609529008881,0.05));
#75870=CARTESIAN_POINT('',(0.376849807542158,-0.328609529008881,0.55));
#75871=CARTESIAN_POINT('',(0.376849807542158,-0.328609529008881,0.29));
#75872=CARTESIAN_POINT('',(0.367701332697109,-0.308538052649539,0.05));
#75873=CARTESIAN_POINT('',(0.394930998874352,-0.368279114433749,0.05));
#75874=CARTESIAN_POINT('',(0.367701332697109,-0.308538052649539,0.55));
#75875=CARTESIAN_POINT('',(0.367701332697109,-0.308538052649539,0.55));
#75876=CARTESIAN_POINT('',(0.394930998874352,-0.368279114433749,0.55));
#75877=CARTESIAN_POINT('Origin',(0.399482254061324,-0.338408583541644,0.55));
#75878=CARTESIAN_POINT('',(0.389056494215466,-0.314062166312295,0.55));
#75879=CARTESIAN_POINT('Origin',(0.,0.,0.55));
#75880=CARTESIAN_POINT('',(0.367701332697109,-0.308538052649539,0.55));
#75881=CARTESIAN_POINT('Origin',(0.367701332697109,-0.308538052649539,0.55));
#75882=CARTESIAN_POINT('',(0.389056494215466,-0.314062166312295,0.05));
#75883=CARTESIAN_POINT('',(0.389056494215466,-0.314062166312295,0.29));
#75884=CARTESIAN_POINT('',(0.367701332697109,-0.308538052649539,0.05));
#75885=CARTESIAN_POINT('Origin',(0.399482254061324,-0.338408583541644,0.05));
#75886=CARTESIAN_POINT('Origin',(0.,0.,0.05));
#75887=CARTESIAN_POINT('Origin',(0.245154869859355,-0.481143523061719,0.55));
#75888=CARTESIAN_POINT('',(0.241731905082157,-0.437682174717398,0.05));
#75889=CARTESIAN_POINT('',(0.241731905082157,-0.437682174717398,0.55));
#75890=CARTESIAN_POINT('',(0.241731905082157,-0.437682174717398,0.29));
#75891=CARTESIAN_POINT('',(0.24,-0.41569219381653,0.05));
#75892=CARTESIAN_POINT('',(0.245154869859355,-0.481143523061719,0.05));
#75893=CARTESIAN_POINT('',(0.24,-0.41569219381653,0.55));
#75894=CARTESIAN_POINT('',(0.24,-0.41569219381653,0.55));
#75895=CARTESIAN_POINT('',(0.245154869859355,-0.481143523061719,0.55));
#75896=CARTESIAN_POINT('Origin',(0.267052539454057,-0.448417858439125,0.55));
#75897=CARTESIAN_POINT('',(0.258177929547807,-0.428187058065056,0.55));
#75898=CARTESIAN_POINT('Origin',(0.,0.,0.55));
#75899=CARTESIAN_POINT('',(0.24,-0.41569219381653,0.55));
#75900=CARTESIAN_POINT('Origin',(0.24,-0.41569219381653,0.55));
#75901=CARTESIAN_POINT('',(0.258177929547807,-0.428187058065056,0.05));
#75902=CARTESIAN_POINT('',(0.258177929547807,-0.428187058065056,0.29));
#75903=CARTESIAN_POINT('',(0.24,-0.41569219381653,0.05));
#75904=CARTESIAN_POINT('Origin',(0.267052539454057,-0.448417858439125,0.05));
#75905=CARTESIAN_POINT('Origin',(0.,0.,0.05));
#75906=CARTESIAN_POINT('Origin',(0.0658094454387798,-0.535974921886314,
0.55));
#75907=CARTESIAN_POINT('',(0.0774575672862877,-0.493963890654054,0.05));
#75908=CARTESIAN_POINT('',(0.0774575672862877,-0.493963890654054,0.55));
#75909=CARTESIAN_POINT('',(0.0774575672862877,-0.493963890654054,0.29));
#75910=CARTESIAN_POINT('',(0.0833511252801264,-0.47270772144586,0.05));
#75911=CARTESIAN_POINT('',(0.0658094454387798,-0.535974921886314,0.05));
#75912=CARTESIAN_POINT('',(0.0833511252801264,-0.47270772144586,0.55));
#75913=CARTESIAN_POINT('',(0.0833511252801264,-0.47270772144586,0.55));
#75914=CARTESIAN_POINT('',(0.0658094454387798,-0.535974921886314,0.55));
#75915=CARTESIAN_POINT('Origin',(0.0936415073922334,-0.504341321666087,
0.55));
#75916=CARTESIAN_POINT('',(0.0961592962762517,-0.490666271247226,0.55));
#75917=CARTESIAN_POINT('Origin',(0.,0.,0.55));
#75918=CARTESIAN_POINT('',(0.0833511252801264,-0.47270772144586,0.55));
#75919=CARTESIAN_POINT('Origin',(0.0833511252801264,-0.47270772144586,0.55));
#75920=CARTESIAN_POINT('',(0.0961592962762517,-0.490666271247226,0.05));
#75921=CARTESIAN_POINT('',(0.0961592962762517,-0.490666271247226,0.29));
#75922=CARTESIAN_POINT('',(0.0833511252801264,-0.47270772144586,0.05));
#75923=CARTESIAN_POINT('Origin',(0.0936415073922334,-0.504341321666087,
0.05));
#75924=CARTESIAN_POINT('Origin',(0.,0.,0.05));
#75925=CARTESIAN_POINT('Origin',(-0.121473569345687,-0.526159834984027,
0.55));
#75926=CARTESIAN_POINT('',(-0.0961592962762519,-0.490666271247226,0.05));
#75927=CARTESIAN_POINT('',(-0.0961592962762519,-0.490666271247226,0.55));
#75928=CARTESIAN_POINT('',(-0.0961592962762519,-0.490666271247226,0.29));
#75929=CARTESIAN_POINT('',(-0.0833511252801266,-0.47270772144586,0.05));
#75930=CARTESIAN_POINT('',(-0.121473569345687,-0.526159834984027,0.05));
#75931=CARTESIAN_POINT('',(-0.0833511252801266,-0.47270772144586,0.55));
#75932=CARTESIAN_POINT('',(-0.0833511252801266,-0.47270772144586,0.55));
#75933=CARTESIAN_POINT('',(-0.121473569345687,-0.526159834984027,0.55));
#75934=CARTESIAN_POINT('Origin',(-0.0936415073922334,-0.504341321666087,
0.55));
#75935=CARTESIAN_POINT('',(-0.0774575672862877,-0.493963890654054,0.55));
#75936=CARTESIAN_POINT('Origin',(0.,0.,0.55));
#75937=CARTESIAN_POINT('',(-0.0833511252801266,-0.47270772144586,0.55));
#75938=CARTESIAN_POINT('Origin',(-0.0833511252801266,-0.47270772144586,
0.55));
#75939=CARTESIAN_POINT('',(-0.0774575672862877,-0.493963890654054,0.05));
#75940=CARTESIAN_POINT('',(-0.0774575672862877,-0.493963890654054,0.29));
#75941=CARTESIAN_POINT('',(-0.0833511252801266,-0.47270772144586,0.05));
#75942=CARTESIAN_POINT('Origin',(-0.0936415073922334,-0.504341321666087,
0.05));
#75943=CARTESIAN_POINT('Origin',(0.,0.,0.05));
#75944=CARTESIAN_POINT('Origin',(-0.294105078908115,-0.452882106690529,
0.55));
#75945=CARTESIAN_POINT('',(-0.258177929547807,-0.428187058065056,0.05));
#75946=CARTESIAN_POINT('',(-0.258177929547807,-0.428187058065056,0.55));
#75947=CARTESIAN_POINT('',(-0.258177929547807,-0.428187058065056,0.29));
#75948=CARTESIAN_POINT('',(-0.24,-0.41569219381653,0.05));
#75949=CARTESIAN_POINT('',(-0.294105078908115,-0.452882106690529,0.05));
#75950=CARTESIAN_POINT('',(-0.24,-0.41569219381653,0.55));
#75951=CARTESIAN_POINT('',(-0.24,-0.41569219381653,0.55));
#75952=CARTESIAN_POINT('',(-0.294105078908115,-0.452882106690529,0.55));
#75953=CARTESIAN_POINT('Origin',(-0.267052539454057,-0.448417858439125,
0.55));
#75954=CARTESIAN_POINT('',(-0.241731905082157,-0.437682174717398,0.55));
#75955=CARTESIAN_POINT('Origin',(0.,0.,0.55));
#75956=CARTESIAN_POINT('',(-0.24,-0.41569219381653,0.55));
#75957=CARTESIAN_POINT('Origin',(-0.24,-0.41569219381653,0.55));
#75958=CARTESIAN_POINT('',(-0.241731905082157,-0.437682174717398,0.05));
#75959=CARTESIAN_POINT('',(-0.241731905082157,-0.437682174717398,0.29));
#75960=CARTESIAN_POINT('',(-0.24,-0.41569219381653,0.05));
#75961=CARTESIAN_POINT('Origin',(-0.267052539454057,-0.448417858439125,
0.05));
#75962=CARTESIAN_POINT('Origin',(0.,0.,0.05));
#75963=CARTESIAN_POINT('Origin',(-0.431263175425538,-0.324980112502106,
0.55));
#75964=CARTESIAN_POINT('',(-0.389056494215466,-0.314062166312295,0.05));
#75965=CARTESIAN_POINT('',(-0.389056494215466,-0.314062166312295,0.55));
#75966=CARTESIAN_POINT('',(-0.389056494215466,-0.314062166312295,0.29));
#75967=CARTESIAN_POINT('',(-0.367701332697109,-0.308538052649539,0.05));
#75968=CARTESIAN_POINT('',(-0.431263175425538,-0.324980112502106,0.05));
#75969=CARTESIAN_POINT('',(-0.367701332697109,-0.308538052649539,0.55));
#75970=CARTESIAN_POINT('',(-0.367701332697109,-0.308538052649539,0.55));
#75971=CARTESIAN_POINT('',(-0.431263175425538,-0.324980112502106,0.55));
#75972=CARTESIAN_POINT('Origin',(-0.399482254061324,-0.338408583541644,
0.55));
#75973=CARTESIAN_POINT('',(-0.376849807542158,-0.328609529008881,0.55));
#75974=CARTESIAN_POINT('Origin',(0.,0.,0.55));
#75975=CARTESIAN_POINT('',(-0.367701332697109,-0.308538052649539,0.55));
#75976=CARTESIAN_POINT('Origin',(-0.367701332697109,-0.308538052649539,
0.55));
#75977=CARTESIAN_POINT('',(-0.376849807542158,-0.328609529008881,0.05));
#75978=CARTESIAN_POINT('',(-0.376849807542158,-0.328609529008881,0.29));
#75979=CARTESIAN_POINT('',(-0.367701332697109,-0.308538052649539,0.05));
#75980=CARTESIAN_POINT('Origin',(-0.399482254061324,-0.338408583541644,
0.05));
#75981=CARTESIAN_POINT('Origin',(0.,0.,0.05));
#75982=CARTESIAN_POINT('Origin',(-0.516404568220039,-0.157880720550278,
0.55));
#75983=CARTESIAN_POINT('',(-0.473009103818409,-0.162056742238344,0.05));
#75984=CARTESIAN_POINT('',(-0.473009103818409,-0.162056742238344,0.55));
#75985=CARTESIAN_POINT('',(-0.473009103818409,-0.162056742238344,0.29));
#75986=CARTESIAN_POINT('',(-0.451052457977236,-0.164169668796321,0.05));
#75987=CARTESIAN_POINT('',(-0.516404568220039,-0.157880720550278,0.05));
#75988=CARTESIAN_POINT('',(-0.451052457977236,-0.164169668796321,0.55));
#75989=CARTESIAN_POINT('',(-0.451052457977236,-0.164169668796321,0.55));
#75990=CARTESIAN_POINT('',(-0.516404568220039,-0.157880720550278,0.55));
#75991=CARTESIAN_POINT('Origin',(-0.483728513098638,-0.184437764967243,
0.55));
#75992=CARTESIAN_POINT('',(-0.466514061501753,-0.179901724341759,0.55));
#75993=CARTESIAN_POINT('Origin',(0.,0.,0.55));
#75994=CARTESIAN_POINT('',(-0.451052457977236,-0.164169668796321,0.55));
#75995=CARTESIAN_POINT('Origin',(-0.451052457977236,-0.164169668796321,
0.55));
#75996=CARTESIAN_POINT('',(-0.466514061501753,-0.179901724341759,0.05));
#75997=CARTESIAN_POINT('',(-0.466514061501753,-0.179901724341759,0.29));
#75998=CARTESIAN_POINT('',(-0.451052457977236,-0.164169668796321,0.05));
#75999=CARTESIAN_POINT('Origin',(-0.483728513098638,-0.184437764967243,
0.05));
#76000=CARTESIAN_POINT('Origin',(0.,0.,0.05));
#76001=CARTESIAN_POINT('Origin',(-0.53925994876747,0.0282614163711897,0.55));
#76002=CARTESIAN_POINT('',(-0.499909834629965,0.00949511665234234,0.05));
#76003=CARTESIAN_POINT('',(-0.499909834629965,0.00949511665234234,0.55));
#76004=CARTESIAN_POINT('',(-0.499909834629965,0.00949511665234234,0.29));
#76005=CARTESIAN_POINT('',(-0.48,5.87830463590729E-17,0.05));
#76006=CARTESIAN_POINT('',(-0.53925994876747,0.0282614163711897,0.05));
#76007=CARTESIAN_POINT('',(-0.48,5.87830463590729E-17,0.55));
#76008=CARTESIAN_POINT('',(-0.48,5.87830463590729E-17,0.55));
#76009=CARTESIAN_POINT('',(-0.53925994876747,0.0282614163711897,0.55));
#76010=CARTESIAN_POINT('Origin',(-0.509629974383735,6.59194920871187E-17,
0.55));
#76011=CARTESIAN_POINT('',(-0.5,-6.12323399573677E-17,0.55));
#76012=CARTESIAN_POINT('Origin',(0.,0.,0.55));
#76013=CARTESIAN_POINT('',(-0.499909834629965,-0.00949511665234226,0.55));
#76014=CARTESIAN_POINT('',(-0.48,5.87830463590729E-17,0.55));
#76015=CARTESIAN_POINT('Origin',(0.,0.,0.55));
#76016=CARTESIAN_POINT('Origin',(-0.48,5.87830463590729E-17,0.55));
#76017=CARTESIAN_POINT('',(-0.499909834629965,-0.00949511665234226,0.05));
#76018=CARTESIAN_POINT('',(-0.499909834629965,-0.00949511665234226,0.29));
#76019=CARTESIAN_POINT('',(-0.48,5.87830463590729E-17,0.05));
#76020=CARTESIAN_POINT('Origin',(-0.509629974383735,6.59194920871187E-17,
0.05));
#76021=CARTESIAN_POINT('',(-0.5,-6.12323399573677E-17,0.05));
#76022=CARTESIAN_POINT('Origin',(0.,0.,0.05));
#76023=CARTESIAN_POINT('Origin',(0.,0.,0.05));
#76024=CARTESIAN_POINT('Origin',(-0.526159834984027,0.121473569345687,0.55));
#76025=CARTESIAN_POINT('',(-0.490666271247226,0.0961592962762519,0.05));
#76026=CARTESIAN_POINT('',(-0.490666271247226,0.0961592962762519,0.55));
#76027=CARTESIAN_POINT('',(-0.490666271247226,0.0961592962762519,0.29));
#76028=CARTESIAN_POINT('',(-0.47270772144586,0.0833511252801265,0.05));
#76029=CARTESIAN_POINT('',(-0.526159834984027,0.121473569345687,0.05));
#76030=CARTESIAN_POINT('',(-0.47270772144586,0.0833511252801265,0.55));
#76031=CARTESIAN_POINT('',(-0.47270772144586,0.0833511252801265,0.55));
#76032=CARTESIAN_POINT('',(-0.526159834984027,0.121473569345687,0.55));
#76033=CARTESIAN_POINT('Origin',(-0.504341321666087,0.0936415073922334,
0.55));
#76034=CARTESIAN_POINT('',(-0.493963890654054,0.0774575672862877,0.55));
#76035=CARTESIAN_POINT('Origin',(0.,0.,0.55));
#76036=CARTESIAN_POINT('',(-0.47270772144586,0.0833511252801265,0.55));
#76037=CARTESIAN_POINT('Origin',(-0.47270772144586,0.0833511252801265,0.55));
#76038=CARTESIAN_POINT('',(-0.493963890654054,0.0774575672862877,0.05));
#76039=CARTESIAN_POINT('',(-0.493963890654054,0.0774575672862877,0.29));
#76040=CARTESIAN_POINT('',(-0.47270772144586,0.0833511252801265,0.05));
#76041=CARTESIAN_POINT('Origin',(-0.504341321666087,0.0936415073922334,
0.05));
#76042=CARTESIAN_POINT('Origin',(0.,0.,0.05));
#76043=CARTESIAN_POINT('Origin',(-0.452882106690529,0.294105078908115,0.55));
#76044=CARTESIAN_POINT('',(-0.428187058065056,0.258177929547807,0.05));
#76045=CARTESIAN_POINT('',(-0.428187058065056,0.258177929547807,0.55));
#76046=CARTESIAN_POINT('',(-0.428187058065056,0.258177929547807,0.29));
#76047=CARTESIAN_POINT('',(-0.415692193816531,0.24,0.05));
#76048=CARTESIAN_POINT('',(-0.452882106690529,0.294105078908115,0.05));
#76049=CARTESIAN_POINT('',(-0.415692193816531,0.24,0.55));
#76050=CARTESIAN_POINT('',(-0.415692193816531,0.24,0.55));
#76051=CARTESIAN_POINT('',(-0.452882106690529,0.294105078908115,0.55));
#76052=CARTESIAN_POINT('Origin',(-0.448417858439125,0.267052539454057,0.55));
#76053=CARTESIAN_POINT('',(-0.437682174717398,0.241731905082157,0.55));
#76054=CARTESIAN_POINT('Origin',(0.,0.,0.55));
#76055=CARTESIAN_POINT('',(-0.415692193816531,0.24,0.55));
#76056=CARTESIAN_POINT('Origin',(-0.415692193816531,0.24,0.55));
#76057=CARTESIAN_POINT('',(-0.437682174717398,0.241731905082157,0.05));
#76058=CARTESIAN_POINT('',(-0.437682174717398,0.241731905082157,0.29));
#76059=CARTESIAN_POINT('',(-0.415692193816531,0.24,0.05));
#76060=CARTESIAN_POINT('Origin',(-0.448417858439125,0.267052539454057,0.05));
#76061=CARTESIAN_POINT('Origin',(0.,0.,0.05));
#76062=CARTESIAN_POINT('Origin',(-0.324980112502106,0.431263175425538,0.55));
#76063=CARTESIAN_POINT('',(-0.314062166312295,0.389056494215465,0.05));
#76064=CARTESIAN_POINT('',(-0.314062166312295,0.389056494215465,0.55));
#76065=CARTESIAN_POINT('',(-0.314062166312295,0.389056494215465,0.29));
#76066=CARTESIAN_POINT('',(-0.308538052649539,0.367701332697109,0.05));
#76067=CARTESIAN_POINT('',(-0.324980112502106,0.431263175425538,0.05));
#76068=CARTESIAN_POINT('',(-0.308538052649539,0.367701332697109,0.55));
#76069=CARTESIAN_POINT('',(-0.308538052649539,0.367701332697109,0.55));
#76070=CARTESIAN_POINT('',(-0.324980112502106,0.431263175425538,0.55));
#76071=CARTESIAN_POINT('Origin',(-0.338408583541644,0.399482254061324,0.55));
#76072=CARTESIAN_POINT('',(-0.328609529008881,0.376849807542158,0.55));
#76073=CARTESIAN_POINT('Origin',(0.,0.,0.55));
#76074=CARTESIAN_POINT('',(-0.308538052649539,0.367701332697109,0.55));
#76075=CARTESIAN_POINT('Origin',(-0.308538052649539,0.367701332697109,0.55));
#76076=CARTESIAN_POINT('',(-0.328609529008881,0.376849807542158,0.05));
#76077=CARTESIAN_POINT('',(-0.328609529008881,0.376849807542158,0.29));
#76078=CARTESIAN_POINT('',(-0.308538052649539,0.367701332697109,0.05));
#76079=CARTESIAN_POINT('Origin',(-0.338408583541644,0.399482254061324,0.05));
#76080=CARTESIAN_POINT('Origin',(0.,0.,0.05));
#76081=CARTESIAN_POINT('Origin',(-0.157880720550278,0.516404568220039,0.55));
#76082=CARTESIAN_POINT('',(-0.162056742238344,0.473009103818409,0.05));
#76083=CARTESIAN_POINT('',(-0.162056742238344,0.473009103818409,0.55));
#76084=CARTESIAN_POINT('',(-0.162056742238344,0.473009103818409,0.29));
#76085=CARTESIAN_POINT('',(-0.164169668796321,0.451052457977236,0.05));
#76086=CARTESIAN_POINT('',(-0.157880720550278,0.516404568220039,0.05));
#76087=CARTESIAN_POINT('',(-0.164169668796321,0.451052457977236,0.55));
#76088=CARTESIAN_POINT('',(-0.164169668796321,0.451052457977236,0.55));
#76089=CARTESIAN_POINT('',(-0.157880720550278,0.516404568220039,0.55));
#76090=CARTESIAN_POINT('Origin',(-0.184437764967243,0.483728513098638,0.55));
#76091=CARTESIAN_POINT('',(-0.179901724341759,0.466514061501753,0.55));
#76092=CARTESIAN_POINT('Origin',(0.,0.,0.55));
#76093=CARTESIAN_POINT('',(-0.164169668796321,0.451052457977236,0.55));
#76094=CARTESIAN_POINT('Origin',(-0.164169668796321,0.451052457977236,0.55));
#76095=CARTESIAN_POINT('',(-0.179901724341759,0.466514061501753,0.05));
#76096=CARTESIAN_POINT('',(-0.179901724341759,0.466514061501753,0.29));
#76097=CARTESIAN_POINT('',(-0.164169668796321,0.451052457977236,0.05));
#76098=CARTESIAN_POINT('Origin',(-0.184437764967243,0.483728513098638,0.05));
#76099=CARTESIAN_POINT('Origin',(0.,0.,0.05));
#76100=CARTESIAN_POINT('Origin',(0.0282614163711897,0.53925994876747,0.55));
#76101=CARTESIAN_POINT('',(0.00949511665234237,0.499909834629964,0.05));
#76102=CARTESIAN_POINT('',(0.00949511665234237,0.499909834629964,0.55));
#76103=CARTESIAN_POINT('',(0.00949511665234237,0.499909834629964,0.29));
#76104=CARTESIAN_POINT('',(2.93915231795365E-17,0.48,0.05));
#76105=CARTESIAN_POINT('',(0.0282614163711897,0.53925994876747,0.05));
#76106=CARTESIAN_POINT('',(2.93915231795365E-17,0.48,0.55));
#76107=CARTESIAN_POINT('',(2.93915231795365E-17,0.48,0.55));
#76108=CARTESIAN_POINT('',(0.0282614163711897,0.53925994876747,0.55));
#76109=CARTESIAN_POINT('Origin',(3.46944695195361E-17,0.509629974383735,
0.55));
#76110=CARTESIAN_POINT('',(-0.00949511665234229,0.499909834629964,0.55));
#76111=CARTESIAN_POINT('Origin',(0.,0.,0.55));
#76112=CARTESIAN_POINT('',(2.93915231795365E-17,0.48,0.55));
#76113=CARTESIAN_POINT('Origin',(2.93915231795365E-17,0.48,0.55));
#76114=CARTESIAN_POINT('',(-0.00949511665234229,0.499909834629964,0.05));
#76115=CARTESIAN_POINT('',(-0.00949511665234229,0.499909834629964,0.29));
#76116=CARTESIAN_POINT('',(2.93915231795365E-17,0.48,0.05));
#76117=CARTESIAN_POINT('Origin',(3.46944695195361E-17,0.509629974383735,
0.05));
#76118=CARTESIAN_POINT('Origin',(0.,0.,0.05));
#76119=CARTESIAN_POINT('Origin',(0.210994809384208,0.497072620864318,0.55));
#76120=CARTESIAN_POINT('',(0.179901724341759,0.466514061501753,0.05));
#76121=CARTESIAN_POINT('',(0.179901724341759,0.466514061501753,0.55));
#76122=CARTESIAN_POINT('',(0.179901724341759,0.466514061501753,0.29));
#76123=CARTESIAN_POINT('',(0.164169668796321,0.451052457977236,0.05));
#76124=CARTESIAN_POINT('',(0.210994809384208,0.497072620864318,0.05));
#76125=CARTESIAN_POINT('',(0.164169668796321,0.451052457977236,0.55));
#76126=CARTESIAN_POINT('',(0.164169668796321,0.451052457977236,0.55));
#76127=CARTESIAN_POINT('',(0.210994809384208,0.497072620864318,0.55));
#76128=CARTESIAN_POINT('Origin',(0.184437764967243,0.483728513098638,0.55));
#76129=CARTESIAN_POINT('',(0.162056742238344,0.473009103818409,0.55));
#76130=CARTESIAN_POINT('Origin',(0.,0.,0.55));
#76131=CARTESIAN_POINT('',(0.164169668796321,0.451052457977236,0.55));
#76132=CARTESIAN_POINT('Origin',(0.164169668796321,0.451052457977236,0.55));
#76133=CARTESIAN_POINT('',(0.162056742238344,0.473009103818409,0.05));
#76134=CARTESIAN_POINT('',(0.162056742238344,0.473009103818409,0.29));
#76135=CARTESIAN_POINT('',(0.164169668796321,0.451052457977236,0.05));
#76136=CARTESIAN_POINT('Origin',(0.184437764967243,0.483728513098638,0.05));
#76137=CARTESIAN_POINT('Origin',(0.,0.,0.05));
#76138=CARTESIAN_POINT('Origin',(0.368279114433749,0.394930998874352,0.55));
#76139=CARTESIAN_POINT('',(0.328609529008881,0.376849807542157,0.05));
#76140=CARTESIAN_POINT('',(0.328609529008881,0.376849807542157,0.55));
#76141=CARTESIAN_POINT('',(0.328609529008881,0.376849807542157,0.29));
#76142=CARTESIAN_POINT('',(0.308538052649539,0.367701332697109,0.05));
#76143=CARTESIAN_POINT('',(0.368279114433749,0.394930998874352,0.05));
#76144=CARTESIAN_POINT('',(0.308538052649539,0.367701332697109,0.55));
#76145=CARTESIAN_POINT('',(0.308538052649539,0.367701332697109,0.55));
#76146=CARTESIAN_POINT('',(0.368279114433749,0.394930998874352,0.55));
#76147=CARTESIAN_POINT('Origin',(0.338408583541644,0.399482254061324,0.55));
#76148=CARTESIAN_POINT('',(0.314062166312295,0.389056494215466,0.55));
#76149=CARTESIAN_POINT('Origin',(0.,0.,0.55));
#76150=CARTESIAN_POINT('',(0.308538052649539,0.367701332697109,0.55));
#76151=CARTESIAN_POINT('Origin',(0.308538052649539,0.367701332697109,0.55));
#76152=CARTESIAN_POINT('',(0.314062166312295,0.389056494215466,0.05));
#76153=CARTESIAN_POINT('',(0.314062166312295,0.389056494215466,0.29));
#76154=CARTESIAN_POINT('',(0.308538052649539,0.367701332697109,0.05));
#76155=CARTESIAN_POINT('Origin',(0.338408583541644,0.399482254061324,0.05));
#76156=CARTESIAN_POINT('Origin',(0.,0.,0.05));
#76157=CARTESIAN_POINT('Origin',(0.481143523061719,0.245154869859355,0.55));
#76158=CARTESIAN_POINT('',(0.437682174717398,0.241731905082157,0.05));
#76159=CARTESIAN_POINT('',(0.437682174717398,0.241731905082157,0.55));
#76160=CARTESIAN_POINT('',(0.437682174717398,0.241731905082157,0.29));
#76161=CARTESIAN_POINT('',(0.415692193816531,0.24,0.05));
#76162=CARTESIAN_POINT('',(0.481143523061719,0.245154869859355,0.05));
#76163=CARTESIAN_POINT('',(0.415692193816531,0.24,0.55));
#76164=CARTESIAN_POINT('',(0.415692193816531,0.24,0.55));
#76165=CARTESIAN_POINT('',(0.481143523061719,0.245154869859355,0.55));
#76166=CARTESIAN_POINT('Origin',(0.448417858439125,0.267052539454057,0.55));
#76167=CARTESIAN_POINT('',(0.428187058065056,0.258177929547807,0.55));
#76168=CARTESIAN_POINT('Origin',(0.,0.,0.55));
#76169=CARTESIAN_POINT('',(0.415692193816531,0.24,0.55));
#76170=CARTESIAN_POINT('Origin',(0.415692193816531,0.24,0.55));
#76171=CARTESIAN_POINT('',(0.428187058065056,0.258177929547807,0.05));
#76172=CARTESIAN_POINT('',(0.428187058065056,0.258177929547807,0.29));
#76173=CARTESIAN_POINT('',(0.415692193816531,0.24,0.05));
#76174=CARTESIAN_POINT('Origin',(0.448417858439125,0.267052539454057,0.05));
#76175=CARTESIAN_POINT('Origin',(0.,0.,0.05));
#76176=CARTESIAN_POINT('Origin',(0.535974921886314,0.0658094454387796,0.55));
#76177=CARTESIAN_POINT('',(0.493963890654054,0.0774575672862878,0.05));
#76178=CARTESIAN_POINT('',(0.493963890654054,0.0774575672862878,0.55));
#76179=CARTESIAN_POINT('',(0.493963890654054,0.0774575672862878,0.29));
#76180=CARTESIAN_POINT('',(0.47270772144586,0.0833511252801266,0.05));
#76181=CARTESIAN_POINT('',(0.535974921886314,0.0658094454387796,0.05));
#76182=CARTESIAN_POINT('',(0.47270772144586,0.0833511252801266,0.55));
#76183=CARTESIAN_POINT('',(0.47270772144586,0.0833511252801266,0.55));
#76184=CARTESIAN_POINT('',(0.535974921886314,0.0658094454387796,0.55));
#76185=CARTESIAN_POINT('Origin',(0.504341321666087,0.0936415073922334,0.55));
#76186=CARTESIAN_POINT('',(0.490666271247226,0.0961592962762519,0.55));
#76187=CARTESIAN_POINT('Origin',(0.,0.,0.55));
#76188=CARTESIAN_POINT('',(0.47270772144586,0.0833511252801266,0.55));
#76189=CARTESIAN_POINT('Origin',(0.47270772144586,0.0833511252801266,0.55));
#76190=CARTESIAN_POINT('',(0.490666271247226,0.0961592962762519,0.05));
#76191=CARTESIAN_POINT('',(0.490666271247226,0.0961592962762519,0.29));
#76192=CARTESIAN_POINT('',(0.47270772144586,0.0833511252801266,0.05));
#76193=CARTESIAN_POINT('Origin',(0.504341321666087,0.0936415073922334,0.05));
#76194=CARTESIAN_POINT('Origin',(0.,0.,0.05));
#76195=CARTESIAN_POINT('Origin',(0.516404568220039,0.157880720550278,0.55));
#76196=CARTESIAN_POINT('',(0.473009103818409,0.162056742238344,0.05));
#76197=CARTESIAN_POINT('',(0.473009103818409,0.162056742238344,0.55));
#76198=CARTESIAN_POINT('',(0.473009103818409,0.162056742238344,0.29));
#76199=CARTESIAN_POINT('',(0.451052457977236,0.164169668796321,0.05));
#76200=CARTESIAN_POINT('',(0.516404568220039,0.157880720550278,0.05));
#76201=CARTESIAN_POINT('',(0.451052457977236,0.164169668796321,0.55));
#76202=CARTESIAN_POINT('',(0.451052457977236,0.164169668796321,0.55));
#76203=CARTESIAN_POINT('',(0.516404568220039,0.157880720550278,0.55));
#76204=CARTESIAN_POINT('Origin',(0.483728513098638,0.184437764967243,0.55));
#76205=CARTESIAN_POINT('',(0.466514061501753,0.179901724341759,0.55));
#76206=CARTESIAN_POINT('Origin',(0.,0.,0.55));
#76207=CARTESIAN_POINT('',(0.451052457977236,0.164169668796321,0.55));
#76208=CARTESIAN_POINT('Origin',(0.451052457977236,0.164169668796321,0.55));
#76209=CARTESIAN_POINT('',(0.466514061501753,0.179901724341759,0.05));
#76210=CARTESIAN_POINT('',(0.466514061501753,0.179901724341759,0.29));
#76211=CARTESIAN_POINT('',(0.451052457977236,0.164169668796321,0.05));
#76212=CARTESIAN_POINT('Origin',(0.483728513098638,0.184437764967243,0.05));
#76213=CARTESIAN_POINT('Origin',(0.,0.,0.05));
#76214=CARTESIAN_POINT('Origin',(0.431263175425538,0.324980112502106,0.55));
#76215=CARTESIAN_POINT('',(0.389056494215466,0.314062166312295,0.05));
#76216=CARTESIAN_POINT('',(0.389056494215466,0.314062166312295,0.55));
#76217=CARTESIAN_POINT('',(0.389056494215466,0.314062166312295,0.29));
#76218=CARTESIAN_POINT('',(0.367701332697109,0.308538052649539,0.05));
#76219=CARTESIAN_POINT('',(0.431263175425538,0.324980112502106,0.05));
#76220=CARTESIAN_POINT('',(0.367701332697109,0.308538052649539,0.55));
#76221=CARTESIAN_POINT('',(0.367701332697109,0.308538052649539,0.55));
#76222=CARTESIAN_POINT('',(0.431263175425538,0.324980112502106,0.55));
#76223=CARTESIAN_POINT('Origin',(0.399482254061324,0.338408583541644,0.55));
#76224=CARTESIAN_POINT('',(0.376849807542158,0.328609529008881,0.55));
#76225=CARTESIAN_POINT('Origin',(0.,0.,0.55));
#76226=CARTESIAN_POINT('',(0.367701332697109,0.308538052649539,0.55));
#76227=CARTESIAN_POINT('Origin',(0.367701332697109,0.308538052649539,0.55));
#76228=CARTESIAN_POINT('',(0.376849807542158,0.328609529008881,0.05));
#76229=CARTESIAN_POINT('',(0.376849807542158,0.328609529008881,0.29));
#76230=CARTESIAN_POINT('',(0.367701332697109,0.308538052649539,0.05));
#76231=CARTESIAN_POINT('Origin',(0.399482254061324,0.338408583541644,0.05));
#76232=CARTESIAN_POINT('Origin',(0.,0.,0.05));
#76233=CARTESIAN_POINT('Origin',(0.294105078908115,0.452882106690529,0.55));
#76234=CARTESIAN_POINT('',(0.258177929547807,0.428187058065056,0.05));
#76235=CARTESIAN_POINT('',(0.258177929547807,0.428187058065056,0.55));
#76236=CARTESIAN_POINT('',(0.258177929547807,0.428187058065056,0.29));
#76237=CARTESIAN_POINT('',(0.24,0.41569219381653,0.05));
#76238=CARTESIAN_POINT('',(0.294105078908115,0.452882106690529,0.05));
#76239=CARTESIAN_POINT('',(0.24,0.41569219381653,0.55));
#76240=CARTESIAN_POINT('',(0.24,0.41569219381653,0.55));
#76241=CARTESIAN_POINT('',(0.294105078908115,0.452882106690529,0.55));
#76242=CARTESIAN_POINT('Origin',(0.267052539454057,0.448417858439125,0.55));
#76243=CARTESIAN_POINT('',(0.241731905082157,0.437682174717398,0.55));
#76244=CARTESIAN_POINT('Origin',(0.,0.,0.55));
#76245=CARTESIAN_POINT('',(0.24,0.41569219381653,0.55));
#76246=CARTESIAN_POINT('Origin',(0.24,0.41569219381653,0.55));
#76247=CARTESIAN_POINT('',(0.241731905082157,0.437682174717398,0.05));
#76248=CARTESIAN_POINT('',(0.241731905082157,0.437682174717398,0.29));
#76249=CARTESIAN_POINT('',(0.24,0.41569219381653,0.05));
#76250=CARTESIAN_POINT('Origin',(0.267052539454057,0.448417858439125,0.05));
#76251=CARTESIAN_POINT('Origin',(0.,0.,0.05));
#76252=CARTESIAN_POINT('Origin',(0.121473569345687,0.526159834984027,0.55));
#76253=CARTESIAN_POINT('',(0.0961592962762519,0.490666271247226,0.05));
#76254=CARTESIAN_POINT('',(0.0961592962762519,0.490666271247226,0.55));
#76255=CARTESIAN_POINT('',(0.0961592962762519,0.490666271247226,0.29));
#76256=CARTESIAN_POINT('',(0.0833511252801266,0.47270772144586,0.05));
#76257=CARTESIAN_POINT('',(0.121473569345687,0.526159834984027,0.05));
#76258=CARTESIAN_POINT('',(0.0833511252801266,0.47270772144586,0.55));
#76259=CARTESIAN_POINT('',(0.0833511252801266,0.47270772144586,0.55));
#76260=CARTESIAN_POINT('',(0.121473569345687,0.526159834984027,0.55));
#76261=CARTESIAN_POINT('Origin',(0.0936415073922334,0.504341321666087,0.55));
#76262=CARTESIAN_POINT('',(0.0774575672862878,0.493963890654054,0.55));
#76263=CARTESIAN_POINT('Origin',(0.,0.,0.55));
#76264=CARTESIAN_POINT('',(0.0833511252801266,0.47270772144586,0.55));
#76265=CARTESIAN_POINT('Origin',(0.0833511252801266,0.47270772144586,0.55));
#76266=CARTESIAN_POINT('',(0.0774575672862878,0.493963890654054,0.05));
#76267=CARTESIAN_POINT('',(0.0774575672862878,0.493963890654054,0.29));
#76268=CARTESIAN_POINT('',(0.0833511252801266,0.47270772144586,0.05));
#76269=CARTESIAN_POINT('Origin',(0.0936415073922334,0.504341321666087,0.05));
#76270=CARTESIAN_POINT('Origin',(0.,0.,0.05));
#76271=CARTESIAN_POINT('Origin',(-0.0658094454387796,0.535974921886314,
0.55));
#76272=CARTESIAN_POINT('',(-0.0774575672862878,0.493963890654054,0.05));
#76273=CARTESIAN_POINT('',(-0.0774575672862878,0.493963890654054,0.55));
#76274=CARTESIAN_POINT('',(-0.0774575672862878,0.493963890654054,0.29));
#76275=CARTESIAN_POINT('',(-0.0833511252801265,0.47270772144586,0.05));
#76276=CARTESIAN_POINT('',(-0.0658094454387796,0.535974921886314,0.05));
#76277=CARTESIAN_POINT('',(-0.0833511252801265,0.47270772144586,0.55));
#76278=CARTESIAN_POINT('',(-0.0833511252801265,0.47270772144586,0.55));
#76279=CARTESIAN_POINT('',(-0.0658094454387796,0.535974921886314,0.55));
#76280=CARTESIAN_POINT('Origin',(-0.0936415073922333,0.504341321666087,
0.55));
#76281=CARTESIAN_POINT('',(-0.0961592962762518,0.490666271247226,0.55));
#76282=CARTESIAN_POINT('Origin',(0.,0.,0.55));
#76283=CARTESIAN_POINT('',(-0.0833511252801265,0.47270772144586,0.55));
#76284=CARTESIAN_POINT('Origin',(-0.0833511252801265,0.47270772144586,0.55));
#76285=CARTESIAN_POINT('',(-0.0961592962762518,0.490666271247226,0.05));
#76286=CARTESIAN_POINT('',(-0.0961592962762518,0.490666271247226,0.29));
#76287=CARTESIAN_POINT('',(-0.0833511252801265,0.47270772144586,0.05));
#76288=CARTESIAN_POINT('Origin',(-0.0936415073922333,0.504341321666087,
0.05));
#76289=CARTESIAN_POINT('Origin',(0.,0.,0.05));
#76290=CARTESIAN_POINT('Origin',(-0.245154869859355,0.481143523061719,0.55));
#76291=CARTESIAN_POINT('',(-0.241731905082157,0.437682174717398,0.05));
#76292=CARTESIAN_POINT('',(-0.241731905082157,0.437682174717398,0.55));
#76293=CARTESIAN_POINT('',(-0.241731905082157,0.437682174717398,0.29));
#76294=CARTESIAN_POINT('',(-0.24,0.415692193816531,0.05));
#76295=CARTESIAN_POINT('',(-0.245154869859355,0.481143523061719,0.05));
#76296=CARTESIAN_POINT('',(-0.24,0.415692193816531,0.55));
#76297=CARTESIAN_POINT('',(-0.24,0.415692193816531,0.55));
#76298=CARTESIAN_POINT('',(-0.245154869859355,0.481143523061719,0.55));
#76299=CARTESIAN_POINT('Origin',(-0.267052539454057,0.448417858439125,0.55));
#76300=CARTESIAN_POINT('',(-0.258177929547807,0.428187058065056,0.55));
#76301=CARTESIAN_POINT('Origin',(0.,0.,0.55));
#76302=CARTESIAN_POINT('',(-0.24,0.415692193816531,0.55));
#76303=CARTESIAN_POINT('Origin',(-0.24,0.415692193816531,0.55));
#76304=CARTESIAN_POINT('',(-0.258177929547807,0.428187058065056,0.05));
#76305=CARTESIAN_POINT('',(-0.258177929547807,0.428187058065056,0.29));
#76306=CARTESIAN_POINT('',(-0.24,0.415692193816531,0.05));
#76307=CARTESIAN_POINT('Origin',(-0.267052539454057,0.448417858439125,0.05));
#76308=CARTESIAN_POINT('Origin',(0.,0.,0.05));
#76309=CARTESIAN_POINT('Origin',(-0.394930998874352,0.368279114433749,0.55));
#76310=CARTESIAN_POINT('',(-0.376849807542157,0.328609529008881,0.05));
#76311=CARTESIAN_POINT('',(-0.376849807542157,0.328609529008881,0.55));
#76312=CARTESIAN_POINT('',(-0.376849807542157,0.328609529008881,0.29));
#76313=CARTESIAN_POINT('',(-0.367701332697109,0.308538052649539,0.05));
#76314=CARTESIAN_POINT('',(-0.394930998874352,0.368279114433749,0.05));
#76315=CARTESIAN_POINT('',(-0.367701332697109,0.308538052649539,0.55));
#76316=CARTESIAN_POINT('',(-0.367701332697109,0.308538052649539,0.55));
#76317=CARTESIAN_POINT('',(-0.394930998874352,0.368279114433749,0.55));
#76318=CARTESIAN_POINT('Origin',(-0.399482254061324,0.338408583541644,0.55));
#76319=CARTESIAN_POINT('',(-0.389056494215466,0.314062166312295,0.55));
#76320=CARTESIAN_POINT('Origin',(0.,0.,0.55));
#76321=CARTESIAN_POINT('',(-0.367701332697109,0.308538052649539,0.55));
#76322=CARTESIAN_POINT('Origin',(-0.367701332697109,0.308538052649539,0.55));
#76323=CARTESIAN_POINT('',(-0.389056494215466,0.314062166312295,0.05));
#76324=CARTESIAN_POINT('',(-0.389056494215466,0.314062166312295,0.29));
#76325=CARTESIAN_POINT('',(-0.367701332697109,0.308538052649539,0.05));
#76326=CARTESIAN_POINT('Origin',(-0.399482254061324,0.338408583541644,0.05));
#76327=CARTESIAN_POINT('Origin',(0.,0.,0.05));
#76328=CARTESIAN_POINT('Origin',(-0.497072620864318,0.210994809384208,0.55));
#76329=CARTESIAN_POINT('',(-0.466514061501753,0.179901724341759,0.05));
#76330=CARTESIAN_POINT('',(-0.466514061501753,0.179901724341759,0.55));
#76331=CARTESIAN_POINT('',(-0.466514061501753,0.179901724341759,0.29));
#76332=CARTESIAN_POINT('',(-0.451052457977236,0.164169668796321,0.05));
#76333=CARTESIAN_POINT('',(-0.497072620864318,0.210994809384208,0.05));
#76334=CARTESIAN_POINT('',(-0.451052457977236,0.164169668796321,0.55));
#76335=CARTESIAN_POINT('',(-0.451052457977236,0.164169668796321,0.55));
#76336=CARTESIAN_POINT('',(-0.497072620864318,0.210994809384208,0.55));
#76337=CARTESIAN_POINT('Origin',(-0.483728513098638,0.184437764967243,0.55));
#76338=CARTESIAN_POINT('',(-0.473009103818409,0.162056742238344,0.55));
#76339=CARTESIAN_POINT('Origin',(0.,0.,0.55));
#76340=CARTESIAN_POINT('',(-0.451052457977236,0.164169668796321,0.55));
#76341=CARTESIAN_POINT('Origin',(-0.451052457977236,0.164169668796321,0.55));
#76342=CARTESIAN_POINT('',(-0.473009103818409,0.162056742238344,0.05));
#76343=CARTESIAN_POINT('',(-0.473009103818409,0.162056742238344,0.29));
#76344=CARTESIAN_POINT('',(-0.451052457977236,0.164169668796321,0.05));
#76345=CARTESIAN_POINT('Origin',(-0.483728513098638,0.184437764967243,0.05));
#76346=CARTESIAN_POINT('Origin',(0.,0.,0.05));
#76347=CARTESIAN_POINT('Origin',(0.509629974383735,0.,0.55));
#76348=CARTESIAN_POINT('',(0.499909834629964,-0.00949511665234232,0.55));
#76349=CARTESIAN_POINT('',(0.499909834629965,0.00949511665234234,0.55));
#76350=CARTESIAN_POINT('Origin',(0.,0.,0.55));
#76351=CARTESIAN_POINT('',(0.48,0.,0.55));
#76352=CARTESIAN_POINT('',(0.53925994876747,-0.0282614163711897,0.55));
#76353=CARTESIAN_POINT('',(0.48,0.,0.55));
#76354=CARTESIAN_POINT('Origin',(0.53925994876747,-0.0282614163711897,0.55));
#76355=CARTESIAN_POINT('',(0.499909834629964,-0.00949511665234232,0.05));
#76356=CARTESIAN_POINT('',(0.499909834629964,-0.00949511665234232,0.29));
#76357=CARTESIAN_POINT('',(0.48,0.,0.05));
#76358=CARTESIAN_POINT('',(0.53925994876747,-0.0282614163711897,0.05));
#76359=CARTESIAN_POINT('',(0.48,0.,0.55));
#76360=CARTESIAN_POINT('Origin',(0.48,0.,0.55));
#76361=CARTESIAN_POINT('',(0.499909834629965,0.00949511665234234,0.05));
#76362=CARTESIAN_POINT('',(0.499909834629965,0.00949511665234234,0.29));
#76363=CARTESIAN_POINT('',(0.48,0.,0.05));
#76364=CARTESIAN_POINT('Origin',(0.509629974383735,0.,0.05));
#76365=CARTESIAN_POINT('Origin',(0.,0.,0.05));
#76366=CARTESIAN_POINT('Origin',(-0.535974921886314,-0.0658094454387796,
0.55));
#76367=CARTESIAN_POINT('',(-0.493963890654054,-0.0774575672862878,0.05));
#76368=CARTESIAN_POINT('',(-0.493963890654054,-0.0774575672862878,0.55));
#76369=CARTESIAN_POINT('',(-0.493963890654054,-0.0774575672862878,0.29));
#76370=CARTESIAN_POINT('',(-0.47270772144586,-0.0833511252801266,0.05));
#76371=CARTESIAN_POINT('',(-0.535974921886314,-0.0658094454387796,0.05));
#76372=CARTESIAN_POINT('',(-0.47270772144586,-0.0833511252801266,0.55));
#76373=CARTESIAN_POINT('',(-0.47270772144586,-0.0833511252801266,0.55));
#76374=CARTESIAN_POINT('',(-0.535974921886314,-0.0658094454387796,0.55));
#76375=CARTESIAN_POINT('Origin',(-0.504341321666087,-0.0936415073922333,
0.55));
#76376=CARTESIAN_POINT('',(-0.490666271247226,-0.0961592962762519,0.55));
#76377=CARTESIAN_POINT('Origin',(0.,0.,0.55));
#76378=CARTESIAN_POINT('',(-0.47270772144586,-0.0833511252801266,0.55));
#76379=CARTESIAN_POINT('Origin',(-0.47270772144586,-0.0833511252801266,
0.55));
#76380=CARTESIAN_POINT('',(-0.490666271247226,-0.0961592962762519,0.05));
#76381=CARTESIAN_POINT('',(-0.490666271247226,-0.0961592962762519,0.29));
#76382=CARTESIAN_POINT('',(-0.47270772144586,-0.0833511252801266,0.05));
#76383=CARTESIAN_POINT('Origin',(-0.504341321666087,-0.0936415073922333,
0.05));
#76384=CARTESIAN_POINT('Origin',(0.,0.,0.05));
#76385=CARTESIAN_POINT('Origin',(-0.481143523061719,-0.245154869859355,
0.55));
#76386=CARTESIAN_POINT('',(-0.437682174717398,-0.241731905082157,0.05));
#76387=CARTESIAN_POINT('',(-0.437682174717398,-0.241731905082157,0.55));
#76388=CARTESIAN_POINT('',(-0.437682174717398,-0.241731905082157,0.29));
#76389=CARTESIAN_POINT('',(-0.41569219381653,-0.24,0.05));
#76390=CARTESIAN_POINT('',(-0.481143523061719,-0.245154869859355,0.05));
#76391=CARTESIAN_POINT('',(-0.41569219381653,-0.24,0.55));
#76392=CARTESIAN_POINT('',(-0.41569219381653,-0.24,0.55));
#76393=CARTESIAN_POINT('',(-0.481143523061719,-0.245154869859355,0.55));
#76394=CARTESIAN_POINT('Origin',(-0.448417858439125,-0.267052539454057,
0.55));
#76395=CARTESIAN_POINT('',(-0.428187058065056,-0.258177929547807,0.55));
#76396=CARTESIAN_POINT('Origin',(0.,0.,0.55));
#76397=CARTESIAN_POINT('',(-0.41569219381653,-0.24,0.55));
#76398=CARTESIAN_POINT('Origin',(-0.41569219381653,-0.24,0.55));
#76399=CARTESIAN_POINT('',(-0.428187058065056,-0.258177929547807,0.05));
#76400=CARTESIAN_POINT('',(-0.428187058065056,-0.258177929547807,0.29));
#76401=CARTESIAN_POINT('',(-0.41569219381653,-0.24,0.05));
#76402=CARTESIAN_POINT('Origin',(-0.448417858439125,-0.267052539454057,
0.05));
#76403=CARTESIAN_POINT('Origin',(0.,0.,0.05));
#76404=CARTESIAN_POINT('Origin',(-0.368279114433749,-0.394930998874352,
0.55));
#76405=CARTESIAN_POINT('',(-0.328609529008881,-0.376849807542157,0.05));
#76406=CARTESIAN_POINT('',(-0.328609529008881,-0.376849807542157,0.55));
#76407=CARTESIAN_POINT('',(-0.328609529008881,-0.376849807542157,0.29));
#76408=CARTESIAN_POINT('',(-0.308538052649539,-0.367701332697109,0.05));
#76409=CARTESIAN_POINT('',(-0.368279114433749,-0.394930998874352,0.05));
#76410=CARTESIAN_POINT('',(-0.308538052649539,-0.367701332697109,0.55));
#76411=CARTESIAN_POINT('',(-0.308538052649539,-0.367701332697109,0.55));
#76412=CARTESIAN_POINT('',(-0.368279114433749,-0.394930998874352,0.55));
#76413=CARTESIAN_POINT('Origin',(-0.338408583541644,-0.399482254061324,
0.55));
#76414=CARTESIAN_POINT('',(-0.314062166312295,-0.389056494215465,0.55));
#76415=CARTESIAN_POINT('Origin',(0.,0.,0.55));
#76416=CARTESIAN_POINT('',(-0.308538052649539,-0.367701332697109,0.55));
#76417=CARTESIAN_POINT('Origin',(-0.308538052649539,-0.367701332697109,
0.55));
#76418=CARTESIAN_POINT('',(-0.314062166312295,-0.389056494215465,0.05));
#76419=CARTESIAN_POINT('',(-0.314062166312295,-0.389056494215465,0.29));
#76420=CARTESIAN_POINT('',(-0.308538052649539,-0.367701332697109,0.05));
#76421=CARTESIAN_POINT('Origin',(-0.338408583541644,-0.399482254061324,
0.05));
#76422=CARTESIAN_POINT('Origin',(0.,0.,0.05));
#76423=CARTESIAN_POINT('Origin',(-0.210994809384208,-0.497072620864318,
0.55));
#76424=CARTESIAN_POINT('',(-0.179901724341759,-0.466514061501753,0.05));
#76425=CARTESIAN_POINT('',(-0.179901724341759,-0.466514061501753,0.55));
#76426=CARTESIAN_POINT('',(-0.179901724341759,-0.466514061501753,0.29));
#76427=CARTESIAN_POINT('',(-0.164169668796321,-0.451052457977236,0.05));
#76428=CARTESIAN_POINT('',(-0.210994809384208,-0.497072620864318,0.05));
#76429=CARTESIAN_POINT('',(-0.164169668796321,-0.451052457977236,0.55));
#76430=CARTESIAN_POINT('',(-0.164169668796321,-0.451052457977236,0.55));
#76431=CARTESIAN_POINT('',(-0.210994809384208,-0.497072620864318,0.55));
#76432=CARTESIAN_POINT('Origin',(-0.184437764967243,-0.483728513098638,
0.55));
#76433=CARTESIAN_POINT('',(-0.162056742238344,-0.473009103818409,0.55));
#76434=CARTESIAN_POINT('Origin',(0.,0.,0.55));
#76435=CARTESIAN_POINT('',(-0.164169668796321,-0.451052457977236,0.55));
#76436=CARTESIAN_POINT('Origin',(-0.164169668796321,-0.451052457977236,
0.55));
#76437=CARTESIAN_POINT('',(-0.162056742238344,-0.473009103818409,0.05));
#76438=CARTESIAN_POINT('',(-0.162056742238344,-0.473009103818409,0.29));
#76439=CARTESIAN_POINT('',(-0.164169668796321,-0.451052457977236,0.05));
#76440=CARTESIAN_POINT('Origin',(-0.184437764967243,-0.483728513098638,
0.05));
#76441=CARTESIAN_POINT('Origin',(0.,0.,0.05));
#76442=CARTESIAN_POINT('Origin',(-0.0282614163711899,-0.53925994876747,
0.55));
#76443=CARTESIAN_POINT('',(-0.00949511665234243,-0.499909834629964,0.05));
#76444=CARTESIAN_POINT('',(-0.00949511665234243,-0.499909834629964,0.55));
#76445=CARTESIAN_POINT('',(-0.00949511665234243,-0.499909834629964,0.29));
#76446=CARTESIAN_POINT('',(-8.81745695386094E-17,-0.48,0.05));
#76447=CARTESIAN_POINT('',(-0.0282614163711899,-0.53925994876747,0.05));
#76448=CARTESIAN_POINT('',(-8.81745695386094E-17,-0.48,0.55));
#76449=CARTESIAN_POINT('',(-8.81745695386094E-17,-0.48,0.55));
#76450=CARTESIAN_POINT('',(-0.0282614163711899,-0.53925994876747,0.55));
#76451=CARTESIAN_POINT('Origin',(-9.71445146547012E-17,-0.509629974383735,
0.55));
#76452=CARTESIAN_POINT('',(0.00949511665234229,-0.499909834629964,0.55));
#76453=CARTESIAN_POINT('Origin',(0.,0.,0.55));
#76454=CARTESIAN_POINT('',(-8.81745695386094E-17,-0.48,0.55));
#76455=CARTESIAN_POINT('Origin',(-8.81745695386094E-17,-0.48,0.55));
#76456=CARTESIAN_POINT('',(0.00949511665234229,-0.499909834629964,0.05));
#76457=CARTESIAN_POINT('',(0.00949511665234229,-0.499909834629964,0.29));
#76458=CARTESIAN_POINT('',(-8.81745695386094E-17,-0.48,0.05));
#76459=CARTESIAN_POINT('Origin',(-9.71445146547012E-17,-0.509629974383735,
0.05));
#76460=CARTESIAN_POINT('Origin',(0.,0.,0.05));
#76461=CARTESIAN_POINT('Origin',(0.157880720550278,-0.516404568220039,0.55));
#76462=CARTESIAN_POINT('',(0.162056742238344,-0.473009103818409,0.05));
#76463=CARTESIAN_POINT('',(0.162056742238344,-0.473009103818409,0.55));
#76464=CARTESIAN_POINT('',(0.162056742238344,-0.473009103818409,0.29));
#76465=CARTESIAN_POINT('',(0.164169668796321,-0.451052457977236,0.05));
#76466=CARTESIAN_POINT('',(0.157880720550278,-0.516404568220039,0.05));
#76467=CARTESIAN_POINT('',(0.164169668796321,-0.451052457977236,0.55));
#76468=CARTESIAN_POINT('',(0.164169668796321,-0.451052457977236,0.55));
#76469=CARTESIAN_POINT('',(0.157880720550278,-0.516404568220039,0.55));
#76470=CARTESIAN_POINT('Origin',(0.184437764967243,-0.483728513098638,0.55));
#76471=CARTESIAN_POINT('',(0.179901724341759,-0.466514061501753,0.55));
#76472=CARTESIAN_POINT('Origin',(0.,0.,0.55));
#76473=CARTESIAN_POINT('',(0.164169668796321,-0.451052457977236,0.55));
#76474=CARTESIAN_POINT('Origin',(0.164169668796321,-0.451052457977236,0.55));
#76475=CARTESIAN_POINT('',(0.179901724341759,-0.466514061501753,0.05));
#76476=CARTESIAN_POINT('',(0.179901724341759,-0.466514061501753,0.29));
#76477=CARTESIAN_POINT('',(0.164169668796321,-0.451052457977236,0.05));
#76478=CARTESIAN_POINT('Origin',(0.184437764967243,-0.483728513098638,0.05));
#76479=CARTESIAN_POINT('Origin',(0.,0.,0.05));
#76480=CARTESIAN_POINT('Origin',(0.324980112502106,-0.431263175425538,0.55));
#76481=CARTESIAN_POINT('',(0.314062166312295,-0.389056494215466,0.05));
#76482=CARTESIAN_POINT('',(0.314062166312295,-0.389056494215466,0.55));
#76483=CARTESIAN_POINT('',(0.314062166312295,-0.389056494215466,0.29));
#76484=CARTESIAN_POINT('',(0.308538052649539,-0.367701332697109,0.05));
#76485=CARTESIAN_POINT('',(0.324980112502106,-0.431263175425538,0.05));
#76486=CARTESIAN_POINT('',(0.308538052649539,-0.367701332697109,0.55));
#76487=CARTESIAN_POINT('',(0.308538052649539,-0.367701332697109,0.55));
#76488=CARTESIAN_POINT('',(0.324980112502106,-0.431263175425538,0.55));
#76489=CARTESIAN_POINT('Origin',(0.338408583541644,-0.399482254061324,0.55));
#76490=CARTESIAN_POINT('',(0.328609529008881,-0.376849807542158,0.55));
#76491=CARTESIAN_POINT('Origin',(0.,0.,0.55));
#76492=CARTESIAN_POINT('',(0.308538052649539,-0.367701332697109,0.55));
#76493=CARTESIAN_POINT('Origin',(0.308538052649539,-0.367701332697109,0.55));
#76494=CARTESIAN_POINT('',(0.328609529008881,-0.376849807542158,0.05));
#76495=CARTESIAN_POINT('',(0.328609529008881,-0.376849807542158,0.29));
#76496=CARTESIAN_POINT('',(0.308538052649539,-0.367701332697109,0.05));
#76497=CARTESIAN_POINT('Origin',(0.338408583541644,-0.399482254061324,0.05));
#76498=CARTESIAN_POINT('Origin',(0.,0.,0.05));
#76499=CARTESIAN_POINT('Origin',(0.452882106690529,-0.294105078908115,0.55));
#76500=CARTESIAN_POINT('',(0.428187058065056,-0.258177929547807,0.05));
#76501=CARTESIAN_POINT('',(0.428187058065056,-0.258177929547807,0.55));
#76502=CARTESIAN_POINT('',(0.428187058065056,-0.258177929547807,0.29));
#76503=CARTESIAN_POINT('',(0.41569219381653,-0.24,0.05));
#76504=CARTESIAN_POINT('',(0.452882106690529,-0.294105078908115,0.05));
#76505=CARTESIAN_POINT('',(0.41569219381653,-0.24,0.55));
#76506=CARTESIAN_POINT('',(0.41569219381653,-0.24,0.55));
#76507=CARTESIAN_POINT('',(0.452882106690529,-0.294105078908115,0.55));
#76508=CARTESIAN_POINT('Origin',(0.448417858439125,-0.267052539454057,0.55));
#76509=CARTESIAN_POINT('',(0.437682174717398,-0.241731905082157,0.55));
#76510=CARTESIAN_POINT('Origin',(0.,0.,0.55));
#76511=CARTESIAN_POINT('',(0.41569219381653,-0.24,0.55));
#76512=CARTESIAN_POINT('Origin',(0.41569219381653,-0.24,0.55));
#76513=CARTESIAN_POINT('',(0.437682174717398,-0.241731905082157,0.05));
#76514=CARTESIAN_POINT('',(0.437682174717398,-0.241731905082157,0.29));
#76515=CARTESIAN_POINT('',(0.41569219381653,-0.24,0.05));
#76516=CARTESIAN_POINT('Origin',(0.448417858439125,-0.267052539454057,0.05));
#76517=CARTESIAN_POINT('Origin',(0.,0.,0.05));
#76518=CARTESIAN_POINT('Origin',(0.526159834984027,-0.121473569345687,0.55));
#76519=CARTESIAN_POINT('',(0.490666271247226,-0.096159296276252,0.05));
#76520=CARTESIAN_POINT('',(0.490666271247226,-0.096159296276252,0.55));
#76521=CARTESIAN_POINT('',(0.490666271247226,-0.096159296276252,0.29));
#76522=CARTESIAN_POINT('',(0.47270772144586,-0.0833511252801266,0.05));
#76523=CARTESIAN_POINT('',(0.526159834984027,-0.121473569345687,0.05));
#76524=CARTESIAN_POINT('',(0.47270772144586,-0.0833511252801266,0.55));
#76525=CARTESIAN_POINT('',(0.47270772144586,-0.0833511252801266,0.55));
#76526=CARTESIAN_POINT('',(0.526159834984027,-0.121473569345687,0.55));
#76527=CARTESIAN_POINT('Origin',(0.504341321666087,-0.0936415073922334,
0.55));
#76528=CARTESIAN_POINT('',(0.493963890654054,-0.0774575672862878,0.55));
#76529=CARTESIAN_POINT('Origin',(0.,0.,0.55));
#76530=CARTESIAN_POINT('',(0.47270772144586,-0.0833511252801266,0.55));
#76531=CARTESIAN_POINT('Origin',(0.47270772144586,-0.0833511252801266,0.55));
#76532=CARTESIAN_POINT('',(0.493963890654054,-0.0774575672862878,0.05));
#76533=CARTESIAN_POINT('',(0.493963890654054,-0.0774575672862878,0.29));
#76534=CARTESIAN_POINT('',(0.47270772144586,-0.0833511252801266,0.05));
#76535=CARTESIAN_POINT('Origin',(0.504341321666087,-0.0936415073922334,
0.05));
#76536=CARTESIAN_POINT('Origin',(0.,0.,0.05));
#76537=CARTESIAN_POINT('Origin',(0.25,0.,-2.));
#76538=CARTESIAN_POINT('',(-0.25,-3.06161699786838E-17,-2.));
#76539=CARTESIAN_POINT('Origin',(0.,0.,-2.));
#76540=CARTESIAN_POINT('Origin',(0.,0.,-1.975));
#76541=CARTESIAN_POINT('',(-0.275,-3.36777869765522E-17,-1.975));
#76542=CARTESIAN_POINT('Origin',(0.,0.,0.015));
#76543=CARTESIAN_POINT('',(-0.5,-6.12323399573677E-17,0.03));
#76544=CARTESIAN_POINT('Origin',(0.,0.,0.03));
#76545=CARTESIAN_POINT('',(-0.485,-5.93953697586466E-17,0.015));
#76546=CARTESIAN_POINT('Origin',(0.,0.,0.29));
#76547=CARTESIAN_POINT('Origin',(0.,0.,0.55));
#76548=CARTESIAN_POINT('Origin',(0.,0.,0.55));
#76549=CARTESIAN_POINT('Origin',(0.,0.,0.55));
#76550=CARTESIAN_POINT('Origin',(0.,0.,0.55));
#76551=CARTESIAN_POINT('Origin',(0.,0.,0.55));
#76552=CARTESIAN_POINT('Origin',(0.,0.,0.55));
#76553=CARTESIAN_POINT('Origin',(0.,0.,0.55));
#76554=CARTESIAN_POINT('Origin',(0.,0.,0.55));
#76555=CARTESIAN_POINT('Origin',(0.,0.,0.55));
#76556=CARTESIAN_POINT('Origin',(0.,0.,0.55));
#76557=CARTESIAN_POINT('Origin',(0.,0.,0.55));
#76558=CARTESIAN_POINT('Origin',(0.,0.,0.55));
#76559=CARTESIAN_POINT('Origin',(0.,0.,0.55));
#76560=CARTESIAN_POINT('Origin',(0.,0.,0.55));
#76561=CARTESIAN_POINT('Origin',(0.,0.,0.55));
#76562=CARTESIAN_POINT('Origin',(0.,0.,0.55));
#76563=CARTESIAN_POINT('',(-0.5,-6.12323399573677E-17,0.29));
#76564=CARTESIAN_POINT('Origin',(0.,0.,0.55));
#76565=CARTESIAN_POINT('Origin',(0.,0.,0.55));
#76566=CARTESIAN_POINT('Origin',(0.,0.,0.55));
#76567=CARTESIAN_POINT('Origin',(0.,0.,0.55));
#76568=CARTESIAN_POINT('Origin',(0.,0.,0.55));
#76569=CARTESIAN_POINT('Origin',(0.,0.,0.55));
#76570=CARTESIAN_POINT('Origin',(0.,0.,0.55));
#76571=CARTESIAN_POINT('Origin',(0.,0.,0.55));
#76572=CARTESIAN_POINT('Origin',(0.,0.,0.55));
#76573=CARTESIAN_POINT('Origin',(0.,0.,0.55));
#76574=CARTESIAN_POINT('Origin',(0.,0.,0.55));
#76575=CARTESIAN_POINT('Origin',(0.,0.,0.55));
#76576=CARTESIAN_POINT('Origin',(0.,0.,0.55));
#76577=CARTESIAN_POINT('Origin',(0.,0.,0.55));
#76578=CARTESIAN_POINT('Origin',(0.,0.,0.55));
#76579=CARTESIAN_POINT('Origin',(0.,0.,0.55));
#76580=CARTESIAN_POINT('Origin',(0.,0.,0.55));
#76581=CARTESIAN_POINT('Origin',(0.,0.,0.55));
#76582=CARTESIAN_POINT('Origin',(0.,0.,0.55));
#76583=CARTESIAN_POINT('Origin',(0.,0.,0.55));
#76584=CARTESIAN_POINT('Origin',(0.,0.,0.575));
#76585=CARTESIAN_POINT('',(-0.45,-5.51091059616309E-17,0.6));
#76586=CARTESIAN_POINT('Origin',(0.,0.,0.6));
#76587=CARTESIAN_POINT('',(-0.475,-5.81707229594993E-17,0.575));
#76588=CARTESIAN_POINT('Origin',(0.,0.,0.6));
#76589=CARTESIAN_POINT('',(0.,0.,0.));
#76590=CARTESIAN_POINT('',(0.,0.,0.));
#76591=CARTESIAN_POINT('',(0.,0.,0.));
#76592=CARTESIAN_POINT('',(0.,0.,0.));
#76593=CARTESIAN_POINT('',(0.,0.,0.));
#76594=CARTESIAN_POINT('',(0.,0.,0.));
#76595=CARTESIAN_POINT('',(0.,0.,0.));
#76596=CARTESIAN_POINT('',(0.,0.,0.));
#76597=CARTESIAN_POINT('',(0.,0.,0.));
#76598=CARTESIAN_POINT('',(0.799999999999999,-1.06581410364015E-14,26.5));
#76599=CARTESIAN_POINT('',(0.,0.,0.));
#76600=CARTESIAN_POINT('',(50.2499999999998,-29.0118510267784,0.));
#76601=CARTESIAN_POINT('',(0.,0.,0.));
#76602=CARTESIAN_POINT('',(34.5,0.,21.2));
#76603=CARTESIAN_POINT('',(20.,15.2,5.2));
#76604=CARTESIAN_POINT('',(0.,0.,0.));
#76605=CARTESIAN_POINT('',(33.6,0.,4.2));
#76606=CARTESIAN_POINT('',(0.,0.,0.));
#76607=CARTESIAN_POINT('',(11.,9.2,6.2));
#76608=CARTESIAN_POINT('',(6.79999999999993,3.53553390593274,30.0355339059327));
#76609=CARTESIAN_POINT('',(13.8,0.,0.));
#76610=CARTESIAN_POINT('',(20.,-15.2,5.2));
#76611=CARTESIAN_POINT('',(11.,-9.2,6.2));
#76612=CARTESIAN_POINT('',(29.,9.2,6.2));
#76613=CARTESIAN_POINT('',(29.,-9.2,6.2));
#76614=CARTESIAN_POINT('',(6.79999999999993,-3.53553390593274,30.0355339059327));
#76615=CARTESIAN_POINT('',(6.79999999999993,-3.53553390593274,22.9644660940675));
#76616=CARTESIAN_POINT('',(6.79999999999993,3.53553390593274,22.9644660940675));
#76617=UNCERTAINTY_MEASURE_WITH_UNIT(LENGTH_MEASURE(0.001),#76661,
'DISTANCE_ACCURACY_VALUE',
'Maximum model space distance between geometric entities at asserted c
onnectivities');
#76618=UNCERTAINTY_MEASURE_WITH_UNIT(LENGTH_MEASURE(0.001),#76661,
'DISTANCE_ACCURACY_VALUE',
'Maximum model space distance between geometric entities at asserted c
onnectivities');
#76619=UNCERTAINTY_MEASURE_WITH_UNIT(LENGTH_MEASURE(0.001),#76661,
'DISTANCE_ACCURACY_VALUE',
'Maximum model space distance between geometric entities at asserted c
onnectivities');
#76620=UNCERTAINTY_MEASURE_WITH_UNIT(LENGTH_MEASURE(0.001),#76661,
'DISTANCE_ACCURACY_VALUE',
'Maximum model space distance between geometric entities at asserted c
onnectivities');
#76621=UNCERTAINTY_MEASURE_WITH_UNIT(LENGTH_MEASURE(0.001),#76661,
'DISTANCE_ACCURACY_VALUE',
'Maximum model space distance between geometric entities at asserted c
onnectivities');
#76622=UNCERTAINTY_MEASURE_WITH_UNIT(LENGTH_MEASURE(0.001),#76661,
'DISTANCE_ACCURACY_VALUE',
'Maximum model space distance between geometric entities at asserted c
onnectivities');
#76623=UNCERTAINTY_MEASURE_WITH_UNIT(LENGTH_MEASURE(0.001),#76661,
'DISTANCE_ACCURACY_VALUE',
'Maximum model space distance between geometric entities at asserted c
onnectivities');
#76624=UNCERTAINTY_MEASURE_WITH_UNIT(LENGTH_MEASURE(0.001),#76661,
'DISTANCE_ACCURACY_VALUE',
'Maximum model space distance between geometric entities at asserted c
onnectivities');
#76625=UNCERTAINTY_MEASURE_WITH_UNIT(LENGTH_MEASURE(0.001),#76661,
'DISTANCE_ACCURACY_VALUE',
'Maximum model space distance between geometric entities at asserted c
onnectivities');
#76626=UNCERTAINTY_MEASURE_WITH_UNIT(LENGTH_MEASURE(0.001),#76661,
'DISTANCE_ACCURACY_VALUE',
'Maximum model space distance between geometric entities at asserted c
onnectivities');
#76627=UNCERTAINTY_MEASURE_WITH_UNIT(LENGTH_MEASURE(0.001),#76661,
'DISTANCE_ACCURACY_VALUE',
'Maximum model space distance between geometric entities at asserted c
onnectivities');
#76628=UNCERTAINTY_MEASURE_WITH_UNIT(LENGTH_MEASURE(0.001),#76661,
'DISTANCE_ACCURACY_VALUE',
'Maximum model space distance between geometric entities at asserted c
onnectivities');
#76629=UNCERTAINTY_MEASURE_WITH_UNIT(LENGTH_MEASURE(0.001),#76661,
'DISTANCE_ACCURACY_VALUE',
'Maximum model space distance between geometric entities at asserted c
onnectivities');
#76630=UNCERTAINTY_MEASURE_WITH_UNIT(LENGTH_MEASURE(0.001),#76661,
'DISTANCE_ACCURACY_VALUE',
'Maximum model space distance between geometric entities at asserted c
onnectivities');
#76631=UNCERTAINTY_MEASURE_WITH_UNIT(LENGTH_MEASURE(0.001),#76661,
'DISTANCE_ACCURACY_VALUE',
'Maximum model space distance between geometric entities at asserted c
onnectivities');
#76632=UNCERTAINTY_MEASURE_WITH_UNIT(LENGTH_MEASURE(0.001),#76661,
'DISTANCE_ACCURACY_VALUE',
'Maximum model space distance between geometric entities at asserted c
onnectivities');
#76633=UNCERTAINTY_MEASURE_WITH_UNIT(LENGTH_MEASURE(0.001),#76661,
'DISTANCE_ACCURACY_VALUE',
'Maximum model space distance between geometric entities at asserted c
onnectivities');
#76634=UNCERTAINTY_MEASURE_WITH_UNIT(LENGTH_MEASURE(0.001),#76661,
'DISTANCE_ACCURACY_VALUE',
'Maximum model space distance between geometric entities at asserted c
onnectivities');
#76635=UNCERTAINTY_MEASURE_WITH_UNIT(LENGTH_MEASURE(0.001),#76661,
'DISTANCE_ACCURACY_VALUE',
'Maximum model space distance between geometric entities at asserted c
onnectivities');
#76636=UNCERTAINTY_MEASURE_WITH_UNIT(LENGTH_MEASURE(0.001),#76661,
'DISTANCE_ACCURACY_VALUE',
'Maximum model space distance between geometric entities at asserted c
onnectivities');
#76637=UNCERTAINTY_MEASURE_WITH_UNIT(LENGTH_MEASURE(0.001),#76661,
'DISTANCE_ACCURACY_VALUE',
'Maximum model space distance between geometric entities at asserted c
onnectivities');
#76638=UNCERTAINTY_MEASURE_WITH_UNIT(LENGTH_MEASURE(0.001),#76661,
'DISTANCE_ACCURACY_VALUE',
'Maximum model space distance between geometric entities at asserted c
onnectivities');
#76639=(
GEOMETRIC_REPRESENTATION_CONTEXT(3)
GLOBAL_UNCERTAINTY_ASSIGNED_CONTEXT((#76617))
GLOBAL_UNIT_ASSIGNED_CONTEXT((#76661,#76663,#76664))
REPRESENTATION_CONTEXT('','3D')
);
#76640=(
GEOMETRIC_REPRESENTATION_CONTEXT(3)
GLOBAL_UNCERTAINTY_ASSIGNED_CONTEXT((#76618))
GLOBAL_UNIT_ASSIGNED_CONTEXT((#76661,#76663,#76664))
REPRESENTATION_CONTEXT('','3D')
);
#76641=(
GEOMETRIC_REPRESENTATION_CONTEXT(3)
GLOBAL_UNCERTAINTY_ASSIGNED_CONTEXT((#76619))
GLOBAL_UNIT_ASSIGNED_CONTEXT((#76661,#76663,#76664))
REPRESENTATION_CONTEXT('','3D')
);
#76642=(
GEOMETRIC_REPRESENTATION_CONTEXT(3)
GLOBAL_UNCERTAINTY_ASSIGNED_CONTEXT((#76620))
GLOBAL_UNIT_ASSIGNED_CONTEXT((#76661,#76663,#76664))
REPRESENTATION_CONTEXT('','3D')
);
#76643=(
GEOMETRIC_REPRESENTATION_CONTEXT(3)
GLOBAL_UNCERTAINTY_ASSIGNED_CONTEXT((#76621))
GLOBAL_UNIT_ASSIGNED_CONTEXT((#76661,#76663,#76664))
REPRESENTATION_CONTEXT('','3D')
);
#76644=(
GEOMETRIC_REPRESENTATION_CONTEXT(3)
GLOBAL_UNCERTAINTY_ASSIGNED_CONTEXT((#76622))
GLOBAL_UNIT_ASSIGNED_CONTEXT((#76661,#76663,#76664))
REPRESENTATION_CONTEXT('','3D')
);
#76645=(
GEOMETRIC_REPRESENTATION_CONTEXT(3)
GLOBAL_UNCERTAINTY_ASSIGNED_CONTEXT((#76623))
GLOBAL_UNIT_ASSIGNED_CONTEXT((#76661,#76663,#76664))
REPRESENTATION_CONTEXT('','3D')
);
#76646=(
GEOMETRIC_REPRESENTATION_CONTEXT(3)
GLOBAL_UNCERTAINTY_ASSIGNED_CONTEXT((#76624))
GLOBAL_UNIT_ASSIGNED_CONTEXT((#76661,#76663,#76664))
REPRESENTATION_CONTEXT('','3D')
);
#76647=(
GEOMETRIC_REPRESENTATION_CONTEXT(3)
GLOBAL_UNCERTAINTY_ASSIGNED_CONTEXT((#76625))
GLOBAL_UNIT_ASSIGNED_CONTEXT((#76661,#76663,#76664))
REPRESENTATION_CONTEXT('','3D')
);
#76648=(
GEOMETRIC_REPRESENTATION_CONTEXT(3)
GLOBAL_UNCERTAINTY_ASSIGNED_CONTEXT((#76626))
GLOBAL_UNIT_ASSIGNED_CONTEXT((#76661,#76663,#76664))
REPRESENTATION_CONTEXT('','3D')
);
#76649=(
GEOMETRIC_REPRESENTATION_CONTEXT(3)
GLOBAL_UNCERTAINTY_ASSIGNED_CONTEXT((#76627))
GLOBAL_UNIT_ASSIGNED_CONTEXT((#76661,#76663,#76664))
REPRESENTATION_CONTEXT('','3D')
);
#76650=(
GEOMETRIC_REPRESENTATION_CONTEXT(3)
GLOBAL_UNCERTAINTY_ASSIGNED_CONTEXT((#76628))
GLOBAL_UNIT_ASSIGNED_CONTEXT((#76661,#76663,#76664))
REPRESENTATION_CONTEXT('','3D')
);
#76651=(
GEOMETRIC_REPRESENTATION_CONTEXT(3)
GLOBAL_UNCERTAINTY_ASSIGNED_CONTEXT((#76629))
GLOBAL_UNIT_ASSIGNED_CONTEXT((#76661,#76663,#76664))
REPRESENTATION_CONTEXT('','3D')
);
#76652=(
GEOMETRIC_REPRESENTATION_CONTEXT(3)
GLOBAL_UNCERTAINTY_ASSIGNED_CONTEXT((#76630))
GLOBAL_UNIT_ASSIGNED_CONTEXT((#76661,#76663,#76664))
REPRESENTATION_CONTEXT('','3D')
);
#76653=(
GEOMETRIC_REPRESENTATION_CONTEXT(3)
GLOBAL_UNCERTAINTY_ASSIGNED_CONTEXT((#76631))
GLOBAL_UNIT_ASSIGNED_CONTEXT((#76661,#76663,#76664))
REPRESENTATION_CONTEXT('','3D')
);
#76654=(
GEOMETRIC_REPRESENTATION_CONTEXT(3)
GLOBAL_UNCERTAINTY_ASSIGNED_CONTEXT((#76632))
GLOBAL_UNIT_ASSIGNED_CONTEXT((#76661,#76663,#76664))
REPRESENTATION_CONTEXT('','3D')
);
#76655=(
GEOMETRIC_REPRESENTATION_CONTEXT(3)
GLOBAL_UNCERTAINTY_ASSIGNED_CONTEXT((#76633))
GLOBAL_UNIT_ASSIGNED_CONTEXT((#76661,#76663,#76664))
REPRESENTATION_CONTEXT('','3D')
);
#76656=(
GEOMETRIC_REPRESENTATION_CONTEXT(3)
GLOBAL_UNCERTAINTY_ASSIGNED_CONTEXT((#76634))
GLOBAL_UNIT_ASSIGNED_CONTEXT((#76661,#76663,#76664))
REPRESENTATION_CONTEXT('','3D')
);
#76657=(
GEOMETRIC_REPRESENTATION_CONTEXT(3)
GLOBAL_UNCERTAINTY_ASSIGNED_CONTEXT((#76635))
GLOBAL_UNIT_ASSIGNED_CONTEXT((#76661,#76663,#76664))
REPRESENTATION_CONTEXT('','3D')
);
#76658=(
GEOMETRIC_REPRESENTATION_CONTEXT(3)
GLOBAL_UNCERTAINTY_ASSIGNED_CONTEXT((#76636))
GLOBAL_UNIT_ASSIGNED_CONTEXT((#76661,#76663,#76664))
REPRESENTATION_CONTEXT('','3D')
);
#76659=(
GEOMETRIC_REPRESENTATION_CONTEXT(3)
GLOBAL_UNCERTAINTY_ASSIGNED_CONTEXT((#76637))
GLOBAL_UNIT_ASSIGNED_CONTEXT((#76661,#76663,#76664))
REPRESENTATION_CONTEXT('','3D')
);
#76660=(
GEOMETRIC_REPRESENTATION_CONTEXT(3)
GLOBAL_UNCERTAINTY_ASSIGNED_CONTEXT((#76638))
GLOBAL_UNIT_ASSIGNED_CONTEXT((#76661,#76663,#76664))
REPRESENTATION_CONTEXT('','3D')
);
#76661=(
LENGTH_UNIT()
NAMED_UNIT(*)
SI_UNIT(.CENTI.,.METRE.)
);
#76662=(
LENGTH_UNIT()
NAMED_UNIT(*)
SI_UNIT($,.METRE.)
);
#76663=(
NAMED_UNIT(*)
PLANE_ANGLE_UNIT()
SI_UNIT($,.RADIAN.)
);
#76664=(
NAMED_UNIT(*)
SI_UNIT($,.STERADIAN.)
SOLID_ANGLE_UNIT()
);
#76665=SHAPE_DEFINITION_REPRESENTATION(#76686,#76735);
#76666=SHAPE_DEFINITION_REPRESENTATION(#76687,#76736);
#76667=SHAPE_DEFINITION_REPRESENTATION(#76688,#76737);
#76668=SHAPE_DEFINITION_REPRESENTATION(#76689,#76738);
#76669=SHAPE_DEFINITION_REPRESENTATION(#76690,#76739);
#76670=SHAPE_DEFINITION_REPRESENTATION(#76691,#76740);
#76671=SHAPE_DEFINITION_REPRESENTATION(#76692,#76741);
#76672=SHAPE_DEFINITION_REPRESENTATION(#76693,#76742);
#76673=SHAPE_DEFINITION_REPRESENTATION(#76694,#76743);
#76674=SHAPE_DEFINITION_REPRESENTATION(#76695,#76744);
#76675=SHAPE_DEFINITION_REPRESENTATION(#76696,#76745);
#76676=SHAPE_DEFINITION_REPRESENTATION(#76697,#76746);
#76677=SHAPE_DEFINITION_REPRESENTATION(#76698,#76747);
#76678=SHAPE_DEFINITION_REPRESENTATION(#76699,#76748);
#76679=SHAPE_DEFINITION_REPRESENTATION(#76700,#76749);
#76680=SHAPE_DEFINITION_REPRESENTATION(#76701,#76750);
#76681=SHAPE_DEFINITION_REPRESENTATION(#76702,#76751);
#76682=SHAPE_DEFINITION_REPRESENTATION(#76703,#76752);
#76683=SHAPE_DEFINITION_REPRESENTATION(#76704,#76753);
#76684=SHAPE_DEFINITION_REPRESENTATION(#76705,#76754);
#76685=SHAPE_DEFINITION_REPRESENTATION(#76706,#76755);
#76686=PRODUCT_DEFINITION_SHAPE('',$,#76757);
#76687=PRODUCT_DEFINITION_SHAPE('',$,#76758);
#76688=PRODUCT_DEFINITION_SHAPE('',$,#76759);
#76689=PRODUCT_DEFINITION_SHAPE('',$,#76760);
#76690=PRODUCT_DEFINITION_SHAPE('',$,#76761);
#76691=PRODUCT_DEFINITION_SHAPE('',$,#76762);
#76692=PRODUCT_DEFINITION_SHAPE('',$,#76763);
#76693=PRODUCT_DEFINITION_SHAPE('',$,#76764);
#76694=PRODUCT_DEFINITION_SHAPE('',$,#76765);
#76695=PRODUCT_DEFINITION_SHAPE('',$,#76766);
#76696=PRODUCT_DEFINITION_SHAPE('',$,#76767);
#76697=PRODUCT_DEFINITION_SHAPE('',$,#76768);
#76698=PRODUCT_DEFINITION_SHAPE('',$,#76769);
#76699=PRODUCT_DEFINITION_SHAPE('',$,#76770);
#76700=PRODUCT_DEFINITION_SHAPE('',$,#76771);
#76701=PRODUCT_DEFINITION_SHAPE('',$,#76772);
#76702=PRODUCT_DEFINITION_SHAPE('',$,#76773);
#76703=PRODUCT_DEFINITION_SHAPE('',$,#76774);
#76704=PRODUCT_DEFINITION_SHAPE('',$,#76775);
#76705=PRODUCT_DEFINITION_SHAPE('',$,#76776);
#76706=PRODUCT_DEFINITION_SHAPE('',$,#76777);
#76707=PRODUCT_DEFINITION_SHAPE($,$,#95);
#76708=PRODUCT_DEFINITION_SHAPE($,$,#96);
#76709=PRODUCT_DEFINITION_SHAPE($,$,#97);
#76710=PRODUCT_DEFINITION_SHAPE($,$,#98);
#76711=PRODUCT_DEFINITION_SHAPE($,$,#99);
#76712=PRODUCT_DEFINITION_SHAPE($,$,#100);
#76713=PRODUCT_DEFINITION_SHAPE($,$,#101);
#76714=PRODUCT_DEFINITION_SHAPE($,$,#102);
#76715=PRODUCT_DEFINITION_SHAPE($,$,#103);
#76716=PRODUCT_DEFINITION_SHAPE($,$,#104);
#76717=PRODUCT_DEFINITION_SHAPE($,$,#105);
#76718=PRODUCT_DEFINITION_SHAPE($,$,#106);
#76719=PRODUCT_DEFINITION_SHAPE($,$,#107);
#76720=PRODUCT_DEFINITION_SHAPE($,$,#108);
#76721=PRODUCT_DEFINITION_SHAPE($,$,#109);
#76722=PRODUCT_DEFINITION_SHAPE($,$,#110);
#76723=PRODUCT_DEFINITION_SHAPE($,$,#111);
#76724=PRODUCT_DEFINITION_SHAPE($,$,#112);
#76725=PRODUCT_DEFINITION_SHAPE($,$,#113);
#76726=PRODUCT_DEFINITION_SHAPE($,$,#114);
#76727=PRODUCT_DEFINITION_SHAPE($,$,#115);
#76728=PRODUCT_DEFINITION_SHAPE($,$,#116);
#76729=PRODUCT_DEFINITION_SHAPE($,$,#117);
#76730=PRODUCT_DEFINITION_SHAPE($,$,#118);
#76731=PRODUCT_DEFINITION_SHAPE($,$,#119);
#76732=PRODUCT_DEFINITION_SHAPE($,$,#120);
#76733=PRODUCT_DEFINITION_SHAPE($,$,#121);
#76734=PRODUCT_DEFINITION_SHAPE($,$,#122);
#76735=SHAPE_REPRESENTATION('',(#26905,#29317,#29318,#29319,#29320,#29321,
#29322,#29323,#29324,#29325,#29326,#29327,#29328,#29329,#29330,#29331,#29332,
#29333,#29334,#29335,#29336,#29337,#29338,#29339,#29340,#29341,#29342,#29343,
#29344),#76639);
#76736=SHAPE_REPRESENTATION('',(#26906),#76640);
#76737=SHAPE_REPRESENTATION('',(#27141),#76641);
#76738=SHAPE_REPRESENTATION('',(#27395),#76642);
#76739=SHAPE_REPRESENTATION('',(#27575),#76643);
#76740=SHAPE_REPRESENTATION('',(#27589),#76644);
#76741=SHAPE_REPRESENTATION('',(#27721),#76645);
#76742=SHAPE_REPRESENTATION('',(#27753),#76646);
#76743=SHAPE_REPRESENTATION('',(#27825),#76647);
#76744=SHAPE_REPRESENTATION('',(#27875),#76648);
#76745=SHAPE_REPRESENTATION('',(#28206),#76649);
#76746=SHAPE_REPRESENTATION('',(#28229),#76650);
#76747=SHAPE_REPRESENTATION('',(#28282),#76651);
#76748=SHAPE_REPRESENTATION('',(#28289),#76652);
#76749=SHAPE_REPRESENTATION('',(#28344),#76653);
#76750=SHAPE_REPRESENTATION('',(#28363),#76654);
#76751=SHAPE_REPRESENTATION('',(#28431),#76655);
#76752=SHAPE_REPRESENTATION('',(#28525),#76656);
#76753=SHAPE_REPRESENTATION('',(#28560),#76657);
#76754=SHAPE_REPRESENTATION('',(#28632),#76658);
#76755=SHAPE_REPRESENTATION('',(#28978),#76659);
#76756=PRODUCT_DEFINITION_CONTEXT('part definition',#76821,'design');
#76757=PRODUCT_DEFINITION('2026-10-26-11-12-26-492','MAS-311',#76778,#76756);
#76758=PRODUCT_DEFINITION('2026-10-26-11-12-28-115',
'01_Base_Bed_Clamp_Block_Cast_Iron',#76779,#76756);
#76759=PRODUCT_DEFINITION('2026-10-26-11-12-31-151',
'02_Upper_Sliding_Tailstock_Casing',#76780,#76756);
#76760=PRODUCT_DEFINITION('2026-10-26-11-12-37-453',
'03_Quill_Sleeve_D70_MT4_Socket',#76781,#76756);
#76761=PRODUCT_DEFINITION('2026-10-26-11-12-44-090',
'04_Dead_Centre_MT4_60deg',#76782,#76756);
#76762=PRODUCT_DEFINITION('2026-10-26-11-12-44-958',
'05_Quill_Feed_Lead_Screw_Tr20x4',#76783,#76756);
#76763=PRODUCT_DEFINITION('2026-10-26-11-12-47-434',
'06_Lead_Screw_Bronze_Nut_Tr20x4',#76784,#76756);
#76764=PRODUCT_DEFINITION('2026-10-26-11-12-49-269',
'07_Rear_Bearing_Cap_D125',#76785,#76756);
#76765=PRODUCT_DEFINITION('2026-10-26-11-12-58-000',
'09_Quill_Handwheel_D230_4_Spoke',#76786,#76756);
#76766=PRODUCT_DEFINITION('2026-10-26-11-13-05-542',
'10_Handwheel_Lock_Screw_ISO_4762_M8x20',#76787,#76756);
#76767=PRODUCT_DEFINITION('2026-10-26-11-13-21-149',
'11_Parallel_Key_DIN_6885_A_5x5x20',#76788,#76756);
#76768=PRODUCT_DEFINITION('2026-10-26-11-13-22-306',
'12_Quill_Locking_Clamp_Lever_M12',#76789,#76756);
#76769=PRODUCT_DEFINITION('2026-10-26-11-13-25-360',
'13_Quill_Clamp_Shoe_Bronze_D20',#76790,#76756);
#76770=PRODUCT_DEFINITION('2026-10-26-11-13-27-477',
'14_Quill_Guide_Screw_ISO_4028_M8x20_Dog_Point',#76791,#76756);
#76771=PRODUCT_DEFINITION('2026-10-26-11-13-33-347',
'16_Bed_Alignment_Key_Bar_20x12x200',#76792,#76756);
#76772=PRODUCT_DEFINITION('2026-10-26-11-13-34-711',
'17_Bed_Clamping_Bolt_ISO_4017_M16x40',#76793,#76756);
#76773=PRODUCT_DEFINITION('2026-10-26-11-13-38-253',
'18_Tailstock_Bed_Clamping_Plate',#76794,#76756);
#76774=PRODUCT_DEFINITION('2026-10-26-11-12-53-512',
'08_Thrust_Ball_Bearing_51104_20x35x10',#76795,#76756);
#76775=PRODUCT_DEFINITION('2026-10-26-11-13-29-864',
'15_Offset_Adjusting_Screw_ISO_4017_M12x40',#76796,#76756);
#76776=PRODUCT_DEFINITION('2026-10-26-11-13-40-862',
'19_Casing_Screw_ISO_4762_M10x35',#76797,#76756);
#76777=PRODUCT_DEFINITION('2026-10-26-11-14-00-117',
'20_Rear_Cap_Screw_ISO_4762_M6x20',#76798,#76756);
#76778=PRODUCT_DEFINITION_FORMATION('',$,#76823);
#76779=PRODUCT_DEFINITION_FORMATION('',$,#76824);
#76780=PRODUCT_DEFINITION_FORMATION('',$,#76825);
#76781=PRODUCT_DEFINITION_FORMATION('',$,#76826);
#76782=PRODUCT_DEFINITION_FORMATION('',$,#76827);
#76783=PRODUCT_DEFINITION_FORMATION('',$,#76828);
#76784=PRODUCT_DEFINITION_FORMATION('',$,#76829);
#76785=PRODUCT_DEFINITION_FORMATION('',$,#76830);
#76786=PRODUCT_DEFINITION_FORMATION('',$,#76831);
#76787=PRODUCT_DEFINITION_FORMATION('',$,#76832);
#76788=PRODUCT_DEFINITION_FORMATION('',$,#76833);
#76789=PRODUCT_DEFINITION_FORMATION('',$,#76834);
#76790=PRODUCT_DEFINITION_FORMATION('',$,#76835);
#76791=PRODUCT_DEFINITION_FORMATION('',$,#76836);
#76792=PRODUCT_DEFINITION_FORMATION('',$,#76837);
#76793=PRODUCT_DEFINITION_FORMATION('',$,#76838);
#76794=PRODUCT_DEFINITION_FORMATION('',$,#76839);
#76795=PRODUCT_DEFINITION_FORMATION('',$,#76840);
#76796=PRODUCT_DEFINITION_FORMATION('',$,#76841);
#76797=PRODUCT_DEFINITION_FORMATION('',$,#76842);
#76798=PRODUCT_DEFINITION_FORMATION('',$,#76843);
#76799=PRODUCT_RELATED_PRODUCT_CATEGORY('MAS-311','MAS-311',(#76823));
#76800=PRODUCT_RELATED_PRODUCT_CATEGORY(
'01_Base_Bed_Clamp_Block_Cast_Iron','01_Base_Bed_Clamp_Block_Cast_Iron',
(#76824));
#76801=PRODUCT_RELATED_PRODUCT_CATEGORY(
'02_Upper_Sliding_Tailstock_Casing','02_Upper_Sliding_Tailstock_Casing',
(#76825));
#76802=PRODUCT_RELATED_PRODUCT_CATEGORY(
'03_Quill_Sleeve_D70_MT4_Socket','03_Quill_Sleeve_D70_MT4_Socket',(#76826));
#76803=PRODUCT_RELATED_PRODUCT_CATEGORY('04_Dead_Centre_MT4_60deg',
'04_Dead_Centre_MT4_60deg',(#76827));
#76804=PRODUCT_RELATED_PRODUCT_CATEGORY(
'05_Quill_Feed_Lead_Screw_Tr20x4','05_Quill_Feed_Lead_Screw_Tr20x4',(#76828));
#76805=PRODUCT_RELATED_PRODUCT_CATEGORY(
'06_Lead_Screw_Bronze_Nut_Tr20x4','06_Lead_Screw_Bronze_Nut_Tr20x4',(#76829));
#76806=PRODUCT_RELATED_PRODUCT_CATEGORY('07_Rear_Bearing_Cap_D125',
'07_Rear_Bearing_Cap_D125',(#76830));
#76807=PRODUCT_RELATED_PRODUCT_CATEGORY(
'09_Quill_Handwheel_D230_4_Spoke','09_Quill_Handwheel_D230_4_Spoke',(#76831));
#76808=PRODUCT_RELATED_PRODUCT_CATEGORY(
'10_Handwheel_Lock_Screw_ISO_4762_M8x20',
'10_Handwheel_Lock_Screw_ISO_4762_M8x20',(#76832));
#76809=PRODUCT_RELATED_PRODUCT_CATEGORY(
'11_Parallel_Key_DIN_6885_A_5x5x20','11_Parallel_Key_DIN_6885_A_5x5x20',
(#76833));
#76810=PRODUCT_RELATED_PRODUCT_CATEGORY(
'12_Quill_Locking_Clamp_Lever_M12','12_Quill_Locking_Clamp_Lever_M12',(#76834));
#76811=PRODUCT_RELATED_PRODUCT_CATEGORY(
'13_Quill_Clamp_Shoe_Bronze_D20','13_Quill_Clamp_Shoe_Bronze_D20',(#76835));
#76812=PRODUCT_RELATED_PRODUCT_CATEGORY(
'14_Quill_Guide_Screw_ISO_4028_M8x20_Dog_Point',
'14_Quill_Guide_Screw_ISO_4028_M8x20_Dog_Point',(#76836));
#76813=PRODUCT_RELATED_PRODUCT_CATEGORY(
'16_Bed_Alignment_Key_Bar_20x12x200',
'16_Bed_Alignment_Key_Bar_20x12x200',(#76837));
#76814=PRODUCT_RELATED_PRODUCT_CATEGORY(
'17_Bed_Clamping_Bolt_ISO_4017_M16x40',
'17_Bed_Clamping_Bolt_ISO_4017_M16x40',(#76838));
#76815=PRODUCT_RELATED_PRODUCT_CATEGORY(
'18_Tailstock_Bed_Clamping_Plate','18_Tailstock_Bed_Clamping_Plate',(#76839));
#76816=PRODUCT_RELATED_PRODUCT_CATEGORY(
'08_Thrust_Ball_Bearing_51104_20x35x10',
'08_Thrust_Ball_Bearing_51104_20x35x10',(#76840));
#76817=PRODUCT_RELATED_PRODUCT_CATEGORY(
'15_Offset_Adjusting_Screw_ISO_4017_M12x40',
'15_Offset_Adjusting_Screw_ISO_4017_M12x40',(#76841));
#76818=PRODUCT_RELATED_PRODUCT_CATEGORY(
'19_Casing_Screw_ISO_4762_M10x35','19_Casing_Screw_ISO_4762_M10x35',(#76842));
#76819=PRODUCT_RELATED_PRODUCT_CATEGORY(
'20_Rear_Cap_Screw_ISO_4762_M6x20','20_Rear_Cap_Screw_ISO_4762_M6x20',(#76843));
#76820=APPLICATION_PROTOCOL_DEFINITION('international standard',
'automotive_design',2009,#76821);
#76821=APPLICATION_CONTEXT(
'Core Data for Automotive Mechanical Design Process');
#76822=PRODUCT_CONTEXT('part definition',#76821,'mechanical');
#76823=PRODUCT('2026-10-26-11-12-26-492','MAS-311',$,(#76822));
#76824=PRODUCT('2026-10-26-11-12-28-115',
'01_Base_Bed_Clamp_Block_Cast_Iron',$,(#76822));
#76825=PRODUCT('2026-10-26-11-12-31-151',
'02_Upper_Sliding_Tailstock_Casing',$,(#76822));
#76826=PRODUCT('2026-10-26-11-12-37-453',
'03_Quill_Sleeve_D70_MT4_Socket',$,(#76822));
#76827=PRODUCT('2026-10-26-11-12-44-090','04_Dead_Centre_MT4_60deg',$,(#76822));
#76828=PRODUCT('2026-10-26-11-12-44-958',
'05_Quill_Feed_Lead_Screw_Tr20x4',$,(#76822));
#76829=PRODUCT('2026-10-26-11-12-47-434',
'06_Lead_Screw_Bronze_Nut_Tr20x4',$,(#76822));
#76830=PRODUCT('2026-10-26-11-12-49-269','07_Rear_Bearing_Cap_D125',$,(#76822));
#76831=PRODUCT('2026-10-26-11-12-58-000',
'09_Quill_Handwheel_D230_4_Spoke',$,(#76822));
#76832=PRODUCT('2026-10-26-11-13-05-542',
'10_Handwheel_Lock_Screw_ISO_4762_M8x20',$,(#76822));
#76833=PRODUCT('2026-10-26-11-13-21-149',
'11_Parallel_Key_DIN_6885_A_5x5x20',$,(#76822));
#76834=PRODUCT('2026-10-26-11-13-22-306',
'12_Quill_Locking_Clamp_Lever_M12',$,(#76822));
#76835=PRODUCT('2026-10-26-11-13-25-360',
'13_Quill_Clamp_Shoe_Bronze_D20',$,(#76822));
#76836=PRODUCT('2026-10-26-11-13-27-477',
'14_Quill_Guide_Screw_ISO_4028_M8x20_Dog_Point',$,(#76822));
#76837=PRODUCT('2026-10-26-11-13-33-347',
'16_Bed_Alignment_Key_Bar_20x12x200',$,(#76822));
#76838=PRODUCT('2026-10-26-11-13-34-711',
'17_Bed_Clamping_Bolt_ISO_4017_M16x40',$,(#76822));
#76839=PRODUCT('2026-10-26-11-13-38-253',
'18_Tailstock_Bed_Clamping_Plate',$,(#76822));
#76840=PRODUCT('2026-10-26-11-12-53-512',
'08_Thrust_Ball_Bearing_51104_20x35x10',$,(#76822));
#76841=PRODUCT('2026-10-26-11-13-29-864',
'15_Offset_Adjusting_Screw_ISO_4017_M12x40',$,(#76822));
#76842=PRODUCT('2026-10-26-11-13-40-862',
'19_Casing_Screw_ISO_4762_M10x35',$,(#76822));
#76843=PRODUCT('2026-10-26-11-14-00-117',
'20_Rear_Cap_Screw_ISO_4762_M6x20',$,(#76822));
#76844=PRESENTATION_STYLE_ASSIGNMENT((#76849));
#76845=PRESENTATION_STYLE_ASSIGNMENT((#76850));
#76846=PRESENTATION_STYLE_ASSIGNMENT((#76851));
#76847=PRESENTATION_STYLE_ASSIGNMENT((#76852));
#76848=PRESENTATION_STYLE_ASSIGNMENT((#76853));
#76849=SURFACE_STYLE_USAGE(.BOTH.,#76854);
#76850=SURFACE_STYLE_USAGE(.BOTH.,#76855);
#76851=SURFACE_STYLE_USAGE(.BOTH.,#76856);
#76852=SURFACE_STYLE_USAGE(.BOTH.,#76857);
#76853=SURFACE_STYLE_USAGE(.BOTH.,#76858);
#76854=SURFACE_SIDE_STYLE('',(#76859));
#76855=SURFACE_SIDE_STYLE('',(#76860));
#76856=SURFACE_SIDE_STYLE('',(#76861));
#76857=SURFACE_SIDE_STYLE('',(#76862));
#76858=SURFACE_SIDE_STYLE('',(#76863));
#76859=SURFACE_STYLE_FILL_AREA(#76864);
#76860=SURFACE_STYLE_FILL_AREA(#76865);
#76861=SURFACE_STYLE_FILL_AREA(#76866);
#76862=SURFACE_STYLE_FILL_AREA(#76867);
#76863=SURFACE_STYLE_FILL_AREA(#76868);
#76864=FILL_AREA_STYLE('Steel - Satin',(#76869));
#76865=FILL_AREA_STYLE('Gunmetal_Silver_50565D',(#76870));
#76866=FILL_AREA_STYLE('Brushed_Titanium_Silver_8C9298',(#76871));
#76867=FILL_AREA_STYLE('Polished_Stainless_Steel_D6D9DC',(#76872));
#76868=FILL_AREA_STYLE('Satin_Aluminium_ADB4BA',(#76873));
#76869=FILL_AREA_STYLE_COLOUR('Steel - Satin',#76874);
#76870=FILL_AREA_STYLE_COLOUR('Gunmetal_Silver_50565D',#76875);
#76871=FILL_AREA_STYLE_COLOUR('Brushed_Titanium_Silver_8C9298',#76876);
#76872=FILL_AREA_STYLE_COLOUR('Polished_Stainless_Steel_D6D9DC',#76877);
#76873=FILL_AREA_STYLE_COLOUR('Satin_Aluminium_ADB4BA',#76878);
#76874=COLOUR_RGB('Steel - Satin',0.627450980392157,0.627450980392157,0.627450980392157);
#76875=COLOUR_RGB('Gunmetal_Silver_50565D',0.313725490196078,0.337254901960784,
0.364705882352941);
#76876=COLOUR_RGB('Brushed_Titanium_Silver_8C9298',0.549019607843137,0.572549019607843,
0.596078431372549);
#76877=COLOUR_RGB('Polished_Stainless_Steel_D6D9DC',0.83921568627451,0.850980392156863,
0.862745098039216);
#76878=COLOUR_RGB('Satin_Aluminium_ADB4BA',0.67843137254902,0.705882352941177,
0.729411764705882);
#76879=COLOUR_RGB('Dark Blue',0.08,0.2,0.34);
#76880=FILL_AREA_STYLE_COLOUR('',#76879);
#76881=FILL_AREA_STYLE('',(#76880));
#76882=SURFACE_STYLE_FILL_AREA(#76881);
#76883=SURFACE_SIDE_STYLE('',(#76882));
#76884=SURFACE_STYLE_USAGE(.BOTH.,#76883);
#76885=PRESENTATION_STYLE_ASSIGNMENT((#76884));
#76886=COLOUR_RGB('Light Blue',0.38,0.62,0.78);
#76887=FILL_AREA_STYLE_COLOUR('',#76886);
#76888=FILL_AREA_STYLE('',(#76887));
#76889=SURFACE_STYLE_FILL_AREA(#76888);
#76890=SURFACE_SIDE_STYLE('',(#76889));
#76891=SURFACE_STYLE_USAGE(.BOTH.,#76890);
#76892=PRESENTATION_STYLE_ASSIGNMENT((#76891));
#76893=COLOUR_RGB('Sky Blue',0.24,0.69,0.87);
#76894=FILL_AREA_STYLE_COLOUR('',#76893);
#76895=FILL_AREA_STYLE('',(#76894));
#76896=SURFACE_STYLE_FILL_AREA(#76895);
#76897=SURFACE_SIDE_STYLE('',(#76896));
#76898=SURFACE_STYLE_USAGE(.BOTH.,#76897);
#76899=PRESENTATION_STYLE_ASSIGNMENT((#76898));
#76900=COLOUR_RGB('Grey',0.48,0.52,0.57);
#76901=FILL_AREA_STYLE_COLOUR('',#76900);
#76902=FILL_AREA_STYLE('',(#76901));
#76903=SURFACE_STYLE_FILL_AREA(#76902);
#76904=SURFACE_SIDE_STYLE('',(#76903));
#76905=SURFACE_STYLE_USAGE(.BOTH.,#76904);
#76906=PRESENTATION_STYLE_ASSIGNMENT((#76905));
#76907=COLOUR_RGB('Black',0.12,0.14,0.17);
#76908=FILL_AREA_STYLE_COLOUR('',#76907);
#76909=FILL_AREA_STYLE('',(#76908));
#76910=SURFACE_STYLE_FILL_AREA(#76909);
#76911=SURFACE_SIDE_STYLE('',(#76910));
#76912=SURFACE_STYLE_USAGE(.BOTH.,#76911);
#76913=PRESENTATION_STYLE_ASSIGNMENT((#76912));
#76914=COLOUR_RGB('Off White',0.89,0.88,0.83);
#76915=FILL_AREA_STYLE_COLOUR('',#76914);
#76916=FILL_AREA_STYLE('',(#76915));
#76917=SURFACE_STYLE_FILL_AREA(#76916);
#76918=SURFACE_SIDE_STYLE('',(#76917));
#76919=SURFACE_STYLE_USAGE(.BOTH.,#76918);
#76920=PRESENTATION_STYLE_ASSIGNMENT((#76919));
ENDSEC;
END-ISO-10303-21;
